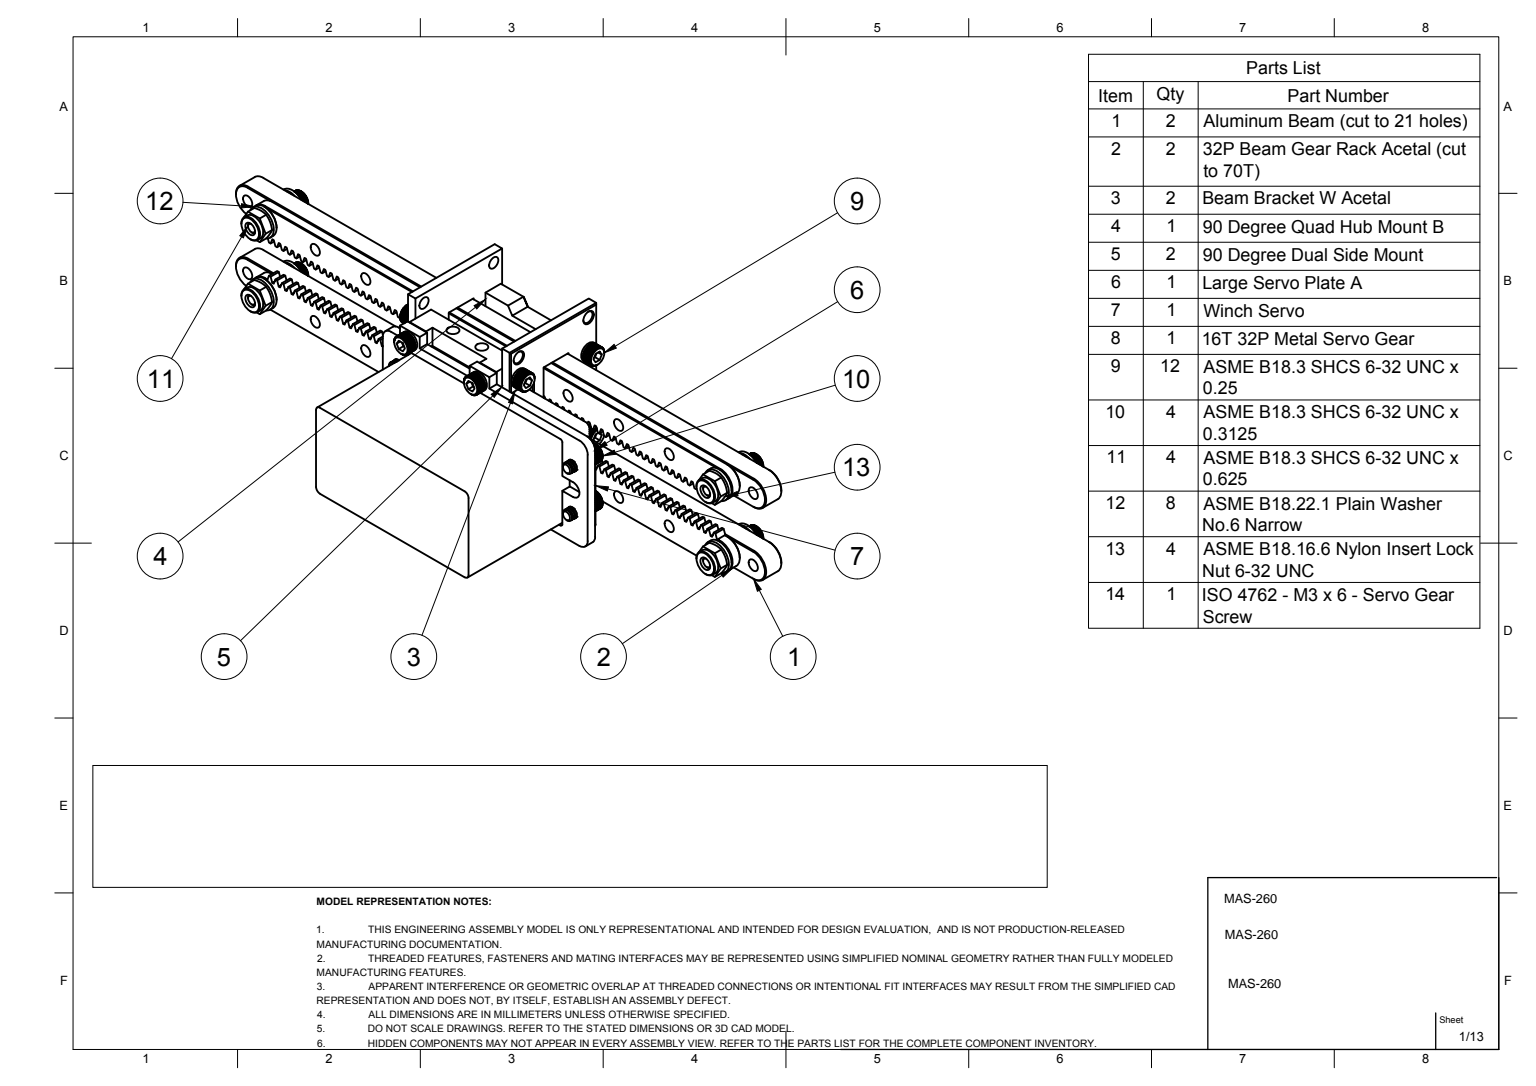
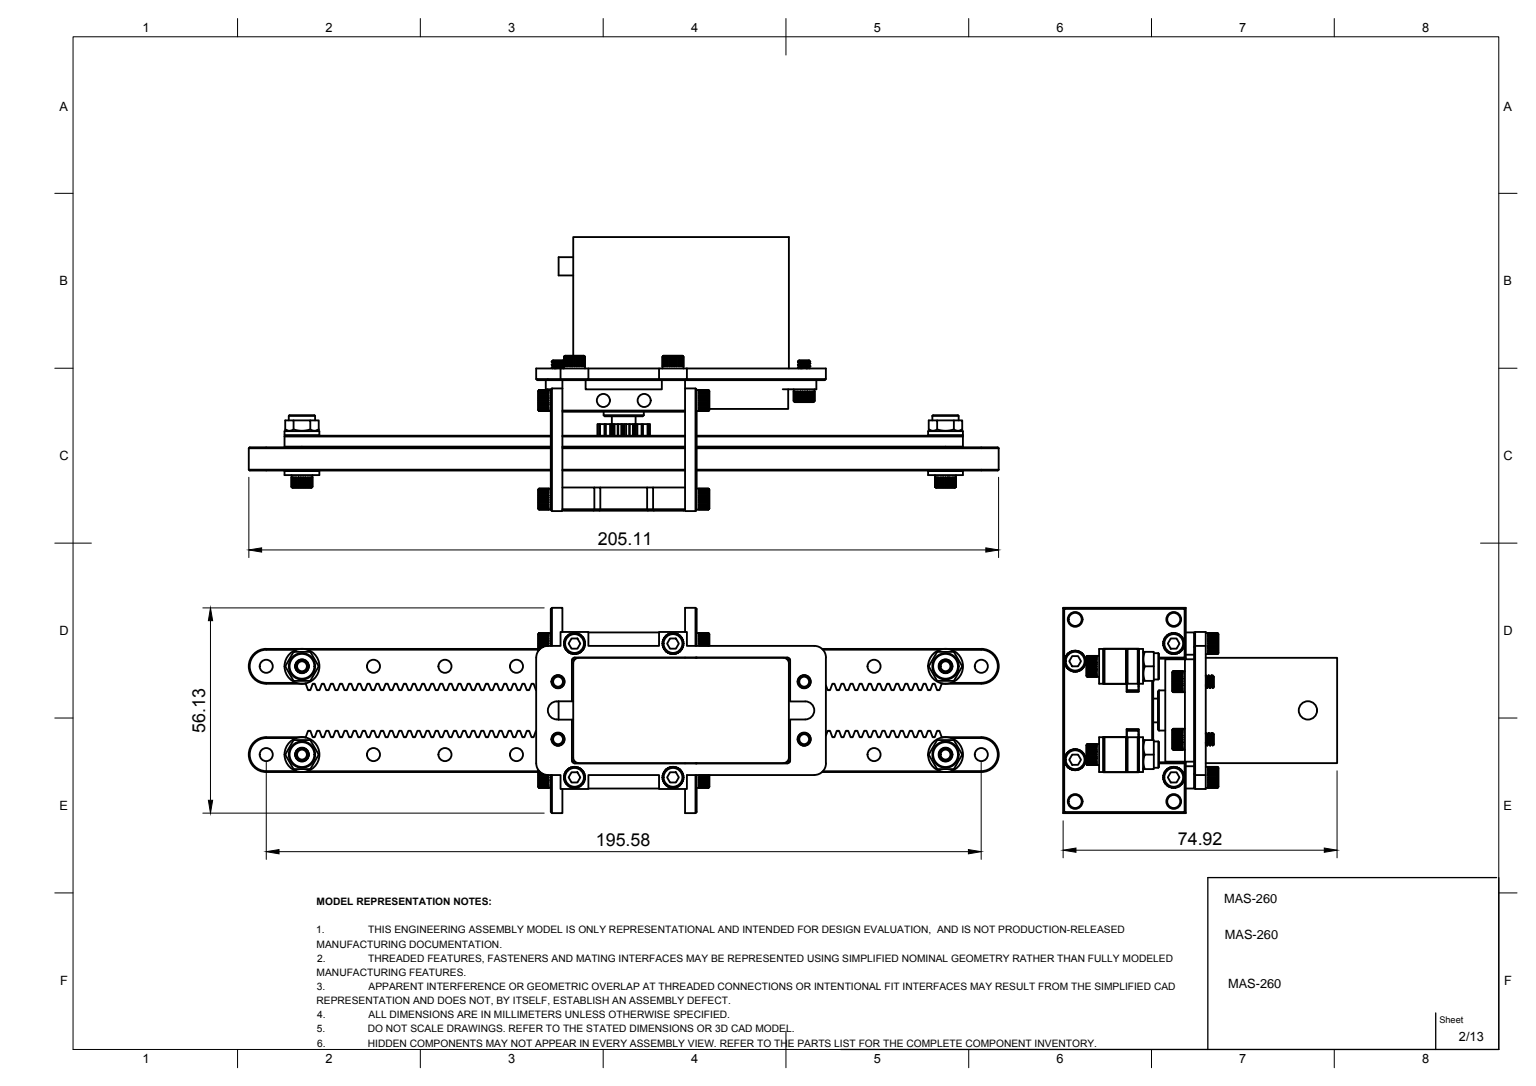
ISO-10303-21;
HEADER;
/* Generated by software containing ST-Developer
 * from STEP Tools, Inc. (www.steptools.com) 
 */

FILE_DESCRIPTION(
/* description */ (''),
/* implementation_level */ '2;1');

FILE_NAME(
/* name */ 'MAS-260',
/* time_stamp */ '2026-10-15T13:29:10-07:00',
/* author */ (''),
/* organization */ (''),
/* preprocessor_version */ 'ST-DEVELOPER v20.2',
/* originating_system */ 'Autodesk Translation Framework v15.15.0.0',
/* authorisation */ '');

FILE_SCHEMA (('AUTOMOTIVE_DESIGN { 1 0 10303 214 3 1 1 }'));
ENDSEC;

DATA;
#10=MECHANICAL_DESIGN_GEOMETRIC_PRESENTATION_REPRESENTATION('',(#933,#934,
#935,#936,#937,#938,#939,#940,#941,#942,#943,#944,#945,#946),#83219);
#11=ITEM_DEFINED_TRANSFORMATION($,$,#27872,#29210);
#12=ITEM_DEFINED_TRANSFORMATION($,$,#28000,#29211);
#13=ITEM_DEFINED_TRANSFORMATION($,$,#28335,#29212);
#14=ITEM_DEFINED_TRANSFORMATION($,$,#27099,#29213);
#15=ITEM_DEFINED_TRANSFORMATION($,$,#28406,#29214);
#16=ITEM_DEFINED_TRANSFORMATION($,$,#27207,#29215);
#17=ITEM_DEFINED_TRANSFORMATION($,$,#27360,#29216);
#18=ITEM_DEFINED_TRANSFORMATION($,$,#27453,#29217);
#19=ITEM_DEFINED_TRANSFORMATION($,$,#28461,#29218);
#20=ITEM_DEFINED_TRANSFORMATION($,$,#28693,#29219);
#21=ITEM_DEFINED_TRANSFORMATION($,$,#28927,#29220);
#22=ITEM_DEFINED_TRANSFORMATION($,$,#29171,#29221);
#23=ITEM_DEFINED_TRANSFORMATION($,$,#29184,#29222);
#24=ITEM_DEFINED_TRANSFORMATION($,$,#27595,#29223);
#25=ITEM_DEFINED_TRANSFORMATION($,$,#27872,#29224);
#26=ITEM_DEFINED_TRANSFORMATION($,$,#28000,#29225);
#27=ITEM_DEFINED_TRANSFORMATION($,$,#28335,#29226);
#28=ITEM_DEFINED_TRANSFORMATION($,$,#28406,#29227);
#29=ITEM_DEFINED_TRANSFORMATION($,$,#28461,#29228);
#30=ITEM_DEFINED_TRANSFORMATION($,$,#28461,#29229);
#31=ITEM_DEFINED_TRANSFORMATION($,$,#28461,#29230);
#32=ITEM_DEFINED_TRANSFORMATION($,$,#28461,#29231);
#33=ITEM_DEFINED_TRANSFORMATION($,$,#28461,#29232);
#34=ITEM_DEFINED_TRANSFORMATION($,$,#28461,#29233);
#35=ITEM_DEFINED_TRANSFORMATION($,$,#28461,#29234);
#36=ITEM_DEFINED_TRANSFORMATION($,$,#28461,#29235);
#37=ITEM_DEFINED_TRANSFORMATION($,$,#28461,#29236);
#38=ITEM_DEFINED_TRANSFORMATION($,$,#28461,#29237);
#39=ITEM_DEFINED_TRANSFORMATION($,$,#28461,#29238);
#40=ITEM_DEFINED_TRANSFORMATION($,$,#28693,#29239);
#41=ITEM_DEFINED_TRANSFORMATION($,$,#28693,#29240);
#42=ITEM_DEFINED_TRANSFORMATION($,$,#28693,#29241);
#43=ITEM_DEFINED_TRANSFORMATION($,$,#28927,#29242);
#44=ITEM_DEFINED_TRANSFORMATION($,$,#28927,#29243);
#45=ITEM_DEFINED_TRANSFORMATION($,$,#28927,#29244);
#46=ITEM_DEFINED_TRANSFORMATION($,$,#29171,#29245);
#47=ITEM_DEFINED_TRANSFORMATION($,$,#29171,#29246);
#48=ITEM_DEFINED_TRANSFORMATION($,$,#29171,#29247);
#49=ITEM_DEFINED_TRANSFORMATION($,$,#29171,#29248);
#50=ITEM_DEFINED_TRANSFORMATION($,$,#29171,#29249);
#51=ITEM_DEFINED_TRANSFORMATION($,$,#29171,#29250);
#52=ITEM_DEFINED_TRANSFORMATION($,$,#29171,#29251);
#53=ITEM_DEFINED_TRANSFORMATION($,$,#29184,#29252);
#54=ITEM_DEFINED_TRANSFORMATION($,$,#29184,#29253);
#55=ITEM_DEFINED_TRANSFORMATION($,$,#29184,#29254);
#56=(
REPRESENTATION_RELATIONSHIP($,$,#83305,#83299)
REPRESENTATION_RELATIONSHIP_WITH_TRANSFORMATION(#11)
SHAPE_REPRESENTATION_RELATIONSHIP()
);
#57=(
REPRESENTATION_RELATIONSHIP($,$,#83306,#83299)
REPRESENTATION_RELATIONSHIP_WITH_TRANSFORMATION(#12)
SHAPE_REPRESENTATION_RELATIONSHIP()
);
#58=(
REPRESENTATION_RELATIONSHIP($,$,#83307,#83299)
REPRESENTATION_RELATIONSHIP_WITH_TRANSFORMATION(#13)
SHAPE_REPRESENTATION_RELATIONSHIP()
);
#59=(
REPRESENTATION_RELATIONSHIP($,$,#83300,#83299)
REPRESENTATION_RELATIONSHIP_WITH_TRANSFORMATION(#14)
SHAPE_REPRESENTATION_RELATIONSHIP()
);
#60=(
REPRESENTATION_RELATIONSHIP($,$,#83308,#83299)
REPRESENTATION_RELATIONSHIP_WITH_TRANSFORMATION(#15)
SHAPE_REPRESENTATION_RELATIONSHIP()
);
#61=(
REPRESENTATION_RELATIONSHIP($,$,#83301,#83299)
REPRESENTATION_RELATIONSHIP_WITH_TRANSFORMATION(#16)
SHAPE_REPRESENTATION_RELATIONSHIP()
);
#62=(
REPRESENTATION_RELATIONSHIP($,$,#83302,#83299)
REPRESENTATION_RELATIONSHIP_WITH_TRANSFORMATION(#17)
SHAPE_REPRESENTATION_RELATIONSHIP()
);
#63=(
REPRESENTATION_RELATIONSHIP($,$,#83303,#83299)
REPRESENTATION_RELATIONSHIP_WITH_TRANSFORMATION(#18)
SHAPE_REPRESENTATION_RELATIONSHIP()
);
#64=(
REPRESENTATION_RELATIONSHIP($,$,#83309,#83299)
REPRESENTATION_RELATIONSHIP_WITH_TRANSFORMATION(#19)
SHAPE_REPRESENTATION_RELATIONSHIP()
);
#65=(
REPRESENTATION_RELATIONSHIP($,$,#83310,#83299)
REPRESENTATION_RELATIONSHIP_WITH_TRANSFORMATION(#20)
SHAPE_REPRESENTATION_RELATIONSHIP()
);
#66=(
REPRESENTATION_RELATIONSHIP($,$,#83311,#83299)
REPRESENTATION_RELATIONSHIP_WITH_TRANSFORMATION(#21)
SHAPE_REPRESENTATION_RELATIONSHIP()
);
#67=(
REPRESENTATION_RELATIONSHIP($,$,#83312,#83299)
REPRESENTATION_RELATIONSHIP_WITH_TRANSFORMATION(#22)
SHAPE_REPRESENTATION_RELATIONSHIP()
);
#68=(
REPRESENTATION_RELATIONSHIP($,$,#83313,#83299)
REPRESENTATION_RELATIONSHIP_WITH_TRANSFORMATION(#23)
SHAPE_REPRESENTATION_RELATIONSHIP()
);
#69=(
REPRESENTATION_RELATIONSHIP($,$,#83304,#83299)
REPRESENTATION_RELATIONSHIP_WITH_TRANSFORMATION(#24)
SHAPE_REPRESENTATION_RELATIONSHIP()
);
#70=(
REPRESENTATION_RELATIONSHIP($,$,#83305,#83299)
REPRESENTATION_RELATIONSHIP_WITH_TRANSFORMATION(#25)
SHAPE_REPRESENTATION_RELATIONSHIP()
);
#71=(
REPRESENTATION_RELATIONSHIP($,$,#83306,#83299)
REPRESENTATION_RELATIONSHIP_WITH_TRANSFORMATION(#26)
SHAPE_REPRESENTATION_RELATIONSHIP()
);
#72=(
REPRESENTATION_RELATIONSHIP($,$,#83307,#83299)
REPRESENTATION_RELATIONSHIP_WITH_TRANSFORMATION(#27)
SHAPE_REPRESENTATION_RELATIONSHIP()
);
#73=(
REPRESENTATION_RELATIONSHIP($,$,#83308,#83299)
REPRESENTATION_RELATIONSHIP_WITH_TRANSFORMATION(#28)
SHAPE_REPRESENTATION_RELATIONSHIP()
);
#74=(
REPRESENTATION_RELATIONSHIP($,$,#83309,#83299)
REPRESENTATION_RELATIONSHIP_WITH_TRANSFORMATION(#29)
SHAPE_REPRESENTATION_RELATIONSHIP()
);
#75=(
REPRESENTATION_RELATIONSHIP($,$,#83309,#83299)
REPRESENTATION_RELATIONSHIP_WITH_TRANSFORMATION(#30)
SHAPE_REPRESENTATION_RELATIONSHIP()
);
#76=(
REPRESENTATION_RELATIONSHIP($,$,#83309,#83299)
REPRESENTATION_RELATIONSHIP_WITH_TRANSFORMATION(#31)
SHAPE_REPRESENTATION_RELATIONSHIP()
);
#77=(
REPRESENTATION_RELATIONSHIP($,$,#83309,#83299)
REPRESENTATION_RELATIONSHIP_WITH_TRANSFORMATION(#32)
SHAPE_REPRESENTATION_RELATIONSHIP()
);
#78=(
REPRESENTATION_RELATIONSHIP($,$,#83309,#83299)
REPRESENTATION_RELATIONSHIP_WITH_TRANSFORMATION(#33)
SHAPE_REPRESENTATION_RELATIONSHIP()
);
#79=(
REPRESENTATION_RELATIONSHIP($,$,#83309,#83299)
REPRESENTATION_RELATIONSHIP_WITH_TRANSFORMATION(#34)
SHAPE_REPRESENTATION_RELATIONSHIP()
);
#80=(
REPRESENTATION_RELATIONSHIP($,$,#83309,#83299)
REPRESENTATION_RELATIONSHIP_WITH_TRANSFORMATION(#35)
SHAPE_REPRESENTATION_RELATIONSHIP()
);
#81=(
REPRESENTATION_RELATIONSHIP($,$,#83309,#83299)
REPRESENTATION_RELATIONSHIP_WITH_TRANSFORMATION(#36)
SHAPE_REPRESENTATION_RELATIONSHIP()
);
#82=(
REPRESENTATION_RELATIONSHIP($,$,#83309,#83299)
REPRESENTATION_RELATIONSHIP_WITH_TRANSFORMATION(#37)
SHAPE_REPRESENTATION_RELATIONSHIP()
);
#83=(
REPRESENTATION_RELATIONSHIP($,$,#83309,#83299)
REPRESENTATION_RELATIONSHIP_WITH_TRANSFORMATION(#38)
SHAPE_REPRESENTATION_RELATIONSHIP()
);
#84=(
REPRESENTATION_RELATIONSHIP($,$,#83309,#83299)
REPRESENTATION_RELATIONSHIP_WITH_TRANSFORMATION(#39)
SHAPE_REPRESENTATION_RELATIONSHIP()
);
#85=(
REPRESENTATION_RELATIONSHIP($,$,#83310,#83299)
REPRESENTATION_RELATIONSHIP_WITH_TRANSFORMATION(#40)
SHAPE_REPRESENTATION_RELATIONSHIP()
);
#86=(
REPRESENTATION_RELATIONSHIP($,$,#83310,#83299)
REPRESENTATION_RELATIONSHIP_WITH_TRANSFORMATION(#41)
SHAPE_REPRESENTATION_RELATIONSHIP()
);
#87=(
REPRESENTATION_RELATIONSHIP($,$,#83310,#83299)
REPRESENTATION_RELATIONSHIP_WITH_TRANSFORMATION(#42)
SHAPE_REPRESENTATION_RELATIONSHIP()
);
#88=(
REPRESENTATION_RELATIONSHIP($,$,#83311,#83299)
REPRESENTATION_RELATIONSHIP_WITH_TRANSFORMATION(#43)
SHAPE_REPRESENTATION_RELATIONSHIP()
);
#89=(
REPRESENTATION_RELATIONSHIP($,$,#83311,#83299)
REPRESENTATION_RELATIONSHIP_WITH_TRANSFORMATION(#44)
SHAPE_REPRESENTATION_RELATIONSHIP()
);
#90=(
REPRESENTATION_RELATIONSHIP($,$,#83311,#83299)
REPRESENTATION_RELATIONSHIP_WITH_TRANSFORMATION(#45)
SHAPE_REPRESENTATION_RELATIONSHIP()
);
#91=(
REPRESENTATION_RELATIONSHIP($,$,#83312,#83299)
REPRESENTATION_RELATIONSHIP_WITH_TRANSFORMATION(#46)
SHAPE_REPRESENTATION_RELATIONSHIP()
);
#92=(
REPRESENTATION_RELATIONSHIP($,$,#83312,#83299)
REPRESENTATION_RELATIONSHIP_WITH_TRANSFORMATION(#47)
SHAPE_REPRESENTATION_RELATIONSHIP()
);
#93=(
REPRESENTATION_RELATIONSHIP($,$,#83312,#83299)
REPRESENTATION_RELATIONSHIP_WITH_TRANSFORMATION(#48)
SHAPE_REPRESENTATION_RELATIONSHIP()
);
#94=(
REPRESENTATION_RELATIONSHIP($,$,#83312,#83299)
REPRESENTATION_RELATIONSHIP_WITH_TRANSFORMATION(#49)
SHAPE_REPRESENTATION_RELATIONSHIP()
);
#95=(
REPRESENTATION_RELATIONSHIP($,$,#83312,#83299)
REPRESENTATION_RELATIONSHIP_WITH_TRANSFORMATION(#50)
SHAPE_REPRESENTATION_RELATIONSHIP()
);
#96=(
REPRESENTATION_RELATIONSHIP($,$,#83312,#83299)
REPRESENTATION_RELATIONSHIP_WITH_TRANSFORMATION(#51)
SHAPE_REPRESENTATION_RELATIONSHIP()
);
#97=(
REPRESENTATION_RELATIONSHIP($,$,#83312,#83299)
REPRESENTATION_RELATIONSHIP_WITH_TRANSFORMATION(#52)
SHAPE_REPRESENTATION_RELATIONSHIP()
);
#98=(
REPRESENTATION_RELATIONSHIP($,$,#83313,#83299)
REPRESENTATION_RELATIONSHIP_WITH_TRANSFORMATION(#53)
SHAPE_REPRESENTATION_RELATIONSHIP()
);
#99=(
REPRESENTATION_RELATIONSHIP($,$,#83313,#83299)
REPRESENTATION_RELATIONSHIP_WITH_TRANSFORMATION(#54)
SHAPE_REPRESENTATION_RELATIONSHIP()
);
#100=(
REPRESENTATION_RELATIONSHIP($,$,#83313,#83299)
REPRESENTATION_RELATIONSHIP_WITH_TRANSFORMATION(#55)
SHAPE_REPRESENTATION_RELATIONSHIP()
);
#101=CONTEXT_DEPENDENT_SHAPE_REPRESENTATION(#56,#83254);
#102=CONTEXT_DEPENDENT_SHAPE_REPRESENTATION(#57,#83255);
#103=CONTEXT_DEPENDENT_SHAPE_REPRESENTATION(#58,#83256);
#104=CONTEXT_DEPENDENT_SHAPE_REPRESENTATION(#59,#83257);
#105=CONTEXT_DEPENDENT_SHAPE_REPRESENTATION(#60,#83258);
#106=CONTEXT_DEPENDENT_SHAPE_REPRESENTATION(#61,#83259);
#107=CONTEXT_DEPENDENT_SHAPE_REPRESENTATION(#62,#83260);
#108=CONTEXT_DEPENDENT_SHAPE_REPRESENTATION(#63,#83261);
#109=CONTEXT_DEPENDENT_SHAPE_REPRESENTATION(#64,#83262);
#110=CONTEXT_DEPENDENT_SHAPE_REPRESENTATION(#65,#83263);
#111=CONTEXT_DEPENDENT_SHAPE_REPRESENTATION(#66,#83264);
#112=CONTEXT_DEPENDENT_SHAPE_REPRESENTATION(#67,#83265);
#113=CONTEXT_DEPENDENT_SHAPE_REPRESENTATION(#68,#83266);
#114=CONTEXT_DEPENDENT_SHAPE_REPRESENTATION(#69,#83267);
#115=CONTEXT_DEPENDENT_SHAPE_REPRESENTATION(#70,#83268);
#116=CONTEXT_DEPENDENT_SHAPE_REPRESENTATION(#71,#83269);
#117=CONTEXT_DEPENDENT_SHAPE_REPRESENTATION(#72,#83270);
#118=CONTEXT_DEPENDENT_SHAPE_REPRESENTATION(#73,#83271);
#119=CONTEXT_DEPENDENT_SHAPE_REPRESENTATION(#74,#83272);
#120=CONTEXT_DEPENDENT_SHAPE_REPRESENTATION(#75,#83273);
#121=CONTEXT_DEPENDENT_SHAPE_REPRESENTATION(#76,#83274);
#122=CONTEXT_DEPENDENT_SHAPE_REPRESENTATION(#77,#83275);
#123=CONTEXT_DEPENDENT_SHAPE_REPRESENTATION(#78,#83276);
#124=CONTEXT_DEPENDENT_SHAPE_REPRESENTATION(#79,#83277);
#125=CONTEXT_DEPENDENT_SHAPE_REPRESENTATION(#80,#83278);
#126=CONTEXT_DEPENDENT_SHAPE_REPRESENTATION(#81,#83279);
#127=CONTEXT_DEPENDENT_SHAPE_REPRESENTATION(#82,#83280);
#128=CONTEXT_DEPENDENT_SHAPE_REPRESENTATION(#83,#83281);
#129=CONTEXT_DEPENDENT_SHAPE_REPRESENTATION(#84,#83282);
#130=CONTEXT_DEPENDENT_SHAPE_REPRESENTATION(#85,#83283);
#131=CONTEXT_DEPENDENT_SHAPE_REPRESENTATION(#86,#83284);
#132=CONTEXT_DEPENDENT_SHAPE_REPRESENTATION(#87,#83285);
#133=CONTEXT_DEPENDENT_SHAPE_REPRESENTATION(#88,#83286);
#134=CONTEXT_DEPENDENT_SHAPE_REPRESENTATION(#89,#83287);
#135=CONTEXT_DEPENDENT_SHAPE_REPRESENTATION(#90,#83288);
#136=CONTEXT_DEPENDENT_SHAPE_REPRESENTATION(#91,#83289);
#137=CONTEXT_DEPENDENT_SHAPE_REPRESENTATION(#92,#83290);
#138=CONTEXT_DEPENDENT_SHAPE_REPRESENTATION(#93,#83291);
#139=CONTEXT_DEPENDENT_SHAPE_REPRESENTATION(#94,#83292);
#140=CONTEXT_DEPENDENT_SHAPE_REPRESENTATION(#95,#83293);
#141=CONTEXT_DEPENDENT_SHAPE_REPRESENTATION(#96,#83294);
#142=CONTEXT_DEPENDENT_SHAPE_REPRESENTATION(#97,#83295);
#143=CONTEXT_DEPENDENT_SHAPE_REPRESENTATION(#98,#83296);
#144=CONTEXT_DEPENDENT_SHAPE_REPRESENTATION(#99,#83297);
#145=CONTEXT_DEPENDENT_SHAPE_REPRESENTATION(#100,#83298);
#146=NEXT_ASSEMBLY_USAGE_OCCURRENCE('Aluminum Beam (cut to 21 holes):1',
'Aluminum Beam (cut to 21 holes):1','Aluminum Beam (cut to 21 holes):1',
#83315,#83321,'Aluminum Beam (cut to 21 holes):1');
#147=NEXT_ASSEMBLY_USAGE_OCCURRENCE(
'32P Beam Gear Rack Acetal (cut to 70T):1',
'32P Beam Gear Rack Acetal (cut to 70T):1',
'32P Beam Gear Rack Acetal (cut to 70T):1',#83315,#83322,
'32P Beam Gear Rack Acetal (cut to 70T):1');
#148=NEXT_ASSEMBLY_USAGE_OCCURRENCE('Beam Bracket W Acetal:1',
'Beam Bracket W Acetal:1','Beam Bracket W Acetal:1',#83315,#83323,
'Beam Bracket W Acetal:1');
#149=NEXT_ASSEMBLY_USAGE_OCCURRENCE('90 Degree Quad Hub Mount B:1',
'90 Degree Quad Hub Mount B:1','90 Degree Quad Hub Mount B:1',#83315,#83316,
'90 Degree Quad Hub Mount B:1');
#150=NEXT_ASSEMBLY_USAGE_OCCURRENCE('90 Degree Dual Side Mount:1',
'90 Degree Dual Side Mount:1','90 Degree Dual Side Mount:1',#83315,#83324,
'90 Degree Dual Side Mount:1');
#151=NEXT_ASSEMBLY_USAGE_OCCURRENCE('Large Servo Plate A:1',
'Large Servo Plate A:1','Large Servo Plate A:1',#83315,#83317,
'Large Servo Plate A:1');
#152=NEXT_ASSEMBLY_USAGE_OCCURRENCE('Winch Servo:1','Winch Servo:1',
'Winch Servo:1',#83315,#83318,'Winch Servo:1');
#153=NEXT_ASSEMBLY_USAGE_OCCURRENCE('16T 32P Metal Servo Gear:1',
'16T 32P Metal Servo Gear:1','16T 32P Metal Servo Gear:1',#83315,#83319,
'16T 32P Metal Servo Gear:1');
#154=NEXT_ASSEMBLY_USAGE_OCCURRENCE('ASME B18.3 SHCS 6-32 UNC x 0.25:1',
'ASME B18.3 SHCS 6-32 UNC x 0.25:1','ASME B18.3 SHCS 6-32 UNC x 0.25:1',
#83315,#83325,'ASME B18.3 SHCS 6-32 UNC x 0.25:1');
#155=NEXT_ASSEMBLY_USAGE_OCCURRENCE(
'ASME B18.3 SHCS 6-32 UNC x 0.3125:1',
'ASME B18.3 SHCS 6-32 UNC x 0.3125:1',
'ASME B18.3 SHCS 6-32 UNC x 0.3125:1',#83315,#83326,
'ASME B18.3 SHCS 6-32 UNC x 0.3125:1');
#156=NEXT_ASSEMBLY_USAGE_OCCURRENCE(
'ASME B18.3 SHCS 6-32 UNC x 0.625:1',
'ASME B18.3 SHCS 6-32 UNC x 0.625:1',
'ASME B18.3 SHCS 6-32 UNC x 0.625:1',#83315,#83327,
'ASME B18.3 SHCS 6-32 UNC x 0.625:1');
#157=NEXT_ASSEMBLY_USAGE_OCCURRENCE(
'ASME B18.22.1 Plain Washer No.6 Narrow:1',
'ASME B18.22.1 Plain Washer No.6 Narrow:1',
'ASME B18.22.1 Plain Washer No.6 Narrow:1',#83315,#83328,
'ASME B18.22.1 Plain Washer No.6 Narrow:1');
#158=NEXT_ASSEMBLY_USAGE_OCCURRENCE(
'ASME B18.16.6 Nylon Insert Lock Nut 6-32 UNC:1',
'ASME B18.16.6 Nylon Insert Lock Nut 6-32 UNC:1',
'ASME B18.16.6 Nylon Insert Lock Nut 6-32 UNC:1',#83315,#83329,
'ASME B18.16.6 Nylon Insert Lock Nut 6-32 UNC:1');
#159=NEXT_ASSEMBLY_USAGE_OCCURRENCE(
'ISO 4762 - M3 x 6 - Servo Gear Screw:1',
'ISO 4762 - M3 x 6 - Servo Gear Screw:1',
'ISO 4762 - M3 x 6 - Servo Gear Screw:1',#83315,#83320,
'ISO 4762 - M3 x 6 - Servo Gear Screw:1');
#160=NEXT_ASSEMBLY_USAGE_OCCURRENCE('Aluminum Beam (cut to 21 holes):2',
'Aluminum Beam (cut to 21 holes):2','Aluminum Beam (cut to 21 holes):2',
#83315,#83321,'Aluminum Beam (cut to 21 holes):2');
#161=NEXT_ASSEMBLY_USAGE_OCCURRENCE(
'32P Beam Gear Rack Acetal (cut to 70T):2',
'32P Beam Gear Rack Acetal (cut to 70T):2',
'32P Beam Gear Rack Acetal (cut to 70T):2',#83315,#83322,
'32P Beam Gear Rack Acetal (cut to 70T):2');
#162=NEXT_ASSEMBLY_USAGE_OCCURRENCE('Beam Bracket W Acetal:2',
'Beam Bracket W Acetal:2','Beam Bracket W Acetal:2',#83315,#83323,
'Beam Bracket W Acetal:2');
#163=NEXT_ASSEMBLY_USAGE_OCCURRENCE('90 Degree Dual Side Mount:2',
'90 Degree Dual Side Mount:2','90 Degree Dual Side Mount:2',#83315,#83324,
'90 Degree Dual Side Mount:2');
#164=NEXT_ASSEMBLY_USAGE_OCCURRENCE('ASME B18.3 SHCS 6-32 UNC x 0.25:2',
'ASME B18.3 SHCS 6-32 UNC x 0.25:2','ASME B18.3 SHCS 6-32 UNC x 0.25:2',
#83315,#83325,'ASME B18.3 SHCS 6-32 UNC x 0.25:2');
#165=NEXT_ASSEMBLY_USAGE_OCCURRENCE('ASME B18.3 SHCS 6-32 UNC x 0.25:3',
'ASME B18.3 SHCS 6-32 UNC x 0.25:3','ASME B18.3 SHCS 6-32 UNC x 0.25:3',
#83315,#83325,'ASME B18.3 SHCS 6-32 UNC x 0.25:3');
#166=NEXT_ASSEMBLY_USAGE_OCCURRENCE('ASME B18.3 SHCS 6-32 UNC x 0.25:4',
'ASME B18.3 SHCS 6-32 UNC x 0.25:4','ASME B18.3 SHCS 6-32 UNC x 0.25:4',
#83315,#83325,'ASME B18.3 SHCS 6-32 UNC x 0.25:4');
#167=NEXT_ASSEMBLY_USAGE_OCCURRENCE('ASME B18.3 SHCS 6-32 UNC x 0.25:5',
'ASME B18.3 SHCS 6-32 UNC x 0.25:5','ASME B18.3 SHCS 6-32 UNC x 0.25:5',
#83315,#83325,'ASME B18.3 SHCS 6-32 UNC x 0.25:5');
#168=NEXT_ASSEMBLY_USAGE_OCCURRENCE('ASME B18.3 SHCS 6-32 UNC x 0.25:6',
'ASME B18.3 SHCS 6-32 UNC x 0.25:6','ASME B18.3 SHCS 6-32 UNC x 0.25:6',
#83315,#83325,'ASME B18.3 SHCS 6-32 UNC x 0.25:6');
#169=NEXT_ASSEMBLY_USAGE_OCCURRENCE('ASME B18.3 SHCS 6-32 UNC x 0.25:7',
'ASME B18.3 SHCS 6-32 UNC x 0.25:7','ASME B18.3 SHCS 6-32 UNC x 0.25:7',
#83315,#83325,'ASME B18.3 SHCS 6-32 UNC x 0.25:7');
#170=NEXT_ASSEMBLY_USAGE_OCCURRENCE('ASME B18.3 SHCS 6-32 UNC x 0.25:8',
'ASME B18.3 SHCS 6-32 UNC x 0.25:8','ASME B18.3 SHCS 6-32 UNC x 0.25:8',
#83315,#83325,'ASME B18.3 SHCS 6-32 UNC x 0.25:8');
#171=NEXT_ASSEMBLY_USAGE_OCCURRENCE('ASME B18.3 SHCS 6-32 UNC x 0.25:9',
'ASME B18.3 SHCS 6-32 UNC x 0.25:9','ASME B18.3 SHCS 6-32 UNC x 0.25:9',
#83315,#83325,'ASME B18.3 SHCS 6-32 UNC x 0.25:9');
#172=NEXT_ASSEMBLY_USAGE_OCCURRENCE(
'ASME B18.3 SHCS 6-32 UNC x 0.25:10',
'ASME B18.3 SHCS 6-32 UNC x 0.25:10',
'ASME B18.3 SHCS 6-32 UNC x 0.25:10',#83315,#83325,
'ASME B18.3 SHCS 6-32 UNC x 0.25:10');
#173=NEXT_ASSEMBLY_USAGE_OCCURRENCE(
'ASME B18.3 SHCS 6-32 UNC x 0.25:11',
'ASME B18.3 SHCS 6-32 UNC x 0.25:11',
'ASME B18.3 SHCS 6-32 UNC x 0.25:11',#83315,#83325,
'ASME B18.3 SHCS 6-32 UNC x 0.25:11');
#174=NEXT_ASSEMBLY_USAGE_OCCURRENCE(
'ASME B18.3 SHCS 6-32 UNC x 0.25:12',
'ASME B18.3 SHCS 6-32 UNC x 0.25:12',
'ASME B18.3 SHCS 6-32 UNC x 0.25:12',#83315,#83325,
'ASME B18.3 SHCS 6-32 UNC x 0.25:12');
#175=NEXT_ASSEMBLY_USAGE_OCCURRENCE(
'ASME B18.3 SHCS 6-32 UNC x 0.3125:2',
'ASME B18.3 SHCS 6-32 UNC x 0.3125:2',
'ASME B18.3 SHCS 6-32 UNC x 0.3125:2',#83315,#83326,
'ASME B18.3 SHCS 6-32 UNC x 0.3125:2');
#176=NEXT_ASSEMBLY_USAGE_OCCURRENCE(
'ASME B18.3 SHCS 6-32 UNC x 0.3125:3',
'ASME B18.3 SHCS 6-32 UNC x 0.3125:3',
'ASME B18.3 SHCS 6-32 UNC x 0.3125:3',#83315,#83326,
'ASME B18.3 SHCS 6-32 UNC x 0.3125:3');
#177=NEXT_ASSEMBLY_USAGE_OCCURRENCE(
'ASME B18.3 SHCS 6-32 UNC x 0.3125:4',
'ASME B18.3 SHCS 6-32 UNC x 0.3125:4',
'ASME B18.3 SHCS 6-32 UNC x 0.3125:4',#83315,#83326,
'ASME B18.3 SHCS 6-32 UNC x 0.3125:4');
#178=NEXT_ASSEMBLY_USAGE_OCCURRENCE(
'ASME B18.3 SHCS 6-32 UNC x 0.625:2',
'ASME B18.3 SHCS 6-32 UNC x 0.625:2',
'ASME B18.3 SHCS 6-32 UNC x 0.625:2',#83315,#83327,
'ASME B18.3 SHCS 6-32 UNC x 0.625:2');
#179=NEXT_ASSEMBLY_USAGE_OCCURRENCE(
'ASME B18.3 SHCS 6-32 UNC x 0.625:3',
'ASME B18.3 SHCS 6-32 UNC x 0.625:3',
'ASME B18.3 SHCS 6-32 UNC x 0.625:3',#83315,#83327,
'ASME B18.3 SHCS 6-32 UNC x 0.625:3');
#180=NEXT_ASSEMBLY_USAGE_OCCURRENCE(
'ASME B18.3 SHCS 6-32 UNC x 0.625:4',
'ASME B18.3 SHCS 6-32 UNC x 0.625:4',
'ASME B18.3 SHCS 6-32 UNC x 0.625:4',#83315,#83327,
'ASME B18.3 SHCS 6-32 UNC x 0.625:4');
#181=NEXT_ASSEMBLY_USAGE_OCCURRENCE(
'ASME B18.22.1 Plain Washer No.6 Narrow:2',
'ASME B18.22.1 Plain Washer No.6 Narrow:2',
'ASME B18.22.1 Plain Washer No.6 Narrow:2',#83315,#83328,
'ASME B18.22.1 Plain Washer No.6 Narrow:2');
#182=NEXT_ASSEMBLY_USAGE_OCCURRENCE(
'ASME B18.22.1 Plain Washer No.6 Narrow:3',
'ASME B18.22.1 Plain Washer No.6 Narrow:3',
'ASME B18.22.1 Plain Washer No.6 Narrow:3',#83315,#83328,
'ASME B18.22.1 Plain Washer No.6 Narrow:3');
#183=NEXT_ASSEMBLY_USAGE_OCCURRENCE(
'ASME B18.22.1 Plain Washer No.6 Narrow:4',
'ASME B18.22.1 Plain Washer No.6 Narrow:4',
'ASME B18.22.1 Plain Washer No.6 Narrow:4',#83315,#83328,
'ASME B18.22.1 Plain Washer No.6 Narrow:4');
#184=NEXT_ASSEMBLY_USAGE_OCCURRENCE(
'ASME B18.22.1 Plain Washer No.6 Narrow:5',
'ASME B18.22.1 Plain Washer No.6 Narrow:5',
'ASME B18.22.1 Plain Washer No.6 Narrow:5',#83315,#83328,
'ASME B18.22.1 Plain Washer No.6 Narrow:5');
#185=NEXT_ASSEMBLY_USAGE_OCCURRENCE(
'ASME B18.22.1 Plain Washer No.6 Narrow:6',
'ASME B18.22.1 Plain Washer No.6 Narrow:6',
'ASME B18.22.1 Plain Washer No.6 Narrow:6',#83315,#83328,
'ASME B18.22.1 Plain Washer No.6 Narrow:6');
#186=NEXT_ASSEMBLY_USAGE_OCCURRENCE(
'ASME B18.22.1 Plain Washer No.6 Narrow:7',
'ASME B18.22.1 Plain Washer No.6 Narrow:7',
'ASME B18.22.1 Plain Washer No.6 Narrow:7',#83315,#83328,
'ASME B18.22.1 Plain Washer No.6 Narrow:7');
#187=NEXT_ASSEMBLY_USAGE_OCCURRENCE(
'ASME B18.22.1 Plain Washer No.6 Narrow:8',
'ASME B18.22.1 Plain Washer No.6 Narrow:8',
'ASME B18.22.1 Plain Washer No.6 Narrow:8',#83315,#83328,
'ASME B18.22.1 Plain Washer No.6 Narrow:8');
#188=NEXT_ASSEMBLY_USAGE_OCCURRENCE(
'ASME B18.16.6 Nylon Insert Lock Nut 6-32 UNC:2',
'ASME B18.16.6 Nylon Insert Lock Nut 6-32 UNC:2',
'ASME B18.16.6 Nylon Insert Lock Nut 6-32 UNC:2',#83315,#83329,
'ASME B18.16.6 Nylon Insert Lock Nut 6-32 UNC:2');
#189=NEXT_ASSEMBLY_USAGE_OCCURRENCE(
'ASME B18.16.6 Nylon Insert Lock Nut 6-32 UNC:3',
'ASME B18.16.6 Nylon Insert Lock Nut 6-32 UNC:3',
'ASME B18.16.6 Nylon Insert Lock Nut 6-32 UNC:3',#83315,#83329,
'ASME B18.16.6 Nylon Insert Lock Nut 6-32 UNC:3');
#190=NEXT_ASSEMBLY_USAGE_OCCURRENCE(
'ASME B18.16.6 Nylon Insert Lock Nut 6-32 UNC:4',
'ASME B18.16.6 Nylon Insert Lock Nut 6-32 UNC:4',
'ASME B18.16.6 Nylon Insert Lock Nut 6-32 UNC:4',#83315,#83329,
'ASME B18.16.6 Nylon Insert Lock Nut 6-32 UNC:4');
#191=ELLIPSE('',#28417,2.5491199461775,1.8025);
#192=ELLIPSE('',#28419,2.5491199461775,1.8025);
#193=ELLIPSE('',#28421,2.5491199461775,1.8025);
#194=ELLIPSE('',#28427,2.5491199461775,1.8025);
#195=ELLIPSE('',#28429,2.5491199461775,1.8025);
#196=ELLIPSE('',#28431,2.5491199461775,1.8025);
#197=(
BOUNDED_CURVE()
B_SPLINE_CURVE(2,(#49716,#49717,#49718),.UNSPECIFIED.,.F.,.F.)
B_SPLINE_CURVE_WITH_KNOTS((3,3),(0.022587909800489,0.0437523366271109),
 .UNSPECIFIED.)
CURVE()
GEOMETRIC_REPRESENTATION_ITEM()
RATIONAL_B_SPLINE_CURVE((1.0009393918053,1.00090979171719,1.))
REPRESENTATION_ITEM('')
);
#198=(
BOUNDED_CURVE()
B_SPLINE_CURVE(2,(#49730,#49731,#49732),.UNSPECIFIED.,.F.,.F.)
B_SPLINE_CURVE_WITH_KNOTS((3,3),(0.,0.021164426826556),.UNSPECIFIED.)
CURVE()
GEOMETRIC_REPRESENTATION_ITEM()
RATIONAL_B_SPLINE_CURVE((1.,1.0009097917188,1.00093939180696))
REPRESENTATION_ITEM('')
);
#199=(
BOUNDED_CURVE()
B_SPLINE_CURVE(2,(#50025,#50026,#50027),.UNSPECIFIED.,.F.,.F.)
B_SPLINE_CURVE_WITH_KNOTS((3,3),(0.0225879098005002,0.0437523366271109),
 .UNSPECIFIED.)
CURVE()
GEOMETRIC_REPRESENTATION_ITEM()
RATIONAL_B_SPLINE_CURVE((1.00093939180451,1.00090979171643,1.))
REPRESENTATION_ITEM('')
);
#200=(
BOUNDED_CURVE()
B_SPLINE_CURVE(2,(#50034,#50035,#50036),.UNSPECIFIED.,.F.,.F.)
B_SPLINE_CURVE_WITH_KNOTS((3,3),(0.,0.0211644268266061),.UNSPECIFIED.)
CURVE()
GEOMETRIC_REPRESENTATION_ITEM()
RATIONAL_B_SPLINE_CURVE((1.,1.00090979171738,1.0009393918055))
REPRESENTATION_ITEM('')
);
#201=(
BOUNDED_CURVE()
B_SPLINE_CURVE(2,(#50039,#50040,#50041),.UNSPECIFIED.,.F.,.F.)
B_SPLINE_CURVE_WITH_KNOTS((3,3),(0.0225879098006031,0.0437523366271109),
 .UNSPECIFIED.)
CURVE()
GEOMETRIC_REPRESENTATION_ITEM()
RATIONAL_B_SPLINE_CURVE((1.00093939180394,1.00090979171587,1.))
REPRESENTATION_ITEM('')
);
#202=(
BOUNDED_CURVE()
B_SPLINE_CURVE(2,(#50048,#50049,#50050),.UNSPECIFIED.,.F.,.F.)
B_SPLINE_CURVE_WITH_KNOTS((3,3),(0.,0.0211644268265667),.UNSPECIFIED.)
CURVE()
GEOMETRIC_REPRESENTATION_ITEM()
RATIONAL_B_SPLINE_CURVE((1.,1.00090979171289,1.00093939180086))
REPRESENTATION_ITEM('')
);
#203=(
BOUNDED_CURVE()
B_SPLINE_CURVE(2,(#50053,#50054,#50055),.UNSPECIFIED.,.F.,.F.)
B_SPLINE_CURVE_WITH_KNOTS((3,3),(0.0225879098005541,0.0437523366271109),
 .UNSPECIFIED.)
CURVE()
GEOMETRIC_REPRESENTATION_ITEM()
RATIONAL_B_SPLINE_CURVE((1.00093939180201,1.000909791714,1.))
REPRESENTATION_ITEM('')
);
#204=(
BOUNDED_CURVE()
B_SPLINE_CURVE(2,(#50062,#50063,#50064),.UNSPECIFIED.,.F.,.F.)
B_SPLINE_CURVE_WITH_KNOTS((3,3),(0.,0.0211644268265858),.UNSPECIFIED.)
CURVE()
GEOMETRIC_REPRESENTATION_ITEM()
RATIONAL_B_SPLINE_CURVE((1.,1.00090979171717,1.00093939180528))
REPRESENTATION_ITEM('')
);
#205=(
BOUNDED_CURVE()
B_SPLINE_CURVE(2,(#50067,#50068,#50069),.UNSPECIFIED.,.F.,.F.)
B_SPLINE_CURVE_WITH_KNOTS((3,3),(0.0225879098004799,0.0437523366271109),
 .UNSPECIFIED.)
CURVE()
GEOMETRIC_REPRESENTATION_ITEM()
RATIONAL_B_SPLINE_CURVE((1.00093939180147,1.00090979171348,1.))
REPRESENTATION_ITEM('')
);
#206=(
BOUNDED_CURVE()
B_SPLINE_CURVE(2,(#50076,#50077,#50078),.UNSPECIFIED.,.F.,.F.)
B_SPLINE_CURVE_WITH_KNOTS((3,3),(0.,0.0211644268266267),.UNSPECIFIED.)
CURVE()
GEOMETRIC_REPRESENTATION_ITEM()
RATIONAL_B_SPLINE_CURVE((1.,1.00090979171262,1.00093939180058))
REPRESENTATION_ITEM('')
);
#207=(
BOUNDED_CURVE()
B_SPLINE_CURVE(2,(#50081,#50082,#50083),.UNSPECIFIED.,.F.,.F.)
B_SPLINE_CURVE_WITH_KNOTS((3,3),(0.0225879098005392,0.0437523366271109),
 .UNSPECIFIED.)
CURVE()
GEOMETRIC_REPRESENTATION_ITEM()
RATIONAL_B_SPLINE_CURVE((1.00093939179924,1.00090979171132,1.))
REPRESENTATION_ITEM('')
);
#208=(
BOUNDED_CURVE()
B_SPLINE_CURVE(2,(#50090,#50091,#50092),.UNSPECIFIED.,.F.,.F.)
B_SPLINE_CURVE_WITH_KNOTS((3,3),(0.,0.0211644268265472),.UNSPECIFIED.)
CURVE()
GEOMETRIC_REPRESENTATION_ITEM()
RATIONAL_B_SPLINE_CURVE((1.,1.00090979171511,1.00093939180316))
REPRESENTATION_ITEM('')
);
#209=(
BOUNDED_CURVE()
B_SPLINE_CURVE(2,(#50095,#50096,#50097),.UNSPECIFIED.,.F.,.F.)
B_SPLINE_CURVE_WITH_KNOTS((3,3),(0.0225879098005708,0.0437523366271109),
 .UNSPECIFIED.)
CURVE()
GEOMETRIC_REPRESENTATION_ITEM()
RATIONAL_B_SPLINE_CURVE((1.00093939180557,1.00090979171745,1.))
REPRESENTATION_ITEM('')
);
#210=(
BOUNDED_CURVE()
B_SPLINE_CURVE(2,(#50104,#50105,#50106),.UNSPECIFIED.,.F.,.F.)
B_SPLINE_CURVE_WITH_KNOTS((3,3),(0.,0.0211644268265667),.UNSPECIFIED.)
CURVE()
GEOMETRIC_REPRESENTATION_ITEM()
RATIONAL_B_SPLINE_CURVE((1.,1.00090979171694,1.00093939180505))
REPRESENTATION_ITEM('')
);
#211=(
BOUNDED_CURVE()
B_SPLINE_CURVE(2,(#50109,#50110,#50111),.UNSPECIFIED.,.F.,.F.)
B_SPLINE_CURVE_WITH_KNOTS((3,3),(0.0225879098005834,0.0437523366271109),
 .UNSPECIFIED.)
CURVE()
GEOMETRIC_REPRESENTATION_ITEM()
RATIONAL_B_SPLINE_CURVE((1.00093939180667,1.00090979171851,1.))
REPRESENTATION_ITEM('')
);
#212=(
BOUNDED_CURVE()
B_SPLINE_CURVE(2,(#50118,#50119,#50120),.UNSPECIFIED.,.F.,.F.)
B_SPLINE_CURVE_WITH_KNOTS((3,3),(0.,0.021164426826593),.UNSPECIFIED.)
CURVE()
GEOMETRIC_REPRESENTATION_ITEM()
RATIONAL_B_SPLINE_CURVE((1.,1.00090979171443,1.00093939180245))
REPRESENTATION_ITEM('')
);
#213=(
BOUNDED_CURVE()
B_SPLINE_CURVE(2,(#50123,#50124,#50125),.UNSPECIFIED.,.F.,.F.)
B_SPLINE_CURVE_WITH_KNOTS((3,3),(0.0225879098005489,0.0437523366271109),
 .UNSPECIFIED.)
CURVE()
GEOMETRIC_REPRESENTATION_ITEM()
RATIONAL_B_SPLINE_CURVE((1.00093939180192,1.00090979171391,1.))
REPRESENTATION_ITEM('')
);
#214=(
BOUNDED_CURVE()
B_SPLINE_CURVE(2,(#50132,#50133,#50134),.UNSPECIFIED.,.F.,.F.)
B_SPLINE_CURVE_WITH_KNOTS((3,3),(0.,0.0211644268265642),.UNSPECIFIED.)
CURVE()
GEOMETRIC_REPRESENTATION_ITEM()
RATIONAL_B_SPLINE_CURVE((1.,1.00090979171418,1.00093939180219))
REPRESENTATION_ITEM('')
);
#215=(
BOUNDED_CURVE()
B_SPLINE_CURVE(2,(#50137,#50138,#50139),.UNSPECIFIED.,.F.,.F.)
B_SPLINE_CURVE_WITH_KNOTS((3,3),(0.022587909800521,0.0437523366271108),
 .UNSPECIFIED.)
CURVE()
GEOMETRIC_REPRESENTATION_ITEM()
RATIONAL_B_SPLINE_CURVE((1.000939391805,1.00090979171689,1.))
REPRESENTATION_ITEM('')
);
#216=(
BOUNDED_CURVE()
B_SPLINE_CURVE(2,(#50146,#50147,#50148),.UNSPECIFIED.,.F.,.F.)
B_SPLINE_CURVE_WITH_KNOTS((3,3),(0.,0.0211644268266283),.UNSPECIFIED.)
CURVE()
GEOMETRIC_REPRESENTATION_ITEM()
RATIONAL_B_SPLINE_CURVE((1.,1.0009097917149,1.00093939180294))
REPRESENTATION_ITEM('')
);
#217=(
BOUNDED_CURVE()
B_SPLINE_CURVE(2,(#50151,#50152,#50153),.UNSPECIFIED.,.F.,.F.)
B_SPLINE_CURVE_WITH_KNOTS((3,3),(0.0225879098005678,0.0437523366271109),
 .UNSPECIFIED.)
CURVE()
GEOMETRIC_REPRESENTATION_ITEM()
RATIONAL_B_SPLINE_CURVE((1.0009393918065,1.00090979171835,1.))
REPRESENTATION_ITEM('')
);
#218=(
BOUNDED_CURVE()
B_SPLINE_CURVE(2,(#50160,#50161,#50162),.UNSPECIFIED.,.F.,.F.)
B_SPLINE_CURVE_WITH_KNOTS((3,3),(0.,0.0211644268266094),.UNSPECIFIED.)
CURVE()
GEOMETRIC_REPRESENTATION_ITEM()
RATIONAL_B_SPLINE_CURVE((1.,1.00090979171261,1.00093939180057))
REPRESENTATION_ITEM('')
);
#219=(
BOUNDED_CURVE()
B_SPLINE_CURVE(2,(#50165,#50166,#50167),.UNSPECIFIED.,.F.,.F.)
B_SPLINE_CURVE_WITH_KNOTS((3,3),(0.022587909800501,0.0437523366271109),
 .UNSPECIFIED.)
CURVE()
GEOMETRIC_REPRESENTATION_ITEM()
RATIONAL_B_SPLINE_CURVE((1.00093939180006,1.00090979171211,1.))
REPRESENTATION_ITEM('')
);
#220=(
BOUNDED_CURVE()
B_SPLINE_CURVE(2,(#50174,#50175,#50176),.UNSPECIFIED.,.F.,.F.)
B_SPLINE_CURVE_WITH_KNOTS((3,3),(0.,0.0211644268266066),.UNSPECIFIED.)
CURVE()
GEOMETRIC_REPRESENTATION_ITEM()
RATIONAL_B_SPLINE_CURVE((1.,1.00090979171135,1.00093939179927))
REPRESENTATION_ITEM('')
);
#221=(
BOUNDED_CURVE()
B_SPLINE_CURVE(2,(#50179,#50180,#50181),.UNSPECIFIED.,.F.,.F.)
B_SPLINE_CURVE_WITH_KNOTS((3,3),(0.0225879098005609,0.0437523366271108),
 .UNSPECIFIED.)
CURVE()
GEOMETRIC_REPRESENTATION_ITEM()
RATIONAL_B_SPLINE_CURVE((1.00093939180654,1.00090979171839,1.))
REPRESENTATION_ITEM('')
);
#222=(
BOUNDED_CURVE()
B_SPLINE_CURVE(2,(#50188,#50189,#50190),.UNSPECIFIED.,.F.,.F.)
B_SPLINE_CURVE_WITH_KNOTS((3,3),(0.,0.0211644268266203),.UNSPECIFIED.)
CURVE()
GEOMETRIC_REPRESENTATION_ITEM()
RATIONAL_B_SPLINE_CURVE((1.,1.00090979171634,1.00093939180443))
REPRESENTATION_ITEM('')
);
#223=(
BOUNDED_CURVE()
B_SPLINE_CURVE(2,(#50193,#50194,#50195),.UNSPECIFIED.,.F.,.F.)
B_SPLINE_CURVE_WITH_KNOTS((3,3),(0.0225879098005457,0.0437523366271109),
 .UNSPECIFIED.)
CURVE()
GEOMETRIC_REPRESENTATION_ITEM()
RATIONAL_B_SPLINE_CURVE((1.00093939180273,1.0009097917147,1.))
REPRESENTATION_ITEM('')
);
#224=(
BOUNDED_CURVE()
B_SPLINE_CURVE(2,(#50202,#50203,#50204),.UNSPECIFIED.,.F.,.F.)
B_SPLINE_CURVE_WITH_KNOTS((3,3),(0.,0.0211644268265952),.UNSPECIFIED.)
CURVE()
GEOMETRIC_REPRESENTATION_ITEM()
RATIONAL_B_SPLINE_CURVE((1.,1.00090979171439,1.00093939180241))
REPRESENTATION_ITEM('')
);
#225=(
BOUNDED_CURVE()
B_SPLINE_CURVE(2,(#50207,#50208,#50209),.UNSPECIFIED.,.F.,.F.)
B_SPLINE_CURVE_WITH_KNOTS((3,3),(0.0225879098005205,0.0437523366271109),
 .UNSPECIFIED.)
CURVE()
GEOMETRIC_REPRESENTATION_ITEM()
RATIONAL_B_SPLINE_CURVE((1.00093939180427,1.00090979171619,1.))
REPRESENTATION_ITEM('')
);
#226=(
BOUNDED_CURVE()
B_SPLINE_CURVE(2,(#50216,#50217,#50218),.UNSPECIFIED.,.F.,.F.)
B_SPLINE_CURVE_WITH_KNOTS((3,3),(0.,0.0211644268265894),.UNSPECIFIED.)
CURVE()
GEOMETRIC_REPRESENTATION_ITEM()
RATIONAL_B_SPLINE_CURVE((1.,1.00090979171495,1.00093939180299))
REPRESENTATION_ITEM('')
);
#227=(
BOUNDED_CURVE()
B_SPLINE_CURVE(2,(#50221,#50222,#50223),.UNSPECIFIED.,.F.,.F.)
B_SPLINE_CURVE_WITH_KNOTS((3,3),(0.0225879098005011,0.0437523366271109),
 .UNSPECIFIED.)
CURVE()
GEOMETRIC_REPRESENTATION_ITEM()
RATIONAL_B_SPLINE_CURVE((1.00093939180012,1.00090979171217,1.))
REPRESENTATION_ITEM('')
);
#228=(
BOUNDED_CURVE()
B_SPLINE_CURVE(2,(#50230,#50231,#50232),.UNSPECIFIED.,.F.,.F.)
B_SPLINE_CURVE_WITH_KNOTS((3,3),(0.,0.0211644268265743),.UNSPECIFIED.)
CURVE()
GEOMETRIC_REPRESENTATION_ITEM()
RATIONAL_B_SPLINE_CURVE((1.,1.00090979171694,1.00093939180504))
REPRESENTATION_ITEM('')
);
#229=(
BOUNDED_CURVE()
B_SPLINE_CURVE(2,(#50235,#50236,#50237),.UNSPECIFIED.,.F.,.F.)
B_SPLINE_CURVE_WITH_KNOTS((3,3),(0.0225879098005504,0.0437523366271109),
 .UNSPECIFIED.)
CURVE()
GEOMETRIC_REPRESENTATION_ITEM()
RATIONAL_B_SPLINE_CURVE((1.00093939180379,1.00090979171572,1.))
REPRESENTATION_ITEM('')
);
#230=(
BOUNDED_CURVE()
B_SPLINE_CURVE(2,(#50244,#50245,#50246),.UNSPECIFIED.,.F.,.F.)
B_SPLINE_CURVE_WITH_KNOTS((3,3),(0.,0.0211644268265842),.UNSPECIFIED.)
CURVE()
GEOMETRIC_REPRESENTATION_ITEM()
RATIONAL_B_SPLINE_CURVE((1.,1.00090979171899,1.00093939180716))
REPRESENTATION_ITEM('')
);
#231=(
BOUNDED_CURVE()
B_SPLINE_CURVE(2,(#50249,#50250,#50251),.UNSPECIFIED.,.F.,.F.)
B_SPLINE_CURVE_WITH_KNOTS((3,3),(0.0225879098005829,0.0437523366271109),
 .UNSPECIFIED.)
CURVE()
GEOMETRIC_REPRESENTATION_ITEM()
RATIONAL_B_SPLINE_CURVE((1.00093939180477,1.00090979171667,1.))
REPRESENTATION_ITEM('')
);
#232=(
BOUNDED_CURVE()
B_SPLINE_CURVE(2,(#50258,#50259,#50260),.UNSPECIFIED.,.F.,.F.)
B_SPLINE_CURVE_WITH_KNOTS((3,3),(0.,0.0211644268266254),.UNSPECIFIED.)
CURVE()
GEOMETRIC_REPRESENTATION_ITEM()
RATIONAL_B_SPLINE_CURVE((1.,1.00090979171259,1.00093939180055))
REPRESENTATION_ITEM('')
);
#233=(
BOUNDED_CURVE()
B_SPLINE_CURVE(2,(#50263,#50264,#50265),.UNSPECIFIED.,.F.,.F.)
B_SPLINE_CURVE_WITH_KNOTS((3,3),(0.0225879098005341,0.0437523366271108),
 .UNSPECIFIED.)
CURVE()
GEOMETRIC_REPRESENTATION_ITEM()
RATIONAL_B_SPLINE_CURVE((1.00093939180657,1.00090979171842,1.))
REPRESENTATION_ITEM('')
);
#234=(
BOUNDED_CURVE()
B_SPLINE_CURVE(2,(#50272,#50273,#50274),.UNSPECIFIED.,.F.,.F.)
B_SPLINE_CURVE_WITH_KNOTS((3,3),(0.,0.0211644268265998),.UNSPECIFIED.)
CURVE()
GEOMETRIC_REPRESENTATION_ITEM()
RATIONAL_B_SPLINE_CURVE((1.,1.00090979171367,1.00093939180166))
REPRESENTATION_ITEM('')
);
#235=(
BOUNDED_CURVE()
B_SPLINE_CURVE(2,(#50277,#50278,#50279),.UNSPECIFIED.,.F.,.F.)
B_SPLINE_CURVE_WITH_KNOTS((3,3),(0.0225879098005594,0.0437523366271109),
 .UNSPECIFIED.)
CURVE()
GEOMETRIC_REPRESENTATION_ITEM()
RATIONAL_B_SPLINE_CURVE((1.00093939180571,1.00090979171758,1.))
REPRESENTATION_ITEM('')
);
#236=(
BOUNDED_CURVE()
B_SPLINE_CURVE(2,(#50286,#50287,#50288),.UNSPECIFIED.,.F.,.F.)
B_SPLINE_CURVE_WITH_KNOTS((3,3),(0.,0.0211644268265771),.UNSPECIFIED.)
CURVE()
GEOMETRIC_REPRESENTATION_ITEM()
RATIONAL_B_SPLINE_CURVE((1.,1.00090979171472,1.00093939180275))
REPRESENTATION_ITEM('')
);
#237=(
BOUNDED_CURVE()
B_SPLINE_CURVE(2,(#50291,#50292,#50293),.UNSPECIFIED.,.F.,.F.)
B_SPLINE_CURVE_WITH_KNOTS((3,3),(0.0225879098005193,0.0437523366271108),
 .UNSPECIFIED.)
CURVE()
GEOMETRIC_REPRESENTATION_ITEM()
RATIONAL_B_SPLINE_CURVE((1.00093939180378,1.00090979171571,1.))
REPRESENTATION_ITEM('')
);
#238=(
BOUNDED_CURVE()
B_SPLINE_CURVE(2,(#50300,#50301,#50302),.UNSPECIFIED.,.F.,.F.)
B_SPLINE_CURVE_WITH_KNOTS((3,3),(0.,0.0211644268265921),.UNSPECIFIED.)
CURVE()
GEOMETRIC_REPRESENTATION_ITEM()
RATIONAL_B_SPLINE_CURVE((1.,1.00090979171676,1.00093939180485))
REPRESENTATION_ITEM('')
);
#239=(
BOUNDED_CURVE()
B_SPLINE_CURVE(2,(#50305,#50306,#50307),.UNSPECIFIED.,.F.,.F.)
B_SPLINE_CURVE_WITH_KNOTS((3,3),(0.0225879098004847,0.0437523366271108),
 .UNSPECIFIED.)
CURVE()
GEOMETRIC_REPRESENTATION_ITEM()
RATIONAL_B_SPLINE_CURVE((1.00093939180062,1.00090979171266,1.))
REPRESENTATION_ITEM('')
);
#240=(
BOUNDED_CURVE()
B_SPLINE_CURVE(2,(#50314,#50315,#50316),.UNSPECIFIED.,.F.,.F.)
B_SPLINE_CURVE_WITH_KNOTS((3,3),(0.,0.0211644268265503),.UNSPECIFIED.)
CURVE()
GEOMETRIC_REPRESENTATION_ITEM()
RATIONAL_B_SPLINE_CURVE((1.,1.00090979171894,1.00093939180711))
REPRESENTATION_ITEM('')
);
#241=(
BOUNDED_CURVE()
B_SPLINE_CURVE(2,(#50319,#50320,#50321),.UNSPECIFIED.,.F.,.F.)
B_SPLINE_CURVE_WITH_KNOTS((3,3),(0.022587909800518,0.0437523366271109),
 .UNSPECIFIED.)
CURVE()
GEOMETRIC_REPRESENTATION_ITEM()
RATIONAL_B_SPLINE_CURVE((1.00093939180195,1.00090979171394,1.))
REPRESENTATION_ITEM('')
);
#242=(
BOUNDED_CURVE()
B_SPLINE_CURVE(2,(#50328,#50329,#50330),.UNSPECIFIED.,.F.,.F.)
B_SPLINE_CURVE_WITH_KNOTS((3,3),(0.,0.0211644268265849),.UNSPECIFIED.)
CURVE()
GEOMETRIC_REPRESENTATION_ITEM()
RATIONAL_B_SPLINE_CURVE((1.,1.00090979171243,1.00093939180038))
REPRESENTATION_ITEM('')
);
#243=(
BOUNDED_CURVE()
B_SPLINE_CURVE(2,(#50333,#50334,#50335),.UNSPECIFIED.,.F.,.F.)
B_SPLINE_CURVE_WITH_KNOTS((3,3),(0.0225879098005176,0.0437523366271109),
 .UNSPECIFIED.)
CURVE()
GEOMETRIC_REPRESENTATION_ITEM()
RATIONAL_B_SPLINE_CURVE((1.00093939180297,1.00090979171494,1.))
REPRESENTATION_ITEM('')
);
#244=(
BOUNDED_CURVE()
B_SPLINE_CURVE(2,(#50342,#50343,#50344),.UNSPECIFIED.,.F.,.F.)
B_SPLINE_CURVE_WITH_KNOTS((3,3),(0.,0.0211644268266227),.UNSPECIFIED.)
CURVE()
GEOMETRIC_REPRESENTATION_ITEM()
RATIONAL_B_SPLINE_CURVE((1.,1.00090979171573,1.00093939180379))
REPRESENTATION_ITEM('')
);
#245=(
BOUNDED_CURVE()
B_SPLINE_CURVE(2,(#50347,#50348,#50349),.UNSPECIFIED.,.F.,.F.)
B_SPLINE_CURVE_WITH_KNOTS((3,3),(0.0225879098005391,0.0437523366271109),
 .UNSPECIFIED.)
CURVE()
GEOMETRIC_REPRESENTATION_ITEM()
RATIONAL_B_SPLINE_CURVE((1.00093939180643,1.00090979171828,1.))
REPRESENTATION_ITEM('')
);
#246=(
BOUNDED_CURVE()
B_SPLINE_CURVE(2,(#50356,#50357,#50358),.UNSPECIFIED.,.F.,.F.)
B_SPLINE_CURVE_WITH_KNOTS((3,3),(0.,0.0211644268265862),.UNSPECIFIED.)
CURVE()
GEOMETRIC_REPRESENTATION_ITEM()
RATIONAL_B_SPLINE_CURVE((1.,1.00090979171409,1.0009393918021))
REPRESENTATION_ITEM('')
);
#247=(
BOUNDED_CURVE()
B_SPLINE_CURVE(2,(#50361,#50362,#50363),.UNSPECIFIED.,.F.,.F.)
B_SPLINE_CURVE_WITH_KNOTS((3,3),(0.0225879098005106,0.0437523366271109),
 .UNSPECIFIED.)
CURVE()
GEOMETRIC_REPRESENTATION_ITEM()
RATIONAL_B_SPLINE_CURVE((1.0009393918006,1.00090979171264,1.))
REPRESENTATION_ITEM('')
);
#248=(
BOUNDED_CURVE()
B_SPLINE_CURVE(2,(#50370,#50371,#50372),.UNSPECIFIED.,.F.,.F.)
B_SPLINE_CURVE_WITH_KNOTS((3,3),(0.,0.0211644268265897),.UNSPECIFIED.)
CURVE()
GEOMETRIC_REPRESENTATION_ITEM()
RATIONAL_B_SPLINE_CURVE((1.,1.00090979171702,1.00093939180512))
REPRESENTATION_ITEM('')
);
#249=(
BOUNDED_CURVE()
B_SPLINE_CURVE(2,(#50375,#50376,#50377),.UNSPECIFIED.,.F.,.F.)
B_SPLINE_CURVE_WITH_KNOTS((3,3),(0.0225879098004859,0.0437523366271109),
 .UNSPECIFIED.)
CURVE()
GEOMETRIC_REPRESENTATION_ITEM()
RATIONAL_B_SPLINE_CURVE((1.0009393918034,1.00090979171535,1.))
REPRESENTATION_ITEM('')
);
#250=(
BOUNDED_CURVE()
B_SPLINE_CURVE(2,(#50384,#50385,#50386),.UNSPECIFIED.,.F.,.F.)
B_SPLINE_CURVE_WITH_KNOTS((3,3),(0.,0.021164426826622),.UNSPECIFIED.)
CURVE()
GEOMETRIC_REPRESENTATION_ITEM()
RATIONAL_B_SPLINE_CURVE((1.,1.0009097917149,1.00093939180294))
REPRESENTATION_ITEM('')
);
#251=(
BOUNDED_CURVE()
B_SPLINE_CURVE(2,(#50389,#50390,#50391),.UNSPECIFIED.,.F.,.F.)
B_SPLINE_CURVE_WITH_KNOTS((3,3),(0.0225879098005208,0.0437523366271109),
 .UNSPECIFIED.)
CURVE()
GEOMETRIC_REPRESENTATION_ITEM()
RATIONAL_B_SPLINE_CURVE((1.00093939180214,1.00090979171413,1.))
REPRESENTATION_ITEM('')
);
#252=(
BOUNDED_CURVE()
B_SPLINE_CURVE(2,(#50398,#50399,#50400),.UNSPECIFIED.,.F.,.F.)
B_SPLINE_CURVE_WITH_KNOTS((3,3),(0.,0.021164426826624),.UNSPECIFIED.)
CURVE()
GEOMETRIC_REPRESENTATION_ITEM()
RATIONAL_B_SPLINE_CURVE((1.,1.00090979171573,1.00093939180379))
REPRESENTATION_ITEM('')
);
#253=(
BOUNDED_CURVE()
B_SPLINE_CURVE(2,(#50403,#50404,#50405),.UNSPECIFIED.,.F.,.F.)
B_SPLINE_CURVE_WITH_KNOTS((3,3),(0.0225879098005246,0.0437523366271109),
 .UNSPECIFIED.)
CURVE()
GEOMETRIC_REPRESENTATION_ITEM()
RATIONAL_B_SPLINE_CURVE((1.00093939179848,1.00090979171058,1.))
REPRESENTATION_ITEM('')
);
#254=(
BOUNDED_CURVE()
B_SPLINE_CURVE(2,(#50412,#50413,#50414),.UNSPECIFIED.,.F.,.F.)
B_SPLINE_CURVE_WITH_KNOTS((3,3),(0.,0.0211644268266093),.UNSPECIFIED.)
CURVE()
GEOMETRIC_REPRESENTATION_ITEM()
RATIONAL_B_SPLINE_CURVE((1.,1.00090979171292,1.00093939180089))
REPRESENTATION_ITEM('')
);
#255=(
BOUNDED_CURVE()
B_SPLINE_CURVE(2,(#50417,#50418,#50419),.UNSPECIFIED.,.F.,.F.)
B_SPLINE_CURVE_WITH_KNOTS((3,3),(0.0225879098005556,0.0437523366271108),
 .UNSPECIFIED.)
CURVE()
GEOMETRIC_REPRESENTATION_ITEM()
RATIONAL_B_SPLINE_CURVE((1.00093939180208,1.00090979171407,1.))
REPRESENTATION_ITEM('')
);
#256=(
BOUNDED_CURVE()
B_SPLINE_CURVE(2,(#50426,#50427,#50428),.UNSPECIFIED.,.F.,.F.)
B_SPLINE_CURVE_WITH_KNOTS((3,3),(0.,0.0211644268265253),.UNSPECIFIED.)
CURVE()
GEOMETRIC_REPRESENTATION_ITEM()
RATIONAL_B_SPLINE_CURVE((1.,1.00090979171634,1.00093939180442))
REPRESENTATION_ITEM('')
);
#257=(
BOUNDED_CURVE()
B_SPLINE_CURVE(2,(#50431,#50432,#50433),.UNSPECIFIED.,.F.,.F.)
B_SPLINE_CURVE_WITH_KNOTS((3,3),(0.0225879098004964,0.0437523366271109),
 .UNSPECIFIED.)
CURVE()
GEOMETRIC_REPRESENTATION_ITEM()
RATIONAL_B_SPLINE_CURVE((1.00093939180221,1.00090979171419,1.))
REPRESENTATION_ITEM('')
);
#258=(
BOUNDED_CURVE()
B_SPLINE_CURVE(2,(#50440,#50441,#50442),.UNSPECIFIED.,.F.,.F.)
B_SPLINE_CURVE_WITH_KNOTS((3,3),(0.,0.0211644268265929),.UNSPECIFIED.)
CURVE()
GEOMETRIC_REPRESENTATION_ITEM()
RATIONAL_B_SPLINE_CURVE((1.,1.00090979171394,1.00093939180195))
REPRESENTATION_ITEM('')
);
#259=(
BOUNDED_CURVE()
B_SPLINE_CURVE(2,(#50445,#50446,#50447),.UNSPECIFIED.,.F.,.F.)
B_SPLINE_CURVE_WITH_KNOTS((3,3),(0.0225879098005457,0.0437523366271109),
 .UNSPECIFIED.)
CURVE()
GEOMETRIC_REPRESENTATION_ITEM()
RATIONAL_B_SPLINE_CURVE((1.00093939180273,1.0009097917147,1.))
REPRESENTATION_ITEM('')
);
#260=(
BOUNDED_CURVE()
B_SPLINE_CURVE(2,(#50454,#50455,#50456),.UNSPECIFIED.,.F.,.F.)
B_SPLINE_CURVE_WITH_KNOTS((3,3),(0.,0.0211644268265952),.UNSPECIFIED.)
CURVE()
GEOMETRIC_REPRESENTATION_ITEM()
RATIONAL_B_SPLINE_CURVE((1.,1.00090979171439,1.00093939180241))
REPRESENTATION_ITEM('')
);
#261=(
BOUNDED_CURVE()
B_SPLINE_CURVE(2,(#50459,#50460,#50461),.UNSPECIFIED.,.F.,.F.)
B_SPLINE_CURVE_WITH_KNOTS((3,3),(0.0225879098005144,0.0437523366271109),
 .UNSPECIFIED.)
CURVE()
GEOMETRIC_REPRESENTATION_ITEM()
RATIONAL_B_SPLINE_CURVE((1.00093939180272,1.00090979171469,1.))
REPRESENTATION_ITEM('')
);
#262=(
BOUNDED_CURVE()
B_SPLINE_CURVE(2,(#50468,#50469,#50470),.UNSPECIFIED.,.F.,.F.)
B_SPLINE_CURVE_WITH_KNOTS((3,3),(0.,0.0211644268265596),.UNSPECIFIED.)
CURVE()
GEOMETRIC_REPRESENTATION_ITEM()
RATIONAL_B_SPLINE_CURVE((1.,1.00090979171197,1.00093939179992))
REPRESENTATION_ITEM('')
);
#263=(
BOUNDED_CURVE()
B_SPLINE_CURVE(2,(#50473,#50474,#50475),.UNSPECIFIED.,.F.,.F.)
B_SPLINE_CURVE_WITH_KNOTS((3,3),(0.0225879098005319,0.0437523366271109),
 .UNSPECIFIED.)
CURVE()
GEOMETRIC_REPRESENTATION_ITEM()
RATIONAL_B_SPLINE_CURVE((1.00093939180304,1.000909791715,1.))
REPRESENTATION_ITEM('')
);
#264=(
BOUNDED_CURVE()
B_SPLINE_CURVE(2,(#50482,#50483,#50484),.UNSPECIFIED.,.F.,.F.)
B_SPLINE_CURVE_WITH_KNOTS((3,3),(0.,0.0211644268266268),.UNSPECIFIED.)
CURVE()
GEOMETRIC_REPRESENTATION_ITEM()
RATIONAL_B_SPLINE_CURVE((1.,1.00090979171561,1.00093939180367))
REPRESENTATION_ITEM('')
);
#265=(
BOUNDED_CURVE()
B_SPLINE_CURVE(2,(#50487,#50488,#50489),.UNSPECIFIED.,.F.,.F.)
B_SPLINE_CURVE_WITH_KNOTS((3,3),(0.0225879098005574,0.0437523366271109),
 .UNSPECIFIED.)
CURVE()
GEOMETRIC_REPRESENTATION_ITEM()
RATIONAL_B_SPLINE_CURVE((1.00093939180693,1.00090979171876,1.))
REPRESENTATION_ITEM('')
);
#266=(
BOUNDED_CURVE()
B_SPLINE_CURVE(2,(#50496,#50497,#50498),.UNSPECIFIED.,.F.,.F.)
B_SPLINE_CURVE_WITH_KNOTS((3,3),(0.,0.0211644268265904),.UNSPECIFIED.)
CURVE()
GEOMETRIC_REPRESENTATION_ITEM()
RATIONAL_B_SPLINE_CURVE((1.,1.0009097917121,1.00093939180005))
REPRESENTATION_ITEM('')
);
#267=(
BOUNDED_CURVE()
B_SPLINE_CURVE(2,(#50501,#50502,#50503),.UNSPECIFIED.,.F.,.F.)
B_SPLINE_CURVE_WITH_KNOTS((3,3),(0.0225879098005213,0.0437523366271109),
 .UNSPECIFIED.)
CURVE()
GEOMETRIC_REPRESENTATION_ITEM()
RATIONAL_B_SPLINE_CURVE((1.00093939180114,1.00090979171316,1.))
REPRESENTATION_ITEM('')
);
#268=(
BOUNDED_CURVE()
B_SPLINE_CURVE(2,(#50510,#50511,#50512),.UNSPECIFIED.,.F.,.F.)
B_SPLINE_CURVE_WITH_KNOTS((3,3),(0.,0.0211644268266229),.UNSPECIFIED.)
CURVE()
GEOMETRIC_REPRESENTATION_ITEM()
RATIONAL_B_SPLINE_CURVE((1.,1.00090979171429,1.00093939180231))
REPRESENTATION_ITEM('')
);
#269=(
BOUNDED_CURVE()
B_SPLINE_CURVE(2,(#50525,#50526,#50527),.UNSPECIFIED.,.F.,.F.)
B_SPLINE_CURVE_WITH_KNOTS((3,3),(0.,0.0126130588257639),.UNSPECIFIED.)
CURVE()
GEOMETRIC_REPRESENTATION_ITEM()
RATIONAL_B_SPLINE_CURVE((1.,1.00234596681253,1.0032929802757))
REPRESENTATION_ITEM('')
);
#270=(
BOUNDED_CURVE()
B_SPLINE_CURVE(2,(#50531,#50532,#50533),.UNSPECIFIED.,.F.,.F.)
B_SPLINE_CURVE_WITH_KNOTS((3,3),(0.0296897347922131,0.0423027936179769),
 .UNSPECIFIED.)
CURVE()
GEOMETRIC_REPRESENTATION_ITEM()
RATIONAL_B_SPLINE_CURVE((1.00329298027569,1.00234596681253,1.))
REPRESENTATION_ITEM('')
);
#271=(
BOUNDED_CURVE()
B_SPLINE_CURVE(2,(#50535,#50536,#50537),.UNSPECIFIED.,.F.,.F.)
B_SPLINE_CURVE_WITH_KNOTS((3,3),(0.,0.0126130588257639),.UNSPECIFIED.)
CURVE()
GEOMETRIC_REPRESENTATION_ITEM()
RATIONAL_B_SPLINE_CURVE((1.,1.00234596681251,1.00329298027567))
REPRESENTATION_ITEM('')
);
#272=(
BOUNDED_CURVE()
B_SPLINE_CURVE(2,(#50541,#50542,#50543),.UNSPECIFIED.,.F.,.F.)
B_SPLINE_CURVE_WITH_KNOTS((3,3),(0.0296897347922128,0.0423027936179769),
 .UNSPECIFIED.)
CURVE()
GEOMETRIC_REPRESENTATION_ITEM()
RATIONAL_B_SPLINE_CURVE((1.00329298027567,1.00234596681251,1.))
REPRESENTATION_ITEM('')
);
#273=(
BOUNDED_CURVE()
B_SPLINE_CURVE(2,(#50545,#50546,#50547),.UNSPECIFIED.,.F.,.F.)
B_SPLINE_CURVE_WITH_KNOTS((3,3),(0.,0.0126130588257636),.UNSPECIFIED.)
CURVE()
GEOMETRIC_REPRESENTATION_ITEM()
RATIONAL_B_SPLINE_CURVE((1.,1.00234596681253,1.00329298027569))
REPRESENTATION_ITEM('')
);
#274=(
BOUNDED_CURVE()
B_SPLINE_CURVE(2,(#50551,#50552,#50553),.UNSPECIFIED.,.F.,.F.)
B_SPLINE_CURVE_WITH_KNOTS((3,3),(0.0296897347922129,0.0423027936179769),
 .UNSPECIFIED.)
CURVE()
GEOMETRIC_REPRESENTATION_ITEM()
RATIONAL_B_SPLINE_CURVE((1.00329298027566,1.0023459668125,1.))
REPRESENTATION_ITEM('')
);
#275=(
BOUNDED_CURVE()
B_SPLINE_CURVE(2,(#50555,#50556,#50557),.UNSPECIFIED.,.F.,.F.)
B_SPLINE_CURVE_WITH_KNOTS((3,3),(0.,0.0126130588257639),.UNSPECIFIED.)
CURVE()
GEOMETRIC_REPRESENTATION_ITEM()
RATIONAL_B_SPLINE_CURVE((1.,1.00234596681251,1.00329298027567))
REPRESENTATION_ITEM('')
);
#276=(
BOUNDED_CURVE()
B_SPLINE_CURVE(2,(#50561,#50562,#50563),.UNSPECIFIED.,.F.,.F.)
B_SPLINE_CURVE_WITH_KNOTS((3,3),(0.0296897347922131,0.0423027936179769),
 .UNSPECIFIED.)
CURVE()
GEOMETRIC_REPRESENTATION_ITEM()
RATIONAL_B_SPLINE_CURVE((1.00329298027568,1.00234596681252,1.))
REPRESENTATION_ITEM('')
);
#277=(
BOUNDED_CURVE()
B_SPLINE_CURVE(2,(#50565,#50566,#50567),.UNSPECIFIED.,.F.,.F.)
B_SPLINE_CURVE_WITH_KNOTS((3,3),(0.,0.0126130588257641),.UNSPECIFIED.)
CURVE()
GEOMETRIC_REPRESENTATION_ITEM()
RATIONAL_B_SPLINE_CURVE((1.,1.00234596681251,1.00329298027567))
REPRESENTATION_ITEM('')
);
#278=(
BOUNDED_CURVE()
B_SPLINE_CURVE(2,(#50571,#50572,#50573),.UNSPECIFIED.,.F.,.F.)
B_SPLINE_CURVE_WITH_KNOTS((3,3),(0.0296897347922131,0.0423027936179769),
 .UNSPECIFIED.)
CURVE()
GEOMETRIC_REPRESENTATION_ITEM()
RATIONAL_B_SPLINE_CURVE((1.0032929802757,1.00234596681253,1.))
REPRESENTATION_ITEM('')
);
#279=(
BOUNDED_CURVE()
B_SPLINE_CURVE(2,(#50575,#50576,#50577),.UNSPECIFIED.,.F.,.F.)
B_SPLINE_CURVE_WITH_KNOTS((3,3),(0.,0.0126130588257639),.UNSPECIFIED.)
CURVE()
GEOMETRIC_REPRESENTATION_ITEM()
RATIONAL_B_SPLINE_CURVE((1.,1.00234596681251,1.00329298027567))
REPRESENTATION_ITEM('')
);
#280=(
BOUNDED_CURVE()
B_SPLINE_CURVE(2,(#50580,#50581,#50582),.UNSPECIFIED.,.F.,.F.)
B_SPLINE_CURVE_WITH_KNOTS((3,3),(0.029689734792213,0.0423027936179769),
 .UNSPECIFIED.)
CURVE()
GEOMETRIC_REPRESENTATION_ITEM()
RATIONAL_B_SPLINE_CURVE((1.00329298027566,1.00234596681251,1.))
REPRESENTATION_ITEM('')
);
#281=(
BOUNDED_CURVE()
B_SPLINE_CURVE(2,(#58539,#58540,#58541),.UNSPECIFIED.,.F.,.F.)
B_SPLINE_CURVE_WITH_KNOTS((3,3),(0.,0.0169283274324264),.UNSPECIFIED.)
CURVE()
GEOMETRIC_REPRESENTATION_ITEM()
RATIONAL_B_SPLINE_CURVE((1.,1.00067437544971,1.00082963690249))
REPRESENTATION_ITEM('')
);
#282=(
BOUNDED_CURVE()
B_SPLINE_CURVE(2,(#58546,#58547,#58548),.UNSPECIFIED.,.F.,.F.)
B_SPLINE_CURVE_WITH_KNOTS((3,3),(0.0270544913418749,0.0439828187741895),
 .UNSPECIFIED.)
CURVE()
GEOMETRIC_REPRESENTATION_ITEM()
RATIONAL_B_SPLINE_CURVE((1.00082963691396,1.00067437545903,1.))
REPRESENTATION_ITEM('')
);
#283=(
BOUNDED_CURVE()
B_SPLINE_CURVE(2,(#58555,#58556,#58557),.UNSPECIFIED.,.F.,.F.)
B_SPLINE_CURVE_WITH_KNOTS((3,3),(0.0270544913418551,0.0439828187741901),
 .UNSPECIFIED.)
CURVE()
GEOMETRIC_REPRESENTATION_ITEM()
RATIONAL_B_SPLINE_CURVE((1.0008296369069,1.0006743754533,1.))
REPRESENTATION_ITEM('')
);
#284=(
BOUNDED_CURVE()
B_SPLINE_CURVE(2,(#58561,#58562,#58563),.UNSPECIFIED.,.F.,.F.)
B_SPLINE_CURVE_WITH_KNOTS((3,3),(0.,0.0169283274323742),.UNSPECIFIED.)
CURVE()
GEOMETRIC_REPRESENTATION_ITEM()
RATIONAL_B_SPLINE_CURVE((1.,1.00067437545167,1.0008296369049))
REPRESENTATION_ITEM('')
);
#285=(
BOUNDED_CURVE()
B_SPLINE_CURVE(2,(#58565,#58566,#58567),.UNSPECIFIED.,.F.,.F.)
B_SPLINE_CURVE_WITH_KNOTS((3,3),(0.0270544913418838,0.0439828187741893),
 .UNSPECIFIED.)
CURVE()
GEOMETRIC_REPRESENTATION_ITEM()
RATIONAL_B_SPLINE_CURVE((1.00082963690705,1.00067437545341,1.))
REPRESENTATION_ITEM('')
);
#286=(
BOUNDED_CURVE()
B_SPLINE_CURVE(2,(#58571,#58572,#58573),.UNSPECIFIED.,.F.,.F.)
B_SPLINE_CURVE_WITH_KNOTS((3,3),(0.,0.0169283274323636),.UNSPECIFIED.)
CURVE()
GEOMETRIC_REPRESENTATION_ITEM()
RATIONAL_B_SPLINE_CURVE((1.,1.00067437545192,1.00082963690521))
REPRESENTATION_ITEM('')
);
#287=(
BOUNDED_CURVE()
B_SPLINE_CURVE(2,(#58575,#58576,#58577),.UNSPECIFIED.,.F.,.F.)
B_SPLINE_CURVE_WITH_KNOTS((3,3),(0.0270544913418794,0.0439828187741893),
 .UNSPECIFIED.)
CURVE()
GEOMETRIC_REPRESENTATION_ITEM()
RATIONAL_B_SPLINE_CURVE((1.00082963691317,1.00067437545839,1.))
REPRESENTATION_ITEM('')
);
#288=(
BOUNDED_CURVE()
B_SPLINE_CURVE(2,(#58581,#58582,#58583),.UNSPECIFIED.,.F.,.F.)
B_SPLINE_CURVE_WITH_KNOTS((3,3),(0.,0.0169283274323019),.UNSPECIFIED.)
CURVE()
GEOMETRIC_REPRESENTATION_ITEM()
RATIONAL_B_SPLINE_CURVE((1.,1.0006743754572,1.00082963691171))
REPRESENTATION_ITEM('')
);
#289=(
BOUNDED_CURVE()
B_SPLINE_CURVE(2,(#58585,#58586,#58587),.UNSPECIFIED.,.F.,.F.)
B_SPLINE_CURVE_WITH_KNOTS((3,3),(0.0270544913418195,0.0439828187741896),
 .UNSPECIFIED.)
CURVE()
GEOMETRIC_REPRESENTATION_ITEM()
RATIONAL_B_SPLINE_CURVE((1.00082963691305,1.00067437545829,1.))
REPRESENTATION_ITEM('')
);
#290=(
BOUNDED_CURVE()
B_SPLINE_CURVE(2,(#58591,#58592,#58593),.UNSPECIFIED.,.F.,.F.)
B_SPLINE_CURVE_WITH_KNOTS((3,3),(0.,0.0169283274324256),.UNSPECIFIED.)
CURVE()
GEOMETRIC_REPRESENTATION_ITEM()
RATIONAL_B_SPLINE_CURVE((1.,1.00067437545036,1.00082963690329))
REPRESENTATION_ITEM('')
);
#291=(
BOUNDED_CURVE()
B_SPLINE_CURVE(2,(#58595,#58596,#58597),.UNSPECIFIED.,.F.,.F.)
B_SPLINE_CURVE_WITH_KNOTS((3,3),(0.0270544913418591,0.0439828187741892),
 .UNSPECIFIED.)
CURVE()
GEOMETRIC_REPRESENTATION_ITEM()
RATIONAL_B_SPLINE_CURVE((1.0008296369132,1.00067437545842,1.))
REPRESENTATION_ITEM('')
);
#292=(
BOUNDED_CURVE()
B_SPLINE_CURVE(2,(#58601,#58602,#58603),.UNSPECIFIED.,.F.,.F.)
B_SPLINE_CURVE_WITH_KNOTS((3,3),(0.,0.0169283274324107),.UNSPECIFIED.)
CURVE()
GEOMETRIC_REPRESENTATION_ITEM()
RATIONAL_B_SPLINE_CURVE((1.,1.00067437544792,1.00082963690028))
REPRESENTATION_ITEM('')
);
#293=(
BOUNDED_CURVE()
B_SPLINE_CURVE(2,(#58605,#58606,#58607),.UNSPECIFIED.,.F.,.F.)
B_SPLINE_CURVE_WITH_KNOTS((3,3),(0.0270544913419236,0.0439828187741892),
 .UNSPECIFIED.)
CURVE()
GEOMETRIC_REPRESENTATION_ITEM()
RATIONAL_B_SPLINE_CURVE((1.00082963691831,1.00067437546256,1.))
REPRESENTATION_ITEM('')
);
#294=(
BOUNDED_CURVE()
B_SPLINE_CURVE(2,(#58611,#58612,#58613),.UNSPECIFIED.,.F.,.F.)
B_SPLINE_CURVE_WITH_KNOTS((3,3),(0.,0.0169283274324074),.UNSPECIFIED.)
CURVE()
GEOMETRIC_REPRESENTATION_ITEM()
RATIONAL_B_SPLINE_CURVE((1.,1.00067437544939,1.00082963690209))
REPRESENTATION_ITEM('')
);
#295=(
BOUNDED_CURVE()
B_SPLINE_CURVE(2,(#58615,#58616,#58617),.UNSPECIFIED.,.F.,.F.)
B_SPLINE_CURVE_WITH_KNOTS((3,3),(0.0270544913418797,0.0439828187741898),
 .UNSPECIFIED.)
CURVE()
GEOMETRIC_REPRESENTATION_ITEM()
RATIONAL_B_SPLINE_CURVE((1.00082963691791,1.00067437546225,1.))
REPRESENTATION_ITEM('')
);
#296=(
BOUNDED_CURVE()
B_SPLINE_CURVE(2,(#58621,#58622,#58623),.UNSPECIFIED.,.F.,.F.)
B_SPLINE_CURVE_WITH_KNOTS((3,3),(0.,0.0169283274324609),.UNSPECIFIED.)
CURVE()
GEOMETRIC_REPRESENTATION_ITEM()
RATIONAL_B_SPLINE_CURVE((1.,1.00067437544233,1.00082963689341))
REPRESENTATION_ITEM('')
);
#297=(
BOUNDED_CURVE()
B_SPLINE_CURVE(2,(#58625,#58626,#58627),.UNSPECIFIED.,.F.,.F.)
B_SPLINE_CURVE_WITH_KNOTS((3,3),(0.0270544913417432,0.043982818774189),
 .UNSPECIFIED.)
CURVE()
GEOMETRIC_REPRESENTATION_ITEM()
RATIONAL_B_SPLINE_CURVE((1.00082963689481,1.00067437544347,1.))
REPRESENTATION_ITEM('')
);
#298=(
BOUNDED_CURVE()
B_SPLINE_CURVE(2,(#58631,#58632,#58633),.UNSPECIFIED.,.F.,.F.)
B_SPLINE_CURVE_WITH_KNOTS((3,3),(0.,0.0169283274323957),.UNSPECIFIED.)
CURVE()
GEOMETRIC_REPRESENTATION_ITEM()
RATIONAL_B_SPLINE_CURVE((1.,1.00067437545152,1.00082963690471))
REPRESENTATION_ITEM('')
);
#299=(
BOUNDED_CURVE()
B_SPLINE_CURVE(2,(#58635,#58636,#58637),.UNSPECIFIED.,.F.,.F.)
B_SPLINE_CURVE_WITH_KNOTS((3,3),(0.0270544913418118,0.043982818774189),
 .UNSPECIFIED.)
CURVE()
GEOMETRIC_REPRESENTATION_ITEM()
RATIONAL_B_SPLINE_CURVE((1.0008296369071,1.00067437545346,1.))
REPRESENTATION_ITEM('')
);
#300=(
BOUNDED_CURVE()
B_SPLINE_CURVE(2,(#58641,#58642,#58643),.UNSPECIFIED.,.F.,.F.)
B_SPLINE_CURVE_WITH_KNOTS((3,3),(0.,0.0169283274322737),.UNSPECIFIED.)
CURVE()
GEOMETRIC_REPRESENTATION_ITEM()
RATIONAL_B_SPLINE_CURVE((1.,1.00067437546411,1.00082963692021))
REPRESENTATION_ITEM('')
);
#301=(
BOUNDED_CURVE()
B_SPLINE_CURVE(2,(#58645,#58646,#58647),.UNSPECIFIED.,.F.,.F.)
B_SPLINE_CURVE_WITH_KNOTS((3,3),(0.0270544913418171,0.0439828187741889),
 .UNSPECIFIED.)
CURVE()
GEOMETRIC_REPRESENTATION_ITEM()
RATIONAL_B_SPLINE_CURVE((1.00082963690763,1.00067437545389,1.))
REPRESENTATION_ITEM('')
);
#302=(
BOUNDED_CURVE()
B_SPLINE_CURVE(2,(#58651,#58652,#58653),.UNSPECIFIED.,.F.,.F.)
B_SPLINE_CURVE_WITH_KNOTS((3,3),(0.,0.0169283274324309),.UNSPECIFIED.)
CURVE()
GEOMETRIC_REPRESENTATION_ITEM()
RATIONAL_B_SPLINE_CURVE((1.,1.00067437544897,1.00082963690158))
REPRESENTATION_ITEM('')
);
#303=(
BOUNDED_CURVE()
B_SPLINE_CURVE(2,(#58655,#58656,#58657),.UNSPECIFIED.,.F.,.F.)
B_SPLINE_CURVE_WITH_KNOTS((3,3),(0.0270544913417901,0.0439828187741889),
 .UNSPECIFIED.)
CURVE()
GEOMETRIC_REPRESENTATION_ITEM()
RATIONAL_B_SPLINE_CURVE((1.00082963690151,1.00067437544892,1.))
REPRESENTATION_ITEM('')
);
#304=(
BOUNDED_CURVE()
B_SPLINE_CURVE(2,(#58661,#58662,#58663),.UNSPECIFIED.,.F.,.F.)
B_SPLINE_CURVE_WITH_KNOTS((3,3),(0.,0.0169283274324599),.UNSPECIFIED.)
CURVE()
GEOMETRIC_REPRESENTATION_ITEM()
RATIONAL_B_SPLINE_CURVE((1.,1.00067437544707,1.00082963689925))
REPRESENTATION_ITEM('')
);
#305=(
BOUNDED_CURVE()
B_SPLINE_CURVE(2,(#58665,#58666,#58667),.UNSPECIFIED.,.F.,.F.)
B_SPLINE_CURVE_WITH_KNOTS((3,3),(0.0270544913417598,0.0439828187741897),
 .UNSPECIFIED.)
CURVE()
GEOMETRIC_REPRESENTATION_ITEM()
RATIONAL_B_SPLINE_CURVE((1.00082963689893,1.00067437544681,1.))
REPRESENTATION_ITEM('')
);
#306=(
BOUNDED_CURVE()
B_SPLINE_CURVE(2,(#58671,#58672,#58673),.UNSPECIFIED.,.F.,.F.)
B_SPLINE_CURVE_WITH_KNOTS((3,3),(0.,0.0169283274324799),.UNSPECIFIED.)
CURVE()
GEOMETRIC_REPRESENTATION_ITEM()
RATIONAL_B_SPLINE_CURVE((1.,1.00067437544677,1.00082963689888))
REPRESENTATION_ITEM('')
);
#307=(
BOUNDED_CURVE()
B_SPLINE_CURVE(2,(#58675,#58676,#58677),.UNSPECIFIED.,.F.,.F.)
B_SPLINE_CURVE_WITH_KNOTS((3,3),(0.0270544913418231,0.0439828187741892),
 .UNSPECIFIED.)
CURVE()
GEOMETRIC_REPRESENTATION_ITEM()
RATIONAL_B_SPLINE_CURVE((1.00082963690453,1.00067437545137,1.))
REPRESENTATION_ITEM('')
);
#308=(
BOUNDED_CURVE()
B_SPLINE_CURVE(2,(#58681,#58682,#58683),.UNSPECIFIED.,.F.,.F.)
B_SPLINE_CURVE_WITH_KNOTS((3,3),(0.,0.0169283274323869),.UNSPECIFIED.)
CURVE()
GEOMETRIC_REPRESENTATION_ITEM()
RATIONAL_B_SPLINE_CURVE((1.,1.00067437545224,1.0008296369056))
REPRESENTATION_ITEM('')
);
#309=(
BOUNDED_CURVE()
B_SPLINE_CURVE(2,(#58685,#58686,#58687),.UNSPECIFIED.,.F.,.F.)
B_SPLINE_CURVE_WITH_KNOTS((3,3),(0.0270544913417943,0.0439828187741897),
 .UNSPECIFIED.)
CURVE()
GEOMETRIC_REPRESENTATION_ITEM()
RATIONAL_B_SPLINE_CURVE((1.00082963690791,1.00067437545412,1.))
REPRESENTATION_ITEM('')
);
#310=(
BOUNDED_CURVE()
B_SPLINE_CURVE(2,(#58691,#58692,#58693),.UNSPECIFIED.,.F.,.F.)
B_SPLINE_CURVE_WITH_KNOTS((3,3),(0.,0.0169283274323051),.UNSPECIFIED.)
CURVE()
GEOMETRIC_REPRESENTATION_ITEM()
RATIONAL_B_SPLINE_CURVE((1.,1.00067437546317,1.00082963691906))
REPRESENTATION_ITEM('')
);
#311=(
BOUNDED_CURVE()
B_SPLINE_CURVE(2,(#58695,#58696,#58697),.UNSPECIFIED.,.F.,.F.)
B_SPLINE_CURVE_WITH_KNOTS((3,3),(0.027054491341705,0.0439828187741902),
 .UNSPECIFIED.)
CURVE()
GEOMETRIC_REPRESENTATION_ITEM()
RATIONAL_B_SPLINE_CURVE((1.00082963689389,1.00067437544272,1.))
REPRESENTATION_ITEM('')
);
#312=(
BOUNDED_CURVE()
B_SPLINE_CURVE(2,(#58701,#58702,#58703),.UNSPECIFIED.,.F.,.F.)
B_SPLINE_CURVE_WITH_KNOTS((3,3),(0.,0.0169283274323258),.UNSPECIFIED.)
CURVE()
GEOMETRIC_REPRESENTATION_ITEM()
RATIONAL_B_SPLINE_CURVE((1.,1.00067437545656,1.00082963691092))
REPRESENTATION_ITEM('')
);
#313=(
BOUNDED_CURVE()
B_SPLINE_CURVE(2,(#58705,#58706,#58707),.UNSPECIFIED.,.F.,.F.)
B_SPLINE_CURVE_WITH_KNOTS((3,3),(0.0270544913418574,0.0439828187741888),
 .UNSPECIFIED.)
CURVE()
GEOMETRIC_REPRESENTATION_ITEM()
RATIONAL_B_SPLINE_CURVE((1.00082963691715,1.00067437546163,1.))
REPRESENTATION_ITEM('')
);
#314=(
BOUNDED_CURVE()
B_SPLINE_CURVE(2,(#58711,#58712,#58713),.UNSPECIFIED.,.F.,.F.)
B_SPLINE_CURVE_WITH_KNOTS((3,3),(0.,0.0169283274323776),.UNSPECIFIED.)
CURVE()
GEOMETRIC_REPRESENTATION_ITEM()
RATIONAL_B_SPLINE_CURVE((1.,1.00067437544935,1.00082963690205))
REPRESENTATION_ITEM('')
);
#315=(
BOUNDED_CURVE()
B_SPLINE_CURVE(2,(#58715,#58716,#58717),.UNSPECIFIED.,.F.,.F.)
B_SPLINE_CURVE_WITH_KNOTS((3,3),(0.0270544913418392,0.0439828187741898),
 .UNSPECIFIED.)
CURVE()
GEOMETRIC_REPRESENTATION_ITEM()
RATIONAL_B_SPLINE_CURVE((1.00082963690784,1.00067437545406,1.))
REPRESENTATION_ITEM('')
);
#316=(
BOUNDED_CURVE()
B_SPLINE_CURVE(2,(#58721,#58722,#58723),.UNSPECIFIED.,.F.,.F.)
B_SPLINE_CURVE_WITH_KNOTS((3,3),(0.,0.0169283274323582),.UNSPECIFIED.)
CURVE()
GEOMETRIC_REPRESENTATION_ITEM()
RATIONAL_B_SPLINE_CURVE((1.,1.0006743754544,1.00082963690826))
REPRESENTATION_ITEM('')
);
#317=(
BOUNDED_CURVE()
B_SPLINE_CURVE(2,(#58725,#58726,#58727),.UNSPECIFIED.,.F.,.F.)
B_SPLINE_CURVE_WITH_KNOTS((3,3),(0.0270544913418716,0.0439828187741891),
 .UNSPECIFIED.)
CURVE()
GEOMETRIC_REPRESENTATION_ITEM()
RATIONAL_B_SPLINE_CURVE((1.00082963691279,1.00067437545808,1.))
REPRESENTATION_ITEM('')
);
#318=(
BOUNDED_CURVE()
B_SPLINE_CURVE(2,(#58731,#58732,#58733),.UNSPECIFIED.,.F.,.F.)
B_SPLINE_CURVE_WITH_KNOTS((3,3),(0.,0.0169283274323239),.UNSPECIFIED.)
CURVE()
GEOMETRIC_REPRESENTATION_ITEM()
RATIONAL_B_SPLINE_CURVE((1.,1.00067437545309,1.00082963690665))
REPRESENTATION_ITEM('')
);
#319=(
BOUNDED_CURVE()
B_SPLINE_CURVE(2,(#58735,#58736,#58737),.UNSPECIFIED.,.F.,.F.)
B_SPLINE_CURVE_WITH_KNOTS((3,3),(0.0270544913418909,0.0439828187741894),
 .UNSPECIFIED.)
CURVE()
GEOMETRIC_REPRESENTATION_ITEM()
RATIONAL_B_SPLINE_CURVE((1.00082963691804,1.00067437546234,1.))
REPRESENTATION_ITEM('')
);
#320=(
BOUNDED_CURVE()
B_SPLINE_CURVE(2,(#58741,#58742,#58743),.UNSPECIFIED.,.F.,.F.)
B_SPLINE_CURVE_WITH_KNOTS((3,3),(0.,0.0169283274323187),.UNSPECIFIED.)
CURVE()
GEOMETRIC_REPRESENTATION_ITEM()
RATIONAL_B_SPLINE_CURVE((1.,1.00067437545808,1.00082963691279))
REPRESENTATION_ITEM('')
);
#321=(
BOUNDED_CURVE()
B_SPLINE_CURVE(2,(#58745,#58746,#58747),.UNSPECIFIED.,.F.,.F.)
B_SPLINE_CURVE_WITH_KNOTS((3,3),(0.0270544913417975,0.0439828187741893),
 .UNSPECIFIED.)
CURVE()
GEOMETRIC_REPRESENTATION_ITEM()
RATIONAL_B_SPLINE_CURVE((1.00082963690175,1.00067437544911,1.))
REPRESENTATION_ITEM('')
);
#322=(
BOUNDED_CURVE()
B_SPLINE_CURVE(2,(#58751,#58752,#58753),.UNSPECIFIED.,.F.,.F.)
B_SPLINE_CURVE_WITH_KNOTS((3,3),(0.,0.0169283274323514),.UNSPECIFIED.)
CURVE()
GEOMETRIC_REPRESENTATION_ITEM()
RATIONAL_B_SPLINE_CURVE((1.,1.00067437545079,1.00082963690382))
REPRESENTATION_ITEM('')
);
#323=(
BOUNDED_CURVE()
B_SPLINE_CURVE(2,(#58755,#58756,#58757),.UNSPECIFIED.,.F.,.F.)
B_SPLINE_CURVE_WITH_KNOTS((3,3),(0.0270544913418461,0.043982818774189),
 .UNSPECIFIED.)
CURVE()
GEOMETRIC_REPRESENTATION_ITEM()
RATIONAL_B_SPLINE_CURVE((1.00082963691007,1.00067437545587,1.))
REPRESENTATION_ITEM('')
);
#324=(
BOUNDED_CURVE()
B_SPLINE_CURVE(2,(#58761,#58762,#58763),.UNSPECIFIED.,.F.,.F.)
B_SPLINE_CURVE_WITH_KNOTS((3,3),(0.,0.0169283274323367),.UNSPECIFIED.)
CURVE()
GEOMETRIC_REPRESENTATION_ITEM()
RATIONAL_B_SPLINE_CURVE((1.,1.00067437545527,1.00082963690933))
REPRESENTATION_ITEM('')
);
#325=(
BOUNDED_CURVE()
B_SPLINE_CURVE(2,(#58765,#58766,#58767),.UNSPECIFIED.,.F.,.F.)
B_SPLINE_CURVE_WITH_KNOTS((3,3),(0.0270544913418436,0.0439828187741888),
 .UNSPECIFIED.)
CURVE()
GEOMETRIC_REPRESENTATION_ITEM()
RATIONAL_B_SPLINE_CURVE((1.00082963691215,1.00067437545756,1.))
REPRESENTATION_ITEM('')
);
#326=(
BOUNDED_CURVE()
B_SPLINE_CURVE(2,(#58771,#58772,#58773),.UNSPECIFIED.,.F.,.F.)
B_SPLINE_CURVE_WITH_KNOTS((3,3),(0.,0.0169283274324564),.UNSPECIFIED.)
CURVE()
GEOMETRIC_REPRESENTATION_ITEM()
RATIONAL_B_SPLINE_CURVE((1.,1.00067437544799,1.00082963690037))
REPRESENTATION_ITEM('')
);
#327=(
BOUNDED_CURVE()
B_SPLINE_CURVE(2,(#58775,#58776,#58777),.UNSPECIFIED.,.F.,.F.)
B_SPLINE_CURVE_WITH_KNOTS((3,3),(0.0270544913419147,0.0439828187741882),
 .UNSPECIFIED.)
CURVE()
GEOMETRIC_REPRESENTATION_ITEM()
RATIONAL_B_SPLINE_CURVE((1.00082963691331,1.00067437545851,1.))
REPRESENTATION_ITEM('')
);
#328=(
BOUNDED_CURVE()
B_SPLINE_CURVE(2,(#58781,#58782,#58783),.UNSPECIFIED.,.F.,.F.)
B_SPLINE_CURVE_WITH_KNOTS((3,3),(0.,0.0169283274324423),.UNSPECIFIED.)
CURVE()
GEOMETRIC_REPRESENTATION_ITEM()
RATIONAL_B_SPLINE_CURVE((1.,1.00067437544741,1.00082963689965))
REPRESENTATION_ITEM('')
);
#329=(
BOUNDED_CURVE()
B_SPLINE_CURVE(2,(#58785,#58786,#58787),.UNSPECIFIED.,.F.,.F.)
B_SPLINE_CURVE_WITH_KNOTS((3,3),(0.0270544913418278,0.0439828187741883),
 .UNSPECIFIED.)
CURVE()
GEOMETRIC_REPRESENTATION_ITEM()
RATIONAL_B_SPLINE_CURVE((1.00082963690487,1.00067437545164,1.))
REPRESENTATION_ITEM('')
);
#330=(
BOUNDED_CURVE()
B_SPLINE_CURVE(2,(#58791,#58792,#58793),.UNSPECIFIED.,.F.,.F.)
B_SPLINE_CURVE_WITH_KNOTS((3,3),(0.,0.0169283274324055),.UNSPECIFIED.)
CURVE()
GEOMETRIC_REPRESENTATION_ITEM()
RATIONAL_B_SPLINE_CURVE((1.,1.00067437544812,1.00082963690053))
REPRESENTATION_ITEM('')
);
#331=(
BOUNDED_CURVE()
B_SPLINE_CURVE(2,(#58795,#58796,#58797),.UNSPECIFIED.,.F.,.F.)
B_SPLINE_CURVE_WITH_KNOTS((3,3),(0.0270544913418545,0.0439828187741889),
 .UNSPECIFIED.)
CURVE()
GEOMETRIC_REPRESENTATION_ITEM()
RATIONAL_B_SPLINE_CURVE((1.00082963690979,1.00067437545564,1.))
REPRESENTATION_ITEM('')
);
#332=(
BOUNDED_CURVE()
B_SPLINE_CURVE(2,(#58801,#58802,#58803),.UNSPECIFIED.,.F.,.F.)
B_SPLINE_CURVE_WITH_KNOTS((3,3),(0.,0.016928327432381),.UNSPECIFIED.)
CURVE()
GEOMETRIC_REPRESENTATION_ITEM()
RATIONAL_B_SPLINE_CURVE((1.,1.0006743754549,1.00082963690887))
REPRESENTATION_ITEM('')
);
#333=(
BOUNDED_CURVE()
B_SPLINE_CURVE(2,(#58805,#58806,#58807),.UNSPECIFIED.,.F.,.F.)
B_SPLINE_CURVE_WITH_KNOTS((3,3),(0.0270544913418599,0.043982818774188),
 .UNSPECIFIED.)
CURVE()
GEOMETRIC_REPRESENTATION_ITEM()
RATIONAL_B_SPLINE_CURVE((1.00082963691264,1.00067437545796,1.))
REPRESENTATION_ITEM('')
);
#334=(
BOUNDED_CURVE()
B_SPLINE_CURVE(2,(#58811,#58812,#58813),.UNSPECIFIED.,.F.,.F.)
B_SPLINE_CURVE_WITH_KNOTS((3,3),(0.,0.0169283274323032),.UNSPECIFIED.)
CURVE()
GEOMETRIC_REPRESENTATION_ITEM()
RATIONAL_B_SPLINE_CURVE((1.,1.00067437546434,1.00082963692049))
REPRESENTATION_ITEM('')
);
#335=(
BOUNDED_CURVE()
B_SPLINE_CURVE(2,(#58815,#58816,#58817),.UNSPECIFIED.,.F.,.F.)
B_SPLINE_CURVE_WITH_KNOTS((3,3),(0.0270544913418524,0.0439828187741887),
 .UNSPECIFIED.)
CURVE()
GEOMETRIC_REPRESENTATION_ITEM()
RATIONAL_B_SPLINE_CURVE((1.00082963690961,1.0006743754555,1.))
REPRESENTATION_ITEM('')
);
#336=(
BOUNDED_CURVE()
B_SPLINE_CURVE(2,(#58821,#58822,#58823),.UNSPECIFIED.,.F.,.F.)
B_SPLINE_CURVE_WITH_KNOTS((3,3),(0.,0.0169283274323137),.UNSPECIFIED.)
CURVE()
GEOMETRIC_REPRESENTATION_ITEM()
RATIONAL_B_SPLINE_CURVE((1.,1.00067437546296,1.00082963691879))
REPRESENTATION_ITEM('')
);
#337=(
BOUNDED_CURVE()
B_SPLINE_CURVE(2,(#58825,#58826,#58827),.UNSPECIFIED.,.F.,.F.)
B_SPLINE_CURVE_WITH_KNOTS((3,3),(0.0270544913418263,0.0439828187741885),
 .UNSPECIFIED.)
CURVE()
GEOMETRIC_REPRESENTATION_ITEM()
RATIONAL_B_SPLINE_CURVE((1.00082963691197,1.00067437545741,1.))
REPRESENTATION_ITEM('')
);
#338=(
BOUNDED_CURVE()
B_SPLINE_CURVE(2,(#58832,#58833,#58834),.UNSPECIFIED.,.F.,.F.)
B_SPLINE_CURVE_WITH_KNOTS((3,3),(0.,0.0169283274323449),.UNSPECIFIED.)
CURVE()
GEOMETRIC_REPRESENTATION_ITEM()
RATIONAL_B_SPLINE_CURVE((1.,1.00067437545405,1.00082963690783))
REPRESENTATION_ITEM('')
);
#339=(
BOUNDED_CURVE()
B_SPLINE_CURVE(2,(#58836,#58837,#58838),.UNSPECIFIED.,.F.,.F.)
B_SPLINE_CURVE_WITH_KNOTS((3,3),(0.0270544913417649,0.0439828187741904),
 .UNSPECIFIED.)
CURVE()
GEOMETRIC_REPRESENTATION_ITEM()
RATIONAL_B_SPLINE_CURVE((1.00082963690075,1.0006743754483,1.))
REPRESENTATION_ITEM('')
);
#340=(
BOUNDED_CURVE()
B_SPLINE_CURVE(2,(#58842,#58843,#58844),.UNSPECIFIED.,.F.,.F.)
B_SPLINE_CURVE_WITH_KNOTS((3,3),(0.,0.0169283274323657),.UNSPECIFIED.)
CURVE()
GEOMETRIC_REPRESENTATION_ITEM()
RATIONAL_B_SPLINE_CURVE((1.,1.00067437545132,1.00082963690448))
REPRESENTATION_ITEM('')
);
#341=(
BOUNDED_CURVE()
B_SPLINE_CURVE(2,(#58846,#58847,#58848),.UNSPECIFIED.,.F.,.F.)
B_SPLINE_CURVE_WITH_KNOTS((3,3),(0.0270544913418314,0.0439828187741895),
 .UNSPECIFIED.)
CURVE()
GEOMETRIC_REPRESENTATION_ITEM()
RATIONAL_B_SPLINE_CURVE((1.00082963690259,1.00067437544979,1.))
REPRESENTATION_ITEM('')
);
#342=(
BOUNDED_CURVE()
B_SPLINE_CURVE(2,(#58852,#58853,#58854),.UNSPECIFIED.,.F.,.F.)
B_SPLINE_CURVE_WITH_KNOTS((3,3),(0.,0.0169283274324112),.UNSPECIFIED.)
CURVE()
GEOMETRIC_REPRESENTATION_ITEM()
RATIONAL_B_SPLINE_CURVE((1.,1.00067437544367,1.00082963689506))
REPRESENTATION_ITEM('')
);
#343=(
BOUNDED_CURVE()
B_SPLINE_CURVE(2,(#58856,#58857,#58858),.UNSPECIFIED.,.F.,.F.)
B_SPLINE_CURVE_WITH_KNOTS((3,3),(0.0270544913417055,0.0439828187741905),
 .UNSPECIFIED.)
CURVE()
GEOMETRIC_REPRESENTATION_ITEM()
RATIONAL_B_SPLINE_CURVE((1.00082963689237,1.00067437544149,1.))
REPRESENTATION_ITEM('')
);
#344=(
BOUNDED_CURVE()
B_SPLINE_CURVE(2,(#58862,#58863,#58864),.UNSPECIFIED.,.F.,.F.)
B_SPLINE_CURVE_WITH_KNOTS((3,3),(0.,0.0169283274324376),.UNSPECIFIED.)
CURVE()
GEOMETRIC_REPRESENTATION_ITEM()
RATIONAL_B_SPLINE_CURVE((1.,1.0006743754461,1.00082963689805))
REPRESENTATION_ITEM('')
);
#345=(
BOUNDED_CURVE()
B_SPLINE_CURVE(2,(#58866,#58867,#58868),.UNSPECIFIED.,.F.,.F.)
B_SPLINE_CURVE_WITH_KNOTS((3,3),(0.0270544913417534,0.0439828187741907),
 .UNSPECIFIED.)
CURVE()
GEOMETRIC_REPRESENTATION_ITEM()
RATIONAL_B_SPLINE_CURVE((1.00082963689691,1.00067437544518,1.))
REPRESENTATION_ITEM('')
);
#346=(
BOUNDED_CURVE()
B_SPLINE_CURVE(2,(#58872,#58873,#58874),.UNSPECIFIED.,.F.,.F.)
B_SPLINE_CURVE_WITH_KNOTS((3,3),(0.,0.0169283274323307),.UNSPECIFIED.)
CURVE()
GEOMETRIC_REPRESENTATION_ITEM()
RATIONAL_B_SPLINE_CURVE((1.,1.00067437545699,1.00082963691144))
REPRESENTATION_ITEM('')
);
#347=(
BOUNDED_CURVE()
B_SPLINE_CURVE(2,(#58876,#58877,#58878),.UNSPECIFIED.,.F.,.F.)
B_SPLINE_CURVE_WITH_KNOTS((3,3),(0.0270544913418834,0.0439828187741894),
 .UNSPECIFIED.)
CURVE()
GEOMETRIC_REPRESENTATION_ITEM()
RATIONAL_B_SPLINE_CURVE((1.00082963691786,1.0006743754622,1.))
REPRESENTATION_ITEM('')
);
#348=(
BOUNDED_CURVE()
B_SPLINE_CURVE(2,(#58882,#58883,#58884),.UNSPECIFIED.,.F.,.F.)
B_SPLINE_CURVE_WITH_KNOTS((3,3),(0.,0.0169283274324524),.UNSPECIFIED.)
CURVE()
GEOMETRIC_REPRESENTATION_ITEM()
RATIONAL_B_SPLINE_CURVE((1.,1.000674375448,1.00082963690039))
REPRESENTATION_ITEM('')
);
#349=(
BOUNDED_CURVE()
B_SPLINE_CURVE(2,(#58886,#58887,#58888),.UNSPECIFIED.,.F.,.F.)
B_SPLINE_CURVE_WITH_KNOTS((3,3),(0.027054491341806,0.0439828187741904),
 .UNSPECIFIED.)
CURVE()
GEOMETRIC_REPRESENTATION_ITEM()
RATIONAL_B_SPLINE_CURVE((1.00082963690582,1.00067437545241,1.))
REPRESENTATION_ITEM('')
);
#350=(
BOUNDED_CURVE()
B_SPLINE_CURVE(2,(#58892,#58893,#58894),.UNSPECIFIED.,.F.,.F.)
B_SPLINE_CURVE_WITH_KNOTS((3,3),(0.,0.0169283274324273),.UNSPECIFIED.)
CURVE()
GEOMETRIC_REPRESENTATION_ITEM()
RATIONAL_B_SPLINE_CURVE((1.,1.00067437544657,1.00082963689862))
REPRESENTATION_ITEM('')
);
#351=(
BOUNDED_CURVE()
B_SPLINE_CURVE(2,(#58896,#58897,#58898),.UNSPECIFIED.,.F.,.F.)
B_SPLINE_CURVE_WITH_KNOTS((3,3),(0.0270544913418182,0.04398281877419),
 .UNSPECIFIED.)
CURVE()
GEOMETRIC_REPRESENTATION_ITEM()
RATIONAL_B_SPLINE_CURVE((1.00082963691171,1.0006743754572,1.))
REPRESENTATION_ITEM('')
);
#352=(
BOUNDED_CURVE()
B_SPLINE_CURVE(2,(#58901,#58902,#58903),.UNSPECIFIED.,.F.,.F.)
B_SPLINE_CURVE_WITH_KNOTS((3,3),(0.,0.0169283274324202),.UNSPECIFIED.)
CURVE()
GEOMETRIC_REPRESENTATION_ITEM()
RATIONAL_B_SPLINE_CURVE((1.,1.00067437545079,1.00082963690381))
REPRESENTATION_ITEM('')
);
#353=(
BOUNDED_CURVE()
B_SPLINE_CURVE(2,(#65992,#65993,#65994),.UNSPECIFIED.,.F.,.F.)
B_SPLINE_CURVE_WITH_KNOTS((3,3),(0.,0.0169283274323722),.UNSPECIFIED.)
CURVE()
GEOMETRIC_REPRESENTATION_ITEM()
RATIONAL_B_SPLINE_CURVE((1.,1.00067437545138,1.00082963690455))
REPRESENTATION_ITEM('')
);
#354=(
BOUNDED_CURVE()
B_SPLINE_CURVE(2,(#65999,#66000,#66001),.UNSPECIFIED.,.F.,.F.)
B_SPLINE_CURVE_WITH_KNOTS((3,3),(0.0270544913418023,0.0439828187741892),
 .UNSPECIFIED.)
CURVE()
GEOMETRIC_REPRESENTATION_ITEM()
RATIONAL_B_SPLINE_CURVE((1.00082963690332,1.00067437545039,1.))
REPRESENTATION_ITEM('')
);
#355=(
BOUNDED_CURVE()
B_SPLINE_CURVE(2,(#66008,#66009,#66010),.UNSPECIFIED.,.F.,.F.)
B_SPLINE_CURVE_WITH_KNOTS((3,3),(0.0270544913418047,0.0439828187741891),
 .UNSPECIFIED.)
CURVE()
GEOMETRIC_REPRESENTATION_ITEM()
RATIONAL_B_SPLINE_CURVE((1.00082963690338,1.00067437545043,1.))
REPRESENTATION_ITEM('')
);
#356=(
BOUNDED_CURVE()
B_SPLINE_CURVE(2,(#66014,#66015,#66016),.UNSPECIFIED.,.F.,.F.)
B_SPLINE_CURVE_WITH_KNOTS((3,3),(0.,0.0169283274323899),.UNSPECIFIED.)
CURVE()
GEOMETRIC_REPRESENTATION_ITEM()
RATIONAL_B_SPLINE_CURVE((1.,1.00067437544971,1.00082963690249))
REPRESENTATION_ITEM('')
);
#357=(
BOUNDED_CURVE()
B_SPLINE_CURVE(2,(#66018,#66019,#66020),.UNSPECIFIED.,.F.,.F.)
B_SPLINE_CURVE_WITH_KNOTS((3,3),(0.0270544913417485,0.0439828187741892),
 .UNSPECIFIED.)
CURVE()
GEOMETRIC_REPRESENTATION_ITEM()
RATIONAL_B_SPLINE_CURVE((1.00082963689667,1.00067437544498,1.))
REPRESENTATION_ITEM('')
);
#358=(
BOUNDED_CURVE()
B_SPLINE_CURVE(2,(#66024,#66025,#66026),.UNSPECIFIED.,.F.,.F.)
B_SPLINE_CURVE_WITH_KNOTS((3,3),(0.,0.0169283274324321),.UNSPECIFIED.)
CURVE()
GEOMETRIC_REPRESENTATION_ITEM()
RATIONAL_B_SPLINE_CURVE((1.,1.00067437544514,1.00082963689687))
REPRESENTATION_ITEM('')
);
#359=(
BOUNDED_CURVE()
B_SPLINE_CURVE(2,(#66028,#66029,#66030),.UNSPECIFIED.,.F.,.F.)
B_SPLINE_CURVE_WITH_KNOTS((3,3),(0.0270544913417875,0.0439828187741892),
 .UNSPECIFIED.)
CURVE()
GEOMETRIC_REPRESENTATION_ITEM()
RATIONAL_B_SPLINE_CURVE((1.00082963689786,1.00067437544595,1.))
REPRESENTATION_ITEM('')
);
#360=(
BOUNDED_CURVE()
B_SPLINE_CURVE(2,(#66034,#66035,#66036),.UNSPECIFIED.,.F.,.F.)
B_SPLINE_CURVE_WITH_KNOTS((3,3),(0.,0.0169283274323828),.UNSPECIFIED.)
CURVE()
GEOMETRIC_REPRESENTATION_ITEM()
RATIONAL_B_SPLINE_CURVE((1.,1.00067437545006,1.00082963690291))
REPRESENTATION_ITEM('')
);
#361=(
BOUNDED_CURVE()
B_SPLINE_CURVE(2,(#66038,#66039,#66040),.UNSPECIFIED.,.F.,.F.)
B_SPLINE_CURVE_WITH_KNOTS((3,3),(0.0270544913418211,0.0439828187741892),
 .UNSPECIFIED.)
CURVE()
GEOMETRIC_REPRESENTATION_ITEM()
RATIONAL_B_SPLINE_CURVE((1.00082963690425,1.00067437545114,1.))
REPRESENTATION_ITEM('')
);
#362=(
BOUNDED_CURVE()
B_SPLINE_CURVE(2,(#66044,#66045,#66046),.UNSPECIFIED.,.F.,.F.)
B_SPLINE_CURVE_WITH_KNOTS((3,3),(0.,0.0169283274323665),.UNSPECIFIED.)
CURVE()
GEOMETRIC_REPRESENTATION_ITEM()
RATIONAL_B_SPLINE_CURVE((1.,1.00067437544743,1.00082963689969))
REPRESENTATION_ITEM('')
);
#363=(
BOUNDED_CURVE()
B_SPLINE_CURVE(2,(#66048,#66049,#66050),.UNSPECIFIED.,.F.,.F.)
B_SPLINE_CURVE_WITH_KNOTS((3,3),(0.0270544913417642,0.043982818774189),
 .UNSPECIFIED.)
CURVE()
GEOMETRIC_REPRESENTATION_ITEM()
RATIONAL_B_SPLINE_CURVE((1.00082963689682,1.0006743754451,1.))
REPRESENTATION_ITEM('')
);
#364=(
BOUNDED_CURVE()
B_SPLINE_CURVE(2,(#66054,#66055,#66056),.UNSPECIFIED.,.F.,.F.)
B_SPLINE_CURVE_WITH_KNOTS((3,3),(0.,0.0169283274324012),.UNSPECIFIED.)
CURVE()
GEOMETRIC_REPRESENTATION_ITEM()
RATIONAL_B_SPLINE_CURVE((1.,1.00067437544784,1.00082963690019))
REPRESENTATION_ITEM('')
);
#365=(
BOUNDED_CURVE()
B_SPLINE_CURVE(2,(#66058,#66059,#66060),.UNSPECIFIED.,.F.,.F.)
B_SPLINE_CURVE_WITH_KNOTS((3,3),(0.0270544913418049,0.0439828187741891),
 .UNSPECIFIED.)
CURVE()
GEOMETRIC_REPRESENTATION_ITEM()
RATIONAL_B_SPLINE_CURVE((1.00082963689975,1.00067437544748,1.))
REPRESENTATION_ITEM('')
);
#366=(
BOUNDED_CURVE()
B_SPLINE_CURVE(2,(#66064,#66065,#66066),.UNSPECIFIED.,.F.,.F.)
B_SPLINE_CURVE_WITH_KNOTS((3,3),(0.,0.0169283274323776),.UNSPECIFIED.)
CURVE()
GEOMETRIC_REPRESENTATION_ITEM()
RATIONAL_B_SPLINE_CURVE((1.,1.00067437545055,1.00082963690352))
REPRESENTATION_ITEM('')
);
#367=(
BOUNDED_CURVE()
B_SPLINE_CURVE(2,(#66068,#66069,#66070),.UNSPECIFIED.,.F.,.F.)
B_SPLINE_CURVE_WITH_KNOTS((3,3),(0.0270544913417675,0.0439828187741888),
 .UNSPECIFIED.)
CURVE()
GEOMETRIC_REPRESENTATION_ITEM()
RATIONAL_B_SPLINE_CURVE((1.00082963689636,1.00067437544473,1.))
REPRESENTATION_ITEM('')
);
#368=(
BOUNDED_CURVE()
B_SPLINE_CURVE(2,(#66074,#66075,#66076),.UNSPECIFIED.,.F.,.F.)
B_SPLINE_CURVE_WITH_KNOTS((3,3),(0.,0.0169283274323805),.UNSPECIFIED.)
CURVE()
GEOMETRIC_REPRESENTATION_ITEM()
RATIONAL_B_SPLINE_CURVE((1.,1.00067437545024,1.00082963690314))
REPRESENTATION_ITEM('')
);
#369=(
BOUNDED_CURVE()
B_SPLINE_CURVE(2,(#66078,#66079,#66080),.UNSPECIFIED.,.F.,.F.)
B_SPLINE_CURVE_WITH_KNOTS((3,3),(0.0270544913417762,0.0439828187741891),
 .UNSPECIFIED.)
CURVE()
GEOMETRIC_REPRESENTATION_ITEM()
RATIONAL_B_SPLINE_CURVE((1.00082963689788,1.00067437544596,1.))
REPRESENTATION_ITEM('')
);
#370=(
BOUNDED_CURVE()
B_SPLINE_CURVE(2,(#66084,#66085,#66086),.UNSPECIFIED.,.F.,.F.)
B_SPLINE_CURVE_WITH_KNOTS((3,3),(0.,0.0169283274323929),.UNSPECIFIED.)
CURVE()
GEOMETRIC_REPRESENTATION_ITEM()
RATIONAL_B_SPLINE_CURVE((1.,1.00067437545034,1.00082963690327))
REPRESENTATION_ITEM('')
);
#371=(
BOUNDED_CURVE()
B_SPLINE_CURVE(2,(#66088,#66089,#66090),.UNSPECIFIED.,.F.,.F.)
B_SPLINE_CURVE_WITH_KNOTS((3,3),(0.0270544913417606,0.0439828187741894),
 .UNSPECIFIED.)
CURVE()
GEOMETRIC_REPRESENTATION_ITEM()
RATIONAL_B_SPLINE_CURVE((1.00082963689914,1.00067437544699,1.))
REPRESENTATION_ITEM('')
);
#372=(
BOUNDED_CURVE()
B_SPLINE_CURVE(2,(#66094,#66095,#66096),.UNSPECIFIED.,.F.,.F.)
B_SPLINE_CURVE_WITH_KNOTS((3,3),(0.,0.0169283274323603),.UNSPECIFIED.)
CURVE()
GEOMETRIC_REPRESENTATION_ITEM()
RATIONAL_B_SPLINE_CURVE((1.,1.00067437544665,1.00082963689872))
REPRESENTATION_ITEM('')
);
#373=(
BOUNDED_CURVE()
B_SPLINE_CURVE(2,(#66098,#66099,#66100),.UNSPECIFIED.,.F.,.F.)
B_SPLINE_CURVE_WITH_KNOTS((3,3),(0.0270544913417842,0.043982818774189),
 .UNSPECIFIED.)
CURVE()
GEOMETRIC_REPRESENTATION_ITEM()
RATIONAL_B_SPLINE_CURVE((1.00082963689636,1.00067437544473,1.))
REPRESENTATION_ITEM('')
);
#374=(
BOUNDED_CURVE()
B_SPLINE_CURVE(2,(#66104,#66105,#66106),.UNSPECIFIED.,.F.,.F.)
B_SPLINE_CURVE_WITH_KNOTS((3,3),(0.,0.0169283274323958),.UNSPECIFIED.)
CURVE()
GEOMETRIC_REPRESENTATION_ITEM()
RATIONAL_B_SPLINE_CURVE((1.,1.00067437544716,1.00082963689935))
REPRESENTATION_ITEM('')
);
#375=(
BOUNDED_CURVE()
B_SPLINE_CURVE(2,(#66108,#66109,#66110),.UNSPECIFIED.,.F.,.F.)
B_SPLINE_CURVE_WITH_KNOTS((3,3),(0.0270544913417961,0.0439828187741891),
 .UNSPECIFIED.)
CURVE()
GEOMETRIC_REPRESENTATION_ITEM()
RATIONAL_B_SPLINE_CURVE((1.00082963689727,1.00067437544546,1.))
REPRESENTATION_ITEM('')
);
#376=(
BOUNDED_CURVE()
B_SPLINE_CURVE(2,(#66114,#66115,#66116),.UNSPECIFIED.,.F.,.F.)
B_SPLINE_CURVE_WITH_KNOTS((3,3),(0.,0.016928327432345),.UNSPECIFIED.)
CURVE()
GEOMETRIC_REPRESENTATION_ITEM()
RATIONAL_B_SPLINE_CURVE((1.,1.00067437545236,1.00082963690575))
REPRESENTATION_ITEM('')
);
#377=(
BOUNDED_CURVE()
B_SPLINE_CURVE(2,(#66118,#66119,#66120),.UNSPECIFIED.,.F.,.F.)
B_SPLINE_CURVE_WITH_KNOTS((3,3),(0.0270544913417455,0.0439828187741891),
 .UNSPECIFIED.)
CURVE()
GEOMETRIC_REPRESENTATION_ITEM()
RATIONAL_B_SPLINE_CURVE((1.00082963689847,1.00067437544644,1.))
REPRESENTATION_ITEM('')
);
#378=(
BOUNDED_CURVE()
B_SPLINE_CURVE(2,(#66124,#66125,#66126),.UNSPECIFIED.,.F.,.F.)
B_SPLINE_CURVE_WITH_KNOTS((3,3),(0.,0.0169283274324359),.UNSPECIFIED.)
CURVE()
GEOMETRIC_REPRESENTATION_ITEM()
RATIONAL_B_SPLINE_CURVE((1.,1.00067437544276,1.00082963689394))
REPRESENTATION_ITEM('')
);
#379=(
BOUNDED_CURVE()
B_SPLINE_CURVE(2,(#66128,#66129,#66130),.UNSPECIFIED.,.F.,.F.)
B_SPLINE_CURVE_WITH_KNOTS((3,3),(0.0270544913417467,0.0439828187741893),
 .UNSPECIFIED.)
CURVE()
GEOMETRIC_REPRESENTATION_ITEM()
RATIONAL_B_SPLINE_CURVE((1.00082963690043,1.00067437544804,1.))
REPRESENTATION_ITEM('')
);
#380=(
BOUNDED_CURVE()
B_SPLINE_CURVE(2,(#66134,#66135,#66136),.UNSPECIFIED.,.F.,.F.)
B_SPLINE_CURVE_WITH_KNOTS((3,3),(0.,0.0169283274323855),.UNSPECIFIED.)
CURVE()
GEOMETRIC_REPRESENTATION_ITEM()
RATIONAL_B_SPLINE_CURVE((1.,1.00067437545031,1.00082963690323))
REPRESENTATION_ITEM('')
);
#381=(
BOUNDED_CURVE()
B_SPLINE_CURVE(2,(#66138,#66139,#66140),.UNSPECIFIED.,.F.,.F.)
B_SPLINE_CURVE_WITH_KNOTS((3,3),(0.0270544913418194,0.043982818774189),
 .UNSPECIFIED.)
CURVE()
GEOMETRIC_REPRESENTATION_ITEM()
RATIONAL_B_SPLINE_CURVE((1.0008296369013,1.00067437544875,1.))
REPRESENTATION_ITEM('')
);
#382=(
BOUNDED_CURVE()
B_SPLINE_CURVE(2,(#66144,#66145,#66146),.UNSPECIFIED.,.F.,.F.)
B_SPLINE_CURVE_WITH_KNOTS((3,3),(0.,0.0169283274324108),.UNSPECIFIED.)
CURVE()
GEOMETRIC_REPRESENTATION_ITEM()
RATIONAL_B_SPLINE_CURVE((1.,1.00067437544706,1.00082963689923))
REPRESENTATION_ITEM('')
);
#383=(
BOUNDED_CURVE()
B_SPLINE_CURVE(2,(#66148,#66149,#66150),.UNSPECIFIED.,.F.,.F.)
B_SPLINE_CURVE_WITH_KNOTS((3,3),(0.0270544913418122,0.043982818774189),
 .UNSPECIFIED.)
CURVE()
GEOMETRIC_REPRESENTATION_ITEM()
RATIONAL_B_SPLINE_CURVE((1.00082963689602,1.00067437544445,1.))
REPRESENTATION_ITEM('')
);
#384=(
BOUNDED_CURVE()
B_SPLINE_CURVE(2,(#66154,#66155,#66156),.UNSPECIFIED.,.F.,.F.)
B_SPLINE_CURVE_WITH_KNOTS((3,3),(0.,0.0169283274323979),.UNSPECIFIED.)
CURVE()
GEOMETRIC_REPRESENTATION_ITEM()
RATIONAL_B_SPLINE_CURVE((1.,1.00067437544686,1.00082963689898))
REPRESENTATION_ITEM('')
);
#385=(
BOUNDED_CURVE()
B_SPLINE_CURVE(2,(#66158,#66159,#66160),.UNSPECIFIED.,.F.,.F.)
B_SPLINE_CURVE_WITH_KNOTS((3,3),(0.0270544913417752,0.0439828187741891),
 .UNSPECIFIED.)
CURVE()
GEOMETRIC_REPRESENTATION_ITEM()
RATIONAL_B_SPLINE_CURVE((1.0008296369011,1.00067437544858,1.))
REPRESENTATION_ITEM('')
);
#386=(
BOUNDED_CURVE()
B_SPLINE_CURVE(2,(#66164,#66165,#66166),.UNSPECIFIED.,.F.,.F.)
B_SPLINE_CURVE_WITH_KNOTS((3,3),(0.,0.0169283274324112),.UNSPECIFIED.)
CURVE()
GEOMETRIC_REPRESENTATION_ITEM()
RATIONAL_B_SPLINE_CURVE((1.,1.00067437544825,1.00082963690069))
REPRESENTATION_ITEM('')
);
#387=(
BOUNDED_CURVE()
B_SPLINE_CURVE(2,(#66168,#66169,#66170),.UNSPECIFIED.,.F.,.F.)
B_SPLINE_CURVE_WITH_KNOTS((3,3),(0.0270544913417757,0.0439828187741891),
 .UNSPECIFIED.)
CURVE()
GEOMETRIC_REPRESENTATION_ITEM()
RATIONAL_B_SPLINE_CURVE((1.00082963690205,1.00067437544935,1.))
REPRESENTATION_ITEM('')
);
#388=(
BOUNDED_CURVE()
B_SPLINE_CURVE(2,(#66174,#66175,#66176),.UNSPECIFIED.,.F.,.F.)
B_SPLINE_CURVE_WITH_KNOTS((3,3),(0.,0.0169283274323844),.UNSPECIFIED.)
CURVE()
GEOMETRIC_REPRESENTATION_ITEM()
RATIONAL_B_SPLINE_CURVE((1.,1.00067437545136,1.00082963690451))
REPRESENTATION_ITEM('')
);
#389=(
BOUNDED_CURVE()
B_SPLINE_CURVE(2,(#66178,#66179,#66180),.UNSPECIFIED.,.F.,.F.)
B_SPLINE_CURVE_WITH_KNOTS((3,3),(0.0270544913417712,0.0439828187741894),
 .UNSPECIFIED.)
CURVE()
GEOMETRIC_REPRESENTATION_ITEM()
RATIONAL_B_SPLINE_CURVE((1.00082963690333,1.00067437545039,1.))
REPRESENTATION_ITEM('')
);
#390=(
BOUNDED_CURVE()
B_SPLINE_CURVE(2,(#66184,#66185,#66186),.UNSPECIFIED.,.F.,.F.)
B_SPLINE_CURVE_WITH_KNOTS((3,3),(0.,0.016928327432381),.UNSPECIFIED.)
CURVE()
GEOMETRIC_REPRESENTATION_ITEM()
RATIONAL_B_SPLINE_CURVE((1.,1.00067437544975,1.00082963690255))
REPRESENTATION_ITEM('')
);
#391=(
BOUNDED_CURVE()
B_SPLINE_CURVE(2,(#66188,#66189,#66190),.UNSPECIFIED.,.F.,.F.)
B_SPLINE_CURVE_WITH_KNOTS((3,3),(0.0270544913418043,0.0439828187741891),
 .UNSPECIFIED.)
CURVE()
GEOMETRIC_REPRESENTATION_ITEM()
RATIONAL_B_SPLINE_CURVE((1.00082963690328,1.00067437545035,1.))
REPRESENTATION_ITEM('')
);
#392=(
BOUNDED_CURVE()
B_SPLINE_CURVE(2,(#66195,#66196,#66197),.UNSPECIFIED.,.F.,.F.)
B_SPLINE_CURVE_WITH_KNOTS((3,3),(0.,0.0169283274323967),.UNSPECIFIED.)
CURVE()
GEOMETRIC_REPRESENTATION_ITEM()
RATIONAL_B_SPLINE_CURVE((1.,1.00067437544999,1.00082963690283))
REPRESENTATION_ITEM('')
);
#393=(
BOUNDED_CURVE()
B_SPLINE_CURVE(2,(#66199,#66200,#66201),.UNSPECIFIED.,.F.,.F.)
B_SPLINE_CURVE_WITH_KNOTS((3,3),(0.0270544913417582,0.0439828187741891),
 .UNSPECIFIED.)
CURVE()
GEOMETRIC_REPRESENTATION_ITEM()
RATIONAL_B_SPLINE_CURVE((1.00082963689937,1.00067437544717,1.))
REPRESENTATION_ITEM('')
);
#394=(
BOUNDED_CURVE()
B_SPLINE_CURVE(2,(#66205,#66206,#66207),.UNSPECIFIED.,.F.,.F.)
B_SPLINE_CURVE_WITH_KNOTS((3,3),(0.,0.0169283274324266),.UNSPECIFIED.)
CURVE()
GEOMETRIC_REPRESENTATION_ITEM()
RATIONAL_B_SPLINE_CURVE((1.,1.00067437544832,1.00082963690078))
REPRESENTATION_ITEM('')
);
#395=(
BOUNDED_CURVE()
B_SPLINE_CURVE(2,(#66209,#66210,#66211),.UNSPECIFIED.,.F.,.F.)
B_SPLINE_CURVE_WITH_KNOTS((3,3),(0.0270544913417777,0.043982818774189),
 .UNSPECIFIED.)
CURVE()
GEOMETRIC_REPRESENTATION_ITEM()
RATIONAL_B_SPLINE_CURVE((1.00082963690226,1.00067437544952,1.))
REPRESENTATION_ITEM('')
);
#396=(
BOUNDED_CURVE()
B_SPLINE_CURVE(2,(#66215,#66216,#66217),.UNSPECIFIED.,.F.,.F.)
B_SPLINE_CURVE_WITH_KNOTS((3,3),(0.,0.0169283274324427),.UNSPECIFIED.)
CURVE()
GEOMETRIC_REPRESENTATION_ITEM()
RATIONAL_B_SPLINE_CURVE((1.,1.00067437544511,1.00082963689683))
REPRESENTATION_ITEM('')
);
#397=(
BOUNDED_CURVE()
B_SPLINE_CURVE(2,(#66219,#66220,#66221),.UNSPECIFIED.,.F.,.F.)
B_SPLINE_CURVE_WITH_KNOTS((3,3),(0.0270544913417577,0.0439828187741891),
 .UNSPECIFIED.)
CURVE()
GEOMETRIC_REPRESENTATION_ITEM()
RATIONAL_B_SPLINE_CURVE((1.00082963689736,1.00067437544554,1.))
REPRESENTATION_ITEM('')
);
#398=(
BOUNDED_CURVE()
B_SPLINE_CURVE(2,(#66225,#66226,#66227),.UNSPECIFIED.,.F.,.F.)
B_SPLINE_CURVE_WITH_KNOTS((3,3),(0.,0.0169283274323561),.UNSPECIFIED.)
CURVE()
GEOMETRIC_REPRESENTATION_ITEM()
RATIONAL_B_SPLINE_CURVE((1.,1.00067437544767,1.00082963689998))
REPRESENTATION_ITEM('')
);
#399=(
BOUNDED_CURVE()
B_SPLINE_CURVE(2,(#66229,#66230,#66231),.UNSPECIFIED.,.F.,.F.)
B_SPLINE_CURVE_WITH_KNOTS((3,3),(0.0270544913417733,0.0439828187741891),
 .UNSPECIFIED.)
CURVE()
GEOMETRIC_REPRESENTATION_ITEM()
RATIONAL_B_SPLINE_CURVE((1.00082963689921,1.00067437544705,1.))
REPRESENTATION_ITEM('')
);
#400=(
BOUNDED_CURVE()
B_SPLINE_CURVE(2,(#66235,#66236,#66237),.UNSPECIFIED.,.F.,.F.)
B_SPLINE_CURVE_WITH_KNOTS((3,3),(0.,0.0169283274323988),.UNSPECIFIED.)
CURVE()
GEOMETRIC_REPRESENTATION_ITEM()
RATIONAL_B_SPLINE_CURVE((1.,1.00067437544932,1.000829636902))
REPRESENTATION_ITEM('')
);
#401=(
BOUNDED_CURVE()
B_SPLINE_CURVE(2,(#66239,#66240,#66241),.UNSPECIFIED.,.F.,.F.)
B_SPLINE_CURVE_WITH_KNOTS((3,3),(0.027054491341826,0.0439828187741891),
 .UNSPECIFIED.)
CURVE()
GEOMETRIC_REPRESENTATION_ITEM()
RATIONAL_B_SPLINE_CURVE((1.00082963690548,1.00067437545214,1.))
REPRESENTATION_ITEM('')
);
#402=(
BOUNDED_CURVE()
B_SPLINE_CURVE(2,(#66245,#66246,#66247),.UNSPECIFIED.,.F.,.F.)
B_SPLINE_CURVE_WITH_KNOTS((3,3),(0.,0.0169283274323669),.UNSPECIFIED.)
CURVE()
GEOMETRIC_REPRESENTATION_ITEM()
RATIONAL_B_SPLINE_CURVE((1.,1.0006743754502,1.00082963690309))
REPRESENTATION_ITEM('')
);
#403=(
BOUNDED_CURVE()
B_SPLINE_CURVE(2,(#66249,#66250,#66251),.UNSPECIFIED.,.F.,.F.)
B_SPLINE_CURVE_WITH_KNOTS((3,3),(0.0270544913418174,0.0439828187741891),
 .UNSPECIFIED.)
CURVE()
GEOMETRIC_REPRESENTATION_ITEM()
RATIONAL_B_SPLINE_CURVE((1.00082963690504,1.00067437545178,1.))
REPRESENTATION_ITEM('')
);
#404=(
BOUNDED_CURVE()
B_SPLINE_CURVE(2,(#66255,#66256,#66257),.UNSPECIFIED.,.F.,.F.)
B_SPLINE_CURVE_WITH_KNOTS((3,3),(0.,0.0169283274323848),.UNSPECIFIED.)
CURVE()
GEOMETRIC_REPRESENTATION_ITEM()
RATIONAL_B_SPLINE_CURVE((1.,1.00067437544897,1.00082963690158))
REPRESENTATION_ITEM('')
);
#405=(
BOUNDED_CURVE()
B_SPLINE_CURVE(2,(#66259,#66260,#66261),.UNSPECIFIED.,.F.,.F.)
B_SPLINE_CURVE_WITH_KNOTS((3,3),(0.0270544913417889,0.0439828187741892),
 .UNSPECIFIED.)
CURVE()
GEOMETRIC_REPRESENTATION_ITEM()
RATIONAL_B_SPLINE_CURVE((1.0008296369053,1.000674375452,1.))
REPRESENTATION_ITEM('')
);
#406=(
BOUNDED_CURVE()
B_SPLINE_CURVE(2,(#66265,#66266,#66267),.UNSPECIFIED.,.F.,.F.)
B_SPLINE_CURVE_WITH_KNOTS((3,3),(0.,0.0169283274323906),.UNSPECIFIED.)
CURVE()
GEOMETRIC_REPRESENTATION_ITEM()
RATIONAL_B_SPLINE_CURVE((1.,1.00067437544955,1.0008296369023))
REPRESENTATION_ITEM('')
);
#407=(
BOUNDED_CURVE()
B_SPLINE_CURVE(2,(#66269,#66270,#66271),.UNSPECIFIED.,.F.,.F.)
B_SPLINE_CURVE_WITH_KNOTS((3,3),(0.02705449134179,0.0439828187741892),
 .UNSPECIFIED.)
CURVE()
GEOMETRIC_REPRESENTATION_ITEM()
RATIONAL_B_SPLINE_CURVE((1.00082963689801,1.00067437544607,1.))
REPRESENTATION_ITEM('')
);
#408=(
BOUNDED_CURVE()
B_SPLINE_CURVE(2,(#66275,#66276,#66277),.UNSPECIFIED.,.F.,.F.)
B_SPLINE_CURVE_WITH_KNOTS((3,3),(0.,0.0169283274324299),.UNSPECIFIED.)
CURVE()
GEOMETRIC_REPRESENTATION_ITEM()
RATIONAL_B_SPLINE_CURVE((1.,1.00067437544605,1.00082963689799))
REPRESENTATION_ITEM('')
);
#409=(
BOUNDED_CURVE()
B_SPLINE_CURVE(2,(#66279,#66280,#66281),.UNSPECIFIED.,.F.,.F.)
B_SPLINE_CURVE_WITH_KNOTS((3,3),(0.0270544913418079,0.0439828187741891),
 .UNSPECIFIED.)
CURVE()
GEOMETRIC_REPRESENTATION_ITEM()
RATIONAL_B_SPLINE_CURVE((1.00082963690421,1.00067437545111,1.))
REPRESENTATION_ITEM('')
);
#410=(
BOUNDED_CURVE()
B_SPLINE_CURVE(2,(#66285,#66286,#66287),.UNSPECIFIED.,.F.,.F.)
B_SPLINE_CURVE_WITH_KNOTS((3,3),(0.,0.0169283274324045),.UNSPECIFIED.)
CURVE()
GEOMETRIC_REPRESENTATION_ITEM()
RATIONAL_B_SPLINE_CURVE((1.,1.00067437544845,1.00082963690094))
REPRESENTATION_ITEM('')
);
#411=(
BOUNDED_CURVE()
B_SPLINE_CURVE(2,(#66289,#66290,#66291),.UNSPECIFIED.,.F.,.F.)
B_SPLINE_CURVE_WITH_KNOTS((3,3),(0.0270544913417581,0.0439828187741892),
 .UNSPECIFIED.)
CURVE()
GEOMETRIC_REPRESENTATION_ITEM()
RATIONAL_B_SPLINE_CURVE((1.00082963689906,1.00067437544692,1.))
REPRESENTATION_ITEM('')
);
#412=(
BOUNDED_CURVE()
B_SPLINE_CURVE(2,(#66295,#66296,#66297),.UNSPECIFIED.,.F.,.F.)
B_SPLINE_CURVE_WITH_KNOTS((3,3),(0.,0.0169283274323899),.UNSPECIFIED.)
CURVE()
GEOMETRIC_REPRESENTATION_ITEM()
RATIONAL_B_SPLINE_CURVE((1.,1.00067437544785,1.0008296369002))
REPRESENTATION_ITEM('')
);
#413=(
BOUNDED_CURVE()
B_SPLINE_CURVE(2,(#66299,#66300,#66301),.UNSPECIFIED.,.F.,.F.)
B_SPLINE_CURVE_WITH_KNOTS((3,3),(0.0270544913417886,0.0439828187741892),
 .UNSPECIFIED.)
CURVE()
GEOMETRIC_REPRESENTATION_ITEM()
RATIONAL_B_SPLINE_CURVE((1.00082963689982,1.00067437544754,1.))
REPRESENTATION_ITEM('')
);
#414=(
BOUNDED_CURVE()
B_SPLINE_CURVE(2,(#66305,#66306,#66307),.UNSPECIFIED.,.F.,.F.)
B_SPLINE_CURVE_WITH_KNOTS((3,3),(0.,0.0169283274324022),.UNSPECIFIED.)
CURVE()
GEOMETRIC_REPRESENTATION_ITEM()
RATIONAL_B_SPLINE_CURVE((1.,1.0006743754471,1.00082963689928))
REPRESENTATION_ITEM('')
);
#415=(
BOUNDED_CURVE()
B_SPLINE_CURVE(2,(#66309,#66310,#66311),.UNSPECIFIED.,.F.,.F.)
B_SPLINE_CURVE_WITH_KNOTS((3,3),(0.02705449134173,0.0439828187741892),
 .UNSPECIFIED.)
CURVE()
GEOMETRIC_REPRESENTATION_ITEM()
RATIONAL_B_SPLINE_CURVE((1.00082963689882,1.00067437544673,1.))
REPRESENTATION_ITEM('')
);
#416=(
BOUNDED_CURVE()
B_SPLINE_CURVE(2,(#66315,#66316,#66317),.UNSPECIFIED.,.F.,.F.)
B_SPLINE_CURVE_WITH_KNOTS((3,3),(0.,0.0169283274323878),.UNSPECIFIED.)
CURVE()
GEOMETRIC_REPRESENTATION_ITEM()
RATIONAL_B_SPLINE_CURVE((1.,1.00067437545001,1.00082963690286))
REPRESENTATION_ITEM('')
);
#417=(
BOUNDED_CURVE()
B_SPLINE_CURVE(2,(#66319,#66320,#66321),.UNSPECIFIED.,.F.,.F.)
B_SPLINE_CURVE_WITH_KNOTS((3,3),(0.0270544913417747,0.043982818774189),
 .UNSPECIFIED.)
CURVE()
GEOMETRIC_REPRESENTATION_ITEM()
RATIONAL_B_SPLINE_CURVE((1.00082963690212,1.00067437544941,1.))
REPRESENTATION_ITEM('')
);
#418=(
BOUNDED_CURVE()
B_SPLINE_CURVE(2,(#66325,#66326,#66327),.UNSPECIFIED.,.F.,.F.)
B_SPLINE_CURVE_WITH_KNOTS((3,3),(0.,0.0169283274324349),.UNSPECIFIED.)
CURVE()
GEOMETRIC_REPRESENTATION_ITEM()
RATIONAL_B_SPLINE_CURVE((1.,1.00067437544449,1.00082963689607))
REPRESENTATION_ITEM('')
);
#419=(
BOUNDED_CURVE()
B_SPLINE_CURVE(2,(#66329,#66330,#66331),.UNSPECIFIED.,.F.,.F.)
B_SPLINE_CURVE_WITH_KNOTS((3,3),(0.0270544913417629,0.0439828187741891),
 .UNSPECIFIED.)
CURVE()
GEOMETRIC_REPRESENTATION_ITEM()
RATIONAL_B_SPLINE_CURVE((1.00082963689925,1.00067437544708,1.))
REPRESENTATION_ITEM('')
);
#420=(
BOUNDED_CURVE()
B_SPLINE_CURVE(2,(#66335,#66336,#66337),.UNSPECIFIED.,.F.,.F.)
B_SPLINE_CURVE_WITH_KNOTS((3,3),(0.,0.01692832743245),.UNSPECIFIED.)
CURVE()
GEOMETRIC_REPRESENTATION_ITEM()
RATIONAL_B_SPLINE_CURVE((1.,1.0006743754471,1.00082963689927))
REPRESENTATION_ITEM('')
);
#421=(
BOUNDED_CURVE()
B_SPLINE_CURVE(2,(#66339,#66340,#66341),.UNSPECIFIED.,.F.,.F.)
B_SPLINE_CURVE_WITH_KNOTS((3,3),(0.027054491341727,0.0439828187741896),
 .UNSPECIFIED.)
CURVE()
GEOMETRIC_REPRESENTATION_ITEM()
RATIONAL_B_SPLINE_CURVE((1.00082963689923,1.00067437544706,1.))
REPRESENTATION_ITEM('')
);
#422=(
BOUNDED_CURVE()
B_SPLINE_CURVE(2,(#66345,#66346,#66347),.UNSPECIFIED.,.F.,.F.)
B_SPLINE_CURVE_WITH_KNOTS((3,3),(0.,0.0169283274324584),.UNSPECIFIED.)
CURVE()
GEOMETRIC_REPRESENTATION_ITEM()
RATIONAL_B_SPLINE_CURVE((1.,1.00067437544543,1.00082963689722))
REPRESENTATION_ITEM('')
);
#423=(
BOUNDED_CURVE()
B_SPLINE_CURVE(2,(#66349,#66350,#66351),.UNSPECIFIED.,.F.,.F.)
B_SPLINE_CURVE_WITH_KNOTS((3,3),(0.0270544913416968,0.0439828187741891),
 .UNSPECIFIED.)
CURVE()
GEOMETRIC_REPRESENTATION_ITEM()
RATIONAL_B_SPLINE_CURVE((1.00082963689609,1.00067437544451,1.))
REPRESENTATION_ITEM('')
);
#424=(
BOUNDED_CURVE()
B_SPLINE_CURVE(2,(#66354,#66355,#66356),.UNSPECIFIED.,.F.,.F.)
B_SPLINE_CURVE_WITH_KNOTS((3,3),(0.,0.0169283274323624),.UNSPECIFIED.)
CURVE()
GEOMETRIC_REPRESENTATION_ITEM()
RATIONAL_B_SPLINE_CURVE((1.,1.00067437544963,1.0008296369024))
REPRESENTATION_ITEM('')
);
#425=(
BOUNDED_CURVE()
B_SPLINE_CURVE(2,(#82193,#82194,#82195),.UNSPECIFIED.,.F.,.F.)
B_SPLINE_CURVE_WITH_KNOTS((3,3),(0.,0.0169283274323949),.UNSPECIFIED.)
CURVE()
GEOMETRIC_REPRESENTATION_ITEM()
RATIONAL_B_SPLINE_CURVE((1.,1.00067437544385,1.00082963689528))
REPRESENTATION_ITEM('')
);
#426=(
BOUNDED_CURVE()
B_SPLINE_CURVE(2,(#82200,#82201,#82202),.UNSPECIFIED.,.F.,.F.)
B_SPLINE_CURVE_WITH_KNOTS((3,3),(0.027054491341878,0.0439828187741921),
 .UNSPECIFIED.)
CURVE()
GEOMETRIC_REPRESENTATION_ITEM()
RATIONAL_B_SPLINE_CURVE((1.00082963691689,1.00067437546141,1.))
REPRESENTATION_ITEM('')
);
#427=(
BOUNDED_CURVE()
B_SPLINE_CURVE(2,(#82209,#82210,#82211),.UNSPECIFIED.,.F.,.F.)
B_SPLINE_CURVE_WITH_KNOTS((3,3),(0.0270544913416899,0.0439828187741926),
 .UNSPECIFIED.)
CURVE()
GEOMETRIC_REPRESENTATION_ITEM()
RATIONAL_B_SPLINE_CURVE((1.00082963689398,1.0006743754428,1.))
REPRESENTATION_ITEM('')
);
#428=(
BOUNDED_CURVE()
B_SPLINE_CURVE(2,(#82215,#82216,#82217),.UNSPECIFIED.,.F.,.F.)
B_SPLINE_CURVE_WITH_KNOTS((3,3),(0.,0.016928327432378),.UNSPECIFIED.)
CURVE()
GEOMETRIC_REPRESENTATION_ITEM()
RATIONAL_B_SPLINE_CURVE((1.,1.00067437544454,1.00082963689613))
REPRESENTATION_ITEM('')
);
#429=(
BOUNDED_CURVE()
B_SPLINE_CURVE(2,(#82219,#82220,#82221),.UNSPECIFIED.,.F.,.F.)
B_SPLINE_CURVE_WITH_KNOTS((3,3),(0.0270544913417352,0.0439828187741927),
 .UNSPECIFIED.)
CURVE()
GEOMETRIC_REPRESENTATION_ITEM()
RATIONAL_B_SPLINE_CURVE((1.00082963690354,1.00067437545056,1.))
REPRESENTATION_ITEM('')
);
#430=(
BOUNDED_CURVE()
B_SPLINE_CURVE(2,(#82225,#82226,#82227),.UNSPECIFIED.,.F.,.F.)
B_SPLINE_CURVE_WITH_KNOTS((3,3),(0.,0.0169283274324875),.UNSPECIFIED.)
CURVE()
GEOMETRIC_REPRESENTATION_ITEM()
RATIONAL_B_SPLINE_CURVE((1.,1.00067437544421,1.00082963689573))
REPRESENTATION_ITEM('')
);
#431=(
BOUNDED_CURVE()
B_SPLINE_CURVE(2,(#82229,#82230,#82231),.UNSPECIFIED.,.F.,.F.)
B_SPLINE_CURVE_WITH_KNOTS((3,3),(0.0270544913417807,0.0439828187741914),
 .UNSPECIFIED.)
CURVE()
GEOMETRIC_REPRESENTATION_ITEM()
RATIONAL_B_SPLINE_CURVE((1.00082963690149,1.0006743754489,1.))
REPRESENTATION_ITEM('')
);
#432=(
BOUNDED_CURVE()
B_SPLINE_CURVE(2,(#82235,#82236,#82237),.UNSPECIFIED.,.F.,.F.)
B_SPLINE_CURVE_WITH_KNOTS((3,3),(0.,0.0169283274326477),.UNSPECIFIED.)
CURVE()
GEOMETRIC_REPRESENTATION_ITEM()
RATIONAL_B_SPLINE_CURVE((1.,1.00067437542316,1.00082963686982))
REPRESENTATION_ITEM('')
);
#433=(
BOUNDED_CURVE()
B_SPLINE_CURVE(2,(#82239,#82240,#82241),.UNSPECIFIED.,.F.,.F.)
B_SPLINE_CURVE_WITH_KNOTS((3,3),(0.0270544913419272,0.0439828187741907),
 .UNSPECIFIED.)
CURVE()
GEOMETRIC_REPRESENTATION_ITEM()
RATIONAL_B_SPLINE_CURVE((1.00082963692254,1.000674375466,1.))
REPRESENTATION_ITEM('')
);
#434=(
BOUNDED_CURVE()
B_SPLINE_CURVE(2,(#82245,#82246,#82247),.UNSPECIFIED.,.F.,.F.)
B_SPLINE_CURVE_WITH_KNOTS((3,3),(0.,0.0169283274324231),.UNSPECIFIED.)
CURVE()
GEOMETRIC_REPRESENTATION_ITEM()
RATIONAL_B_SPLINE_CURVE((1.,1.00067437544818,1.00082963690061))
REPRESENTATION_ITEM('')
);
#435=(
BOUNDED_CURVE()
B_SPLINE_CURVE(2,(#82249,#82250,#82251),.UNSPECIFIED.,.F.,.F.)
B_SPLINE_CURVE_WITH_KNOTS((3,3),(0.0270544913416623,0.0439828187741918),
 .UNSPECIFIED.)
CURVE()
GEOMETRIC_REPRESENTATION_ITEM()
RATIONAL_B_SPLINE_CURVE((1.00082963688688,1.00067437543703,1.))
REPRESENTATION_ITEM('')
);
#436=(
BOUNDED_CURVE()
B_SPLINE_CURVE(2,(#82255,#82256,#82257),.UNSPECIFIED.,.F.,.F.)
B_SPLINE_CURVE_WITH_KNOTS((3,3),(0.,0.016928327432524),.UNSPECIFIED.)
CURVE()
GEOMETRIC_REPRESENTATION_ITEM()
RATIONAL_B_SPLINE_CURVE((1.,1.00067437543311,1.00082963688207))
REPRESENTATION_ITEM('')
);
#437=(
BOUNDED_CURVE()
B_SPLINE_CURVE(2,(#82259,#82260,#82261),.UNSPECIFIED.,.F.,.F.)
B_SPLINE_CURVE_WITH_KNOTS((3,3),(0.0270544913417664,0.0439828187741907),
 .UNSPECIFIED.)
CURVE()
GEOMETRIC_REPRESENTATION_ITEM()
RATIONAL_B_SPLINE_CURVE((1.00082963689261,1.00067437544168,1.))
REPRESENTATION_ITEM('')
);
#438=(
BOUNDED_CURVE()
B_SPLINE_CURVE(2,(#82265,#82266,#82267),.UNSPECIFIED.,.F.,.F.)
B_SPLINE_CURVE_WITH_KNOTS((3,3),(0.,0.0169283274324059),.UNSPECIFIED.)
CURVE()
GEOMETRIC_REPRESENTATION_ITEM()
RATIONAL_B_SPLINE_CURVE((1.,1.00067437545304,1.00082963690658))
REPRESENTATION_ITEM('')
);
#439=(
BOUNDED_CURVE()
B_SPLINE_CURVE(2,(#82269,#82270,#82271),.UNSPECIFIED.,.F.,.F.)
B_SPLINE_CURVE_WITH_KNOTS((3,3),(0.0270544913417434,0.0439828187741902),
 .UNSPECIFIED.)
CURVE()
GEOMETRIC_REPRESENTATION_ITEM()
RATIONAL_B_SPLINE_CURVE((1.0008296368963,1.00067437544468,1.))
REPRESENTATION_ITEM('')
);
#440=(
BOUNDED_CURVE()
B_SPLINE_CURVE(2,(#82275,#82276,#82277),.UNSPECIFIED.,.F.,.F.)
B_SPLINE_CURVE_WITH_KNOTS((3,3),(0.,0.0169283274323925),.UNSPECIFIED.)
CURVE()
GEOMETRIC_REPRESENTATION_ITEM()
RATIONAL_B_SPLINE_CURVE((1.,1.00067437545304,1.00082963690659))
REPRESENTATION_ITEM('')
);
#441=(
BOUNDED_CURVE()
B_SPLINE_CURVE(2,(#82279,#82280,#82281),.UNSPECIFIED.,.F.,.F.)
B_SPLINE_CURVE_WITH_KNOTS((3,3),(0.0270544913417717,0.0439828187741908),
 .UNSPECIFIED.)
CURVE()
GEOMETRIC_REPRESENTATION_ITEM()
RATIONAL_B_SPLINE_CURVE((1.00082963689559,1.0006743754441,1.))
REPRESENTATION_ITEM('')
);
#442=(
BOUNDED_CURVE()
B_SPLINE_CURVE(2,(#82285,#82286,#82287),.UNSPECIFIED.,.F.,.F.)
B_SPLINE_CURVE_WITH_KNOTS((3,3),(0.,0.0169283274324336),.UNSPECIFIED.)
CURVE()
GEOMETRIC_REPRESENTATION_ITEM()
RATIONAL_B_SPLINE_CURVE((1.,1.00067437544179,1.00082963689274))
REPRESENTATION_ITEM('')
);
#443=(
BOUNDED_CURVE()
B_SPLINE_CURVE(2,(#82289,#82290,#82291),.UNSPECIFIED.,.F.,.F.)
B_SPLINE_CURVE_WITH_KNOTS((3,3),(0.0270544913417271,0.04398281877419),
 .UNSPECIFIED.)
CURVE()
GEOMETRIC_REPRESENTATION_ITEM()
RATIONAL_B_SPLINE_CURVE((1.00082963690167,1.00067437544904,1.))
REPRESENTATION_ITEM('')
);
#444=(
BOUNDED_CURVE()
B_SPLINE_CURVE(2,(#82295,#82296,#82297),.UNSPECIFIED.,.F.,.F.)
B_SPLINE_CURVE_WITH_KNOTS((3,3),(0.,0.0169283274323986),.UNSPECIFIED.)
CURVE()
GEOMETRIC_REPRESENTATION_ITEM()
RATIONAL_B_SPLINE_CURVE((1.,1.00067437544723,1.00082963689944))
REPRESENTATION_ITEM('')
);
#445=(
BOUNDED_CURVE()
B_SPLINE_CURVE(2,(#82299,#82300,#82301),.UNSPECIFIED.,.F.,.F.)
B_SPLINE_CURVE_WITH_KNOTS((3,3),(0.0270544913417658,0.0439828187741907),
 .UNSPECIFIED.)
CURVE()
GEOMETRIC_REPRESENTATION_ITEM()
RATIONAL_B_SPLINE_CURVE((1.00082963689458,1.00067437544328,1.))
REPRESENTATION_ITEM('')
);
#446=(
BOUNDED_CURVE()
B_SPLINE_CURVE(2,(#82305,#82306,#82307),.UNSPECIFIED.,.F.,.F.)
B_SPLINE_CURVE_WITH_KNOTS((3,3),(0.,0.0169283274323524),.UNSPECIFIED.)
CURVE()
GEOMETRIC_REPRESENTATION_ITEM()
RATIONAL_B_SPLINE_CURVE((1.,1.00067437545192,1.00082963690521))
REPRESENTATION_ITEM('')
);
#447=(
BOUNDED_CURVE()
B_SPLINE_CURVE(2,(#82309,#82310,#82311),.UNSPECIFIED.,.F.,.F.)
B_SPLINE_CURVE_WITH_KNOTS((3,3),(0.0270544913417437,0.0439828187741922),
 .UNSPECIFIED.)
CURVE()
GEOMETRIC_REPRESENTATION_ITEM()
RATIONAL_B_SPLINE_CURVE((1.0008296368979,1.00067437544598,1.))
REPRESENTATION_ITEM('')
);
#448=(
BOUNDED_CURVE()
B_SPLINE_CURVE(2,(#82315,#82316,#82317),.UNSPECIFIED.,.F.,.F.)
B_SPLINE_CURVE_WITH_KNOTS((3,3),(0.,0.0169283274322953),.UNSPECIFIED.)
CURVE()
GEOMETRIC_REPRESENTATION_ITEM()
RATIONAL_B_SPLINE_CURVE((1.,1.00067437546283,1.00082963691863))
REPRESENTATION_ITEM('')
);
#449=(
BOUNDED_CURVE()
B_SPLINE_CURVE(2,(#82319,#82320,#82321),.UNSPECIFIED.,.F.,.F.)
B_SPLINE_CURVE_WITH_KNOTS((3,3),(0.027054491341941,0.0439828187741898),
 .UNSPECIFIED.)
CURVE()
GEOMETRIC_REPRESENTATION_ITEM()
RATIONAL_B_SPLINE_CURVE((1.00082963692429,1.00067437546742,1.))
REPRESENTATION_ITEM('')
);
#450=(
BOUNDED_CURVE()
B_SPLINE_CURVE(2,(#82325,#82326,#82327),.UNSPECIFIED.,.F.,.F.)
B_SPLINE_CURVE_WITH_KNOTS((3,3),(0.,0.0169283274322328),.UNSPECIFIED.)
CURVE()
GEOMETRIC_REPRESENTATION_ITEM()
RATIONAL_B_SPLINE_CURVE((1.,1.00067437546617,1.00082963692274))
REPRESENTATION_ITEM('')
);
#451=(
BOUNDED_CURVE()
B_SPLINE_CURVE(2,(#82329,#82330,#82331),.UNSPECIFIED.,.F.,.F.)
B_SPLINE_CURVE_WITH_KNOTS((3,3),(0.0270544913418974,0.0439828187741896),
 .UNSPECIFIED.)
CURVE()
GEOMETRIC_REPRESENTATION_ITEM()
RATIONAL_B_SPLINE_CURVE((1.00082963691993,1.00067437546389,1.))
REPRESENTATION_ITEM('')
);
#452=(
BOUNDED_CURVE()
B_SPLINE_CURVE(2,(#82335,#82336,#82337),.UNSPECIFIED.,.F.,.F.)
B_SPLINE_CURVE_WITH_KNOTS((3,3),(0.,0.0169283274324175),.UNSPECIFIED.)
CURVE()
GEOMETRIC_REPRESENTATION_ITEM()
RATIONAL_B_SPLINE_CURVE((1.,1.00067437544813,1.00082963690054))
REPRESENTATION_ITEM('')
);
#453=(
BOUNDED_CURVE()
B_SPLINE_CURVE(2,(#82339,#82340,#82341),.UNSPECIFIED.,.F.,.F.)
B_SPLINE_CURVE_WITH_KNOTS((3,3),(0.0270544913419329,0.0439828187741885),
 .UNSPECIFIED.)
CURVE()
GEOMETRIC_REPRESENTATION_ITEM()
RATIONAL_B_SPLINE_CURVE((1.00082963691274,1.00067437545804,1.))
REPRESENTATION_ITEM('')
);
#454=(
BOUNDED_CURVE()
B_SPLINE_CURVE(2,(#82345,#82346,#82347),.UNSPECIFIED.,.F.,.F.)
B_SPLINE_CURVE_WITH_KNOTS((3,3),(0.,0.0169283274323868),.UNSPECIFIED.)
CURVE()
GEOMETRIC_REPRESENTATION_ITEM()
RATIONAL_B_SPLINE_CURVE((1.,1.00067437545154,1.00082963690474))
REPRESENTATION_ITEM('')
);
#455=(
BOUNDED_CURVE()
B_SPLINE_CURVE(2,(#82349,#82350,#82351),.UNSPECIFIED.,.F.,.F.)
B_SPLINE_CURVE_WITH_KNOTS((3,3),(0.0270544913418465,0.0439828187741911),
 .UNSPECIFIED.)
CURVE()
GEOMETRIC_REPRESENTATION_ITEM()
RATIONAL_B_SPLINE_CURVE((1.00082963692434,1.00067437546747,1.))
REPRESENTATION_ITEM('')
);
#456=(
BOUNDED_CURVE()
B_SPLINE_CURVE(2,(#82355,#82356,#82357),.UNSPECIFIED.,.F.,.F.)
B_SPLINE_CURVE_WITH_KNOTS((3,3),(0.,0.016928327432223),.UNSPECIFIED.)
CURVE()
GEOMETRIC_REPRESENTATION_ITEM()
RATIONAL_B_SPLINE_CURVE((1.,1.00067437546906,1.00082963692629))
REPRESENTATION_ITEM('')
);
#457=(
BOUNDED_CURVE()
B_SPLINE_CURVE(2,(#82359,#82360,#82361),.UNSPECIFIED.,.F.,.F.)
B_SPLINE_CURVE_WITH_KNOTS((3,3),(0.0270544913418792,0.0439828187741897),
 .UNSPECIFIED.)
CURVE()
GEOMETRIC_REPRESENTATION_ITEM()
RATIONAL_B_SPLINE_CURVE((1.0008296369223,1.00067437546581,1.))
REPRESENTATION_ITEM('')
);
#458=(
BOUNDED_CURVE()
B_SPLINE_CURVE(2,(#82365,#82366,#82367),.UNSPECIFIED.,.F.,.F.)
B_SPLINE_CURVE_WITH_KNOTS((3,3),(0.,0.0169283274325481),.UNSPECIFIED.)
CURVE()
GEOMETRIC_REPRESENTATION_ITEM()
RATIONAL_B_SPLINE_CURVE((1.,1.00067437544352,1.00082963689487))
REPRESENTATION_ITEM('')
);
#459=(
BOUNDED_CURVE()
B_SPLINE_CURVE(2,(#82369,#82370,#82371),.UNSPECIFIED.,.F.,.F.)
B_SPLINE_CURVE_WITH_KNOTS((3,3),(0.0270544913417793,0.0439828187741915),
 .UNSPECIFIED.)
CURVE()
GEOMETRIC_REPRESENTATION_ITEM()
RATIONAL_B_SPLINE_CURVE((1.00082963691087,1.00067437545653,1.))
REPRESENTATION_ITEM('')
);
#460=(
BOUNDED_CURVE()
B_SPLINE_CURVE(2,(#82375,#82376,#82377),.UNSPECIFIED.,.F.,.F.)
B_SPLINE_CURVE_WITH_KNOTS((3,3),(0.,0.0169283274323758),.UNSPECIFIED.)
CURVE()
GEOMETRIC_REPRESENTATION_ITEM()
RATIONAL_B_SPLINE_CURVE((1.,1.00067437544934,1.00082963690204))
REPRESENTATION_ITEM('')
);
#461=(
BOUNDED_CURVE()
B_SPLINE_CURVE(2,(#82379,#82380,#82381),.UNSPECIFIED.,.F.,.F.)
B_SPLINE_CURVE_WITH_KNOTS((3,3),(0.0270544913417685,0.0439828187741897),
 .UNSPECIFIED.)
CURVE()
GEOMETRIC_REPRESENTATION_ITEM()
RATIONAL_B_SPLINE_CURVE((1.00082963689898,1.00067437544686,1.))
REPRESENTATION_ITEM('')
);
#462=(
BOUNDED_CURVE()
B_SPLINE_CURVE(2,(#82385,#82386,#82387),.UNSPECIFIED.,.F.,.F.)
B_SPLINE_CURVE_WITH_KNOTS((3,3),(0.,0.0169283274324469),.UNSPECIFIED.)
CURVE()
GEOMETRIC_REPRESENTATION_ITEM()
RATIONAL_B_SPLINE_CURVE((1.,1.00067437544897,1.00082963690158))
REPRESENTATION_ITEM('')
);
#463=(
BOUNDED_CURVE()
B_SPLINE_CURVE(2,(#82389,#82390,#82391),.UNSPECIFIED.,.F.,.F.)
B_SPLINE_CURVE_WITH_KNOTS((3,3),(0.0270544913418427,0.04398281877419),
 .UNSPECIFIED.)
CURVE()
GEOMETRIC_REPRESENTATION_ITEM()
RATIONAL_B_SPLINE_CURVE((1.00082963692428,1.00067437546742,1.))
REPRESENTATION_ITEM('')
);
#464=(
BOUNDED_CURVE()
B_SPLINE_CURVE(2,(#82396,#82397,#82398),.UNSPECIFIED.,.F.,.F.)
B_SPLINE_CURVE_WITH_KNOTS((3,3),(0.,0.0169283274326309),.UNSPECIFIED.)
CURVE()
GEOMETRIC_REPRESENTATION_ITEM()
RATIONAL_B_SPLINE_CURVE((1.,1.00067437542865,1.00082963687657))
REPRESENTATION_ITEM('')
);
#465=(
BOUNDED_CURVE()
B_SPLINE_CURVE(2,(#82400,#82401,#82402),.UNSPECIFIED.,.F.,.F.)
B_SPLINE_CURVE_WITH_KNOTS((3,3),(0.0270544913417494,0.0439828187741933),
 .UNSPECIFIED.)
CURVE()
GEOMETRIC_REPRESENTATION_ITEM()
RATIONAL_B_SPLINE_CURVE((1.00082963689727,1.00067437544547,1.))
REPRESENTATION_ITEM('')
);
#466=(
BOUNDED_CURVE()
B_SPLINE_CURVE(2,(#82406,#82407,#82408),.UNSPECIFIED.,.F.,.F.)
B_SPLINE_CURVE_WITH_KNOTS((3,3),(0.,0.0169283274321813),.UNSPECIFIED.)
CURVE()
GEOMETRIC_REPRESENTATION_ITEM()
RATIONAL_B_SPLINE_CURVE((1.,1.00067437546612,1.00082963692269))
REPRESENTATION_ITEM('')
);
#467=(
BOUNDED_CURVE()
B_SPLINE_CURVE(2,(#82410,#82411,#82412),.UNSPECIFIED.,.F.,.F.)
B_SPLINE_CURVE_WITH_KNOTS((3,3),(0.0270544913418634,0.0439828187741926),
 .UNSPECIFIED.)
CURVE()
GEOMETRIC_REPRESENTATION_ITEM()
RATIONAL_B_SPLINE_CURVE((1.00082963691427,1.00067437545928,1.))
REPRESENTATION_ITEM('')
);
#468=(
BOUNDED_CURVE()
B_SPLINE_CURVE(2,(#82416,#82417,#82418),.UNSPECIFIED.,.F.,.F.)
B_SPLINE_CURVE_WITH_KNOTS((3,3),(0.,0.0169283274324664),.UNSPECIFIED.)
CURVE()
GEOMETRIC_REPRESENTATION_ITEM()
RATIONAL_B_SPLINE_CURVE((1.,1.00067437544028,1.00082963689088))
REPRESENTATION_ITEM('')
);
#469=(
BOUNDED_CURVE()
B_SPLINE_CURVE(2,(#82420,#82421,#82422),.UNSPECIFIED.,.F.,.F.)
B_SPLINE_CURVE_WITH_KNOTS((3,3),(0.0270544913418777,0.0439828187741926),
 .UNSPECIFIED.)
CURVE()
GEOMETRIC_REPRESENTATION_ITEM()
RATIONAL_B_SPLINE_CURVE((1.00082963691853,1.00067437546274,1.))
REPRESENTATION_ITEM('')
);
#470=(
BOUNDED_CURVE()
B_SPLINE_CURVE(2,(#82426,#82427,#82428),.UNSPECIFIED.,.F.,.F.)
B_SPLINE_CURVE_WITH_KNOTS((3,3),(0.,0.0169283274323108),.UNSPECIFIED.)
CURVE()
GEOMETRIC_REPRESENTATION_ITEM()
RATIONAL_B_SPLINE_CURVE((1.,1.00067437545943,1.00082963691444))
REPRESENTATION_ITEM('')
);
#471=(
BOUNDED_CURVE()
B_SPLINE_CURVE(2,(#82430,#82431,#82432),.UNSPECIFIED.,.F.,.F.)
B_SPLINE_CURVE_WITH_KNOTS((3,3),(0.0270544913417395,0.0439828187741916),
 .UNSPECIFIED.)
CURVE()
GEOMETRIC_REPRESENTATION_ITEM()
RATIONAL_B_SPLINE_CURVE((1.00082963689027,1.00067437543978,1.))
REPRESENTATION_ITEM('')
);
#472=(
BOUNDED_CURVE()
B_SPLINE_CURVE(2,(#82436,#82437,#82438),.UNSPECIFIED.,.F.,.F.)
B_SPLINE_CURVE_WITH_KNOTS((3,3),(0.,0.0169283274323638),.UNSPECIFIED.)
CURVE()
GEOMETRIC_REPRESENTATION_ITEM()
RATIONAL_B_SPLINE_CURVE((1.,1.00067437545187,1.00082963690515))
REPRESENTATION_ITEM('')
);
#473=(
BOUNDED_CURVE()
B_SPLINE_CURVE(2,(#82440,#82441,#82442),.UNSPECIFIED.,.F.,.F.)
B_SPLINE_CURVE_WITH_KNOTS((3,3),(0.0270544913417076,0.0439828187741916),
 .UNSPECIFIED.)
CURVE()
GEOMETRIC_REPRESENTATION_ITEM()
RATIONAL_B_SPLINE_CURVE((1.00082963689143,1.00067437544072,1.))
REPRESENTATION_ITEM('')
);
#474=(
BOUNDED_CURVE()
B_SPLINE_CURVE(2,(#82446,#82447,#82448),.UNSPECIFIED.,.F.,.F.)
B_SPLINE_CURVE_WITH_KNOTS((3,3),(0.,0.0169283274324132),.UNSPECIFIED.)
CURVE()
GEOMETRIC_REPRESENTATION_ITEM()
RATIONAL_B_SPLINE_CURVE((1.,1.00067437545166,1.00082963690489))
REPRESENTATION_ITEM('')
);
#475=(
BOUNDED_CURVE()
B_SPLINE_CURVE(2,(#82450,#82451,#82452),.UNSPECIFIED.,.F.,.F.)
B_SPLINE_CURVE_WITH_KNOTS((3,3),(0.0270544913417581,0.0439828187741926),
 .UNSPECIFIED.)
CURVE()
GEOMETRIC_REPRESENTATION_ITEM()
RATIONAL_B_SPLINE_CURVE((1.00082963689712,1.00067437544534,1.))
REPRESENTATION_ITEM('')
);
#476=(
BOUNDED_CURVE()
B_SPLINE_CURVE(2,(#82456,#82457,#82458),.UNSPECIFIED.,.F.,.F.)
B_SPLINE_CURVE_WITH_KNOTS((3,3),(0.,0.0169283274323258),.UNSPECIFIED.)
CURVE()
GEOMETRIC_REPRESENTATION_ITEM()
RATIONAL_B_SPLINE_CURVE((1.,1.00067437545421,1.00082963690803))
REPRESENTATION_ITEM('')
);
#477=(
BOUNDED_CURVE()
B_SPLINE_CURVE(2,(#82460,#82461,#82462),.UNSPECIFIED.,.F.,.F.)
B_SPLINE_CURVE_WITH_KNOTS((3,3),(0.0270544913417721,0.0439828187741926),
 .UNSPECIFIED.)
CURVE()
GEOMETRIC_REPRESENTATION_ITEM()
RATIONAL_B_SPLINE_CURVE((1.00082963689922,1.00067437544705,1.))
REPRESENTATION_ITEM('')
);
#478=(
BOUNDED_CURVE()
B_SPLINE_CURVE(2,(#82466,#82467,#82468),.UNSPECIFIED.,.F.,.F.)
B_SPLINE_CURVE_WITH_KNOTS((3,3),(0.,0.0169283274323368),.UNSPECIFIED.)
CURVE()
GEOMETRIC_REPRESENTATION_ITEM()
RATIONAL_B_SPLINE_CURVE((1.,1.00067437545165,1.00082963690488))
REPRESENTATION_ITEM('')
);
#479=(
BOUNDED_CURVE()
B_SPLINE_CURVE(2,(#82470,#82471,#82472),.UNSPECIFIED.,.F.,.F.)
B_SPLINE_CURVE_WITH_KNOTS((3,3),(0.0270544913418129,0.0439828187741918),
 .UNSPECIFIED.)
CURVE()
GEOMETRIC_REPRESENTATION_ITEM()
RATIONAL_B_SPLINE_CURVE((1.00082963690488,1.00067437545165,1.))
REPRESENTATION_ITEM('')
);
#480=(
BOUNDED_CURVE()
B_SPLINE_CURVE(2,(#82476,#82477,#82478),.UNSPECIFIED.,.F.,.F.)
B_SPLINE_CURVE_WITH_KNOTS((3,3),(0.,0.0169283274323829),.UNSPECIFIED.)
CURVE()
GEOMETRIC_REPRESENTATION_ITEM()
RATIONAL_B_SPLINE_CURVE((1.,1.00067437545407,1.00082963690785))
REPRESENTATION_ITEM('')
);
#481=(
BOUNDED_CURVE()
B_SPLINE_CURVE(2,(#82480,#82481,#82482),.UNSPECIFIED.,.F.,.F.)
B_SPLINE_CURVE_WITH_KNOTS((3,3),(0.0270544913418384,0.0439828187741921),
 .UNSPECIFIED.)
CURVE()
GEOMETRIC_REPRESENTATION_ITEM()
RATIONAL_B_SPLINE_CURVE((1.00082963690821,1.00067437545436,1.))
REPRESENTATION_ITEM('')
);
#482=(
BOUNDED_CURVE()
B_SPLINE_CURVE(2,(#82486,#82487,#82488),.UNSPECIFIED.,.F.,.F.)
B_SPLINE_CURVE_WITH_KNOTS((3,3),(0.,0.0169283274323058),.UNSPECIFIED.)
CURVE()
GEOMETRIC_REPRESENTATION_ITEM()
RATIONAL_B_SPLINE_CURVE((1.,1.00067437546416,1.00082963692027))
REPRESENTATION_ITEM('')
);
#483=(
BOUNDED_CURVE()
B_SPLINE_CURVE(2,(#82490,#82491,#82492),.UNSPECIFIED.,.F.,.F.)
B_SPLINE_CURVE_WITH_KNOTS((3,3),(0.0270544913418702,0.0439828187741907),
 .UNSPECIFIED.)
CURVE()
GEOMETRIC_REPRESENTATION_ITEM()
RATIONAL_B_SPLINE_CURVE((1.00082963692018,1.00067437546409,1.))
REPRESENTATION_ITEM('')
);
#484=(
BOUNDED_CURVE()
B_SPLINE_CURVE(2,(#82496,#82497,#82498),.UNSPECIFIED.,.F.,.F.)
B_SPLINE_CURVE_WITH_KNOTS((3,3),(0.,0.0169283274324372),.UNSPECIFIED.)
CURVE()
GEOMETRIC_REPRESENTATION_ITEM()
RATIONAL_B_SPLINE_CURVE((1.,1.00067437545102,1.0008296369041))
REPRESENTATION_ITEM('')
);
#485=(
BOUNDED_CURVE()
B_SPLINE_CURVE(2,(#82500,#82501,#82502),.UNSPECIFIED.,.F.,.F.)
B_SPLINE_CURVE_WITH_KNOTS((3,3),(0.0270544913418863,0.0439828187741916),
 .UNSPECIFIED.)
CURVE()
GEOMETRIC_REPRESENTATION_ITEM()
RATIONAL_B_SPLINE_CURVE((1.00082963691192,1.00067437545738,1.))
REPRESENTATION_ITEM('')
);
#486=(
BOUNDED_CURVE()
B_SPLINE_CURVE(2,(#82506,#82507,#82508),.UNSPECIFIED.,.F.,.F.)
B_SPLINE_CURVE_WITH_KNOTS((3,3),(0.,0.0169283274323833),.UNSPECIFIED.)
CURVE()
GEOMETRIC_REPRESENTATION_ITEM()
RATIONAL_B_SPLINE_CURVE((1.,1.00067437544615,1.00082963689811))
REPRESENTATION_ITEM('')
);
#487=(
BOUNDED_CURVE()
B_SPLINE_CURVE(2,(#82510,#82511,#82512),.UNSPECIFIED.,.F.,.F.)
B_SPLINE_CURVE_WITH_KNOTS((3,3),(0.0270544913417211,0.0439828187741927),
 .UNSPECIFIED.)
CURVE()
GEOMETRIC_REPRESENTATION_ITEM()
RATIONAL_B_SPLINE_CURVE((1.00082963690189,1.00067437544923,1.))
REPRESENTATION_ITEM('')
);
#488=(
BOUNDED_CURVE()
B_SPLINE_CURVE(2,(#82516,#82517,#82518),.UNSPECIFIED.,.F.,.F.)
B_SPLINE_CURVE_WITH_KNOTS((3,3),(0.,0.0169283274324049),.UNSPECIFIED.)
CURVE()
GEOMETRIC_REPRESENTATION_ITEM()
RATIONAL_B_SPLINE_CURVE((1.,1.00067437545222,1.00082963690557))
REPRESENTATION_ITEM('')
);
#489=(
BOUNDED_CURVE()
B_SPLINE_CURVE(2,(#82520,#82521,#82522),.UNSPECIFIED.,.F.,.F.)
B_SPLINE_CURVE_WITH_KNOTS((3,3),(0.0270544913418404,0.0439828187741917),
 .UNSPECIFIED.)
CURVE()
GEOMETRIC_REPRESENTATION_ITEM()
RATIONAL_B_SPLINE_CURVE((1.00082963691628,1.00067437546092,1.))
REPRESENTATION_ITEM('')
);
#490=(
BOUNDED_CURVE()
B_SPLINE_CURVE(2,(#82526,#82527,#82528),.UNSPECIFIED.,.F.,.F.)
B_SPLINE_CURVE_WITH_KNOTS((3,3),(0.,0.016928327432346),.UNSPECIFIED.)
CURVE()
GEOMETRIC_REPRESENTATION_ITEM()
RATIONAL_B_SPLINE_CURVE((1.,1.00067437545423,1.00082963690805))
REPRESENTATION_ITEM('')
);
#491=(
BOUNDED_CURVE()
B_SPLINE_CURVE(2,(#82530,#82531,#82532),.UNSPECIFIED.,.F.,.F.)
B_SPLINE_CURVE_WITH_KNOTS((3,3),(0.0270544913418446,0.0439828187741916),
 .UNSPECIFIED.)
CURVE()
GEOMETRIC_REPRESENTATION_ITEM()
RATIONAL_B_SPLINE_CURVE((1.00082963690992,1.00067437545575,1.))
REPRESENTATION_ITEM('')
);
#492=(
BOUNDED_CURVE()
B_SPLINE_CURVE(2,(#82536,#82537,#82538),.UNSPECIFIED.,.F.,.F.)
B_SPLINE_CURVE_WITH_KNOTS((3,3),(0.,0.0169283274324851),.UNSPECIFIED.)
CURVE()
GEOMETRIC_REPRESENTATION_ITEM()
RATIONAL_B_SPLINE_CURVE((1.,1.00067437545061,1.00082963690359))
REPRESENTATION_ITEM('')
);
#493=(
BOUNDED_CURVE()
B_SPLINE_CURVE(2,(#82540,#82541,#82542),.UNSPECIFIED.,.F.,.F.)
B_SPLINE_CURVE_WITH_KNOTS((3,3),(0.0270544913417195,0.0439828187741921),
 .UNSPECIFIED.)
CURVE()
GEOMETRIC_REPRESENTATION_ITEM()
RATIONAL_B_SPLINE_CURVE((1.00082963689352,1.00067437544242,1.))
REPRESENTATION_ITEM('')
);
#494=(
BOUNDED_CURVE()
B_SPLINE_CURVE(2,(#82546,#82547,#82548),.UNSPECIFIED.,.F.,.F.)
B_SPLINE_CURVE_WITH_KNOTS((3,3),(0.,0.0169283274324387),.UNSPECIFIED.)
CURVE()
GEOMETRIC_REPRESENTATION_ITEM()
RATIONAL_B_SPLINE_CURVE((1.,1.00067437545353,1.00082963690719))
REPRESENTATION_ITEM('')
);
#495=(
BOUNDED_CURVE()
B_SPLINE_CURVE(2,(#82550,#82551,#82552),.UNSPECIFIED.,.F.,.F.)
B_SPLINE_CURVE_WITH_KNOTS((3,3),(0.0270544913416745,0.0439828187741916),
 .UNSPECIFIED.)
CURVE()
GEOMETRIC_REPRESENTATION_ITEM()
RATIONAL_B_SPLINE_CURVE((1.00082963688426,1.00067437543489,1.))
REPRESENTATION_ITEM('')
);
#496=(
BOUNDED_CURVE()
B_SPLINE_CURVE(2,(#82555,#82556,#82557),.UNSPECIFIED.,.F.,.F.)
B_SPLINE_CURVE_WITH_KNOTS((3,3),(0.,0.0169283274326045),.UNSPECIFIED.)
CURVE()
GEOMETRIC_REPRESENTATION_ITEM()
RATIONAL_B_SPLINE_CURVE((1.,1.0006743754289,1.00082963687688))
REPRESENTATION_ITEM('')
);
#497=(
BOUNDED_CURVE()
B_SPLINE_CURVE(2,(#83095,#83096,#83097),.UNSPECIFIED.,.F.,.F.)
B_SPLINE_CURVE_WITH_KNOTS((3,3),(0.0765277474505289,0.571444001127736),
 .UNSPECIFIED.)
CURVE()
GEOMETRIC_REPRESENTATION_ITEM()
RATIONAL_B_SPLINE_CURVE((1.05846949482053,1.2222152955272,1.05846949482053))
REPRESENTATION_ITEM('')
);
#498=(
BOUNDED_CURVE()
B_SPLINE_CURVE(2,(#83099,#83100,#83101),.UNSPECIFIED.,.F.,.F.)
B_SPLINE_CURVE_WITH_KNOTS((3,3),(0.0765277474505272,0.571444001127737),
 .UNSPECIFIED.)
CURVE()
GEOMETRIC_REPRESENTATION_ITEM()
RATIONAL_B_SPLINE_CURVE((1.05846949482054,1.22221529552722,1.05846949482054))
REPRESENTATION_ITEM('')
);
#499=(
BOUNDED_CURVE()
B_SPLINE_CURVE(2,(#83103,#83104,#83105),.UNSPECIFIED.,.F.,.F.)
B_SPLINE_CURVE_WITH_KNOTS((3,3),(0.0765277474505292,0.571444001127744),
 .UNSPECIFIED.)
CURVE()
GEOMETRIC_REPRESENTATION_ITEM()
RATIONAL_B_SPLINE_CURVE((1.05846949482055,1.22221529552726,1.05846949482055))
REPRESENTATION_ITEM('')
);
#500=(
BOUNDED_CURVE()
B_SPLINE_CURVE(2,(#83107,#83108,#83109),.UNSPECIFIED.,.F.,.F.)
B_SPLINE_CURVE_WITH_KNOTS((3,3),(0.0765277474505268,0.571444001127737),
 .UNSPECIFIED.)
CURVE()
GEOMETRIC_REPRESENTATION_ITEM()
RATIONAL_B_SPLINE_CURVE((1.05846949482054,1.22221529552723,1.05846949482054))
REPRESENTATION_ITEM('')
);
#501=(
BOUNDED_CURVE()
B_SPLINE_CURVE(2,(#83111,#83112,#83113),.UNSPECIFIED.,.F.,.F.)
B_SPLINE_CURVE_WITH_KNOTS((3,3),(0.0765277474505273,0.571444001127738),
 .UNSPECIFIED.)
CURVE()
GEOMETRIC_REPRESENTATION_ITEM()
RATIONAL_B_SPLINE_CURVE((1.05846949482054,1.22221529552722,1.05846949482054))
REPRESENTATION_ITEM('')
);
#502=(
BOUNDED_CURVE()
B_SPLINE_CURVE(2,(#83114,#83115,#83116),.UNSPECIFIED.,.F.,.F.)
B_SPLINE_CURVE_WITH_KNOTS((3,3),(0.0765277474505272,0.571444001127742),
 .UNSPECIFIED.)
CURVE()
GEOMETRIC_REPRESENTATION_ITEM()
RATIONAL_B_SPLINE_CURVE((1.05846949482054,1.22221529552725,1.05846949482054))
REPRESENTATION_ITEM('')
);
#503=TOROIDAL_SURFACE('',#27630,1.5635,0.1);
#504=TOROIDAL_SURFACE('',#27822,2.55,0.2);
#505=TOROIDAL_SURFACE('',#28481,1.85434,0.15);
#506=TOROIDAL_SURFACE('',#28715,1.85434,0.15);
#507=TOROIDAL_SURFACE('',#28959,1.85434,0.15);
#508=B_SPLINE_CURVE_WITH_KNOTS('',5,(#37220,#37221,#37222,#37223,#37224,
#37225,#37226,#37227,#37228,#37229,#37230,#37231,#37232,#37233,#37234,#37235,
#37236,#37237,#37238,#37239,#37240,#37241,#37242,#37243,#37244,#37245,#37246,
#37247,#37248,#37249,#37250,#37251,#37252,#37253,#37254),.UNSPECIFIED.,
 .F.,.F.,(6,1,1,1,1,1,1,1,1,1,1,1,1,1,1,1,1,1,1,1,1,1,1,1,1,1,1,1,1,1,6),
(0.,0.0333333333333333,0.0666666666666667,0.1,0.133333333333333,0.166666666666667,
0.2,0.233333333333333,0.266666666666667,0.3,0.333333333333333,0.366666666666667,
0.4,0.433333333333333,0.466666666666667,0.5,0.533333333333333,0.566666666666667,
0.6,0.633333333333333,0.666666666666667,0.7,0.733333333333333,0.766666666666667,
0.8,0.833333333333333,0.866666666666667,0.9,0.933333333333333,0.966666666666667,
1.),.UNSPECIFIED.);
#509=B_SPLINE_CURVE_WITH_KNOTS('',5,(#37256,#37257,#37258,#37259,#37260,
#37261,#37262,#37263,#37264,#37265,#37266,#37267,#37268,#37269,#37270,#37271,
#37272,#37273,#37274,#37275,#37276,#37277,#37278,#37279,#37280,#37281,#37282,
#37283,#37284,#37285,#37286,#37287,#37288,#37289,#37290),.UNSPECIFIED.,
 .F.,.F.,(6,1,1,1,1,1,1,1,1,1,1,1,1,1,1,1,1,1,1,1,1,1,1,1,1,1,1,1,1,1,6),
(0.,0.0333333333333333,0.0666666666666667,0.1,0.133333333333333,0.166666666666667,
0.2,0.233333333333333,0.266666666666667,0.3,0.333333333333333,0.366666666666667,
0.4,0.433333333333333,0.466666666666667,0.5,0.533333333333333,0.566666666666667,
0.6,0.633333333333333,0.666666666666667,0.7,0.733333333333333,0.766666666666667,
0.8,0.833333333333333,0.866666666666667,0.9,0.933333333333333,0.966666666666667,
1.),.UNSPECIFIED.);
#510=B_SPLINE_CURVE_WITH_KNOTS('',5,(#37368,#37369,#37370,#37371,#37372,
#37373,#37374,#37375,#37376,#37377,#37378,#37379,#37380,#37381,#37382,#37383,
#37384,#37385,#37386,#37387,#37388,#37389,#37390,#37391,#37392,#37393,#37394,
#37395,#37396,#37397,#37398,#37399,#37400,#37401,#37402),.UNSPECIFIED.,
 .F.,.F.,(6,1,1,1,1,1,1,1,1,1,1,1,1,1,1,1,1,1,1,1,1,1,1,1,1,1,1,1,1,1,6),
(0.,0.0333333333333333,0.0666666666666667,0.1,0.133333333333333,0.166666666666667,
0.2,0.233333333333333,0.266666666666667,0.3,0.333333333333333,0.366666666666667,
0.4,0.433333333333333,0.466666666666667,0.5,0.533333333333333,0.566666666666667,
0.6,0.633333333333333,0.666666666666667,0.7,0.733333333333333,0.766666666666667,
0.8,0.833333333333333,0.866666666666667,0.9,0.933333333333333,0.966666666666667,
1.),.UNSPECIFIED.);
#511=B_SPLINE_CURVE_WITH_KNOTS('',5,(#37403,#37404,#37405,#37406,#37407,
#37408,#37409,#37410,#37411,#37412,#37413,#37414,#37415,#37416,#37417,#37418,
#37419,#37420,#37421,#37422,#37423,#37424,#37425,#37426,#37427,#37428,#37429,
#37430,#37431,#37432,#37433,#37434,#37435,#37436,#37437),.UNSPECIFIED.,
 .F.,.F.,(6,1,1,1,1,1,1,1,1,1,1,1,1,1,1,1,1,1,1,1,1,1,1,1,1,1,1,1,1,1,6),
(-1.,-0.966666666666667,-0.933333333333333,-0.9,-0.866666666666667,-0.833333333333333,
-0.8,-0.766666666666667,-0.733333333333333,-0.7,-0.666666666666667,-0.633333333333333,
-0.6,-0.566666666666667,-0.533333333333333,-0.5,-0.466666666666667,-0.433333333333333,
-0.4,-0.366666666666667,-0.333333333333333,-0.3,-0.266666666666667,-0.233333333333333,
-0.2,-0.166666666666667,-0.133333333333333,-0.1,-0.0666666666666667,-0.0333333333333333,
0.),.UNSPECIFIED.);
#512=B_SPLINE_CURVE_WITH_KNOTS('',5,(#37444,#37445,#37446,#37447,#37448,
#37449,#37450,#37451,#37452,#37453,#37454,#37455,#37456,#37457,#37458,#37459,
#37460,#37461,#37462,#37463,#37464,#37465,#37466,#37467,#37468,#37469,#37470,
#37471,#37472,#37473,#37474,#37475,#37476,#37477,#37478),.UNSPECIFIED.,
 .F.,.F.,(6,1,1,1,1,1,1,1,1,1,1,1,1,1,1,1,1,1,1,1,1,1,1,1,1,1,1,1,1,1,6),
(0.,0.0333333333333333,0.0666666666666667,0.1,0.133333333333333,0.166666666666667,
0.2,0.233333333333333,0.266666666666667,0.3,0.333333333333333,0.366666666666667,
0.4,0.433333333333333,0.466666666666667,0.5,0.533333333333333,0.566666666666667,
0.6,0.633333333333333,0.666666666666667,0.7,0.733333333333333,0.766666666666667,
0.8,0.833333333333333,0.866666666666667,0.9,0.933333333333333,0.966666666666667,
1.),.UNSPECIFIED.);
#513=B_SPLINE_CURVE_WITH_KNOTS('',5,(#37482,#37483,#37484,#37485,#37486,
#37487,#37488,#37489,#37490,#37491,#37492,#37493,#37494,#37495,#37496,#37497,
#37498,#37499,#37500,#37501,#37502,#37503,#37504,#37505,#37506,#37507,#37508,
#37509,#37510,#37511,#37512,#37513,#37514,#37515,#37516),.UNSPECIFIED.,
 .F.,.F.,(6,1,1,1,1,1,1,1,1,1,1,1,1,1,1,1,1,1,1,1,1,1,1,1,1,1,1,1,1,1,6),
(0.,0.0333333333333333,0.0666666666666667,0.1,0.133333333333333,0.166666666666667,
0.2,0.233333333333333,0.266666666666667,0.3,0.333333333333333,0.366666666666667,
0.4,0.433333333333333,0.466666666666667,0.5,0.533333333333333,0.566666666666667,
0.6,0.633333333333333,0.666666666666667,0.7,0.733333333333333,0.766666666666667,
0.8,0.833333333333333,0.866666666666667,0.9,0.933333333333333,0.966666666666667,
1.),.UNSPECIFIED.);
#514=B_SPLINE_CURVE_WITH_KNOTS('',5,(#37524,#37525,#37526,#37527,#37528,
#37529,#37530,#37531,#37532,#37533,#37534,#37535,#37536,#37537,#37538,#37539,
#37540,#37541,#37542,#37543,#37544,#37545,#37546,#37547,#37548,#37549,#37550,
#37551,#37552,#37553,#37554,#37555,#37556,#37557,#37558),.UNSPECIFIED.,
 .F.,.F.,(6,1,1,1,1,1,1,1,1,1,1,1,1,1,1,1,1,1,1,1,1,1,1,1,1,1,1,1,1,1,6),
(0.,0.0333333333333333,0.0666666666666667,0.1,0.133333333333333,0.166666666666667,
0.2,0.233333333333333,0.266666666666667,0.3,0.333333333333333,0.366666666666667,
0.4,0.433333333333333,0.466666666666667,0.5,0.533333333333333,0.566666666666667,
0.6,0.633333333333333,0.666666666666667,0.7,0.733333333333333,0.766666666666667,
0.8,0.833333333333333,0.866666666666667,0.9,0.933333333333333,0.966666666666667,
1.),.UNSPECIFIED.);
#515=B_SPLINE_CURVE_WITH_KNOTS('',5,(#37562,#37563,#37564,#37565,#37566,
#37567,#37568,#37569,#37570,#37571,#37572,#37573,#37574,#37575,#37576,#37577,
#37578,#37579,#37580,#37581,#37582,#37583,#37584,#37585,#37586,#37587,#37588,
#37589,#37590,#37591,#37592,#37593,#37594,#37595,#37596),.UNSPECIFIED.,
 .F.,.F.,(6,1,1,1,1,1,1,1,1,1,1,1,1,1,1,1,1,1,1,1,1,1,1,1,1,1,1,1,1,1,6),
(0.,0.0333333333333333,0.0666666666666667,0.1,0.133333333333333,0.166666666666667,
0.2,0.233333333333333,0.266666666666667,0.3,0.333333333333333,0.366666666666667,
0.4,0.433333333333333,0.466666666666667,0.5,0.533333333333333,0.566666666666667,
0.6,0.633333333333333,0.666666666666667,0.7,0.733333333333333,0.766666666666667,
0.8,0.833333333333333,0.866666666666667,0.9,0.933333333333333,0.966666666666667,
1.),.UNSPECIFIED.);
#516=B_SPLINE_CURVE_WITH_KNOTS('',5,(#37604,#37605,#37606,#37607,#37608,
#37609,#37610,#37611,#37612,#37613,#37614,#37615,#37616,#37617,#37618,#37619,
#37620,#37621,#37622,#37623,#37624,#37625,#37626,#37627,#37628,#37629,#37630,
#37631,#37632,#37633,#37634,#37635,#37636,#37637,#37638),.UNSPECIFIED.,
 .F.,.F.,(6,1,1,1,1,1,1,1,1,1,1,1,1,1,1,1,1,1,1,1,1,1,1,1,1,1,1,1,1,1,6),
(0.,0.0333333333333333,0.0666666666666667,0.1,0.133333333333333,0.166666666666667,
0.2,0.233333333333333,0.266666666666667,0.3,0.333333333333333,0.366666666666667,
0.4,0.433333333333333,0.466666666666667,0.5,0.533333333333333,0.566666666666667,
0.6,0.633333333333333,0.666666666666667,0.7,0.733333333333333,0.766666666666667,
0.8,0.833333333333333,0.866666666666667,0.9,0.933333333333333,0.966666666666667,
1.),.UNSPECIFIED.);
#517=B_SPLINE_CURVE_WITH_KNOTS('',5,(#37642,#37643,#37644,#37645,#37646,
#37647,#37648,#37649,#37650,#37651,#37652,#37653,#37654,#37655,#37656,#37657,
#37658,#37659,#37660,#37661,#37662,#37663,#37664,#37665,#37666,#37667,#37668,
#37669,#37670,#37671,#37672,#37673,#37674,#37675,#37676),.UNSPECIFIED.,
 .F.,.F.,(6,1,1,1,1,1,1,1,1,1,1,1,1,1,1,1,1,1,1,1,1,1,1,1,1,1,1,1,1,1,6),
(0.,0.0333333333333333,0.0666666666666667,0.1,0.133333333333333,0.166666666666667,
0.2,0.233333333333333,0.266666666666667,0.3,0.333333333333333,0.366666666666667,
0.4,0.433333333333333,0.466666666666667,0.5,0.533333333333333,0.566666666666667,
0.6,0.633333333333333,0.666666666666667,0.7,0.733333333333333,0.766666666666667,
0.8,0.833333333333333,0.866666666666667,0.9,0.933333333333333,0.966666666666667,
1.),.UNSPECIFIED.);
#518=B_SPLINE_CURVE_WITH_KNOTS('',5,(#37684,#37685,#37686,#37687,#37688,
#37689,#37690,#37691,#37692,#37693,#37694,#37695,#37696,#37697,#37698,#37699,
#37700,#37701,#37702,#37703,#37704,#37705,#37706,#37707,#37708,#37709,#37710,
#37711,#37712,#37713,#37714,#37715,#37716,#37717,#37718),.UNSPECIFIED.,
 .F.,.F.,(6,1,1,1,1,1,1,1,1,1,1,1,1,1,1,1,1,1,1,1,1,1,1,1,1,1,1,1,1,1,6),
(0.,0.0333333333333333,0.0666666666666667,0.1,0.133333333333333,0.166666666666667,
0.2,0.233333333333333,0.266666666666667,0.3,0.333333333333333,0.366666666666667,
0.4,0.433333333333333,0.466666666666667,0.5,0.533333333333333,0.566666666666667,
0.6,0.633333333333333,0.666666666666667,0.7,0.733333333333333,0.766666666666667,
0.8,0.833333333333333,0.866666666666667,0.9,0.933333333333333,0.966666666666667,
1.),.UNSPECIFIED.);
#519=B_SPLINE_CURVE_WITH_KNOTS('',5,(#37722,#37723,#37724,#37725,#37726,
#37727,#37728,#37729,#37730,#37731,#37732,#37733,#37734,#37735,#37736,#37737,
#37738,#37739,#37740,#37741,#37742,#37743,#37744,#37745,#37746,#37747,#37748,
#37749,#37750,#37751,#37752,#37753,#37754,#37755,#37756),.UNSPECIFIED.,
 .F.,.F.,(6,1,1,1,1,1,1,1,1,1,1,1,1,1,1,1,1,1,1,1,1,1,1,1,1,1,1,1,1,1,6),
(0.,0.0333333333333333,0.0666666666666667,0.1,0.133333333333333,0.166666666666667,
0.2,0.233333333333333,0.266666666666667,0.3,0.333333333333333,0.366666666666667,
0.4,0.433333333333333,0.466666666666667,0.5,0.533333333333333,0.566666666666667,
0.6,0.633333333333333,0.666666666666667,0.7,0.733333333333333,0.766666666666667,
0.8,0.833333333333333,0.866666666666667,0.9,0.933333333333333,0.966666666666667,
1.),.UNSPECIFIED.);
#520=B_SPLINE_CURVE_WITH_KNOTS('',5,(#37764,#37765,#37766,#37767,#37768,
#37769,#37770,#37771,#37772,#37773,#37774,#37775,#37776,#37777,#37778,#37779,
#37780,#37781,#37782,#37783,#37784,#37785,#37786,#37787,#37788,#37789,#37790,
#37791,#37792,#37793,#37794,#37795,#37796,#37797,#37798),.UNSPECIFIED.,
 .F.,.F.,(6,1,1,1,1,1,1,1,1,1,1,1,1,1,1,1,1,1,1,1,1,1,1,1,1,1,1,1,1,1,6),
(0.,0.0333333333333333,0.0666666666666667,0.1,0.133333333333333,0.166666666666667,
0.2,0.233333333333333,0.266666666666667,0.3,0.333333333333333,0.366666666666667,
0.4,0.433333333333333,0.466666666666667,0.5,0.533333333333333,0.566666666666667,
0.6,0.633333333333333,0.666666666666667,0.7,0.733333333333333,0.766666666666667,
0.8,0.833333333333333,0.866666666666667,0.9,0.933333333333333,0.966666666666667,
1.),.UNSPECIFIED.);
#521=B_SPLINE_CURVE_WITH_KNOTS('',5,(#37802,#37803,#37804,#37805,#37806,
#37807,#37808,#37809,#37810,#37811,#37812,#37813,#37814,#37815,#37816,#37817,
#37818,#37819,#37820,#37821,#37822,#37823,#37824,#37825,#37826,#37827,#37828,
#37829,#37830,#37831,#37832,#37833,#37834,#37835,#37836),.UNSPECIFIED.,
 .F.,.F.,(6,1,1,1,1,1,1,1,1,1,1,1,1,1,1,1,1,1,1,1,1,1,1,1,1,1,1,1,1,1,6),
(0.,0.0333333333333333,0.0666666666666667,0.1,0.133333333333333,0.166666666666667,
0.2,0.233333333333333,0.266666666666667,0.3,0.333333333333333,0.366666666666667,
0.4,0.433333333333333,0.466666666666667,0.5,0.533333333333333,0.566666666666667,
0.6,0.633333333333333,0.666666666666667,0.7,0.733333333333333,0.766666666666667,
0.8,0.833333333333333,0.866666666666667,0.9,0.933333333333333,0.966666666666667,
1.),.UNSPECIFIED.);
#522=B_SPLINE_CURVE_WITH_KNOTS('',5,(#37844,#37845,#37846,#37847,#37848,
#37849,#37850,#37851,#37852,#37853,#37854,#37855,#37856,#37857,#37858,#37859,
#37860,#37861,#37862,#37863,#37864,#37865,#37866,#37867,#37868,#37869,#37870,
#37871,#37872,#37873,#37874,#37875,#37876,#37877,#37878),.UNSPECIFIED.,
 .F.,.F.,(6,1,1,1,1,1,1,1,1,1,1,1,1,1,1,1,1,1,1,1,1,1,1,1,1,1,1,1,1,1,6),
(0.,0.0333333333333333,0.0666666666666667,0.1,0.133333333333333,0.166666666666667,
0.2,0.233333333333333,0.266666666666667,0.3,0.333333333333333,0.366666666666667,
0.4,0.433333333333333,0.466666666666667,0.5,0.533333333333333,0.566666666666667,
0.6,0.633333333333333,0.666666666666667,0.7,0.733333333333333,0.766666666666667,
0.8,0.833333333333333,0.866666666666667,0.9,0.933333333333333,0.966666666666667,
1.),.UNSPECIFIED.);
#523=B_SPLINE_CURVE_WITH_KNOTS('',5,(#37882,#37883,#37884,#37885,#37886,
#37887,#37888,#37889,#37890,#37891,#37892,#37893,#37894,#37895,#37896,#37897,
#37898,#37899,#37900,#37901,#37902,#37903,#37904,#37905,#37906,#37907,#37908,
#37909,#37910,#37911,#37912,#37913,#37914,#37915,#37916),.UNSPECIFIED.,
 .F.,.F.,(6,1,1,1,1,1,1,1,1,1,1,1,1,1,1,1,1,1,1,1,1,1,1,1,1,1,1,1,1,1,6),
(0.,0.0333333333333333,0.0666666666666667,0.1,0.133333333333333,0.166666666666667,
0.2,0.233333333333333,0.266666666666667,0.3,0.333333333333333,0.366666666666667,
0.4,0.433333333333333,0.466666666666667,0.5,0.533333333333333,0.566666666666667,
0.6,0.633333333333333,0.666666666666667,0.7,0.733333333333333,0.766666666666667,
0.8,0.833333333333333,0.866666666666667,0.9,0.933333333333333,0.966666666666667,
1.),.UNSPECIFIED.);
#524=B_SPLINE_CURVE_WITH_KNOTS('',5,(#37924,#37925,#37926,#37927,#37928,
#37929,#37930,#37931,#37932,#37933,#37934,#37935,#37936,#37937,#37938,#37939,
#37940,#37941,#37942,#37943,#37944,#37945,#37946,#37947,#37948,#37949,#37950,
#37951,#37952,#37953,#37954,#37955,#37956,#37957,#37958),.UNSPECIFIED.,
 .F.,.F.,(6,1,1,1,1,1,1,1,1,1,1,1,1,1,1,1,1,1,1,1,1,1,1,1,1,1,1,1,1,1,6),
(0.,0.0333333333333333,0.0666666666666667,0.1,0.133333333333333,0.166666666666667,
0.2,0.233333333333333,0.266666666666667,0.3,0.333333333333333,0.366666666666667,
0.4,0.433333333333333,0.466666666666667,0.5,0.533333333333333,0.566666666666667,
0.6,0.633333333333333,0.666666666666667,0.7,0.733333333333333,0.766666666666667,
0.8,0.833333333333333,0.866666666666667,0.9,0.933333333333333,0.966666666666667,
1.),.UNSPECIFIED.);
#525=B_SPLINE_CURVE_WITH_KNOTS('',5,(#37962,#37963,#37964,#37965,#37966,
#37967,#37968,#37969,#37970,#37971,#37972,#37973,#37974,#37975,#37976,#37977,
#37978,#37979,#37980,#37981,#37982,#37983,#37984,#37985,#37986,#37987,#37988,
#37989,#37990,#37991,#37992,#37993,#37994,#37995,#37996),.UNSPECIFIED.,
 .F.,.F.,(6,1,1,1,1,1,1,1,1,1,1,1,1,1,1,1,1,1,1,1,1,1,1,1,1,1,1,1,1,1,6),
(0.,0.0333333333333333,0.0666666666666667,0.1,0.133333333333333,0.166666666666667,
0.2,0.233333333333333,0.266666666666667,0.3,0.333333333333333,0.366666666666667,
0.4,0.433333333333333,0.466666666666667,0.5,0.533333333333333,0.566666666666667,
0.6,0.633333333333333,0.666666666666667,0.7,0.733333333333333,0.766666666666667,
0.8,0.833333333333333,0.866666666666667,0.9,0.933333333333333,0.966666666666667,
1.),.UNSPECIFIED.);
#526=B_SPLINE_CURVE_WITH_KNOTS('',5,(#38004,#38005,#38006,#38007,#38008,
#38009,#38010,#38011,#38012,#38013,#38014,#38015,#38016,#38017,#38018,#38019,
#38020,#38021,#38022,#38023,#38024,#38025,#38026,#38027,#38028,#38029,#38030,
#38031,#38032,#38033,#38034,#38035,#38036,#38037,#38038),.UNSPECIFIED.,
 .F.,.F.,(6,1,1,1,1,1,1,1,1,1,1,1,1,1,1,1,1,1,1,1,1,1,1,1,1,1,1,1,1,1,6),
(0.,0.0333333333333333,0.0666666666666667,0.1,0.133333333333333,0.166666666666667,
0.2,0.233333333333333,0.266666666666667,0.3,0.333333333333333,0.366666666666667,
0.4,0.433333333333333,0.466666666666667,0.5,0.533333333333333,0.566666666666667,
0.6,0.633333333333333,0.666666666666667,0.7,0.733333333333333,0.766666666666667,
0.8,0.833333333333333,0.866666666666667,0.9,0.933333333333333,0.966666666666667,
1.),.UNSPECIFIED.);
#527=B_SPLINE_CURVE_WITH_KNOTS('',5,(#38042,#38043,#38044,#38045,#38046,
#38047,#38048,#38049,#38050,#38051,#38052,#38053,#38054,#38055,#38056,#38057,
#38058,#38059,#38060,#38061,#38062,#38063,#38064,#38065,#38066,#38067,#38068,
#38069,#38070,#38071,#38072,#38073,#38074,#38075,#38076),.UNSPECIFIED.,
 .F.,.F.,(6,1,1,1,1,1,1,1,1,1,1,1,1,1,1,1,1,1,1,1,1,1,1,1,1,1,1,1,1,1,6),
(0.,0.0333333333333333,0.0666666666666667,0.1,0.133333333333333,0.166666666666667,
0.2,0.233333333333333,0.266666666666667,0.3,0.333333333333333,0.366666666666667,
0.4,0.433333333333333,0.466666666666667,0.5,0.533333333333333,0.566666666666667,
0.6,0.633333333333333,0.666666666666667,0.7,0.733333333333333,0.766666666666667,
0.8,0.833333333333333,0.866666666666667,0.9,0.933333333333333,0.966666666666667,
1.),.UNSPECIFIED.);
#528=B_SPLINE_CURVE_WITH_KNOTS('',5,(#38084,#38085,#38086,#38087,#38088,
#38089,#38090,#38091,#38092,#38093,#38094,#38095,#38096,#38097,#38098,#38099,
#38100,#38101,#38102,#38103,#38104,#38105,#38106,#38107,#38108,#38109,#38110,
#38111,#38112,#38113,#38114,#38115,#38116,#38117,#38118),.UNSPECIFIED.,
 .F.,.F.,(6,1,1,1,1,1,1,1,1,1,1,1,1,1,1,1,1,1,1,1,1,1,1,1,1,1,1,1,1,1,6),
(0.,0.0333333333333333,0.0666666666666667,0.1,0.133333333333333,0.166666666666667,
0.2,0.233333333333333,0.266666666666667,0.3,0.333333333333333,0.366666666666667,
0.4,0.433333333333333,0.466666666666667,0.5,0.533333333333333,0.566666666666667,
0.6,0.633333333333333,0.666666666666667,0.7,0.733333333333333,0.766666666666667,
0.8,0.833333333333333,0.866666666666667,0.9,0.933333333333333,0.966666666666667,
1.),.UNSPECIFIED.);
#529=B_SPLINE_CURVE_WITH_KNOTS('',5,(#38122,#38123,#38124,#38125,#38126,
#38127,#38128,#38129,#38130,#38131,#38132,#38133,#38134,#38135,#38136,#38137,
#38138,#38139,#38140,#38141,#38142,#38143,#38144,#38145,#38146,#38147,#38148,
#38149,#38150,#38151,#38152,#38153,#38154,#38155,#38156),.UNSPECIFIED.,
 .F.,.F.,(6,1,1,1,1,1,1,1,1,1,1,1,1,1,1,1,1,1,1,1,1,1,1,1,1,1,1,1,1,1,6),
(0.,0.0333333333333333,0.0666666666666667,0.1,0.133333333333333,0.166666666666667,
0.2,0.233333333333333,0.266666666666667,0.3,0.333333333333333,0.366666666666667,
0.4,0.433333333333333,0.466666666666667,0.5,0.533333333333333,0.566666666666667,
0.6,0.633333333333333,0.666666666666667,0.7,0.733333333333333,0.766666666666667,
0.8,0.833333333333333,0.866666666666667,0.9,0.933333333333333,0.966666666666667,
1.),.UNSPECIFIED.);
#530=B_SPLINE_CURVE_WITH_KNOTS('',5,(#38164,#38165,#38166,#38167,#38168,
#38169,#38170,#38171,#38172,#38173,#38174,#38175,#38176,#38177,#38178,#38179,
#38180,#38181,#38182,#38183,#38184,#38185,#38186,#38187,#38188,#38189,#38190,
#38191,#38192,#38193,#38194,#38195,#38196,#38197,#38198),.UNSPECIFIED.,
 .F.,.F.,(6,1,1,1,1,1,1,1,1,1,1,1,1,1,1,1,1,1,1,1,1,1,1,1,1,1,1,1,1,1,6),
(0.,0.0333333333333333,0.0666666666666667,0.1,0.133333333333333,0.166666666666667,
0.2,0.233333333333333,0.266666666666667,0.3,0.333333333333333,0.366666666666667,
0.4,0.433333333333333,0.466666666666667,0.5,0.533333333333333,0.566666666666667,
0.6,0.633333333333333,0.666666666666667,0.7,0.733333333333333,0.766666666666667,
0.8,0.833333333333333,0.866666666666667,0.9,0.933333333333333,0.966666666666667,
1.),.UNSPECIFIED.);
#531=B_SPLINE_CURVE_WITH_KNOTS('',5,(#38202,#38203,#38204,#38205,#38206,
#38207,#38208,#38209,#38210,#38211,#38212,#38213,#38214,#38215,#38216,#38217,
#38218,#38219,#38220,#38221,#38222,#38223,#38224,#38225,#38226,#38227,#38228,
#38229,#38230,#38231,#38232,#38233,#38234,#38235,#38236),.UNSPECIFIED.,
 .F.,.F.,(6,1,1,1,1,1,1,1,1,1,1,1,1,1,1,1,1,1,1,1,1,1,1,1,1,1,1,1,1,1,6),
(0.,0.0333333333333333,0.0666666666666667,0.1,0.133333333333333,0.166666666666667,
0.2,0.233333333333333,0.266666666666667,0.3,0.333333333333333,0.366666666666667,
0.4,0.433333333333333,0.466666666666667,0.5,0.533333333333333,0.566666666666667,
0.6,0.633333333333333,0.666666666666667,0.7,0.733333333333333,0.766666666666667,
0.8,0.833333333333333,0.866666666666667,0.9,0.933333333333333,0.966666666666667,
1.),.UNSPECIFIED.);
#532=B_SPLINE_CURVE_WITH_KNOTS('',5,(#38244,#38245,#38246,#38247,#38248,
#38249,#38250,#38251,#38252,#38253,#38254,#38255,#38256,#38257,#38258,#38259,
#38260,#38261,#38262,#38263,#38264,#38265,#38266,#38267,#38268,#38269,#38270,
#38271,#38272,#38273,#38274,#38275,#38276,#38277,#38278),.UNSPECIFIED.,
 .F.,.F.,(6,1,1,1,1,1,1,1,1,1,1,1,1,1,1,1,1,1,1,1,1,1,1,1,1,1,1,1,1,1,6),
(0.,0.0333333333333333,0.0666666666666667,0.1,0.133333333333333,0.166666666666667,
0.2,0.233333333333333,0.266666666666667,0.3,0.333333333333333,0.366666666666667,
0.4,0.433333333333333,0.466666666666667,0.5,0.533333333333333,0.566666666666667,
0.6,0.633333333333333,0.666666666666667,0.7,0.733333333333333,0.766666666666667,
0.8,0.833333333333333,0.866666666666667,0.9,0.933333333333333,0.966666666666667,
1.),.UNSPECIFIED.);
#533=B_SPLINE_CURVE_WITH_KNOTS('',5,(#38282,#38283,#38284,#38285,#38286,
#38287,#38288,#38289,#38290,#38291,#38292,#38293,#38294,#38295,#38296,#38297,
#38298,#38299,#38300,#38301,#38302,#38303,#38304,#38305,#38306,#38307,#38308,
#38309,#38310,#38311,#38312,#38313,#38314,#38315,#38316),.UNSPECIFIED.,
 .F.,.F.,(6,1,1,1,1,1,1,1,1,1,1,1,1,1,1,1,1,1,1,1,1,1,1,1,1,1,1,1,1,1,6),
(0.,0.0333333333333333,0.0666666666666667,0.1,0.133333333333333,0.166666666666667,
0.2,0.233333333333333,0.266666666666667,0.3,0.333333333333333,0.366666666666667,
0.4,0.433333333333333,0.466666666666667,0.5,0.533333333333333,0.566666666666667,
0.6,0.633333333333333,0.666666666666667,0.7,0.733333333333333,0.766666666666667,
0.8,0.833333333333333,0.866666666666667,0.9,0.933333333333333,0.966666666666667,
1.),.UNSPECIFIED.);
#534=B_SPLINE_CURVE_WITH_KNOTS('',5,(#38324,#38325,#38326,#38327,#38328,
#38329,#38330,#38331,#38332,#38333,#38334,#38335,#38336,#38337,#38338,#38339,
#38340,#38341,#38342,#38343,#38344,#38345,#38346,#38347,#38348,#38349,#38350,
#38351,#38352,#38353,#38354,#38355,#38356,#38357,#38358),.UNSPECIFIED.,
 .F.,.F.,(6,1,1,1,1,1,1,1,1,1,1,1,1,1,1,1,1,1,1,1,1,1,1,1,1,1,1,1,1,1,6),
(0.,0.0333333333333333,0.0666666666666667,0.1,0.133333333333333,0.166666666666667,
0.2,0.233333333333333,0.266666666666667,0.3,0.333333333333333,0.366666666666667,
0.4,0.433333333333333,0.466666666666667,0.5,0.533333333333333,0.566666666666667,
0.6,0.633333333333333,0.666666666666667,0.7,0.733333333333333,0.766666666666667,
0.8,0.833333333333333,0.866666666666667,0.9,0.933333333333333,0.966666666666667,
1.),.UNSPECIFIED.);
#535=B_SPLINE_CURVE_WITH_KNOTS('',5,(#38362,#38363,#38364,#38365,#38366,
#38367,#38368,#38369,#38370,#38371,#38372,#38373,#38374,#38375,#38376,#38377,
#38378,#38379,#38380,#38381,#38382,#38383,#38384,#38385,#38386,#38387,#38388,
#38389,#38390,#38391,#38392,#38393,#38394,#38395,#38396),.UNSPECIFIED.,
 .F.,.F.,(6,1,1,1,1,1,1,1,1,1,1,1,1,1,1,1,1,1,1,1,1,1,1,1,1,1,1,1,1,1,6),
(0.,0.0333333333333333,0.0666666666666667,0.1,0.133333333333333,0.166666666666667,
0.2,0.233333333333333,0.266666666666667,0.3,0.333333333333333,0.366666666666667,
0.4,0.433333333333333,0.466666666666667,0.5,0.533333333333333,0.566666666666667,
0.6,0.633333333333333,0.666666666666667,0.7,0.733333333333333,0.766666666666667,
0.8,0.833333333333333,0.866666666666667,0.9,0.933333333333333,0.966666666666667,
1.),.UNSPECIFIED.);
#536=B_SPLINE_CURVE_WITH_KNOTS('',5,(#38404,#38405,#38406,#38407,#38408,
#38409,#38410,#38411,#38412,#38413,#38414,#38415,#38416,#38417,#38418,#38419,
#38420,#38421,#38422,#38423,#38424,#38425,#38426,#38427,#38428,#38429,#38430,
#38431,#38432,#38433,#38434,#38435,#38436,#38437,#38438),.UNSPECIFIED.,
 .F.,.F.,(6,1,1,1,1,1,1,1,1,1,1,1,1,1,1,1,1,1,1,1,1,1,1,1,1,1,1,1,1,1,6),
(0.,0.0333333333333333,0.0666666666666667,0.1,0.133333333333333,0.166666666666667,
0.2,0.233333333333333,0.266666666666667,0.3,0.333333333333333,0.366666666666667,
0.4,0.433333333333333,0.466666666666667,0.5,0.533333333333333,0.566666666666667,
0.6,0.633333333333333,0.666666666666667,0.7,0.733333333333333,0.766666666666667,
0.8,0.833333333333333,0.866666666666667,0.9,0.933333333333333,0.966666666666667,
1.),.UNSPECIFIED.);
#537=B_SPLINE_CURVE_WITH_KNOTS('',5,(#38442,#38443,#38444,#38445,#38446,
#38447,#38448,#38449,#38450,#38451,#38452,#38453,#38454,#38455,#38456,#38457,
#38458,#38459,#38460,#38461,#38462,#38463,#38464,#38465,#38466,#38467,#38468,
#38469,#38470,#38471,#38472,#38473,#38474,#38475,#38476),.UNSPECIFIED.,
 .F.,.F.,(6,1,1,1,1,1,1,1,1,1,1,1,1,1,1,1,1,1,1,1,1,1,1,1,1,1,1,1,1,1,6),
(0.,0.0333333333333333,0.0666666666666667,0.1,0.133333333333333,0.166666666666667,
0.2,0.233333333333333,0.266666666666667,0.3,0.333333333333333,0.366666666666667,
0.4,0.433333333333333,0.466666666666667,0.5,0.533333333333333,0.566666666666667,
0.6,0.633333333333333,0.666666666666667,0.7,0.733333333333333,0.766666666666667,
0.8,0.833333333333333,0.866666666666667,0.9,0.933333333333333,0.966666666666667,
1.),.UNSPECIFIED.);
#538=B_SPLINE_CURVE_WITH_KNOTS('',5,(#38484,#38485,#38486,#38487,#38488,
#38489,#38490,#38491,#38492,#38493,#38494,#38495,#38496,#38497,#38498,#38499,
#38500,#38501,#38502,#38503,#38504,#38505,#38506,#38507,#38508,#38509,#38510,
#38511,#38512,#38513,#38514,#38515,#38516,#38517,#38518),.UNSPECIFIED.,
 .F.,.F.,(6,1,1,1,1,1,1,1,1,1,1,1,1,1,1,1,1,1,1,1,1,1,1,1,1,1,1,1,1,1,6),
(0.,0.0333333333333333,0.0666666666666667,0.1,0.133333333333333,0.166666666666667,
0.2,0.233333333333333,0.266666666666667,0.3,0.333333333333333,0.366666666666667,
0.4,0.433333333333333,0.466666666666667,0.5,0.533333333333333,0.566666666666667,
0.6,0.633333333333333,0.666666666666667,0.7,0.733333333333333,0.766666666666667,
0.8,0.833333333333333,0.866666666666667,0.9,0.933333333333333,0.966666666666667,
1.),.UNSPECIFIED.);
#539=B_SPLINE_CURVE_WITH_KNOTS('',5,(#38522,#38523,#38524,#38525,#38526,
#38527,#38528,#38529,#38530,#38531,#38532,#38533,#38534,#38535,#38536,#38537,
#38538,#38539,#38540,#38541,#38542,#38543,#38544,#38545,#38546,#38547,#38548,
#38549,#38550,#38551,#38552,#38553,#38554,#38555,#38556),.UNSPECIFIED.,
 .F.,.F.,(6,1,1,1,1,1,1,1,1,1,1,1,1,1,1,1,1,1,1,1,1,1,1,1,1,1,1,1,1,1,6),
(0.,0.0333333333333333,0.0666666666666667,0.1,0.133333333333333,0.166666666666667,
0.2,0.233333333333333,0.266666666666667,0.3,0.333333333333333,0.366666666666667,
0.4,0.433333333333333,0.466666666666667,0.5,0.533333333333333,0.566666666666667,
0.6,0.633333333333333,0.666666666666667,0.7,0.733333333333333,0.766666666666667,
0.8,0.833333333333333,0.866666666666667,0.9,0.933333333333333,0.966666666666667,
1.),.UNSPECIFIED.);
#540=B_SPLINE_CURVE_WITH_KNOTS('',5,(#38564,#38565,#38566,#38567,#38568,
#38569,#38570,#38571,#38572,#38573,#38574,#38575,#38576,#38577,#38578,#38579,
#38580,#38581,#38582,#38583,#38584,#38585,#38586,#38587,#38588,#38589,#38590,
#38591,#38592,#38593,#38594,#38595,#38596,#38597,#38598),.UNSPECIFIED.,
 .F.,.F.,(6,1,1,1,1,1,1,1,1,1,1,1,1,1,1,1,1,1,1,1,1,1,1,1,1,1,1,1,1,1,6),
(0.,0.0333333333333333,0.0666666666666667,0.1,0.133333333333333,0.166666666666667,
0.2,0.233333333333333,0.266666666666667,0.3,0.333333333333333,0.366666666666667,
0.4,0.433333333333333,0.466666666666667,0.5,0.533333333333333,0.566666666666667,
0.6,0.633333333333333,0.666666666666667,0.7,0.733333333333333,0.766666666666667,
0.8,0.833333333333333,0.866666666666667,0.9,0.933333333333333,0.966666666666667,
1.),.UNSPECIFIED.);
#541=B_SPLINE_CURVE_WITH_KNOTS('',5,(#38602,#38603,#38604,#38605,#38606,
#38607,#38608,#38609,#38610,#38611,#38612,#38613,#38614,#38615,#38616,#38617,
#38618,#38619,#38620,#38621,#38622,#38623,#38624,#38625,#38626,#38627,#38628,
#38629,#38630,#38631,#38632,#38633,#38634,#38635,#38636),.UNSPECIFIED.,
 .F.,.F.,(6,1,1,1,1,1,1,1,1,1,1,1,1,1,1,1,1,1,1,1,1,1,1,1,1,1,1,1,1,1,6),
(0.,0.0333333333333333,0.0666666666666667,0.1,0.133333333333333,0.166666666666667,
0.2,0.233333333333333,0.266666666666667,0.3,0.333333333333333,0.366666666666667,
0.4,0.433333333333333,0.466666666666667,0.5,0.533333333333333,0.566666666666667,
0.6,0.633333333333333,0.666666666666667,0.7,0.733333333333333,0.766666666666667,
0.8,0.833333333333333,0.866666666666667,0.9,0.933333333333333,0.966666666666667,
1.),.UNSPECIFIED.);
#542=B_SPLINE_CURVE_WITH_KNOTS('',5,(#38727,#38728,#38729,#38730,#38731,
#38732,#38733,#38734,#38735,#38736,#38737,#38738,#38739,#38740,#38741,#38742,
#38743,#38744,#38745,#38746,#38747,#38748,#38749,#38750,#38751,#38752,#38753,
#38754,#38755,#38756,#38757,#38758,#38759,#38760,#38761),.UNSPECIFIED.,
 .F.,.F.,(6,1,1,1,1,1,1,1,1,1,1,1,1,1,1,1,1,1,1,1,1,1,1,1,1,1,1,1,1,1,6),
(0.,0.0333333333333333,0.0666666666666667,0.1,0.133333333333333,0.166666666666667,
0.2,0.233333333333333,0.266666666666667,0.3,0.333333333333333,0.366666666666667,
0.4,0.433333333333333,0.466666666666667,0.5,0.533333333333333,0.566666666666667,
0.6,0.633333333333333,0.666666666666667,0.7,0.733333333333333,0.766666666666667,
0.8,0.833333333333333,0.866666666666667,0.9,0.933333333333333,0.966666666666667,
1.),.UNSPECIFIED.);
#543=B_SPLINE_CURVE_WITH_KNOTS('',5,(#38837,#38838,#38839,#38840,#38841,
#38842,#38843,#38844,#38845,#38846,#38847,#38848,#38849,#38850,#38851,#38852,
#38853,#38854,#38855,#38856,#38857,#38858,#38859,#38860,#38861,#38862,#38863,
#38864,#38865,#38866,#38867,#38868,#38869,#38870,#38871),.UNSPECIFIED.,
 .F.,.F.,(6,1,1,1,1,1,1,1,1,1,1,1,1,1,1,1,1,1,1,1,1,1,1,1,1,1,1,1,1,1,6),
(-1.,-0.966666666666667,-0.933333333333333,-0.9,-0.866666666666667,-0.833333333333333,
-0.8,-0.766666666666667,-0.733333333333333,-0.7,-0.666666666666667,-0.633333333333333,
-0.6,-0.566666666666667,-0.533333333333333,-0.5,-0.466666666666667,-0.433333333333333,
-0.4,-0.366666666666667,-0.333333333333333,-0.3,-0.266666666666667,-0.233333333333333,
-0.2,-0.166666666666667,-0.133333333333333,-0.1,-0.0666666666666667,-0.0333333333333333,
0.),.UNSPECIFIED.);
#544=B_SPLINE_CURVE_WITH_KNOTS('',5,(#38957,#38958,#38959,#38960,#38961,
#38962,#38963,#38964,#38965,#38966,#38967,#38968,#38969,#38970,#38971,#38972,
#38973,#38974,#38975,#38976,#38977,#38978,#38979,#38980,#38981,#38982,#38983,
#38984,#38985,#38986,#38987,#38988,#38989,#38990,#38991),.UNSPECIFIED.,
 .F.,.F.,(6,1,1,1,1,1,1,1,1,1,1,1,1,1,1,1,1,1,1,1,1,1,1,1,1,1,1,1,1,1,6),
(0.,0.0333333333333333,0.0666666666666667,0.1,0.133333333333333,0.166666666666667,
0.2,0.233333333333333,0.266666666666667,0.3,0.333333333333333,0.366666666666667,
0.4,0.433333333333333,0.466666666666667,0.5,0.533333333333333,0.566666666666667,
0.6,0.633333333333333,0.666666666666667,0.7,0.733333333333333,0.766666666666667,
0.8,0.833333333333333,0.866666666666667,0.9,0.933333333333333,0.966666666666667,
1.),.UNSPECIFIED.);
#545=B_SPLINE_CURVE_WITH_KNOTS('',5,(#39067,#39068,#39069,#39070,#39071,
#39072,#39073,#39074,#39075,#39076,#39077,#39078,#39079,#39080,#39081,#39082,
#39083,#39084,#39085,#39086,#39087,#39088,#39089,#39090,#39091,#39092,#39093,
#39094,#39095,#39096,#39097,#39098,#39099,#39100,#39101),.UNSPECIFIED.,
 .F.,.F.,(6,1,1,1,1,1,1,1,1,1,1,1,1,1,1,1,1,1,1,1,1,1,1,1,1,1,1,1,1,1,6),
(-1.,-0.966666666666667,-0.933333333333333,-0.9,-0.866666666666667,-0.833333333333333,
-0.8,-0.766666666666667,-0.733333333333333,-0.7,-0.666666666666667,-0.633333333333333,
-0.6,-0.566666666666667,-0.533333333333333,-0.5,-0.466666666666667,-0.433333333333333,
-0.4,-0.366666666666667,-0.333333333333333,-0.3,-0.266666666666667,-0.233333333333333,
-0.2,-0.166666666666667,-0.133333333333333,-0.1,-0.0666666666666667,-0.0333333333333333,
0.),.UNSPECIFIED.);
#546=B_SPLINE_CURVE_WITH_KNOTS('',5,(#39187,#39188,#39189,#39190,#39191,
#39192,#39193,#39194,#39195,#39196,#39197,#39198,#39199,#39200,#39201,#39202,
#39203,#39204,#39205,#39206,#39207,#39208,#39209,#39210,#39211,#39212,#39213,
#39214,#39215,#39216,#39217,#39218,#39219,#39220,#39221),.UNSPECIFIED.,
 .F.,.F.,(6,1,1,1,1,1,1,1,1,1,1,1,1,1,1,1,1,1,1,1,1,1,1,1,1,1,1,1,1,1,6),
(0.,0.0333333333333333,0.0666666666666667,0.1,0.133333333333333,0.166666666666667,
0.2,0.233333333333333,0.266666666666667,0.3,0.333333333333333,0.366666666666667,
0.4,0.433333333333333,0.466666666666667,0.5,0.533333333333333,0.566666666666667,
0.6,0.633333333333333,0.666666666666667,0.7,0.733333333333333,0.766666666666667,
0.8,0.833333333333333,0.866666666666667,0.9,0.933333333333333,0.966666666666667,
1.),.UNSPECIFIED.);
#547=B_SPLINE_CURVE_WITH_KNOTS('',5,(#39297,#39298,#39299,#39300,#39301,
#39302,#39303,#39304,#39305,#39306,#39307,#39308,#39309,#39310,#39311,#39312,
#39313,#39314,#39315,#39316,#39317,#39318,#39319,#39320,#39321,#39322,#39323,
#39324,#39325,#39326,#39327,#39328,#39329,#39330,#39331),.UNSPECIFIED.,
 .F.,.F.,(6,1,1,1,1,1,1,1,1,1,1,1,1,1,1,1,1,1,1,1,1,1,1,1,1,1,1,1,1,1,6),
(-1.,-0.966666666666667,-0.933333333333333,-0.9,-0.866666666666667,-0.833333333333333,
-0.8,-0.766666666666667,-0.733333333333333,-0.7,-0.666666666666667,-0.633333333333333,
-0.6,-0.566666666666667,-0.533333333333333,-0.5,-0.466666666666667,-0.433333333333333,
-0.4,-0.366666666666667,-0.333333333333333,-0.3,-0.266666666666667,-0.233333333333333,
-0.2,-0.166666666666667,-0.133333333333333,-0.1,-0.0666666666666667,-0.0333333333333333,
0.),.UNSPECIFIED.);
#548=B_SPLINE_CURVE_WITH_KNOTS('',5,(#39417,#39418,#39419,#39420,#39421,
#39422,#39423,#39424,#39425,#39426,#39427,#39428,#39429,#39430,#39431,#39432,
#39433,#39434,#39435,#39436,#39437,#39438,#39439,#39440,#39441,#39442,#39443,
#39444,#39445,#39446,#39447,#39448,#39449,#39450,#39451),.UNSPECIFIED.,
 .F.,.F.,(6,1,1,1,1,1,1,1,1,1,1,1,1,1,1,1,1,1,1,1,1,1,1,1,1,1,1,1,1,1,6),
(0.,0.0333333333333333,0.0666666666666667,0.1,0.133333333333333,0.166666666666667,
0.2,0.233333333333333,0.266666666666667,0.3,0.333333333333333,0.366666666666667,
0.4,0.433333333333333,0.466666666666667,0.5,0.533333333333333,0.566666666666667,
0.6,0.633333333333333,0.666666666666667,0.7,0.733333333333333,0.766666666666667,
0.8,0.833333333333333,0.866666666666667,0.9,0.933333333333333,0.966666666666667,
1.),.UNSPECIFIED.);
#549=B_SPLINE_CURVE_WITH_KNOTS('',5,(#39527,#39528,#39529,#39530,#39531,
#39532,#39533,#39534,#39535,#39536,#39537,#39538,#39539,#39540,#39541,#39542,
#39543,#39544,#39545,#39546,#39547,#39548,#39549,#39550,#39551,#39552,#39553,
#39554,#39555,#39556,#39557,#39558,#39559,#39560,#39561),.UNSPECIFIED.,
 .F.,.F.,(6,1,1,1,1,1,1,1,1,1,1,1,1,1,1,1,1,1,1,1,1,1,1,1,1,1,1,1,1,1,6),
(-1.,-0.966666666666667,-0.933333333333333,-0.9,-0.866666666666667,-0.833333333333333,
-0.8,-0.766666666666667,-0.733333333333333,-0.7,-0.666666666666667,-0.633333333333333,
-0.6,-0.566666666666667,-0.533333333333333,-0.5,-0.466666666666667,-0.433333333333333,
-0.4,-0.366666666666667,-0.333333333333333,-0.3,-0.266666666666667,-0.233333333333333,
-0.2,-0.166666666666667,-0.133333333333333,-0.1,-0.0666666666666667,-0.0333333333333333,
0.),.UNSPECIFIED.);
#550=B_SPLINE_CURVE_WITH_KNOTS('',5,(#39647,#39648,#39649,#39650,#39651,
#39652,#39653,#39654,#39655,#39656,#39657,#39658,#39659,#39660,#39661,#39662,
#39663,#39664,#39665,#39666,#39667,#39668,#39669,#39670,#39671,#39672,#39673,
#39674,#39675,#39676,#39677,#39678,#39679,#39680,#39681),.UNSPECIFIED.,
 .F.,.F.,(6,1,1,1,1,1,1,1,1,1,1,1,1,1,1,1,1,1,1,1,1,1,1,1,1,1,1,1,1,1,6),
(0.,0.0333333333333333,0.0666666666666667,0.1,0.133333333333333,0.166666666666667,
0.2,0.233333333333333,0.266666666666667,0.3,0.333333333333333,0.366666666666667,
0.4,0.433333333333333,0.466666666666667,0.5,0.533333333333333,0.566666666666667,
0.6,0.633333333333333,0.666666666666667,0.7,0.733333333333333,0.766666666666667,
0.8,0.833333333333333,0.866666666666667,0.9,0.933333333333333,0.966666666666667,
1.),.UNSPECIFIED.);
#551=B_SPLINE_CURVE_WITH_KNOTS('',5,(#39757,#39758,#39759,#39760,#39761,
#39762,#39763,#39764,#39765,#39766,#39767,#39768,#39769,#39770,#39771,#39772,
#39773,#39774,#39775,#39776,#39777,#39778,#39779,#39780,#39781,#39782,#39783,
#39784,#39785,#39786,#39787,#39788,#39789,#39790,#39791),.UNSPECIFIED.,
 .F.,.F.,(6,1,1,1,1,1,1,1,1,1,1,1,1,1,1,1,1,1,1,1,1,1,1,1,1,1,1,1,1,1,6),
(-1.,-0.966666666666667,-0.933333333333333,-0.9,-0.866666666666667,-0.833333333333333,
-0.8,-0.766666666666667,-0.733333333333333,-0.7,-0.666666666666667,-0.633333333333333,
-0.6,-0.566666666666667,-0.533333333333333,-0.5,-0.466666666666667,-0.433333333333333,
-0.4,-0.366666666666667,-0.333333333333333,-0.3,-0.266666666666667,-0.233333333333333,
-0.2,-0.166666666666667,-0.133333333333333,-0.1,-0.0666666666666667,-0.0333333333333333,
0.),.UNSPECIFIED.);
#552=B_SPLINE_CURVE_WITH_KNOTS('',5,(#39877,#39878,#39879,#39880,#39881,
#39882,#39883,#39884,#39885,#39886,#39887,#39888,#39889,#39890,#39891,#39892,
#39893,#39894,#39895,#39896,#39897,#39898,#39899,#39900,#39901,#39902,#39903,
#39904,#39905,#39906,#39907,#39908,#39909,#39910,#39911),.UNSPECIFIED.,
 .F.,.F.,(6,1,1,1,1,1,1,1,1,1,1,1,1,1,1,1,1,1,1,1,1,1,1,1,1,1,1,1,1,1,6),
(0.,0.0333333333333333,0.0666666666666667,0.1,0.133333333333333,0.166666666666667,
0.2,0.233333333333333,0.266666666666667,0.3,0.333333333333333,0.366666666666667,
0.4,0.433333333333333,0.466666666666667,0.5,0.533333333333333,0.566666666666667,
0.6,0.633333333333333,0.666666666666667,0.7,0.733333333333333,0.766666666666667,
0.8,0.833333333333333,0.866666666666667,0.9,0.933333333333333,0.966666666666667,
1.),.UNSPECIFIED.);
#553=B_SPLINE_CURVE_WITH_KNOTS('',5,(#39987,#39988,#39989,#39990,#39991,
#39992,#39993,#39994,#39995,#39996,#39997,#39998,#39999,#40000,#40001,#40002,
#40003,#40004,#40005,#40006,#40007,#40008,#40009,#40010,#40011,#40012,#40013,
#40014,#40015,#40016,#40017,#40018,#40019,#40020,#40021),.UNSPECIFIED.,
 .F.,.F.,(6,1,1,1,1,1,1,1,1,1,1,1,1,1,1,1,1,1,1,1,1,1,1,1,1,1,1,1,1,1,6),
(-1.,-0.966666666666667,-0.933333333333333,-0.9,-0.866666666666667,-0.833333333333333,
-0.8,-0.766666666666667,-0.733333333333333,-0.7,-0.666666666666667,-0.633333333333333,
-0.6,-0.566666666666667,-0.533333333333333,-0.5,-0.466666666666667,-0.433333333333333,
-0.4,-0.366666666666667,-0.333333333333333,-0.3,-0.266666666666667,-0.233333333333333,
-0.2,-0.166666666666667,-0.133333333333333,-0.1,-0.0666666666666667,-0.0333333333333333,
0.),.UNSPECIFIED.);
#554=B_SPLINE_CURVE_WITH_KNOTS('',5,(#40107,#40108,#40109,#40110,#40111,
#40112,#40113,#40114,#40115,#40116,#40117,#40118,#40119,#40120,#40121,#40122,
#40123,#40124,#40125,#40126,#40127,#40128,#40129,#40130,#40131,#40132,#40133,
#40134,#40135,#40136,#40137,#40138,#40139,#40140,#40141),.UNSPECIFIED.,
 .F.,.F.,(6,1,1,1,1,1,1,1,1,1,1,1,1,1,1,1,1,1,1,1,1,1,1,1,1,1,1,1,1,1,6),
(0.,0.0333333333333333,0.0666666666666667,0.1,0.133333333333333,0.166666666666667,
0.2,0.233333333333333,0.266666666666667,0.3,0.333333333333333,0.366666666666667,
0.4,0.433333333333333,0.466666666666667,0.5,0.533333333333333,0.566666666666667,
0.6,0.633333333333333,0.666666666666667,0.7,0.733333333333333,0.766666666666667,
0.8,0.833333333333333,0.866666666666667,0.9,0.933333333333333,0.966666666666667,
1.),.UNSPECIFIED.);
#555=B_SPLINE_CURVE_WITH_KNOTS('',5,(#40217,#40218,#40219,#40220,#40221,
#40222,#40223,#40224,#40225,#40226,#40227,#40228,#40229,#40230,#40231,#40232,
#40233,#40234,#40235,#40236,#40237,#40238,#40239,#40240,#40241,#40242,#40243,
#40244,#40245,#40246,#40247,#40248,#40249,#40250,#40251),.UNSPECIFIED.,
 .F.,.F.,(6,1,1,1,1,1,1,1,1,1,1,1,1,1,1,1,1,1,1,1,1,1,1,1,1,1,1,1,1,1,6),
(-1.,-0.966666666666667,-0.933333333333333,-0.9,-0.866666666666667,-0.833333333333333,
-0.8,-0.766666666666667,-0.733333333333333,-0.7,-0.666666666666667,-0.633333333333333,
-0.6,-0.566666666666667,-0.533333333333333,-0.5,-0.466666666666667,-0.433333333333333,
-0.4,-0.366666666666667,-0.333333333333333,-0.3,-0.266666666666667,-0.233333333333333,
-0.2,-0.166666666666667,-0.133333333333333,-0.1,-0.0666666666666667,-0.0333333333333333,
0.),.UNSPECIFIED.);
#556=B_SPLINE_CURVE_WITH_KNOTS('',5,(#40337,#40338,#40339,#40340,#40341,
#40342,#40343,#40344,#40345,#40346,#40347,#40348,#40349,#40350,#40351,#40352,
#40353,#40354,#40355,#40356,#40357,#40358,#40359,#40360,#40361,#40362,#40363,
#40364,#40365,#40366,#40367,#40368,#40369,#40370,#40371),.UNSPECIFIED.,
 .F.,.F.,(6,1,1,1,1,1,1,1,1,1,1,1,1,1,1,1,1,1,1,1,1,1,1,1,1,1,1,1,1,1,6),
(0.,0.0333333333333333,0.0666666666666667,0.1,0.133333333333333,0.166666666666667,
0.2,0.233333333333333,0.266666666666667,0.3,0.333333333333333,0.366666666666667,
0.4,0.433333333333333,0.466666666666667,0.5,0.533333333333333,0.566666666666667,
0.6,0.633333333333333,0.666666666666667,0.7,0.733333333333333,0.766666666666667,
0.8,0.833333333333333,0.866666666666667,0.9,0.933333333333333,0.966666666666667,
1.),.UNSPECIFIED.);
#557=B_SPLINE_CURVE_WITH_KNOTS('',5,(#40447,#40448,#40449,#40450,#40451,
#40452,#40453,#40454,#40455,#40456,#40457,#40458,#40459,#40460,#40461,#40462,
#40463,#40464,#40465,#40466,#40467,#40468,#40469,#40470,#40471,#40472,#40473,
#40474,#40475,#40476,#40477,#40478,#40479,#40480,#40481),.UNSPECIFIED.,
 .F.,.F.,(6,1,1,1,1,1,1,1,1,1,1,1,1,1,1,1,1,1,1,1,1,1,1,1,1,1,1,1,1,1,6),
(-1.,-0.966666666666667,-0.933333333333333,-0.9,-0.866666666666667,-0.833333333333333,
-0.8,-0.766666666666667,-0.733333333333333,-0.7,-0.666666666666667,-0.633333333333333,
-0.6,-0.566666666666667,-0.533333333333333,-0.5,-0.466666666666667,-0.433333333333333,
-0.4,-0.366666666666667,-0.333333333333333,-0.3,-0.266666666666667,-0.233333333333333,
-0.2,-0.166666666666667,-0.133333333333333,-0.1,-0.0666666666666667,-0.0333333333333333,
0.),.UNSPECIFIED.);
#558=B_SPLINE_CURVE_WITH_KNOTS('',5,(#40567,#40568,#40569,#40570,#40571,
#40572,#40573,#40574,#40575,#40576,#40577,#40578,#40579,#40580,#40581,#40582,
#40583,#40584,#40585,#40586,#40587,#40588,#40589,#40590,#40591,#40592,#40593,
#40594,#40595,#40596,#40597,#40598,#40599,#40600,#40601),.UNSPECIFIED.,
 .F.,.F.,(6,1,1,1,1,1,1,1,1,1,1,1,1,1,1,1,1,1,1,1,1,1,1,1,1,1,1,1,1,1,6),
(0.,0.0333333333333333,0.0666666666666667,0.1,0.133333333333333,0.166666666666667,
0.2,0.233333333333333,0.266666666666667,0.3,0.333333333333333,0.366666666666667,
0.4,0.433333333333333,0.466666666666667,0.5,0.533333333333333,0.566666666666667,
0.6,0.633333333333333,0.666666666666667,0.7,0.733333333333333,0.766666666666667,
0.8,0.833333333333333,0.866666666666667,0.9,0.933333333333333,0.966666666666667,
1.),.UNSPECIFIED.);
#559=B_SPLINE_CURVE_WITH_KNOTS('',5,(#40677,#40678,#40679,#40680,#40681,
#40682,#40683,#40684,#40685,#40686,#40687,#40688,#40689,#40690,#40691,#40692,
#40693,#40694,#40695,#40696,#40697,#40698,#40699,#40700,#40701,#40702,#40703,
#40704,#40705,#40706,#40707,#40708,#40709,#40710,#40711),.UNSPECIFIED.,
 .F.,.F.,(6,1,1,1,1,1,1,1,1,1,1,1,1,1,1,1,1,1,1,1,1,1,1,1,1,1,1,1,1,1,6),
(-1.,-0.966666666666667,-0.933333333333333,-0.9,-0.866666666666667,-0.833333333333333,
-0.8,-0.766666666666667,-0.733333333333333,-0.7,-0.666666666666667,-0.633333333333333,
-0.6,-0.566666666666667,-0.533333333333333,-0.5,-0.466666666666667,-0.433333333333333,
-0.4,-0.366666666666667,-0.333333333333333,-0.3,-0.266666666666667,-0.233333333333333,
-0.2,-0.166666666666667,-0.133333333333333,-0.1,-0.0666666666666667,-0.0333333333333333,
0.),.UNSPECIFIED.);
#560=B_SPLINE_CURVE_WITH_KNOTS('',5,(#40797,#40798,#40799,#40800,#40801,
#40802,#40803,#40804,#40805,#40806,#40807,#40808,#40809,#40810,#40811,#40812,
#40813,#40814,#40815,#40816,#40817,#40818,#40819,#40820,#40821,#40822,#40823,
#40824,#40825,#40826,#40827,#40828,#40829,#40830,#40831),.UNSPECIFIED.,
 .F.,.F.,(6,1,1,1,1,1,1,1,1,1,1,1,1,1,1,1,1,1,1,1,1,1,1,1,1,1,1,1,1,1,6),
(0.,0.0333333333333333,0.0666666666666667,0.1,0.133333333333333,0.166666666666667,
0.2,0.233333333333333,0.266666666666667,0.3,0.333333333333333,0.366666666666667,
0.4,0.433333333333333,0.466666666666667,0.5,0.533333333333333,0.566666666666667,
0.6,0.633333333333333,0.666666666666667,0.7,0.733333333333333,0.766666666666667,
0.8,0.833333333333333,0.866666666666667,0.9,0.933333333333333,0.966666666666667,
1.),.UNSPECIFIED.);
#561=B_SPLINE_CURVE_WITH_KNOTS('',5,(#40907,#40908,#40909,#40910,#40911,
#40912,#40913,#40914,#40915,#40916,#40917,#40918,#40919,#40920,#40921,#40922,
#40923,#40924,#40925,#40926,#40927,#40928,#40929,#40930,#40931,#40932,#40933,
#40934,#40935,#40936,#40937,#40938,#40939,#40940,#40941),.UNSPECIFIED.,
 .F.,.F.,(6,1,1,1,1,1,1,1,1,1,1,1,1,1,1,1,1,1,1,1,1,1,1,1,1,1,1,1,1,1,6),
(-1.,-0.966666666666667,-0.933333333333333,-0.9,-0.866666666666667,-0.833333333333333,
-0.8,-0.766666666666667,-0.733333333333333,-0.7,-0.666666666666667,-0.633333333333333,
-0.6,-0.566666666666667,-0.533333333333333,-0.5,-0.466666666666667,-0.433333333333333,
-0.4,-0.366666666666667,-0.333333333333333,-0.3,-0.266666666666667,-0.233333333333333,
-0.2,-0.166666666666667,-0.133333333333333,-0.1,-0.0666666666666667,-0.0333333333333333,
0.),.UNSPECIFIED.);
#562=B_SPLINE_CURVE_WITH_KNOTS('',5,(#41027,#41028,#41029,#41030,#41031,
#41032,#41033,#41034,#41035,#41036,#41037,#41038,#41039,#41040,#41041,#41042,
#41043,#41044,#41045,#41046,#41047,#41048,#41049,#41050,#41051,#41052,#41053,
#41054,#41055,#41056,#41057,#41058,#41059,#41060,#41061),.UNSPECIFIED.,
 .F.,.F.,(6,1,1,1,1,1,1,1,1,1,1,1,1,1,1,1,1,1,1,1,1,1,1,1,1,1,1,1,1,1,6),
(0.,0.0333333333333333,0.0666666666666667,0.1,0.133333333333333,0.166666666666667,
0.2,0.233333333333333,0.266666666666667,0.3,0.333333333333333,0.366666666666667,
0.4,0.433333333333333,0.466666666666667,0.5,0.533333333333333,0.566666666666667,
0.6,0.633333333333333,0.666666666666667,0.7,0.733333333333333,0.766666666666667,
0.8,0.833333333333333,0.866666666666667,0.9,0.933333333333333,0.966666666666667,
1.),.UNSPECIFIED.);
#563=B_SPLINE_CURVE_WITH_KNOTS('',5,(#41137,#41138,#41139,#41140,#41141,
#41142,#41143,#41144,#41145,#41146,#41147,#41148,#41149,#41150,#41151,#41152,
#41153,#41154,#41155,#41156,#41157,#41158,#41159,#41160,#41161,#41162,#41163,
#41164,#41165,#41166,#41167,#41168,#41169,#41170,#41171),.UNSPECIFIED.,
 .F.,.F.,(6,1,1,1,1,1,1,1,1,1,1,1,1,1,1,1,1,1,1,1,1,1,1,1,1,1,1,1,1,1,6),
(-1.,-0.966666666666667,-0.933333333333333,-0.9,-0.866666666666667,-0.833333333333333,
-0.8,-0.766666666666667,-0.733333333333333,-0.7,-0.666666666666667,-0.633333333333333,
-0.6,-0.566666666666667,-0.533333333333333,-0.5,-0.466666666666667,-0.433333333333333,
-0.4,-0.366666666666667,-0.333333333333333,-0.3,-0.266666666666667,-0.233333333333333,
-0.2,-0.166666666666667,-0.133333333333333,-0.1,-0.0666666666666667,-0.0333333333333333,
0.),.UNSPECIFIED.);
#564=B_SPLINE_CURVE_WITH_KNOTS('',5,(#41257,#41258,#41259,#41260,#41261,
#41262,#41263,#41264,#41265,#41266,#41267,#41268,#41269,#41270,#41271,#41272,
#41273,#41274,#41275,#41276,#41277,#41278,#41279,#41280,#41281,#41282,#41283,
#41284,#41285,#41286,#41287,#41288,#41289,#41290,#41291),.UNSPECIFIED.,
 .F.,.F.,(6,1,1,1,1,1,1,1,1,1,1,1,1,1,1,1,1,1,1,1,1,1,1,1,1,1,1,1,1,1,6),
(0.,0.0333333333333333,0.0666666666666667,0.1,0.133333333333333,0.166666666666667,
0.2,0.233333333333333,0.266666666666667,0.3,0.333333333333333,0.366666666666667,
0.4,0.433333333333333,0.466666666666667,0.5,0.533333333333333,0.566666666666667,
0.6,0.633333333333333,0.666666666666667,0.7,0.733333333333333,0.766666666666667,
0.8,0.833333333333333,0.866666666666667,0.9,0.933333333333333,0.966666666666667,
1.),.UNSPECIFIED.);
#565=B_SPLINE_CURVE_WITH_KNOTS('',5,(#41367,#41368,#41369,#41370,#41371,
#41372,#41373,#41374,#41375,#41376,#41377,#41378,#41379,#41380,#41381,#41382,
#41383,#41384,#41385,#41386,#41387,#41388,#41389,#41390,#41391,#41392,#41393,
#41394,#41395,#41396,#41397,#41398,#41399,#41400,#41401),.UNSPECIFIED.,
 .F.,.F.,(6,1,1,1,1,1,1,1,1,1,1,1,1,1,1,1,1,1,1,1,1,1,1,1,1,1,1,1,1,1,6),
(-1.,-0.966666666666667,-0.933333333333333,-0.9,-0.866666666666667,-0.833333333333333,
-0.8,-0.766666666666667,-0.733333333333333,-0.7,-0.666666666666667,-0.633333333333333,
-0.6,-0.566666666666667,-0.533333333333333,-0.5,-0.466666666666667,-0.433333333333333,
-0.4,-0.366666666666667,-0.333333333333333,-0.3,-0.266666666666667,-0.233333333333333,
-0.2,-0.166666666666667,-0.133333333333333,-0.1,-0.0666666666666667,-0.0333333333333333,
0.),.UNSPECIFIED.);
#566=B_SPLINE_CURVE_WITH_KNOTS('',5,(#41487,#41488,#41489,#41490,#41491,
#41492,#41493,#41494,#41495,#41496,#41497,#41498,#41499,#41500,#41501,#41502,
#41503,#41504,#41505,#41506,#41507,#41508,#41509,#41510,#41511,#41512,#41513,
#41514,#41515,#41516,#41517,#41518,#41519,#41520,#41521),.UNSPECIFIED.,
 .F.,.F.,(6,1,1,1,1,1,1,1,1,1,1,1,1,1,1,1,1,1,1,1,1,1,1,1,1,1,1,1,1,1,6),
(0.,0.0333333333333333,0.0666666666666667,0.1,0.133333333333333,0.166666666666667,
0.2,0.233333333333333,0.266666666666667,0.3,0.333333333333333,0.366666666666667,
0.4,0.433333333333333,0.466666666666667,0.5,0.533333333333333,0.566666666666667,
0.6,0.633333333333333,0.666666666666667,0.7,0.733333333333333,0.766666666666667,
0.8,0.833333333333333,0.866666666666667,0.9,0.933333333333333,0.966666666666667,
1.),.UNSPECIFIED.);
#567=B_SPLINE_CURVE_WITH_KNOTS('',5,(#41597,#41598,#41599,#41600,#41601,
#41602,#41603,#41604,#41605,#41606,#41607,#41608,#41609,#41610,#41611,#41612,
#41613,#41614,#41615,#41616,#41617,#41618,#41619,#41620,#41621,#41622,#41623,
#41624,#41625,#41626,#41627,#41628,#41629,#41630,#41631),.UNSPECIFIED.,
 .F.,.F.,(6,1,1,1,1,1,1,1,1,1,1,1,1,1,1,1,1,1,1,1,1,1,1,1,1,1,1,1,1,1,6),
(-1.,-0.966666666666667,-0.933333333333333,-0.9,-0.866666666666667,-0.833333333333333,
-0.8,-0.766666666666667,-0.733333333333333,-0.7,-0.666666666666667,-0.633333333333333,
-0.6,-0.566666666666667,-0.533333333333333,-0.5,-0.466666666666667,-0.433333333333333,
-0.4,-0.366666666666667,-0.333333333333333,-0.3,-0.266666666666667,-0.233333333333333,
-0.2,-0.166666666666667,-0.133333333333333,-0.1,-0.0666666666666667,-0.0333333333333333,
0.),.UNSPECIFIED.);
#568=B_SPLINE_CURVE_WITH_KNOTS('',5,(#41722,#41723,#41724,#41725,#41726,
#41727,#41728,#41729,#41730,#41731,#41732,#41733,#41734,#41735,#41736,#41737,
#41738,#41739,#41740,#41741,#41742,#41743,#41744,#41745,#41746,#41747,#41748,
#41749,#41750,#41751,#41752,#41753,#41754,#41755,#41756),.UNSPECIFIED.,
 .F.,.F.,(6,1,1,1,1,1,1,1,1,1,1,1,1,1,1,1,1,1,1,1,1,1,1,1,1,1,1,1,1,1,6),
(0.,0.0333333333333333,0.0666666666666667,0.1,0.133333333333333,0.166666666666667,
0.2,0.233333333333333,0.266666666666667,0.3,0.333333333333333,0.366666666666667,
0.4,0.433333333333333,0.466666666666667,0.5,0.533333333333333,0.566666666666667,
0.6,0.633333333333333,0.666666666666667,0.7,0.733333333333333,0.766666666666667,
0.8,0.833333333333333,0.866666666666667,0.9,0.933333333333333,0.966666666666667,
1.),.UNSPECIFIED.);
#569=B_SPLINE_CURVE_WITH_KNOTS('',5,(#41827,#41828,#41829,#41830,#41831,
#41832,#41833,#41834,#41835,#41836,#41837,#41838,#41839,#41840,#41841,#41842,
#41843,#41844,#41845,#41846,#41847,#41848,#41849,#41850,#41851,#41852,#41853,
#41854,#41855,#41856,#41857,#41858,#41859,#41860,#41861),.UNSPECIFIED.,
 .F.,.F.,(6,1,1,1,1,1,1,1,1,1,1,1,1,1,1,1,1,1,1,1,1,1,1,1,1,1,1,1,1,1,6),
(-1.,-0.966666666666667,-0.933333333333333,-0.9,-0.866666666666667,-0.833333333333333,
-0.8,-0.766666666666667,-0.733333333333333,-0.7,-0.666666666666667,-0.633333333333333,
-0.6,-0.566666666666667,-0.533333333333333,-0.5,-0.466666666666667,-0.433333333333333,
-0.4,-0.366666666666667,-0.333333333333333,-0.3,-0.266666666666667,-0.233333333333333,
-0.2,-0.166666666666667,-0.133333333333333,-0.1,-0.0666666666666667,-0.0333333333333333,
0.),.UNSPECIFIED.);
#570=B_SPLINE_CURVE_WITH_KNOTS('',5,(#41868,#41869,#41870,#41871,#41872,
#41873,#41874,#41875,#41876,#41877,#41878,#41879,#41880,#41881,#41882,#41883,
#41884,#41885,#41886,#41887,#41888,#41889,#41890,#41891,#41892,#41893,#41894,
#41895,#41896,#41897,#41898,#41899,#41900,#41901,#41902),.UNSPECIFIED.,
 .F.,.F.,(6,1,1,1,1,1,1,1,1,1,1,1,1,1,1,1,1,1,1,1,1,1,1,1,1,1,1,1,1,1,6),
(0.,0.0333333333333333,0.0666666666666667,0.1,0.133333333333333,0.166666666666667,
0.2,0.233333333333333,0.266666666666667,0.3,0.333333333333333,0.366666666666667,
0.4,0.433333333333333,0.466666666666667,0.5,0.533333333333333,0.566666666666667,
0.6,0.633333333333333,0.666666666666667,0.7,0.733333333333333,0.766666666666667,
0.8,0.833333333333333,0.866666666666667,0.9,0.933333333333333,0.966666666666667,
1.),.UNSPECIFIED.);
#571=B_SPLINE_CURVE_WITH_KNOTS('',5,(#41906,#41907,#41908,#41909,#41910,
#41911,#41912,#41913,#41914,#41915,#41916,#41917,#41918,#41919,#41920,#41921,
#41922,#41923,#41924,#41925,#41926,#41927,#41928,#41929,#41930,#41931,#41932,
#41933,#41934,#41935,#41936,#41937,#41938,#41939,#41940),.UNSPECIFIED.,
 .F.,.F.,(6,1,1,1,1,1,1,1,1,1,1,1,1,1,1,1,1,1,1,1,1,1,1,1,1,1,1,1,1,1,6),
(-1.,-0.966666666666667,-0.933333333333333,-0.9,-0.866666666666667,-0.833333333333333,
-0.8,-0.766666666666667,-0.733333333333333,-0.7,-0.666666666666667,-0.633333333333333,
-0.6,-0.566666666666667,-0.533333333333333,-0.5,-0.466666666666667,-0.433333333333333,
-0.4,-0.366666666666667,-0.333333333333333,-0.3,-0.266666666666667,-0.233333333333333,
-0.2,-0.166666666666667,-0.133333333333333,-0.1,-0.0666666666666667,-0.0333333333333333,
0.),.UNSPECIFIED.);
#572=B_SPLINE_CURVE_WITH_KNOTS('',3,(#42119,#42120,#42121,#42122,#42123,
#42124,#42125,#42126,#42127,#42128,#42129,#42130,#42131,#42132,#42133,#42134,
#42135,#42136,#42137,#42138,#42139,#42140,#42141,#42142,#42143,#42144,#42145,
#42146,#42147,#42148,#42149,#42150,#42151,#42152,#42153,#42154,#42155,#42156,
#42157,#42158,#42159,#42160,#42161,#42162,#42163,#42164,#42165,#42166,#42167,
#42168,#42169,#42170,#42171,#42172,#42173,#42174,#42175,#42176,#42177,#42178,
#42179,#42180,#42181,#42182,#42183,#42184,#42185,#42186,#42187,#42188,#42189,
#42190,#42191,#42192,#42193,#42194,#42195,#42196,#42197,#42198,#42199,#42200,
#42201,#42202,#42203,#42204,#42205,#42206,#42207,#42208,#42209,#42210,#42211,
#42212,#42213,#42214,#42215),.UNSPECIFIED.,.F.,.F.,(4,3,3,3,3,3,3,3,3,3,
3,3,3,3,3,3,3,3,3,3,3,3,3,3,3,3,3,3,3,3,3,3,4),(10.375658882214,10.4940757531313,
10.6123285343078,10.7304723820773,10.8485622595653,10.9667391963694,11.0849569770027,
11.2034015018678,11.2943915536004,11.4190730285709,11.5387903701137,11.6583914925965,
11.7779288428205,11.8974547568011,12.0171050008759,12.1368293768595,12.2567726910946,
12.2918433533645,12.416524828335,12.535895449855,12.655144429834,12.7743249216265,
12.8934899602376,13.0127760613286,13.1321339785519,13.2517111469998,13.2892951531286,
13.4090351474352,13.5285879960393,13.6480165300828,13.7673687408495,13.8867531641114,
13.9755457854933),.UNSPECIFIED.);
#573=B_SPLINE_CURVE_WITH_KNOTS('',3,(#42218,#42219,#42220,#42221,#42222,
#42223,#42224,#42225,#42226,#42227,#42228,#42229,#42230,#42231,#42232,#42233,
#42234,#42235,#42236,#42237,#42238,#42239,#42240,#42241,#42242,#42243,#42244,
#42245,#42246,#42247,#42248,#42249,#42250,#42251,#42252,#42253,#42254,#42255,
#42256,#42257,#42258,#42259,#42260,#42261,#42262,#42263,#42264,#42265,#42266,
#42267,#42268,#42269,#42270,#42271,#42272,#42273,#42274,#42275,#42276,#42277,
#42278),.UNSPECIFIED.,.F.,.F.,(4,3,3,3,3,3,3,3,3,3,3,3,3,3,3,3,3,3,3,3,
4),(11.6159397475002,11.7406212224707,11.8630161036116,11.9853820192075,
12.1077619590757,12.2341693561229,12.3568053456408,12.4850984464526,12.6133915472643,
12.7380730222348,12.8564493642578,12.9746907770413,13.092852164952,13.2109882875043,
13.3292381165421,13.4475540306047,13.5660912434974,13.6108433470284,13.7306772169464,
13.8535403363031,13.9764034556599),.UNSPECIFIED.);
#574=B_SPLINE_CURVE_WITH_KNOTS('',3,(#42284,#42285,#42286,#42287,#42288,
#42289,#42290,#42291),.UNSPECIFIED.,.F.,.F.,(4,1,1,1,1,4),(15.707963267949,
16.2816505524208,17.2791023521849,18.2765541519489,19.274005951713,20.2591548474271),
 .UNSPECIFIED.);
#575=B_SPLINE_CURVE_WITH_KNOTS('',3,(#42292,#42293,#42294,#42295,#42296,
#42297,#42298,#42299,#42300,#42301,#42302,#42303,#42304,#42305,#42306,#42307,
#42308,#42309,#42310,#42311,#42312,#42313,#42314,#42315,#42316,#42317,#42318,
#42319,#42320,#42321,#42322,#42323,#42324,#42325,#42326,#42327,#42328,#42329,
#42330,#42331,#42332,#42333,#42334,#42335,#42336,#42337,#42338,#42339,#42340),
 .UNSPECIFIED.,.F.,.F.,(4,3,3,3,3,3,3,3,3,3,3,3,3,3,3,3,4),(13.9755457854933,
14.0950474522977,14.2147780392736,14.2867469528926,14.4114284278631,14.5309629044171,
14.6503778549302,14.7697261077932,14.8890603761317,15.0085166358431,15.1280454520991,
15.2477928763345,15.2841987526567,15.4149977650239,15.5453793024121,15.6751404895075,
15.707963267949),.UNSPECIFIED.);
#576=B_SPLINE_CURVE_WITH_KNOTS('',3,(#42342,#42343,#42344,#42345,#42346,
#42347,#42348,#42349,#42350,#42351,#42352,#42353,#42354,#42355,#42356,#42357,
#42358,#42359,#42360,#42361,#42362,#42363,#42364,#42365,#42366,#42367,#42368,
#42369,#42370,#42371,#42372,#42373,#42374,#42375,#42376,#42377,#42378,#42379,
#42380,#42381,#42382,#42383,#42384,#42385,#42386,#42387,#42388,#42389,#42390),
 .UNSPECIFIED.,.F.,.F.,(4,3,3,3,3,3,3,3,3,3,3,3,3,3,3,3,4),(13.9764034556599,
14.0958475312092,14.2152765458788,14.3348246052786,14.4544439781282,14.5742776798784,
14.6082951467925,14.732976621763,14.8526939294842,14.9722950172258,15.0918323318563,
15.2113582094568,15.3310084162456,15.4507327543743,15.5706760302905,15.6057469465565,
15.707963267949),.UNSPECIFIED.);
#577=B_SPLINE_CURVE_WITH_KNOTS('',3,(#42391,#42392,#42393,#42394,#42395,
#42396,#42397,#42398,#42399,#42400,#42401,#42402,#42403,#42404,#42405,#42406,
#42407,#42408,#42409,#42410,#42411,#42412,#42413,#42414,#42415,#42416,#42417,
#42418,#42419,#42420,#42421,#42422,#42423,#42424,#42425,#42426,#42427,#42428,
#42429,#42430,#42431,#42432,#42433,#42434,#42435,#42436,#42437,#42438,#42439,
#42440,#42441,#42442,#42443,#42444,#42445,#42446,#42447,#42448,#42449,#42450,
#42451,#42452,#42453,#42454,#42455,#42456,#42457,#42458,#42459,#42460,#42461,
#42462,#42463,#42464,#42465,#42466,#42467,#42468,#42469,#42470,#42471,#42472,
#42473,#42474,#42475,#42476,#42477,#42478,#42479,#42480,#42481,#42482,#42483,
#42484,#42485,#42486,#42487,#42488,#42489,#42490,#42491,#42492,#42493,#42494,
#42495,#42496,#42497,#42498,#42499,#42500,#42501,#42502,#42503,#42504,#42505,
#42506,#42507,#42508,#42509,#42510,#42511,#42512,#42513,#42514,#42515,#42516,
#42517,#42518,#42519,#42520,#42521,#42522),.UNSPECIFIED.,.F.,.F.,(4,2,2,
2,2,2,2,2,2,2,2,2,2,2,2,2,2,2,2,2,2,2,2,2,2,2,2,2,2,2,2,2,2,2,2,2,2,2,2,
2,2,2,2,2,2,2,2,2,2,2,2,2,2,2,2,2,2,2,2,2,2,2,2,2,2,4),(-1.4844552026344,
-1.4687011027748,-1.44918397915652,-1.44256183555755,-1.43903750723833,
-1.43605059148294,-1.43240348709774,-1.42536314863845,-1.39659887439657,
-1.38770269719831,-1.38202502955999,-1.37970402710656,-1.37799993621768,
-1.37597493952397,-1.37216460249553,-1.35415839979739,-1.33678878154718,
-1.32633578172632,-1.32217004114304,-1.31910561777712,-1.31582777999402,
-1.31053219723985,-1.28253713340363,-1.27130417776362,-1.26675415588416,
-1.263239795581,-1.26129440045607,-1.25955561692127,-1.25744215010448,-1.25204579873155,
-1.22788915726227,-1.21371449333436,-1.20700536901352,-1.20344927278234,
-1.20044123866201,-1.19677420197572,-1.18947140855754,-1.16322223138289,
-1.15299657988415,-1.14676844006402,-1.1443565384256,-1.14263564515379,
-1.14065300064361,-1.13703741418214,-1.11526709117371,-1.09576750079987,
-1.08913123132775,-1.08559192209381,-1.08258745843083,-1.07891171828405,
-1.07178573968222,-1.04544936146396,-1.03520056552958,-1.02896468341169,
-1.02655299984568,-1.02483256359335,-1.02284935705574,-1.01923551350903,
-0.992909690546232,-0.974649809101956,-0.969804634397468,-0.966621120941967,
-0.96354867336833,-0.959827504685779,-0.950405395849426,-0.946967500878228),
 .UNSPECIFIED.);
#578=B_SPLINE_CURVE_WITH_KNOTS('',3,(#42528,#42529,#42530,#42531,#42532,
#42533,#42534,#42535,#42536,#42537,#42538,#42539,#42540,#42541,#42542,#42543,
#42544,#42545,#42546,#42547,#42548,#42549,#42550,#42551,#42552,#42553,#42554,
#42555,#42556,#42557,#42558,#42559,#42560,#42561,#42562,#42563,#42564,#42565,
#42566,#42567,#42568,#42569,#42570,#42571,#42572,#42573,#42574,#42575,#42576,
#42577,#42578,#42579,#42580,#42581,#42582,#42583,#42584,#42585,#42586,#42587,
#42588,#42589,#42590,#42591,#42592,#42593,#42594,#42595,#42596,#42597,#42598,
#42599,#42600,#42601,#42602,#42603,#42604,#42605,#42606,#42607,#42608,#42609,
#42610,#42611,#42612,#42613,#42614,#42615,#42616,#42617,#42618,#42619,#42620,
#42621,#42622,#42623,#42624,#42625,#42626,#42627,#42628,#42629,#42630,#42631,
#42632,#42633,#42634,#42635,#42636,#42637,#42638,#42639,#42640,#42641,#42642,
#42643,#42644,#42645,#42646,#42647,#42648,#42649,#42650,#42651),
 .UNSPECIFIED.,.F.,.F.,(4,3,3,3,3,3,3,3,3,3,3,3,3,3,3,3,3,3,3,3,3,3,3,3,
3,3,3,3,3,3,3,3,3,3,3,3,3,3,3,3,3,4),(21.9911485751285,22.1403488486178,
22.2663613510052,22.3910428259757,22.5105544745963,22.6299461484162,22.7492707221346,
22.8685809545573,22.9880128266408,23.1075170226214,23.2272397326252,23.2638131507693,
23.3884946257398,23.5080061717731,23.6273977426734,23.7467222133455,23.8660323428005,
23.9854641128103,24.1049682071207,24.224690817093,24.2612649505334,24.3859464255039,
24.5054579125581,24.6248494232083,24.7441738324787,24.8634838994978,24.982915605997,
25.102419636098,25.2221421814788,25.2587167502974,25.3833982252679,25.5029097714894,
25.622301342095,25.7416258119897,25.8609359401839,25.9803677082202,26.0998718001396,
26.2195944071251,26.2561685500615,26.3758980412773,26.49541998721,26.5429554215432),
 .UNSPECIFIED.);
#579=B_SPLINE_CURVE_WITH_KNOTS('',3,(#42652,#42653,#42654,#42655,#42656,
#42657),.UNSPECIFIED.,.F.,.F.,(4,1,1,4),(20.2591548474271,20.2714577514771,
21.2689095512411,21.9911485751285),.UNSPECIFIED.);
#580=B_SPLINE_CURVE_WITH_KNOTS('',3,(#42658,#42659,#42660,#42661,#42662,
#42663,#42664,#42665,#42666,#42667,#42668,#42669,#42670,#42671,#42672,#42673,
#42674,#42675,#42676,#42677,#42678,#42679,#42680,#42681,#42682,#42683,#42684,
#42685,#42686,#42687,#42688,#42689,#42690,#42691,#42692,#42693,#42694,#42695,
#42696,#42697,#42698,#42699,#42700,#42701,#42702,#42703,#42704,#42705,#42706,
#42707,#42708,#42709,#42710,#42711,#42712,#42713,#42714,#42715,#42716,#42717,
#42718,#42719,#42720,#42721,#42722,#42723,#42724,#42725,#42726,#42727,#42728,
#42729,#42730,#42731,#42732,#42733,#42734,#42735,#42736,#42737,#42738,#42739,
#42740,#42741,#42742,#42743,#42744,#42745,#42746,#42747,#42748,#42749,#42750,
#42751,#42752,#42753,#42754,#42755,#42756,#42757,#42758,#42759,#42760,#42761,
#42762,#42763,#42764,#42765,#42766,#42767,#42768,#42769,#42770,#42771,#42772,
#42773,#42774,#42775,#42776,#42777,#42778,#42779,#42780,#42781,#42782,#42783,
#42784,#42785,#42786,#42787,#42788,#42789,#42790,#42791,#42792,#42793,#42794,
#42795,#42796,#42797,#42798,#42799,#42800,#42801,#42802,#42803,#42804,#42805,
#42806,#42807,#42808,#42809,#42810,#42811,#42812,#42813,#42814,#42815,#42816,
#42817,#42818,#42819,#42820,#42821,#42822,#42823,#42824,#42825,#42826,#42827,
#42828,#42829,#42830,#42831,#42832,#42833,#42834,#42835),.UNSPECIFIED.,
 .F.,.F.,(4,2,2,2,2,2,2,2,2,2,2,2,2,2,2,2,2,2,2,2,2,2,2,2,2,2,2,2,2,2,2,
2,2,2,2,2,2,2,2,2,2,2,2,2,2,2,2,2,2,2,2,2,2,2,2,2,2,2,2,2,2,2,2,2,2,2,2,
2,2,2,2,2,2,2,2,2,2,2,2,2,2,2,2,2,2,2,2,2,4),(-0.946967500878228,-0.922468381690924,
-0.9154497701354,-0.910623957938968,-0.908431352505289,-0.906728346015609,
-0.904587904538674,-0.900053005137895,-0.877656795984915,-0.863912309720635,
-0.854825984971083,-0.850861003386889,-0.847829553977103,-0.844475295835823,
-0.838783116619881,-0.814017640143533,-0.795421493232167,-0.791998583472935,
-0.790076333873346,-0.78835448338196,-0.785825473887368,-0.779220455523365,
-0.756333432072061,-0.742490702556759,-0.736452638884795,-0.732691638190658,
-0.72968033513473,-0.726202818948079,-0.719893697788476,-0.711793903380419,
-0.689064812622101,-0.676898828139983,-0.673877130821646,-0.672040096985284,
-0.670247592003958,-0.667436559693061,-0.657525906745013,-0.632781276830887,
-0.620497135619826,-0.616020208073954,-0.612938375214289,-0.609768497229987,
-0.604991286731526,-0.587983419408895,-0.566370404228104,-0.558453727339228,
-0.555757057426252,-0.55416241386504,-0.552346877506135,-0.54942650625239,
-0.538007567037238,-0.523231383622395,-0.503753954143981,-0.498796130489219,
-0.495590539120956,-0.492498210231896,-0.488135856670422,-0.476038041351705,
-0.452682391769221,-0.441262258631334,-0.438270575162246,-0.436439791116939,
-0.434641737719111,-0.431804121868399,-0.421558482683881,-0.394402140799076,
-0.384280571523664,-0.38006974107086,-0.377002865800729,-0.373750673545418,
-0.368561547521138,-0.362325469483097,-0.348724021782114,-0.326744854498311,
-0.322227696775696,-0.32005298073731,-0.318319520768126,-0.316422919866036,
-0.313122529392659,-0.294157839183677,-0.269596750480482,-0.263891141771936,
-0.260534051336492,-0.257503056534744,-0.253543047323409,-0.244490680461125,
-0.230827395743105,-0.20867538173197,-0.204951810495098),.UNSPECIFIED.);
#581=B_SPLINE_CURVE_WITH_KNOTS('',3,(#42841,#42842,#42843,#42844,#42845,
#42846,#42847,#42848,#42849,#42850,#42851,#42852,#42853,#42854,#42855,#42856,
#42857,#42858,#42859,#42860,#42861,#42862,#42863,#42864,#42865,#42866,#42867,
#42868,#42869,#42870,#42871,#42872,#42873,#42874,#42875,#42876,#42877,#42878,
#42879,#42880,#42881,#42882,#42883,#42884,#42885,#42886,#42887,#42888,#42889,
#42890,#42891,#42892,#42893,#42894,#42895,#42896,#42897,#42898,#42899,#42900,
#42901,#42902,#42903,#42904,#42905,#42906,#42907,#42908,#42909,#42910,#42911,
#42912,#42913,#42914,#42915,#42916,#42917,#42918,#42919,#42920,#42921,#42922,
#42923,#42924,#42925,#42926,#42927,#42928,#42929,#42930,#42931,#42932,#42933,
#42934,#42935,#42936,#42937,#42938,#42939,#42940,#42941,#42942,#42943,#42944,
#42945,#42946,#42947,#42948,#42949,#42950,#42951,#42952,#42953,#42954,#42955,
#42956,#42957,#42958,#42959,#42960,#42961,#42962,#42963,#42964,#42965,#42966,
#42967,#42968,#42969,#42970,#42971,#42972,#42973,#42974,#42975,#42976),
 .UNSPECIFIED.,.F.,.F.,(4,2,2,2,2,2,2,2,2,2,2,2,2,2,2,2,2,2,2,2,2,2,2,2,
2,2,2,2,2,2,2,2,2,2,2,2,2,2,2,2,2,2,2,2,2,2,2,2,2,2,2,2,2,2,2,2,2,2,2,2,
2,2,2,2,2,2,2,4),(-0.537798266923256,-0.537506177459864,-0.531828068379447,
-0.528476355256648,-0.525443664043516,-0.521471867161082,-0.512343872931895,
-0.49849892361335,-0.47582306554166,-0.47155583492274,-0.469464843665186,
-0.467930616541699,-0.465780794147544,-0.461194588604739,-0.454660833371519,
-0.431721753353976,-0.417784759497364,-0.413092174304632,-0.410253500056579,
-0.407171279366293,-0.402868930199637,-0.391294205042398,-0.370114387362929,
-0.356068269150041,-0.352971699200996,-0.351118368510108,-0.34933777418127,
-0.346585987814439,-0.33736871064637,-0.316618981244855,-0.300306726738104,
-0.295478867603218,-0.292298808074558,-0.289188091770254,-0.284724252264618,
-0.271670552930376,-0.242972075436281,-0.236923170882173,-0.234478471263787,
-0.232752178756607,-0.230783658570783,-0.227139109909182,-0.222361304504011,
-0.210140098101275,-0.183923339213203,-0.178379309571443,-0.175054630686975,
-0.172014250956594,-0.167984732748016,-0.158473319658752,-0.14367931676018,
-0.12143378486745,-0.117854328944166,-0.115878250468057,-0.114154047461705,
-0.111724251984774,-0.105370515420435,-0.0948209917293399,-0.0672337401268089,
-0.0611511488656624,-0.0576837640980859,-0.0546703587498685,-0.0508923214782159,
-0.0429597972058361,-0.0317796072960284,-0.00405094180321479,-0.00172829229899956,
-0.000347817018397109),.UNSPECIFIED.);
#582=B_SPLINE_CURVE_WITH_KNOTS('',3,(#42977,#42978,#42979,#42980,#42981,
#42982,#42983,#42984,#42985,#42986,#42987,#42988,#42989,#42990,#42991,#42992,
#42993,#42994,#42995,#42996,#42997,#42998,#42999,#43000,#43001,#43002,#43003,
#43004,#43005,#43006,#43007,#43008,#43009,#43010,#43011,#43012,#43013,#43014,
#43015,#43016,#43017,#43018,#43019,#43020,#43021,#43022,#43023,#43024,#43025),
 .UNSPECIFIED.,.F.,.F.,(4,3,3,3,3,3,3,3,3,3,3,3,3,3,3,3,4),(26.5429554215432,
26.662316983425,26.7816302714825,26.9010405400129,27.0204926839711,27.1401882500657,
27.2536203498256,27.3783018247961,27.4978133478951,27.6172048951266,27.7365293414421,
27.8558394458981,27.9752711901376,28.0947752581988,28.2144978414786,28.2510721495896,
28.2743338823081),.UNSPECIFIED.);
#583=B_SPLINE_CURVE_WITH_KNOTS('',3,(#43027,#43028,#43029,#43030,#43031,
#43032,#43033,#43034,#43035,#43036,#43037,#43038,#43039,#43040,#43041,#43042,
#43043,#43044,#43045,#43046,#43047,#43048,#43049,#43050,#43051,#43052,#43053,
#43054,#43055,#43056,#43057,#43058,#43059,#43060,#43061,#43062,#43063,#43064,
#43065,#43066,#43067,#43068,#43069,#43070,#43071,#43072,#43073,#43074,#43075,
#43076,#43077,#43078,#43079,#43080,#43081,#43082,#43083,#43084),
 .UNSPECIFIED.,.F.,.F.,(4,2,2,2,2,2,2,2,2,2,2,2,2,2,2,2,2,2,2,2,2,2,2,2,
2,2,2,2,4),(-0.204951810495098,-0.203866411973684,-0.201677215860401,-0.19997466997083,
-0.197832178585648,-0.193285796636486,-0.186830922190499,-0.164570720576338,
-0.149832570566503,-0.145128439035206,-0.14228798365646,-0.139207791737628,
-0.134915838393065,-0.123426758250936,-0.102575518544609,-0.0881021819418686,
-0.0849945881575372,-0.0831390340203034,-0.0813604380740051,-0.0786179340158351,
-0.0695181708168154,-0.0493400313179309,-0.0322943140846844,-0.0274741063806191,
-0.0242958061789282,-0.0211844177002832,-0.0180756740011476,-0.0114983792101034,
-0.000347679328245713),.UNSPECIFIED.);
#584=B_SPLINE_CURVE_WITH_KNOTS('',3,(#43085,#43086,#43087,#43088,#43089,
#43090,#43091,#43092,#43093,#43094,#43095,#43096,#43097,#43098,#43099,#43100,
#43101,#43102,#43103,#43104,#43105,#43106,#43107,#43108,#43109,#43110,#43111,
#43112,#43113,#43114,#43115,#43116,#43117,#43118,#43119,#43120,#43121,#43122,
#43123,#43124,#43125,#43126,#43127,#43128,#43129,#43130,#43131,#43132,#43133,
#43134,#43135,#43136,#43137,#43138,#43139,#43140,#43141,#43142,#43143,#43144,
#43145,#43146,#43147,#43148,#43149,#43150,#43151,#43152,#43153,#43154,#43155,
#43156,#43157,#43158,#43159,#43160,#43161,#43162,#43163,#43164,#43165,#43166,
#43167,#43168,#43169,#43170,#43171,#43172,#43173,#43174,#43175,#43176,#43177,
#43178,#43179,#43180,#43181,#43182,#43183,#43184,#43185,#43186,#43187,#43188,
#43189,#43190,#43191,#43192,#43193,#43194,#43195,#43196,#43197,#43198,#43199,
#43200,#43201,#43202,#43203,#43204,#43205,#43206,#43207,#43208,#43209,#43210,
#43211,#43212,#43213,#43214,#43215,#43216,#43217,#43218),.UNSPECIFIED.,
 .F.,.F.,(4,2,2,2,2,2,2,2,2,2,2,2,2,2,2,2,2,2,2,2,2,2,2,2,2,2,2,2,2,2,2,
2,2,2,2,2,2,2,2,2,2,2,2,2,2,2,2,2,2,2,2,2,2,2,2,2,2,2,2,2,2,2,2,2,2,2,4),
(-1.48424114304962,-1.45604830120501,-1.45378992240823,-1.45089582985086,
-1.4490862183476,-1.44748832179174,-1.44477148214394,-1.43666243918882,
-1.4152524700204,-1.40391645806674,-1.39590905713369,-1.39211920263731,
-1.38913352407874,-1.3856871257414,-1.37970053019196,-1.34959551788675,
-1.34054677256897,-1.33655821862586,-1.3333790029775,-1.33150834333437,
-1.32976132477736,-1.32708995194451,-1.31938996172512,-1.29979482818213,
-1.28074995764395,-1.27586985834611,-1.27268006380297,-1.26961349564257,
-1.26591420844108,-1.25665984176262,-1.2285012221601,-1.21813033006686,
-1.21528316827322,-1.21348325667859,-1.2116549800296,-1.20867453763984,
-1.19738117055466,-1.17393361909052,-1.16181821780584,-1.15745437878462,
-1.15436201404728,-1.15115724093523,-1.14620250992566,-1.1267277110755,
-1.10867429175684,-1.10003980983029,-1.0973431720958,-1.09557375209416,
-1.09370495614477,-1.09053485040334,-1.07281567825276,-1.05479576455955,
-1.04727433373738,-1.04130064784165,-1.03788967846321,-1.03486973065885,
-1.03100774115379,-1.02257121807353,-0.993940066231286,-0.986307563268444,
-0.981189491840714,-0.978947672249757,-0.977405866271079,-0.975387956099528,
-0.971611167607907,-0.952423986733965,-0.946896429152393),.UNSPECIFIED.);
#585=B_SPLINE_CURVE_WITH_KNOTS('',3,(#43223,#43224,#43225,#43226,#43227,
#43228,#43229,#43230,#43231,#43232,#43233,#43234,#43235,#43236,#43237,#43238,
#43239,#43240,#43241,#43242,#43243,#43244,#43245,#43246,#43247,#43248,#43249,
#43250,#43251,#43252,#43253,#43254,#43255,#43256,#43257,#43258,#43259,#43260,
#43261,#43262,#43263,#43264,#43265,#43266,#43267,#43268,#43269,#43270,#43271,
#43272,#43273,#43274,#43275,#43276,#43277,#43278,#43279,#43280,#43281,#43282,
#43283,#43284,#43285,#43286,#43287,#43288,#43289,#43290,#43291,#43292,#43293,
#43294,#43295,#43296,#43297,#43298,#43299,#43300,#43301,#43302,#43303,#43304,
#43305,#43306,#43307,#43308,#43309,#43310,#43311,#43312,#43313,#43314,#43315,
#43316,#43317,#43318,#43319,#43320,#43321,#43322,#43323,#43324,#43325,#43326,
#43327,#43328,#43329,#43330,#43331,#43332,#43333,#43334,#43335,#43336,#43337,
#43338,#43339,#43340,#43341,#43342,#43343,#43344,#43345,#43346,#43347,#43348,
#43349,#43350,#43351,#43352,#43353,#43354,#43355,#43356,#43357,#43358,#43359,
#43360,#43361,#43362,#43363,#43364,#43365,#43366,#43367,#43368,#43369,#43370,
#43371,#43372,#43373,#43374,#43375,#43376,#43377,#43378,#43379,#43380,#43381,
#43382,#43383,#43384,#43385,#43386,#43387,#43388,#43389,#43390,#43391,#43392,
#43393,#43394),.UNSPECIFIED.,.F.,.F.,(4,2,2,2,2,2,2,2,2,2,2,2,2,2,2,2,2,
2,2,2,2,2,2,2,2,2,2,2,2,2,2,2,2,2,2,2,2,2,2,2,2,2,2,2,2,2,2,2,2,2,2,2,2,
2,2,2,2,2,2,2,2,2,2,2,2,2,2,2,2,2,2,2,2,2,2,2,2,2,2,2,2,2,2,2,2,4),(-1.27966179244307,
-1.25432717498015,-1.24158842886276,-1.2371574925959,-1.2340531215572,-1.230865718625,
-1.22599879383902,-1.20863462638208,-1.18878268537098,-1.17974795108809,
-1.17701303955952,-1.17523602989445,-1.17337834488173,-1.17026057131706,
-1.15477728216396,-1.14126503865543,-1.13009250046016,-1.12216360894302,
-1.11838673713112,-1.11537396990238,-1.11190699758364,-1.10582434286145,
-1.07321315589925,-1.06228504618835,-1.05939720603118,-1.0575885328328,
-1.05576912087322,-1.05283101130116,-1.042165278365,-1.0181625283419,-1.00592840967352,
-1.00155107299411,-0.99845596497942,-0.995254117715596,-0.990315806241641,
-0.97096163951348,-0.956362066789855,-0.944624942034149,-0.941684404284013,
-0.939864510715884,-0.938272617597187,-0.935591697269273,-0.927813272939215,
-0.901041368883797,-0.888286906079143,-0.883854085520051,-0.880749188036927,
-0.877561907294845,-0.872696513530942,-0.855396477001483,-0.8354872592761,
-0.826440120405065,-0.823703904789483,-0.821926535121514,-0.820299941522499,
-0.817429748403217,-0.807925467898566,-0.782888236627016,-0.770446084880686,
-0.766046329086853,-0.762947409578457,-0.760128455756349,-0.755549687091231,
-0.742209132301279,-0.718619495801313,-0.708938212870643,-0.706072629149713,
-0.704446909773715,-0.70266865940466,-0.699928157616893,-0.690833355869004,
-0.670688859175166,-0.653687280382199,-0.648832169237673,-0.645646882679134,
-0.642540424940144,-0.638099238427744,-0.625266498095185,-0.598035051358098,
-0.590673835796256,-0.58804340024516,-0.586303653107998,-0.584418742815152,
-0.581174035884805,-0.562400442600069,-0.537798266923256),.UNSPECIFIED.);
#586=B_SPLINE_CURVE_WITH_KNOTS('',3,(#43395,#43396,#43397,#43398,#43399,
#43400,#43401,#43402,#43403,#43404,#43405,#43406,#43407,#43408,#43409,#43410,
#43411,#43412,#43413,#43414,#43415,#43416,#43417,#43418,#43419,#43420,#43421,
#43422,#43423,#43424,#43425,#43426,#43427,#43428,#43429,#43430,#43431,#43432,
#43433,#43434,#43435,#43436,#43437,#43438,#43439,#43440,#43441,#43442,#43443,
#43444,#43445,#43446,#43447,#43448,#43449,#43450,#43451,#43452,#43453,#43454,
#43455,#43456,#43457,#43458,#43459,#43460,#43461,#43462,#43463,#43464,#43465,
#43466,#43467,#43468,#43469,#43470,#43471,#43472,#43473,#43474,#43475,#43476,
#43477,#43478,#43479,#43480,#43481,#43482,#43483,#43484,#43485,#43486,#43487,
#43488,#43489,#43490,#43491,#43492,#43493,#43494,#43495,#43496,#43497,#43498,
#43499,#43500,#43501,#43502,#43503,#43504,#43505,#43506,#43507,#43508,#43509,
#43510,#43511,#43512,#43513,#43514,#43515,#43516,#43517,#43518,#43519,#43520,
#43521,#43522,#43523,#43524,#43525,#43526,#43527,#43528,#43529,#43530,#43531,
#43532,#43533,#43534,#43535,#43536,#43537,#43538,#43539,#43540,#43541,#43542,
#43543,#43544,#43545,#43546,#43547,#43548,#43549,#43550,#43551,#43552,#43553,
#43554,#43555,#43556,#43557,#43558,#43559,#43560,#43561,#43562,#43563,#43564,
#43565,#43566,#43567,#43568,#43569,#43570,#43571,#43572,#43573,#43574),
 .UNSPECIFIED.,.F.,.F.,(4,2,2,2,2,2,2,2,2,2,2,2,2,2,2,2,2,2,2,2,2,2,2,2,
2,2,2,2,2,2,2,2,2,2,2,2,2,2,2,2,2,2,2,2,2,2,2,2,2,2,2,2,2,2,2,2,2,2,2,2,
2,2,2,2,2,2,2,2,2,2,2,2,2,2,2,2,2,2,2,2,2,2,2,2,2,2,2,2,2,4),(-0.946896429152393,
-0.935842993036999,-0.925667135350627,-0.921543726905473,-0.918490479732483,
-0.915206420376403,-0.909860056159538,-0.878666036446273,-0.869470750707056,
-0.865441875260651,-0.862238073896102,-0.860361933680669,-0.858617532695414,
-0.855961512331845,-0.848392397106035,-0.821390886709287,-0.808596590695199,
-0.804159511298146,-0.801053857304842,-0.797867696746628,-0.793007940488407,
-0.775902769465838,-0.758062947926695,-0.747047635991104,-0.744153776794232,
-0.742343881263691,-0.740525987880981,-0.737594727649649,-0.726004914285177,
-0.711299885231577,-0.691912226532235,-0.686968316133644,-0.683765414514044,
-0.680671158006654,-0.676298327255101,-0.664107267223547,-0.640323824407185,
-0.629373892365169,-0.626419761938131,-0.624596948961982,-0.622791564500296,
-0.619919320312464,-0.609210400316061,-0.577821792500602,-0.570876153331307,
-0.567233633494638,-0.564227199620881,-0.560651367644482,-0.553835042197994,
-0.537625984015797,-0.516897578586285,-0.510574211193969,-0.508085876193291,
-0.506353295857856,-0.50440631757677,-0.500865282665242,-0.483657092636642,
-0.457470251759231,-0.451922636834185,-0.448597667376053,-0.445558219757716,
-0.441531780187535,-0.432038120329208,-0.417288952292675,-0.394954804695401,
-0.391383788395766,-0.389409766908238,-0.387685497361857,-0.385253175592056,
-0.378879091347329,-0.368276097846622,-0.340470326342199,-0.334552944295256,
-0.331120680243266,-0.328405549661733,-0.324729312773739,-0.317370994331972,
-0.288257050103309,-0.276071876122829,-0.273049223859322,-0.271211782379053,
-0.269419243667921,-0.266608375613737,-0.256700962337173,-0.231980086619663,
-0.219672029865783,-0.215192207549624,-0.212109813356784,-0.208940536423249,
-0.204814060717158),.UNSPECIFIED.);
#587=B_SPLINE_CURVE_WITH_KNOTS('',3,(#43580,#43581,#43582,#43583,#43584,
#43585,#43586,#43587,#43588,#43589,#43590,#43591,#43592,#43593,#43594,#43595,
#43596,#43597,#43598,#43599,#43600,#43601,#43602,#43603,#43604,#43605,#43606,
#43607,#43608,#43609,#43610,#43611,#43612,#43613,#43614,#43615,#43616,#43617,
#43618,#43619,#43620,#43621,#43622,#43623,#43624,#43625,#43626,#43627,#43628,
#43629,#43630,#43631,#43632,#43633,#43634,#43635,#43636,#43637,#43638,#43639,
#43640,#43641,#43642,#43643,#43644,#43645,#43646,#43647,#43648,#43649,#43650,
#43651,#43652,#43653,#43654,#43655,#43656,#43657,#43658,#43659,#43660,#43661,
#43662,#43663,#43664,#43665,#43666,#43667,#43668,#43669,#43670,#43671,#43672,
#43673,#43674,#43675,#43676,#43677,#43678,#43679,#43680,#43681,#43682,#43683,
#43684,#43685,#43686,#43687,#43688,#43689,#43690,#43691,#43692,#43693,#43694,
#43695,#43696,#43697,#43698,#43699,#43700,#43701,#43702,#43703,#43704,#43705,
#43706,#43707,#43708,#43709),.UNSPECIFIED.,.F.,.F.,(4,2,2,2,2,2,2,2,2,2,
2,2,2,2,2,2,2,2,2,2,2,2,2,2,2,2,2,2,2,2,2,2,2,2,2,2,2,2,2,2,2,2,2,2,2,2,
2,2,2,2,2,2,2,2,2,2,2,2,2,2,2,2,2,2,4),(-0.537776489716364,-0.534198513703777,
-0.52103880817225,-0.517975708792139,-0.516129398949848,-0.514343229570971,
-0.511564537665593,-0.502044724931717,-0.479685058663251,-0.4650862917619,
-0.46037386413174,-0.457531440826043,-0.454451372287482,-0.450163793312434,
-0.438716588464773,-0.418023263243845,-0.403348000688067,-0.400236089950503,
-0.398379310035032,-0.396600727053666,-0.393859877240925,-0.384765717702204,
-0.364629473374132,-0.347609664737636,-0.342753020577864,-0.339566955288556,
-0.336459904990986,-0.33201816515001,-0.319186530878157,-0.291973217950856,
-0.284587916690818,-0.281954092550411,-0.28021345836489,-0.278329107447126,
-0.27508823695252,-0.256411419357537,-0.231381764138882,-0.225713760365959,
-0.222363627386267,-0.219329715902291,-0.215352458514932,-0.20619229086423,
-0.192271411725321,-0.169374160836966,-0.165316050793369,-0.163264831626422,
-0.161555085887664,-0.159250430226323,-0.153746726175966,-0.145264839539994,
-0.119316067387194,-0.11021533613045,-0.10653845342432,-0.103476209136044,
-0.100276211392115,-0.0953498031450175,-0.0751294366217575,-0.0534188318608297,
-0.0482609969301123,-0.0461655263615747,-0.0444325672152798,-0.042484323128687,
-0.0389390292264036,-0.0146040278328785,-0.000347987605346437),
 .UNSPECIFIED.);
#588=B_SPLINE_CURVE_WITH_KNOTS('',3,(#43710,#43711,#43712,#43713,#43714,
#43715,#43716,#43717,#43718,#43719,#43720,#43721,#43722,#43723,#43724,#43725,
#43726,#43727,#43728,#43729,#43730,#43731,#43732,#43733,#43734,#43735,#43736,
#43737,#43738,#43739,#43740,#43741,#43742,#43743,#43744,#43745,#43746,#43747,
#43748,#43749,#43750,#43751,#43752,#43753,#43754,#43755,#43756,#43757,#43758,
#43759,#43760,#43761,#43762,#43763,#43764,#43765,#43766,#43767,#43768,#43769),
 .UNSPECIFIED.,.F.,.F.,(4,2,2,2,2,2,2,2,2,2,2,2,2,2,2,2,2,2,2,2,2,2,2,2,
2,2,2,2,2,4),(-1.4841886454229,-1.47940069237929,-1.47549041408193,-1.47244534473254,
-1.46959525256703,-1.46641335063947,-1.46157478749194,-1.44411610319639,
-1.42625695166726,-1.41554489031622,-1.41267248613528,-1.4108671759522,
-1.40904449329911,-1.40609063216606,-1.3951333211173,-1.37138855096943,
-1.35920971863448,-1.35483872415153,-1.35174491660862,-1.34854170222424,
-1.34359564740901,-1.3241801964729,-1.30944087487755,-1.29790114529091,
-1.29497302760088,-1.29315588500588,-1.29156242598973,-1.28887205891143,
-1.28100926508778,-1.27966179244307),.UNSPECIFIED.);
#589=B_SPLINE_CURVE_WITH_KNOTS('',3,(#43771,#43772,#43773,#43774,#43775,
#43776,#43777,#43778,#43779,#43780,#43781,#43782,#43783,#43784,#43785,#43786,
#43787,#43788,#43789,#43790,#43791,#43792,#43793,#43794,#43795,#43796,#43797,
#43798,#43799,#43800,#43801,#43802,#43803,#43804,#43805,#43806,#43807,#43808,
#43809,#43810,#43811,#43812,#43813,#43814,#43815,#43816,#43817,#43818,#43819,
#43820),.UNSPECIFIED.,.F.,.F.,(4,2,2,2,2,2,2,2,2,2,2,2,2,2,2,2,2,2,2,2,
2,2,2,2,4),(-0.204814060717158,-0.204166609680667,-0.187215917834386,-0.165816146214042,
-0.157668351142534,-0.154946746566997,-0.153347665623864,-0.15153847245285,
-0.14864814877196,-0.137682112602079,-0.108778642902585,-0.100318642772258,
-0.0964526102798113,-0.0934319757398673,-0.0900228099528017,-0.0840594167740254,
-0.0765548085537383,-0.0573560458344415,-0.0419804058744758,-0.0381441985147878,
-0.0361137299898091,-0.0344178346005035,-0.032094638147647,-0.0264692456979172,
-0.000347917537283366),.UNSPECIFIED.);
#590=B_SPLINE_CURVE_WITH_KNOTS('',3,(#43821,#43822,#43823,#43824,#43825,
#43826,#43827,#43828,#43829,#43830,#43831,#43832,#43833,#43834,#43835,#43836,
#43837,#43838,#43839,#43840,#43841,#43842,#43843,#43844,#43845,#43846,#43847,
#43848,#43849,#43850,#43851,#43852,#43853,#43854,#43855,#43856,#43857,#43858,
#43859,#43860,#43861,#43862,#43863,#43864,#43865,#43866,#43867,#43868,#43869,
#43870,#43871,#43872,#43873,#43874,#43875,#43876,#43877,#43878,#43879,#43880,
#43881,#43882,#43883,#43884,#43885,#43886,#43887,#43888,#43889,#43890,#43891,
#43892,#43893,#43894,#43895,#43896,#43897,#43898,#43899,#43900,#43901,#43902,
#43903,#43904,#43905,#43906,#43907,#43908,#43909,#43910,#43911,#43912,#43913,
#43914,#43915,#43916,#43917,#43918,#43919,#43920,#43921,#43922,#43923,#43924,
#43925,#43926,#43927,#43928,#43929,#43930,#43931,#43932,#43933,#43934,#43935,
#43936,#43937,#43938,#43939,#43940,#43941,#43942,#43943,#43944,#43945,#43946,
#43947,#43948,#43949,#43950),.UNSPECIFIED.,.F.,.F.,(4,2,2,2,2,2,2,2,2,2,
2,2,2,2,2,2,2,2,2,2,2,2,2,2,2,2,2,2,2,2,2,2,2,2,2,2,2,2,2,2,2,2,2,2,2,2,
2,2,2,2,2,2,2,2,2,2,2,2,2,2,2,2,2,2,4),(-1.48422776005814,-1.47313386088049,
-1.46656213293468,-1.46345549907946,-1.46034567045354,-1.45716791219661,
-1.45234645931115,-1.43524767424402,-1.41510713073786,-1.40601550622607,
-1.40327431232798,-1.40149641561978,-1.3996413756044,-1.39653435055193,
-1.38201921101944,-1.36123076358577,-1.34976145861204,-1.34547298846352,
-1.34239416073621,-1.33955416351908,-1.33484897705716,-1.32031076266756,
-1.29787871881556,-1.29140299357479,-1.28684684144652,-1.28470299019188,
-1.28316971808169,-1.28107519164268,-1.2767863312319,-1.25415083719961,
-1.24032371616758,-1.23120356317904,-1.22723401446115,-1.22420262816217,
-1.22085198138127,-1.21517493004383,-1.19025670760812,-1.17147896937039,
-1.16823757337857,-1.16635382954829,-1.16461454636331,-1.16198408125417,
-1.15461732365704,-1.12741318748726,-1.11458880234348,-1.11014964182435,
-1.10704436714992,-1.10386012497405,-1.09900638818332,-1.08203829039826,
-1.06184523177728,-1.05273989569101,-1.04999886908596,-1.04822094435502,
-1.04636572578455,-1.04325814328873,-1.0287220277255,-1.0079481971626,-0.996482490150635,
-0.992194304677656,-0.989115407141688,-0.986275159095789,-0.981569112867491,
-0.967492830556251,-0.946819715823378),.UNSPECIFIED.);
#591=B_SPLINE_CURVE_WITH_KNOTS('',3,(#43955,#43956,#43957,#43958,#43959,
#43960,#43961,#43962,#43963,#43964,#43965,#43966,#43967,#43968,#43969,#43970,
#43971,#43972,#43973,#43974,#43975,#43976,#43977,#43978,#43979,#43980,#43981,
#43982,#43983,#43984,#43985,#43986,#43987,#43988,#43989,#43990,#43991,#43992,
#43993,#43994,#43995,#43996,#43997,#43998,#43999,#44000,#44001,#44002,#44003,
#44004,#44005,#44006,#44007,#44008,#44009,#44010,#44011,#44012,#44013,#44014,
#44015,#44016,#44017,#44018,#44019,#44020,#44021,#44022,#44023,#44024,#44025,
#44026,#44027,#44028,#44029,#44030,#44031,#44032,#44033,#44034,#44035,#44036,
#44037,#44038,#44039,#44040,#44041,#44042,#44043,#44044,#44045,#44046,#44047,
#44048,#44049,#44050,#44051,#44052,#44053,#44054,#44055,#44056,#44057,#44058,
#44059,#44060,#44061,#44062,#44063,#44064,#44065,#44066,#44067,#44068,#44069,
#44070,#44071,#44072,#44073,#44074,#44075,#44076,#44077,#44078,#44079,#44080,
#44081,#44082,#44083,#44084,#44085,#44086,#44087,#44088,#44089,#44090,#44091,
#44092,#44093,#44094,#44095,#44096,#44097,#44098,#44099,#44100,#44101,#44102,
#44103,#44104,#44105,#44106,#44107,#44108,#44109,#44110,#44111,#44112,#44113,
#44114,#44115,#44116,#44117,#44118,#44119,#44120,#44121,#44122,#44123,#44124,
#44125,#44126,#44127,#44128,#44129,#44130,#44131,#44132,#44133,#44134),
 .UNSPECIFIED.,.F.,.F.,(4,2,2,2,2,2,2,2,2,2,2,2,2,2,2,2,2,2,2,2,2,2,2,2,
2,2,2,2,2,2,2,2,2,2,2,2,2,2,2,2,2,2,2,2,2,2,2,2,2,2,2,2,2,2,2,2,2,2,2,2,
2,2,2,2,2,2,2,2,2,2,2,2,2,2,2,2,2,2,2,2,2,2,2,2,2,2,2,2,2,4),(-1.27980850632928,
-1.27760533835833,-1.27202400355896,-1.24611093649757,-1.22869009499228,
-1.22513691135587,-1.22318718483132,-1.22145497831031,-1.21936252476966,
-1.21422187449833,-1.18980813348732,-1.17555817832044,-1.16884423297993,
-1.16528746138688,-1.16227985960788,-1.1586146109491,-1.15155555990615,
-1.12514953797021,-1.11488751227358,-1.10864533370155,-1.10623098369459,
-1.10450887174509,-1.10252454383414,-1.09890703173291,-1.07714016506507,
-1.0576408461584,-1.05100093532538,-1.04745835761557,-1.04445023580903,
-1.04076869989509,-1.03338403181038,-1.00725094959236,-0.997057566574456,
-0.990842310947649,-0.98843176089814,-0.986710165402452,-0.984723815926787,
-0.981096858518842,-0.959476954769453,-0.9443465784611,-0.934704038503723,
-0.930655288161407,-0.927612124994902,-0.924295706468068,-0.918793080749838,
-0.892200275205504,-0.88016266695316,-0.873264695418516,-0.870762543215849,
-0.869027460866021,-0.867085875578691,-0.863572197940217,-0.840357004955942,
-0.826083239451038,-0.816778620106407,-0.81277975525902,-0.80974325775482,
-0.806403958164091,-0.800788746354681,-0.775187405426704,-0.757119737238613,
-0.75379055254264,-0.75188756155927,-0.750156351888907,-0.747992531102661,
-0.742373700943728,-0.733308050256024,-0.703048005436398,-0.697171720781083,
-0.69374756147312,-0.691030517810713,-0.687340693368818,-0.679910401741977,
-0.669740234184557,-0.65590759122521,-0.640288952476128,-0.636439345855426,
-0.634405829272063,-0.632709976205251,-0.630390158255074,-0.62478842292603,
-0.616081811044127,-0.588534007849584,-0.580572312185066,-0.576789239067628,
-0.573775365067762,-0.570311301098227,-0.564074295972497,-0.556100784075032,
-0.537776489716364),.UNSPECIFIED.);
#592=B_SPLINE_CURVE_WITH_KNOTS('',3,(#44135,#44136,#44137,#44138,#44139,
#44140,#44141,#44142,#44143,#44144,#44145,#44146,#44147,#44148,#44149,#44150,
#44151,#44152,#44153,#44154,#44155,#44156,#44157,#44158,#44159,#44160,#44161,
#44162,#44163,#44164,#44165,#44166,#44167,#44168,#44169,#44170,#44171,#44172,
#44173,#44174,#44175,#44176,#44177,#44178,#44179,#44180,#44181,#44182,#44183,
#44184,#44185,#44186,#44187,#44188,#44189,#44190,#44191,#44192,#44193,#44194,
#44195,#44196,#44197,#44198,#44199,#44200,#44201,#44202,#44203,#44204,#44205,
#44206,#44207,#44208,#44209,#44210,#44211,#44212,#44213,#44214,#44215,#44216,
#44217,#44218,#44219,#44220,#44221,#44222,#44223,#44224,#44225,#44226,#44227,
#44228,#44229,#44230,#44231,#44232,#44233,#44234,#44235,#44236,#44237,#44238,
#44239,#44240,#44241,#44242,#44243,#44244,#44245,#44246,#44247,#44248,#44249,
#44250,#44251,#44252,#44253,#44254,#44255,#44256,#44257,#44258,#44259,#44260,
#44261,#44262,#44263,#44264,#44265,#44266,#44267,#44268,#44269,#44270,#44271,
#44272,#44273,#44274,#44275,#44276,#44277,#44278,#44279,#44280,#44281,#44282,
#44283,#44284,#44285,#44286,#44287,#44288,#44289,#44290,#44291,#44292,#44293,
#44294,#44295,#44296,#44297,#44298,#44299,#44300,#44301,#44302,#44303,#44304,
#44305,#44306,#44307,#44308,#44309,#44310,#44311,#44312,#44313,#44314,#44315,
#44316,#44317,#44318,#44319,#44320,#44321,#44322),.UNSPECIFIED.,.F.,.F.,
(4,2,2,2,2,2,2,2,2,2,2,2,2,2,2,2,2,2,2,2,2,2,2,2,2,2,2,2,2,2,2,2,2,2,2,
2,2,2,2,2,2,2,2,2,2,2,2,2,2,2,2,2,2,2,2,2,2,2,2,2,2,2,2,2,2,2,2,2,2,2,2,
2,2,2,2,2,2,2,2,2,2,2,2,2,2,2,2,2,2,2,2,2,2,4),(-0.946819715823378,-0.944676539999871,
-0.935076828038626,-0.932292076290245,-0.930505316705579,-0.928889090752232,
-0.926071942353666,-0.916881483189701,-0.891504469725059,-0.878998296090072,
-0.874592534986822,-0.871493295580457,-0.868676647070157,-0.864107604048417,
-0.850872411149378,-0.827100572834544,-0.817341449412502,-0.814543299147451,
-0.81275380795323,-0.810913986593012,-0.807878394495823,-0.795293230791608,
-0.772939415035423,-0.764898993792395,-0.758623664436144,-0.755153180680186,
-0.752141708206595,-0.748372244106774,-0.742302342198529,-0.727623535650372,
-0.701102900562991,-0.697522563918068,-0.695546785226429,-0.693823469602608,
-0.691395878611511,-0.685053685381215,-0.674532593703952,-0.647063413207413,
-0.640893185733333,-0.637408414405273,-0.634398072474785,-0.630647714502164,
-0.622869592828021,-0.612004485384715,-0.599054768639518,-0.583764540586666,
-0.579933276122199,-0.577904173494799,-0.576208601054083,-0.573884764731901,
-0.56825267410162,-0.559474394781421,-0.531398598766086,-0.523864120927975,
-0.520156844101676,-0.517149029385311,-0.513631118177445,-0.507113610239251,
-0.49864538529204,-0.473157169991846,-0.464060753103059,-0.46125124283949,
-0.459636384436826,-0.45784789805943,-0.45505513997049,-0.445360404148334,
-0.421972869851715,-0.408371971523109,-0.403771542685049,-0.400949395119775,
-0.397854853428461,-0.393476856731378,-0.381231570422997,-0.357183016218841,
-0.346545791215524,-0.34360951195502,-0.341790832733748,-0.339982494335379,
-0.337094783929389,-0.326158788437954,-0.294858651238629,-0.28802652325261,
-0.284407072230248,-0.281401714403851,-0.27780583378705,-0.270880043155716,
-0.238549072877998,-0.22863218022941,-0.225743671118562,-0.224113771967344,
-0.222340105173282,-0.219621574969192,-0.210758836892982,-0.204933271960559),
 .UNSPECIFIED.);
#593=B_SPLINE_CURVE_WITH_KNOTS('',3,(#44328,#44329,#44330,#44331,#44332,
#44333,#44334,#44335),.UNSPECIFIED.,.F.,.F.,(4,1,1,1,1,4),(53.4070764126742,
54.1848189434555,55.1822707432196,56.1797225429836,57.1771743427477,57.9574404719481),
 .UNSPECIFIED.);
#594=B_SPLINE_CURVE_WITH_KNOTS('',3,(#44336,#44337,#44338,#44339,#44340,
#44341,#44342,#44343,#44344,#44345,#44346,#44347,#44348,#44349,#44350,#44351,
#44352,#44353,#44354,#44355,#44356,#44357,#44358,#44359,#44360,#44361,#44362,
#44363,#44364,#44365,#44366,#44367,#44368,#44369,#44370,#44371,#44372,#44373,
#44374,#44375,#44376,#44377,#44378,#44379,#44380,#44381,#44382,#44383,#44384,
#44385,#44386,#44387,#44388,#44389),.UNSPECIFIED.,.F.,.F.,(4,2,2,2,2,2,
2,2,2,2,2,2,2,2,2,2,2,2,2,2,2,2,2,2,2,2,4),(-1.48420160976377,-1.46442302160507,
-1.46177965705685,-1.45945977695506,-1.45776409714973,-1.45573100399282,
-1.45188281404087,-1.43516050495058,-1.4169622897526,-1.40625631497045,
-1.40205626670841,-1.39899079202854,-1.39573420029934,-1.39052476860652,
-1.36183780261404,-1.35084074448908,-1.34431803830977,-1.34186519269882,
-1.34013776811861,-1.33817340543135,-1.33464796804164,-1.31190142067794,
-1.29738895903596,-1.28798870265809,-1.28397574080648,-1.28093759263062,
-1.27980850632928),.UNSPECIFIED.);
#595=B_SPLINE_CURVE_WITH_KNOTS('',3,(#44391,#44392,#44393,#44394,#44395,
#44396,#44397,#44398,#44399,#44400,#44401,#44402,#44403,#44404,#44405,#44406,
#44407,#44408,#44409,#44410,#44411,#44412,#44413,#44414,#44415,#44416,#44417,
#44418,#44419,#44420,#44421,#44422,#44423,#44424,#44425,#44426,#44427,#44428,
#44429,#44430,#44431,#44432,#44433,#44434,#44435,#44436),.UNSPECIFIED.,
 .F.,.F.,(4,2,2,2,2,2,2,2,2,2,2,2,2,2,2,2,2,2,2,2,2,2,4),(-0.204933271960559,
-0.193610744071927,-0.173609752213875,-0.168619346997917,-0.165407512488029,
-0.162319690211239,-0.157981592593195,-0.146094999274754,-0.123657667876321,
-0.111154201353178,-0.108114289236958,-0.106273326207953,-0.104484102155178,
-0.101688499279261,-0.091962803369415,-0.0683916817828056,-0.0549692722591983,
-0.0503840172232408,-0.0475641962116398,-0.0444667589965546,-0.0400740093147337,
-0.0276969669859353,-0.000348048528551123),.UNSPECIFIED.);
#596=B_SPLINE_CURVE_WITH_KNOTS('',3,(#44437,#44438,#44439,#44440,#44441,
#44442,#44443,#44444,#44445,#44446,#44447,#44448,#44449,#44450,#44451,#44452,
#44453,#44454,#44455,#44456,#44457,#44458,#44459,#44460,#44461,#44462,#44463,
#44464,#44465,#44466,#44467,#44468,#44469,#44470,#44471,#44472,#44473,#44474,
#44475,#44476,#44477,#44478,#44479,#44480,#44481,#44482,#44483,#44484,#44485,
#44486,#44487,#44488,#44489,#44490,#44491,#44492,#44493,#44494,#44495,#44496,
#44497,#44498,#44499,#44500,#44501,#44502,#44503,#44504,#44505,#44506,#44507,
#44508,#44509,#44510,#44511,#44512,#44513,#44514,#44515,#44516,#44517,#44518,
#44519,#44520,#44521,#44522,#44523,#44524,#44525,#44526,#44527,#44528,#44529,
#44530,#44531,#44532,#44533,#44534,#44535,#44536,#44537,#44538,#44539,#44540,
#44541,#44542,#44543,#44544,#44545,#44546,#44547,#44548,#44549,#44550,#44551,
#44552,#44553,#44554,#44555,#44556,#44557,#44558,#44559,#44560,#44561,#44562,
#44563,#44564,#44565,#44566,#44567,#44568,#44569,#44570),.UNSPECIFIED.,
 .F.,.F.,(4,2,2,2,2,2,2,2,2,2,2,2,2,2,2,2,2,2,2,2,2,2,2,2,2,2,2,2,2,2,2,
2,2,2,2,2,2,2,2,2,2,2,2,2,2,2,2,2,2,2,2,2,2,2,2,2,2,2,2,2,2,2,2,2,2,2,4),
(-1.48430166607142,-1.47889192298633,-1.47529624805926,-1.4735682429476,
-1.47191690410003,-1.46995830580524,-1.4664577751231,-1.45041785091773,
-1.43284714499154,-1.42065567768791,-1.41628357434739,-1.41318989829041,
-1.40998764063816,-1.40504485665597,-1.38564972040756,-1.3709383577164,
-1.35934261495105,-1.35641116887526,-1.35459347556701,-1.35300080675906,
-1.35031405421988,-1.34248172221607,-1.31576207622309,-1.3030162681603,
-1.29858488322316,-1.29548075354232,-1.29229410238292,-1.28742943295573,
-1.27013735491797,-1.24455416434874,-1.23982938758071,-1.23765512330591,
-1.23595297366096,-1.23379673766841,-1.22917327113744,-1.20686195338864,
-1.19314628642084,-1.18407187511922,-1.18010879638047,-1.17707767033437,
-1.17372264365296,-1.1680262731,-1.14332349154197,-1.12468305174694,-1.12125810824455,
-1.1193353868194,-1.11761352652868,-1.11508512112894,-1.10848631069315,
-1.08800488269144,-1.07495625118098,-1.06616600206954,-1.0622469985798,
-1.05922083654373,-1.05584218653558,-1.05002996954381,-1.02995476766433,
-1.01362235263153,-1.00802780286182,-1.00393075188198,-1.00187240562504,
-1.00016424924206,-0.99791134675134,-0.992793649928703,-0.962952904346267,
-0.949751005501392,-0.946940986422606),.UNSPECIFIED.);
#597=B_SPLINE_CURVE_WITH_KNOTS('',3,(#44576,#44577,#44578,#44579,#44580,
#44581,#44582,#44583,#44584,#44585,#44586,#44587,#44588,#44589,#44590,#44591,
#44592,#44593,#44594,#44595,#44596,#44597,#44598,#44599,#44600,#44601,#44602,
#44603,#44604,#44605,#44606,#44607,#44608,#44609,#44610,#44611,#44612,#44613,
#44614,#44615,#44616,#44617,#44618,#44619,#44620,#44621,#44622,#44623,#44624,
#44625,#44626,#44627,#44628,#44629,#44630,#44631,#44632,#44633,#44634,#44635,
#44636,#44637,#44638,#44639,#44640,#44641,#44642,#44643,#44644,#44645,#44646,
#44647,#44648,#44649,#44650,#44651,#44652,#44653,#44654,#44655,#44656,#44657,
#44658,#44659,#44660,#44661,#44662,#44663,#44664,#44665,#44666,#44667,#44668,
#44669,#44670,#44671,#44672,#44673,#44674,#44675,#44676,#44677,#44678,#44679,
#44680,#44681,#44682,#44683,#44684,#44685,#44686,#44687,#44688,#44689,#44690,
#44691,#44692,#44693,#44694,#44695,#44696,#44697,#44698,#44699,#44700,#44701,
#44702,#44703,#44704,#44705,#44706,#44707),.UNSPECIFIED.,.F.,.F.,(4,2,2,
2,2,2,2,2,2,2,2,2,2,2,2,2,2,2,2,2,2,2,2,2,2,2,2,2,2,2,2,2,2,2,2,2,2,2,2,
2,2,2,2,2,2,2,2,2,2,2,2,2,2,2,2,2,2,2,2,2,2,2,2,2,2,4),(-0.537894309400619,
-0.533213023061253,-0.530146767499444,-0.528299718798876,-0.526513942106161,
-0.523737506313799,-0.514245033064368,-0.492040195169155,-0.477283299942744,
-0.472556031510676,-0.469710903305401,-0.4666325925218,-0.462356285683449,
-0.451003884271354,-0.430660626675176,-0.41552074734285,-0.412403153331535,
-0.410545094255675,-0.408767235546628,-0.406030368929641,-0.396980563888222,
-0.377059427124444,-0.359785895119985,-0.354920900350778,-0.351733055542335,
-0.348626984053177,-0.344191413696158,-0.331421255928584,-0.304586585746469,
-0.296839343142064,-0.29416142786641,-0.292569704049276,-0.290748153301413,
-0.287801726779752,-0.275975268433924,-0.261471724955338,-0.242132862770731,
-0.23719417371081,-0.233991537569654,-0.230895255952026,-0.226515573942646,
-0.214270844514413,-0.190238637442558,-0.179571531704665,-0.176632253726846,
-0.174812200456691,-0.173002919717492,-0.1701142396868,-0.159181724509775,
-0.127151370184006,-0.121302249952503,-0.117592966019391,-0.11458328867609,
-0.111062890349529,-0.104539639292293,-0.0875154561512914,-0.066232950840203,
-0.0605865857542987,-0.0584200588427744,-0.0566881374008508,-0.0547862963146238,
-0.051463008905974,-0.0335559941265448,-0.00733093514828557,-0.0031099699046096,
-0.00036640004475231),.UNSPECIFIED.);
#598=B_SPLINE_CURVE_WITH_KNOTS('',3,(#44708,#44709,#44710,#44711,#44712,
#44713),.UNSPECIFIED.,.F.,.F.,(4,1,1,4),(57.9574404719481,58.1746261425118,
59.1720779422758,59.690260418206),.UNSPECIFIED.);
#599=B_SPLINE_CURVE_WITH_KNOTS('',3,(#44714,#44715,#44716,#44717,#44718,
#44719,#44720,#44721,#44722,#44723,#44724,#44725,#44726,#44727,#44728,#44729,
#44730,#44731,#44732,#44733,#44734,#44735,#44736,#44737,#44738,#44739,#44740,
#44741,#44742,#44743,#44744,#44745,#44746,#44747,#44748,#44749,#44750,#44751,
#44752,#44753,#44754,#44755,#44756,#44757,#44758,#44759,#44760,#44761,#44762,
#44763,#44764,#44765,#44766,#44767,#44768,#44769,#44770,#44771,#44772,#44773,
#44774,#44775,#44776,#44777,#44778,#44779,#44780,#44781,#44782,#44783,#44784,
#44785,#44786,#44787,#44788,#44789,#44790,#44791,#44792,#44793,#44794,#44795,
#44796,#44797,#44798,#44799,#44800,#44801,#44802,#44803,#44804,#44805,#44806,
#44807,#44808,#44809,#44810,#44811,#44812,#44813,#44814,#44815,#44816,#44817,
#44818,#44819,#44820,#44821,#44822,#44823,#44824,#44825,#44826,#44827,#44828,
#44829,#44830,#44831,#44832,#44833,#44834,#44835,#44836,#44837,#44838,#44839,
#44840,#44841,#44842,#44843,#44844,#44845,#44846,#44847,#44848,#44849,#44850,
#44851,#44852,#44853,#44854,#44855,#44856,#44857,#44858,#44859,#44860,#44861,
#44862,#44863,#44864,#44865,#44866,#44867,#44868,#44869,#44870,#44871,#44872,
#44873,#44874,#44875,#44876,#44877,#44878,#44879,#44880,#44881,#44882,#44883,
#44884,#44885,#44886,#44887,#44888,#44889,#44890,#44891,#44892,#44893,#44894,
#44895,#44896,#44897,#44898,#44899),.UNSPECIFIED.,.F.,.F.,(4,2,2,2,2,2,
2,2,2,2,2,2,2,2,2,2,2,2,2,2,2,2,2,2,2,2,2,2,2,2,2,2,2,2,2,2,2,2,2,2,2,2,
2,2,2,2,2,2,2,2,2,2,2,2,2,2,2,2,2,2,2,2,2,2,2,2,2,2,2,2,2,2,2,2,2,2,2,2,
2,2,2,2,2,2,2,2,2,2,2,2,2,2,4),(-0.946940986422606,-0.945273129429978,-0.942160311314846,
-0.938984453190988,-0.934175772564391,-0.918248594807293,-0.897127199870089,
-0.887835764106582,-0.885077458287909,-0.883295787308269,-0.881444785116189,
-0.878358208390088,-0.864596914267385,-0.843204236032207,-0.835314447087802,
-0.829125524487421,-0.825671593094014,-0.822657541866112,-0.818862318905677,
-0.810826146230518,-0.78335051547628,-0.774650674287677,-0.769052473036572,
-0.766733531961685,-0.765038182655621,-0.763005133583983,-0.759156303535479,
-0.742523950964127,-0.716361306456947,-0.71081108452574,-0.707485634065531,
-0.704446417435343,-0.70042128422846,-0.690936090814075,-0.676208217414093,
-0.653835422583673,-0.65026833950149,-0.648295193675655,-0.646570733017929,
-0.644136839121935,-0.637751084756656,-0.627117411670784,-0.599182957370083,
-0.593362861750196,-0.589951202174112,-0.586931213099849,-0.583069957631787,
-0.574638569714413,-0.562395052833682,-0.53613807859232,-0.532507612759943,
-0.530520765212932,-0.528799765121625,-0.526391624163697,-0.520191088440316,
-0.510035419802304,-0.484044541654161,-0.476546816441148,-0.472845431415462,
-0.469837085995646,-0.46631252417331,-0.459763982547263,-0.44175462194786,
-0.418645314570392,-0.414830573686059,-0.412804561520743,-0.411263783971376,
-0.409032986596193,-0.403981540457007,-0.396492341688873,-0.367777930730709,
-0.359248162891342,-0.355370748663632,-0.352348935800174,-0.348946461336781,
-0.343016513313748,-0.335568494788288,-0.316665470627747,-0.300913413829313,
-0.297055588947873,-0.295020588922136,-0.293325397822012,-0.291009091073461,
-0.285428307338621,-0.276769629828269,-0.249570163727085,-0.241320447274573,
-0.237489117061739,-0.234471782714412,-0.231041172390308,-0.224970569268392,
-0.217283494883199,-0.204898626771331),.UNSPECIFIED.);
#600=B_SPLINE_CURVE_WITH_KNOTS('',3,(#44904,#44905,#44906,#44907,#44908,
#44909,#44910,#44911,#44912,#44913,#44914,#44915,#44916,#44917,#44918,#44919,
#44920,#44921,#44922,#44923,#44924,#44925,#44926,#44927,#44928,#44929,#44930,
#44931,#44932,#44933,#44934,#44935,#44936,#44937,#44938,#44939,#44940,#44941,
#44942,#44943,#44944,#44945,#44946,#44947,#44948,#44949,#44950,#44951,#44952,
#44953,#44954,#44955,#44956,#44957,#44958,#44959,#44960,#44961,#44962,#44963,
#44964,#44965,#44966,#44967,#44968,#44969,#44970,#44971,#44972,#44973,#44974,
#44975,#44976,#44977,#44978,#44979,#44980,#44981,#44982,#44983,#44984,#44985,
#44986,#44987,#44988,#44989,#44990,#44991,#44992,#44993,#44994,#44995,#44996,
#44997,#44998,#44999,#45000,#45001,#45002,#45003,#45004,#45005,#45006,#45007,
#45008,#45009,#45010,#45011,#45012,#45013,#45014,#45015,#45016,#45017,#45018,
#45019,#45020,#45021,#45022,#45023,#45024,#45025,#45026,#45027,#45028,#45029,
#45030,#45031,#45032,#45033,#45034,#45035,#45036,#45037,#45038,#45039,#45040,
#45041,#45042,#45043,#45044,#45045,#45046,#45047,#45048,#45049,#45050,#45051,
#45052,#45053,#45054,#45055,#45056,#45057,#45058,#45059,#45060,#45061,#45062,
#45063,#45064,#45065,#45066,#45067,#45068,#45069,#45070,#45071,#45072,#45073,
#45074,#45075,#45076,#45077,#45078,#45079,#45080,#45081),.UNSPECIFIED.,
 .F.,.F.,(4,2,2,2,2,2,2,2,2,2,2,2,2,2,2,2,2,2,2,2,2,2,2,2,2,2,2,2,2,2,2,
2,2,2,2,2,2,2,2,2,2,2,2,2,2,2,2,2,2,2,2,2,2,2,2,2,2,2,2,2,2,2,2,2,2,2,2,
2,2,2,2,2,2,2,2,2,2,2,2,2,2,2,2,2,2,2,2,2,4),(-1.27993629200949,-1.25838528934253,
-1.24046364626388,-1.23714001774422,-1.23523842844544,-1.23350717076722,
-1.23134194145366,-1.22570290877557,-1.20443469292664,-1.19109793829111,
-1.18218348531449,-1.17824477603145,-1.17521611578875,-1.17184751934819,
-1.16608598933105,-1.13689143543466,-1.12691592614631,-1.12078703885223,
-1.11838894770219,-1.11666911667411,-1.11467618616052,-1.11101845011242,
-1.09003583687508,-1.07452246129919,-1.06780472055512,-1.06231488789013,
-1.05900103536451,-1.05595695983437,-1.05197226829816,-1.0431911546825,
-1.01685093444682,-1.00831211758722,-1.00278388854634,-1.00047540770876,
-0.998765398195904,-0.996716971036565,-0.992672705825595,-0.969777975801975,
-0.955862542643372,-0.946704510215881,-0.942727833543562,-0.939694163111128,
-0.93634408901286,-0.930675744374352,-0.905625657612196,-0.887022359456591,
-0.883738917736678,-0.881845619516375,-0.880109790718354,-0.877502229657632,
-0.870321639209526,-0.850312656505014,-0.831035632592875,-0.82614456984875,
-0.8229516795489,-0.819884988601071,-0.816189006419218,-0.806962714754732,
-0.779555801492472,-0.772049316339871,-0.766989871910192,-0.764757372632763,
-0.763216078827397,-0.761190190844976,-0.757377645968129,-0.742551582456069,
-0.713866195979949,-0.70865222442012,-0.705394378095877,-0.702328759868338,
-0.698130193527889,-0.687397720548324,-0.669151973577296,-0.652464714678316,
-0.648614527989473,-0.646580810570882,-0.644884865664761,-0.642565013702663,
-0.636963594497172,-0.628257948666415,-0.600719074393753,-0.59274849249036,
-0.588963763656592,-0.585949614305228,-0.582486369257423,-0.576254132829627,
-0.568289060658438,-0.546441838554268,-0.537894309400619),.UNSPECIFIED.);
#601=B_SPLINE_CURVE_WITH_KNOTS('',3,(#45083,#45084,#45085,#45086,#45087,
#45088,#45089,#45090,#45091,#45092,#45093,#45094,#45095,#45096,#45097,#45098,
#45099,#45100,#45101,#45102,#45103,#45104,#45105,#45106,#45107,#45108,#45109,
#45110,#45111,#45112,#45113,#45114,#45115,#45116,#45117,#45118,#45119,#45120,
#45121,#45122,#45123,#45124,#45125,#45126,#45127,#45128,#45129,#45130,#45131,
#45132,#45133,#45134,#45135,#45136),.UNSPECIFIED.,.F.,.F.,(4,2,2,2,2,2,
2,2,2,2,2,2,2,2,2,2,2,2,2,2,2,2,2,2,2,2,4),(-0.204898626771331,-0.198446153233599,
-0.183080360398766,-0.17924463951519,-0.177214273588691,-0.175518362895264,
-0.173195011964068,-0.16756861108729,-0.158804659985722,-0.130843744826638,
-0.123210654704607,-0.119485237308615,-0.116475728362113,-0.112970479982118,
-0.106521256637508,-0.0833930600211793,-0.065258886004377,-0.0614304673950918,
-0.0594016131898563,-0.05770542227049,-0.0553796452063263,-0.049737640895587,
-0.040937586280751,-0.0142283439117813,-0.00595310739962801,-0.00265801665500284,
-0.000347696305143031),.UNSPECIFIED.);
#602=B_SPLINE_CURVE_WITH_KNOTS('',3,(#45137,#45138,#45139,#45140,#45141,
#45142,#45143,#45144,#45145,#45146,#45147,#45148,#45149,#45150,#45151,#45152,
#45153,#45154,#45155,#45156,#45157,#45158,#45159,#45160,#45161,#45162,#45163,
#45164,#45165,#45166,#45167,#45168,#45169,#45170,#45171,#45172,#45173,#45174,
#45175,#45176,#45177,#45178,#45179,#45180,#45181,#45182,#45183,#45184,#45185,
#45186,#45187,#45188,#45189,#45190,#45191,#45192,#45193,#45194,#45195,#45196,
#45197,#45198,#45199,#45200,#45201,#45202,#45203,#45204,#45205,#45206,#45207,
#45208,#45209,#45210,#45211,#45212,#45213,#45214,#45215,#45216,#45217,#45218,
#45219,#45220,#45221,#45222,#45223,#45224,#45225,#45226,#45227,#45228,#45229,
#45230,#45231,#45232,#45233,#45234,#45235,#45236,#45237,#45238,#45239,#45240,
#45241,#45242,#45243,#45244,#45245,#45246,#45247,#45248,#45249,#45250,#45251,
#45252,#45253,#45254,#45255,#45256,#45257,#45258,#45259,#45260),
 .UNSPECIFIED.,.F.,.F.,(4,3,3,3,3,3,3,3,3,3,3,3,3,3,3,3,3,3,3,3,3,3,3,3,
3,3,3,3,3,3,3,3,3,3,3,3,3,3,3,3,3,4),(65.9734457253857,66.0990314776703,
66.2241716615538,66.3499801980389,66.4757887345241,66.6004702094946,66.719981694683,
66.8393732042342,66.95869761317,67.078007680618,67.1974393886703,67.3169434209799,
67.4366659695107,67.4732405342882,67.5979220092587,67.7174335580785,67.8368251306602,
67.9561496019118,68.0754597308459,68.1948914987132,68.3143955899358,68.4341181954617,
68.4706923340523,68.5953738090228,68.7148854589353,68.8342771334435,68.9536017072489,
69.0729119391582,69.1923438098461,69.3118480039161,69.4315707112718,69.4681441338164,
69.5928256087869,69.7123367977167,69.8317280117834,69.951052126569,70.070361901761,
70.18979332251,70.3092970700651,70.4290193404745,70.4655959335804,70.525019783164),
 .UNSPECIFIED.);
#603=B_SPLINE_CURVE_WITH_KNOTS('',3,(#45266,#45267,#45268,#45269,#45270,
#45271,#45272,#45273,#45274,#45275,#45276,#45277,#45278,#45279,#45280,#45281,
#45282,#45283,#45284,#45285,#45286,#45287,#45288,#45289,#45290,#45291,#45292,
#45293,#45294,#45295,#45296,#45297,#45298,#45299,#45300,#45301,#45302,#45303,
#45304,#45305,#45306,#45307,#45308,#45309,#45310,#45311,#45312,#45313,#45314,
#45315,#45316,#45317,#45318,#45319,#45320,#45321,#45322,#45323,#45324,#45325,
#45326,#45327,#45328,#45329,#45330,#45331,#45332,#45333,#45334,#45335,#45336,
#45337,#45338,#45339,#45340,#45341,#45342,#45343,#45344,#45345,#45346,#45347,
#45348,#45349,#45350,#45351,#45352,#45353,#45354,#45355,#45356,#45357,#45358,
#45359,#45360,#45361,#45362,#45363,#45364,#45365,#45366,#45367,#45368,#45369,
#45370,#45371,#45372,#45373,#45374,#45375,#45376,#45377,#45378,#45379,#45380,
#45381,#45382,#45383,#45384,#45385,#45386,#45387,#45388,#45389),
 .UNSPECIFIED.,.F.,.F.,(4,3,3,3,3,3,3,3,3,3,3,3,3,3,3,3,3,3,3,3,3,3,3,3,
3,3,3,3,3,3,3,3,3,3,3,3,3,3,3,3,3,4),(72.2566310330981,72.3746000738282,
72.4924200944505,72.6101467448915,72.7278354973385,72.8456247185995,72.9634700790888,
73.0815331296642,73.1364031389728,73.2610846139433,73.3806207054347,73.5000366324537,
73.6193852251617,73.7387191975766,73.858174224532,73.977701261838,74.0974461224598,
74.1338549387369,74.2585364137074,74.3780718711446,74.497487656099,74.616836592913,
74.7361713904628,74.8556279384821,74.9751569026416,75.0949042603196,75.131306738501,
75.2559882134715,75.3753544000741,75.4946006959659,75.6137802495987,75.7329460935138,
75.8522355715341,75.9715983635803,76.0911825638886,76.128758538265,76.2486946695722,
76.3684426008254,76.4880621388945,76.6076039822474,76.7271699042361,76.8075006878804),
 .UNSPECIFIED.);
#604=B_SPLINE_CURVE_WITH_KNOTS('',3,(#45390,#45391,#45392,#45393,#45394,
#45395,#45396,#45397,#45398,#45399,#45400,#45401,#45402,#45403,#45404,#45405,
#45406,#45407,#45408,#45409,#45410,#45411,#45412,#45413,#45414,#45415,#45416,
#45417,#45418,#45419,#45420,#45421,#45422,#45423,#45424,#45425,#45426,#45427,
#45428,#45429,#45430,#45431,#45432,#45433,#45434,#45435,#45436,#45437,#45438,
#45439,#45440,#45441,#45442,#45443,#45444,#45445,#45446,#45447),
 .UNSPECIFIED.,.F.,.F.,(4,2,2,2,2,2,2,2,2,2,2,2,2,2,2,2,2,2,2,2,2,2,2,2,
2,2,2,2,4),(-1.48433766817237,-1.47563063748376,-1.47332014712585,-1.47161845788704,
-1.46993229781918,-1.46790905738358,-1.46410793341904,-1.44500910995515,
-1.4287553840491,-1.41830408844958,-1.41414242371745,-1.4110823356441,-1.40781066287085,
-1.4025296177577,-1.37431356910048,-1.36311234463794,-1.35651410134926,
-1.35405056104863,-1.35232111084505,-1.35036111278482,-1.34685611593369,
-1.32392877667923,-1.30951371641234,-1.30015284979804,-1.29614588730459,
-1.29310863275993,-1.28977378438033,-1.28417923565751,-1.27993629200949),
 .UNSPECIFIED.);
#605=B_SPLINE_CURVE_WITH_KNOTS('',3,(#45449,#45450,#45451,#45452,#45453,
#45454,#45455,#45456,#45457,#45458,#45459,#45460,#45461,#45462,#45463,#45464,
#45465,#45466,#45467,#45468,#45469,#45470,#45471,#45472,#45473,#45474,#45475,
#45476,#45477,#45478,#45479,#45480,#45481,#45482,#45483,#45484,#45485,#45486,
#45487,#45488,#45489,#45490,#45491,#45492,#45493,#45494),.UNSPECIFIED.,
 .F.,.F.,(4,3,3,3,3,3,3,3,3,3,3,3,3,3,3,4),(70.525019783164,70.6446193576465,
70.7640700377342,70.8834247914381,71.0027364317802,71.1221489412945,71.2416079535534,
71.3613062955418,71.4630477333445,71.5810393630235,71.6988537785785,71.8165468469208,
71.9342244217906,72.05188624816,72.1696834755421,72.2566308475935),
 .UNSPECIFIED.);
#606=B_SPLINE_CURVE_WITH_KNOTS('',3,(#45495,#45496,#45497,#45498,#45499,
#45500,#45501,#45502,#45503),.UNSPECIFIED.,.F.,.F.,(4,1,1,1,1,1,4),(72.2566310325653,
72.4604995331086,73.4579513328726,74.4554031326367,75.4528549324008,76.4503067321649,
76.8085816652527),.UNSPECIFIED.);
#607=B_SPLINE_CURVE_WITH_KNOTS('',3,(#45509,#45510,#45511,#45512,#45513,
#45514,#45515,#45516,#45517,#45518,#45519,#45520,#45521,#45522,#45523,#45524,
#45525,#45526,#45527,#45528,#45529,#45530,#45531,#45532,#45533,#45534,#45535,
#45536,#45537,#45538,#45539,#45540,#45541,#45542,#45543,#45544,#45545,#45546,
#45547,#45548,#45549,#45550,#45551,#45552,#45553,#45554,#45555,#45556,#45557,
#45558,#45559,#45560,#45561,#45562,#45563,#45564,#45565,#45566),
 .UNSPECIFIED.,.F.,.F.,(4,3,3,3,3,3,3,3,3,3,3,3,3,3,3,3,3,3,3,4),(-4.09202352044871,
-3.98980719905628,-3.87618720905945,-3.76277252994605,-3.64947230427638,
-3.53624194244134,-3.42303695779458,-3.3097318571573,-3.19637810523371,
-3.08281265733122,-2.99235539929221,-2.87748405249459,-2.76546218494948,
-2.65354723694333,-2.54169248379193,-2.42461551907177,-2.31267073081522,
-2.20066051905403,-2.08847033816625,-2.07338462491128),.UNSPECIFIED.);
#608=B_SPLINE_CURVE_WITH_KNOTS('',3,(#45569,#45570,#45571,#45572,#45573),
 .UNSPECIFIED.,.F.,.F.,(4,1,4),(0.,0.997451799764071,1.12274180646108),
 .UNSPECIFIED.);
#609=B_SPLINE_CURVE_WITH_KNOTS('',3,(#45578,#45579,#45580,#45581,#45582,
#45583,#45584,#45585,#45586,#45587,#45588,#45589,#45590,#45591,#45592,#45593,
#45594,#45595,#45596,#45597,#45598,#45599,#45600,#45601,#45602,#45603,#45604,
#45605,#45606,#45607,#45608,#45609,#45610,#45611,#45612,#45613,#45614,#45615,
#45616,#45617,#45618,#45619,#45620,#45621,#45622,#45623,#45624,#45625,#45626,
#45627,#45628,#45629,#45630,#45631,#45632,#45633,#45634,#45635,#45636,#45637,
#45638,#45639,#45640,#45641,#45642,#45643,#45644,#45645,#45646,#45647,#45648,
#45649,#45650,#45651,#45652,#45653,#45654,#45655,#45656,#45657,#45658,#45659,
#45660,#45661,#45662,#45663,#45664,#45665,#45666,#45667,#45668,#45669,#45670,
#45671,#45672,#45673,#45674,#45675,#45676,#45677,#45678,#45679,#45680,#45681,
#45682,#45683,#45684,#45685,#45686,#45687,#45688,#45689,#45690,#45691,#45692,
#45693,#45694,#45695,#45696,#45697,#45698,#45699,#45700,#45701,#45702,#45703,
#45704,#45705,#45706,#45707,#45708,#45709,#45710,#45711,#45712,#45713,#45714,
#45715,#45716,#45717,#45718,#45719,#45720,#45721,#45722,#45723,#45724,#45725,
#45726,#45727,#45728,#45729,#45730,#45731,#45732,#45733,#45734,#45735,#45736,
#45737,#45738,#45739,#45740,#45741,#45742,#45743,#45744,#45745,#45746,#45747,
#45748,#45749),.UNSPECIFIED.,.F.,.F.,(4,3,3,3,3,3,3,3,3,3,3,3,3,3,3,3,3,
3,3,3,3,3,3,3,3,3,3,3,3,3,3,3,3,3,3,3,3,3,3,3,3,3,3,3,3,3,3,3,3,3,3,3,3,
3,3,3,3,4),(-10.3752083948442,-10.2503833026325,-10.1250731934845,-9.99915640520669,
-9.97451799764071,-9.86110404478188,-9.7478938926556,-9.63479711949915,
-9.5217687878178,-9.40876406182607,-9.29565488796158,-9.18249497057902,
-9.06911746887118,-8.97706619787663,-8.86365051339009,-8.7504385362878,
-8.63733988266257,-8.52430961893586,-8.41130291316752,-8.29819170237126,
-8.1850297132015,-8.07165010949183,-7.97961439811257,-7.866221606749,-7.75303258758301,
-7.6399569151839,-7.52694961616527,-7.41396581883048,-7.30087724665411,
-7.1877377834431,-7.07438023313187,-6.9821625983485,-6.86872768090052,-6.7554967577242,
-6.64237934606444,-6.52933054251218,-6.416305545515,-6.30317657085608,-6.18999708090129,
-6.07660062945385,-5.98471079858443,-5.87127727316595,-5.75804701760528,
-5.64492983239768,-5.53188081910232,-5.41885518058614,-5.30572490890431,
-5.19254375753916,-5.07914507247754,-4.98725899882036,-4.87535456408063,
-4.76370217495604,-4.65215993920821,-4.54068066613504,-4.42851637982691,
-4.31695888287723,-4.20449120188987,-4.09202352090251),.UNSPECIFIED.);
#610=B_SPLINE_CURVE_WITH_KNOTS('',3,(#45750,#45751,#45752,#45753,#45754,
#45755,#45756,#45757,#45758,#45759,#45760,#45761,#45762,#45763,#45764,#45765,
#45766,#45767,#45768,#45769,#45770,#45771,#45772,#45773,#45774,#45775,#45776,
#45777,#45778,#45779,#45780,#45781,#45782,#45783,#45784,#45785,#45786,#45787,
#45788,#45789,#45790,#45791,#45792,#45793,#45794,#45795,#45796,#45797,#45798,
#45799,#45800,#45801,#45802,#45803,#45804,#45805,#45806,#45807,#45808,#45809,
#45810,#45811,#45812,#45813,#45814,#45815,#45816,#45817,#45818,#45819,#45820,
#45821,#45822,#45823,#45824,#45825,#45826,#45827,#45828,#45829,#45830,#45831,
#45832,#45833,#45834,#45835,#45836,#45837,#45838,#45839,#45840,#45841,#45842,
#45843,#45844,#45845,#45846,#45847,#45848,#45849,#45850,#45851,#45852,#45853,
#45854,#45855,#45856,#45857,#45858,#45859,#45860,#45861,#45862,#45863,#45864,
#45865,#45866,#45867,#45868,#45869,#45870,#45871,#45872,#45873,#45874,#45875,
#45876,#45877,#45878,#45879,#45880,#45881,#45882,#45883,#45884,#45885,#45886,
#45887,#45888,#45889,#45890,#45891,#45892,#45893,#45894,#45895,#45896,#45897,
#45898,#45899,#45900,#45901,#45902,#45903,#45904,#45905,#45906,#45907,#45908,
#45909,#45910,#45911,#45912,#45913,#45914,#45915,#45916,#45917,#45918,#45919,
#45920,#45921),.UNSPECIFIED.,.F.,.F.,(4,3,3,3,3,3,3,3,3,3,3,3,3,3,3,3,3,
3,3,3,3,3,3,3,3,3,3,3,3,3,3,3,3,3,3,3,3,3,3,3,3,3,3,3,3,3,3,3,3,3,3,3,3,
3,3,3,3,4),(1.12274180646108,1.23349876035573,1.34411485397831,1.45463835255786,
1.56511733193191,1.67568120756514,1.78628277695729,1.89709830417144,1.99490359952814,
2.10843227033142,2.22175603103796,2.33496564339142,2.4481058330173,2.5612212229477,
2.67443827120793,2.78770468900851,2.90118502291775,2.99235539929221,3.10595521961689,
3.21935723981433,3.33264940080441,3.44587627945317,3.55908235530706,3.67239561566932,
3.78576145357676,3.89934529158946,3.98980719905628,4.10308827144724,4.21616283373811,
4.32912245662456,4.442012318588,4.55487749425247,4.66784654485166,4.78086579292607,
4.8941035087682,4.98725899882035,5.1006938369561,5.21392493052826,5.32704266355744,
5.44009193523297,5.55311754307617,5.66624733656245,5.77942776152503,5.89282532003093,
5.98471079858443,6.09814320678973,6.21137255611537,6.32448896567656,6.43753733727379,
6.55056247156036,6.66369246422572,6.77687346077531,6.89027220554026,6.98216259834849,
7.10604783685458,7.22955918790001,7.35249446618955,7.4059271132892),
 .UNSPECIFIED.);
#611=B_SPLINE_CURVE_WITH_KNOTS('',3,(#45926,#45927,#45928,#45929,#45930,
#45931,#45932,#45933,#45934,#45935),.UNSPECIFIED.,.F.,.F.,(4,1,1,1,1,1,
1,4),(-16.6583941348078,-15.9592287962251,-14.9617769964611,-13.964325196697,
-12.9668733969329,-11.9694215971689,-10.9719697974048,-10.3752088276283),
 .UNSPECIFIED.);
#612=B_SPLINE_CURVE_WITH_KNOTS('',3,(#45936,#45937,#45938,#45939,#45940,
#45941,#45942,#45943,#45944,#45945,#45946,#45947,#45948,#45949,#45950,#45951,
#45952,#45953,#45954,#45955,#45956,#45957,#45958,#45959,#45960,#45961,#45962,
#45963,#45964,#45965,#45966,#45967,#45968,#45969,#45970,#45971,#45972,#45973,
#45974,#45975,#45976,#45977,#45978,#45979,#45980,#45981,#45982,#45983,#45984,
#45985,#45986,#45987,#45988,#45989,#45990,#45991,#45992,#45993,#45994,#45995,
#45996,#45997,#45998,#45999,#46000,#46001,#46002,#46003,#46004,#46005,#46006,
#46007,#46008,#46009,#46010,#46011,#46012,#46013,#46014,#46015,#46016,#46017,
#46018,#46019,#46020,#46021,#46022,#46023,#46024,#46025,#46026,#46027,#46028,
#46029,#46030,#46031,#46032,#46033,#46034,#46035,#46036,#46037,#46038,#46039,
#46040,#46041,#46042,#46043,#46044,#46045,#46046,#46047,#46048,#46049,#46050,
#46051,#46052,#46053,#46054,#46055,#46056,#46057,#46058,#46059,#46060,#46061,
#46062,#46063,#46064,#46065,#46066,#46067,#46068,#46069,#46070,#46071,#46072,
#46073,#46074,#46075,#46076,#46077,#46078,#46079,#46080,#46081,#46082,#46083,
#46084,#46085,#46086,#46087,#46088,#46089,#46090,#46091,#46092,#46093,#46094,
#46095,#46096,#46097,#46098,#46099,#46100,#46101,#46102,#46103,#46104,#46105,
#46106,#46107),.UNSPECIFIED.,.F.,.F.,(4,3,3,3,3,3,3,3,3,3,3,3,3,3,3,3,3,
3,3,3,3,3,3,3,3,3,3,3,3,3,3,3,3,3,3,3,3,3,3,3,3,3,3,3,3,3,3,3,3,3,3,3,3,
3,3,3,3,4),(7.40592711364064,7.52121005042001,7.63668183552839,7.75224539306113,
7.86809182454605,7.97961439811257,8.09303015678759,8.20624218300847,8.31934087042466,
8.43237115264579,8.54537786162435,8.6584890519252,8.77165100746136,8.8850305562887,
8.97706619787664,9.09047984077282,9.20368979858075,9.31678644809962,9.42981472662471,
9.54281946982981,9.65592876979487,9.76908887367652,9.88246665916506,9.97451799764071,
10.0879271238153,10.2011324266134,10.3142243399969,10.4272478097423,10.5402476798992,
10.653352045565,10.7665071733445,10.8798799765599,10.9719697974048,11.0853819666047,
11.1985903765148,11.3116854339006,11.4247120789009,11.5377151499773,11.6508227308402,
11.7639810868815,11.8773570988817,11.9694215971689,12.0828332562848,12.1960411565483,
12.3091357049343,12.422161842498,12.5351644086174,12.6482714925108,12.7614293552009,
12.8748048862075,12.9668733969329,13.0792407947244,13.1914409444974,13.303520564868,
13.4155510689317,13.5275526454623,13.6396214903294,13.6891124208202),
 .UNSPECIFIED.);
#613=B_SPLINE_CURVE_WITH_KNOTS('',3,(#46112,#46113,#46114,#46115,#46116,
#46117,#46118,#46119,#46120,#46121,#46122,#46123,#46124,#46125,#46126,#46127,
#46128,#46129,#46130,#46131,#46132,#46133,#46134,#46135,#46136,#46137,#46138,
#46139,#46140,#46141,#46142,#46143,#46144,#46145,#46146,#46147,#46148,#46149,
#46150,#46151,#46152,#46153,#46154,#46155,#46156,#46157,#46158,#46159,#46160,
#46161,#46162,#46163,#46164,#46165,#46166,#46167,#46168,#46169,#46170,#46171,
#46172,#46173,#46174,#46175,#46176,#46177,#46178,#46179,#46180,#46181,#46182,
#46183,#46184,#46185,#46186,#46187,#46188,#46189,#46190,#46191,#46192,#46193,
#46194,#46195,#46196,#46197,#46198,#46199,#46200,#46201,#46202,#46203,#46204,
#46205,#46206,#46207,#46208,#46209,#46210,#46211,#46212,#46213,#46214,#46215,
#46216,#46217,#46218,#46219,#46220,#46221,#46222,#46223,#46224,#46225,#46226,
#46227,#46228,#46229,#46230,#46231,#46232,#46233,#46234,#46235,#46236,#46237,
#46238,#46239,#46240,#46241,#46242,#46243,#46244,#46245,#46246,#46247,#46248,
#46249,#46250,#46251,#46252,#46253,#46254,#46255,#46256,#46257,#46258,#46259,
#46260,#46261,#46262,#46263,#46264,#46265,#46266,#46267,#46268,#46269,#46270,
#46271,#46272,#46273,#46274,#46275,#46276,#46277,#46278,#46279,#46280,#46281,
#46282,#46283),.UNSPECIFIED.,.F.,.F.,(4,3,3,3,3,3,3,3,3,3,3,3,3,3,3,3,3,
3,3,3,3,3,3,3,3,3,3,3,3,3,3,3,3,3,3,3,3,3,3,3,3,3,3,3,3,3,3,3,3,3,3,3,3,
3,3,3,3,4),(-22.9415794419855,-22.8281641120224,-22.7149525583976,-22.6018543727819,
-22.4888246206922,-22.375818469337,-22.2627078130779,-22.1495464168245,
-22.0361672912024,-21.9439395948096,-21.8305281426948,-21.7173204588114,
-21.6042261323817,-21.4912002219535,-21.3781978877594,-21.265091041421,
-21.1519334197811,-21.0385581325795,-20.9464877950455,-20.8330763403247,
-20.7198686538157,-20.60677432475,-20.4937484116803,-20.3807460748438,-20.267639225883,
-20.1544816016273,-20.0411063118546,-19.9490359952814,-19.8356245481252,
-19.722416869167,-19.6093225476384,-19.4962966420793,-19.3832943127141,
-19.2701874711044,-19.1570298541452,-19.0436545714864,-18.9515841955173,
-18.8381727422958,-18.724965057378,-18.6118707299584,-18.4988448185861,
-18.385842483495,-18.2727356363388,-18.1595780139235,-18.0462027260256,
-17.9541323957533,-17.8407209262676,-17.7275132249132,-17.6144188809639,
-17.5013929529983,-17.3883906012796,-17.2752837375772,-17.1621260986338,
-17.0487507944498,-16.9566805959892,-16.81839297033,-16.6820945023375,-16.658394483377),
 .UNSPECIFIED.);
#614=B_SPLINE_CURVE_WITH_KNOTS('',3,(#46284,#46285,#46286,#46287,#46288,
#46289,#46290,#46291,#46292,#46293,#46294,#46295,#46296,#46297,#46298,#46299,
#46300,#46301,#46302,#46303,#46304,#46305,#46306,#46307,#46308,#46309,#46310,
#46311,#46312,#46313,#46314,#46315,#46316,#46317,#46318,#46319,#46320,#46321,
#46322,#46323,#46324,#46325,#46326,#46327,#46328,#46329,#46330,#46331,#46332,
#46333,#46334,#46335,#46336,#46337,#46338,#46339,#46340,#46341,#46342,#46343,
#46344,#46345,#46346,#46347,#46348,#46349,#46350,#46351,#46352,#46353,#46354,
#46355,#46356,#46357,#46358,#46359,#46360,#46361,#46362,#46363,#46364,#46365,
#46366,#46367,#46368,#46369,#46370,#46371,#46372,#46373,#46374,#46375,#46376,
#46377,#46378,#46379,#46380,#46381,#46382,#46383,#46384,#46385,#46386,#46387,
#46388,#46389,#46390,#46391,#46392,#46393,#46394,#46395,#46396,#46397,#46398,
#46399,#46400,#46401,#46402,#46403,#46404,#46405,#46406,#46407,#46408,#46409,
#46410,#46411,#46412,#46413,#46414,#46415,#46416,#46417,#46418,#46419,#46420,
#46421,#46422,#46423,#46424,#46425,#46426,#46427,#46428,#46429,#46430,#46431,
#46432,#46433,#46434,#46435,#46436,#46437,#46438,#46439,#46440,#46441,#46442,
#46443,#46444,#46445,#46446,#46447,#46448,#46449,#46450,#46451,#46452,#46453,
#46454,#46455),.UNSPECIFIED.,.F.,.F.,(4,3,3,3,3,3,3,3,3,3,3,3,3,3,3,3,3,
3,3,3,3,3,3,3,3,3,3,3,3,3,3,3,3,3,3,3,3,3,3,3,3,3,3,3,3,3,3,3,3,3,3,3,3,
3,3,3,3,4),(13.6891124212831,13.830426267103,13.964325196697,14.0777367610392,
14.1909445588691,14.304039000212,14.4170650263139,14.5300674767369,14.6431744392318,
14.7563321771748,14.869707579436,14.9617769964611,15.075188464516,15.1883961653478,
15.3014905093303,15.4145164378841,15.5275187907461,15.6406256564511,15.7537832978754,
15.8671586053055,15.9592287962251,16.0726402106002,16.1858478557609,16.2989421428955,
16.4119680135264,16.5249703074907,16.6380771132471,16.7512346940451,16.8646099404927,
16.9566805959892,17.0700920649716,17.1832997660237,17.2963941097936,17.4094200377023,
17.5224223894861,17.6355292534425,17.7486868927446,17.8620621974556,17.9541323957533,
18.067543848488,18.1807515330992,18.2938458603223,18.406871771608,18.5198741067224,
18.6329809540715,18.746138576774,18.8595138651107,18.9515841955174,19.064995643072,
19.1782033222769,19.2912976439594,19.40432354958,19.5173258789145,19.6304327203509,
19.7435903370575,19.8569656193363,19.9490359952814,19.9722977279999),
 .UNSPECIFIED.);
#615=B_SPLINE_CURVE_WITH_KNOTS('',3,(#46460,#46461,#46462,#46463,#46464,
#46465,#46466,#46467,#46468,#46469,#46470,#46471,#46472,#46473,#46474,#46475,
#46476,#46477,#46478,#46479,#46480,#46481,#46482,#46483,#46484,#46485,#46486,
#46487,#46488,#46489,#46490,#46491,#46492,#46493,#46494,#46495,#46496,#46497,
#46498,#46499,#46500,#46501,#46502,#46503,#46504,#46505,#46506,#46507,#46508,
#46509,#46510,#46511,#46512,#46513,#46514,#46515,#46516,#46517,#46518,#46519,
#46520,#46521,#46522,#46523,#46524,#46525,#46526,#46527,#46528,#46529,#46530,
#46531,#46532,#46533,#46534,#46535,#46536,#46537,#46538,#46539,#46540,#46541,
#46542,#46543,#46544,#46545,#46546,#46547,#46548,#46549,#46550,#46551,#46552,
#46553,#46554,#46555,#46556,#46557,#46558,#46559,#46560,#46561,#46562,#46563,
#46564,#46565,#46566,#46567,#46568,#46569,#46570,#46571,#46572,#46573,#46574,
#46575,#46576,#46577,#46578,#46579,#46580,#46581,#46582,#46583,#46584,#46585,
#46586,#46587,#46588,#46589,#46590,#46591,#46592,#46593,#46594,#46595,#46596,
#46597,#46598,#46599,#46600,#46601,#46602,#46603,#46604,#46605,#46606,#46607,
#46608,#46609,#46610,#46611,#46612,#46613,#46614,#46615,#46616,#46617,#46618,
#46619,#46620,#46621,#46622,#46623,#46624,#46625,#46626,#46627,#46628,#46629,
#46630,#46631),.UNSPECIFIED.,.F.,.F.,(4,3,3,3,3,3,3,3,3,3,3,3,3,3,3,3,3,
3,3,3,3,3,3,3,3,3,3,3,3,3,3,3,3,3,3,3,3,3,3,3,3,3,3,3,3,3,3,3,3,3,3,3,3,
3,3,3,3,4),(-29.2247643991025,-29.0886098418601,-28.9504612883211,-28.9261021931581,
-28.8126907409659,-28.6994830569944,-28.5863887304699,-28.4733628199404,
-28.360360485639,-28.2472536391849,-28.1340960174244,-28.0207207300958,
-27.928650393394,-27.815238941203,-27.7020312572328,-27.5889369307099,-27.4759110201822,
-27.3629086858827,-27.2498018394306,-27.1366442176723,-27.0232689303461,
-26.9311985936299,-26.8177871413807,-26.7045794573521,-26.5914851307706,
-26.4784592201845,-26.3654568858265,-26.2523500393167,-26.1391924175008,
-26.0258171301183,-25.9337467938658,-25.8203353417363,-25.7071276578268,
-25.5940333313641,-25.4810074208961,-25.3680050866555,-25.254898240261,
-25.1417406185593,-25.0283653312878,-24.9362949941018,-24.8228835419418,
-24.7096758580039,-24.5965815315139,-24.4835556210198,-24.3705532867545,
-24.2574464403373,-24.1442888186141,-24.0309135313233,-23.9388431943377,
-23.8254356156578,-23.7122317969665,-23.5991413251002,-23.486119251654,
-23.3731207299011,-23.2600176887708,-23.1468638370261,-23.0334923835988,
-22.9415794423358),.UNSPECIFIED.);
#616=B_SPLINE_CURVE_WITH_KNOTS('',3,(#46632,#46633,#46634,#46635,#46636,
#46637,#46638,#46639,#46640,#46641,#46642,#46643,#46644,#46645,#46646,#46647,
#46648,#46649,#46650,#46651,#46652,#46653,#46654,#46655,#46656,#46657,#46658,
#46659,#46660,#46661,#46662,#46663,#46664,#46665,#46666,#46667,#46668,#46669,
#46670,#46671,#46672,#46673,#46674,#46675,#46676,#46677,#46678,#46679,#46680,
#46681,#46682,#46683,#46684,#46685,#46686,#46687,#46688,#46689,#46690,#46691,
#46692,#46693,#46694,#46695,#46696,#46697,#46698,#46699,#46700,#46701,#46702,
#46703,#46704,#46705,#46706,#46707,#46708,#46709,#46710,#46711,#46712,#46713,
#46714,#46715,#46716,#46717,#46718,#46719,#46720,#46721,#46722,#46723,#46724,
#46725,#46726,#46727,#46728,#46729,#46730,#46731,#46732,#46733,#46734,#46735,
#46736,#46737,#46738,#46739,#46740,#46741,#46742,#46743,#46744,#46745,#46746,
#46747,#46748,#46749,#46750,#46751,#46752,#46753,#46754,#46755,#46756,#46757,
#46758,#46759,#46760,#46761,#46762,#46763,#46764,#46765,#46766,#46767,#46768,
#46769,#46770,#46771,#46772,#46773,#46774,#46775,#46776,#46777,#46778,#46779,
#46780,#46781,#46782,#46783,#46784,#46785,#46786,#46787,#46788,#46789,#46790,
#46791,#46792,#46793,#46794,#46795,#46796,#46797,#46798,#46799,#46800,#46801,
#46802,#46803),.UNSPECIFIED.,.F.,.F.,(4,3,3,3,3,3,3,3,3,3,3,3,3,3,3,3,3,
3,3,3,3,3,3,3,3,3,3,3,3,3,3,3,3,3,3,3,3,3,3,3,3,3,3,3,3,3,3,3,3,3,3,3,3,
3,3,3,3,4),(19.9722977286751,20.0852614447579,20.1980240325097,20.3106755095438,
20.4232615627257,20.5358277786643,20.6484999916156,20.7612277552495,20.8741653780159,
20.9464877950455,21.0598992471089,21.1731069309596,21.2862012573683,21.3992271677869,
21.5122295019828,21.6253363483408,21.7384939700102,21.8518692572571,21.9439395948096,
22.0573510464558,22.170558729865,22.2836530558175,22.3966789657663,22.5096812994795,
22.6227881453382,22.7359457664985,22.8493210532263,22.9413913945736,23.0548028471147,
23.1680105314422,23.2811048583265,23.394130769219,23.5071331038862,23.6202399507073,
23.7333975728362,23.8467728605304,23.9388431943377,24.0522546464927,24.1654623304275,
24.2785566569154,24.3915825674085,24.5045849016738,24.6176917480928,24.7308493698188,
24.8442246571138,24.9362949941018,25.049706446238,25.1629141301516,25.276008456617,
25.389034367086,25.502036701326,25.6151435477177,25.728301169415,25.84167645668,
25.9337467938658,26.0684010631508,26.2015071711322,26.2554830347735),
 .UNSPECIFIED.);
#617=B_SPLINE_CURVE_WITH_KNOTS('',3,(#46808,#46809,#46810,#46811,#46812,
#46813,#46814,#46815,#46816,#46817),.UNSPECIFIED.,.F.,.F.,(4,1,1,1,1,1,
1,4),(-35.5079500563466,-34.9108129917425,-33.9133611919784,-32.9159093922143,
-31.9184575924503,-30.9210057926862,-29.9235539929221,-29.2247647491671),
 .UNSPECIFIED.);
#618=B_SPLINE_CURVE_WITH_KNOTS('',3,(#46818,#46819,#46820,#46821,#46822,
#46823,#46824,#46825,#46826,#46827,#46828,#46829,#46830,#46831,#46832,#46833,
#46834,#46835,#46836,#46837,#46838,#46839,#46840,#46841,#46842,#46843,#46844,
#46845,#46846,#46847,#46848,#46849,#46850,#46851,#46852,#46853,#46854,#46855,
#46856,#46857,#46858,#46859,#46860,#46861,#46862,#46863,#46864,#46865,#46866,
#46867,#46868,#46869,#46870,#46871,#46872,#46873,#46874,#46875,#46876,#46877,
#46878,#46879,#46880,#46881,#46882,#46883,#46884,#46885,#46886,#46887,#46888,
#46889,#46890,#46891,#46892,#46893,#46894,#46895,#46896,#46897,#46898,#46899,
#46900,#46901,#46902,#46903,#46904,#46905,#46906,#46907,#46908,#46909,#46910,
#46911,#46912,#46913,#46914,#46915,#46916,#46917,#46918,#46919,#46920,#46921,
#46922,#46923,#46924,#46925,#46926,#46927,#46928,#46929,#46930,#46931,#46932,
#46933,#46934,#46935,#46936,#46937,#46938,#46939,#46940,#46941,#46942,#46943,
#46944,#46945,#46946,#46947,#46948,#46949,#46950,#46951,#46952,#46953,#46954,
#46955,#46956,#46957,#46958,#46959,#46960,#46961,#46962,#46963,#46964,#46965,
#46966,#46967,#46968,#46969,#46970,#46971,#46972,#46973,#46974,#46975,#46976,
#46977,#46978,#46979,#46980,#46981,#46982,#46983,#46984,#46985,#46986,#46987,
#46988,#46989),.UNSPECIFIED.,.F.,.F.,(4,3,3,3,3,3,3,3,3,3,3,3,3,3,3,3,3,
3,3,3,3,3,3,3,3,3,3,3,3,3,3,3,3,3,3,3,3,3,3,3,3,3,3,3,3,3,3,3,3,3,3,3,3,
3,3,3,3,4),(26.2554830351794,26.3682243124585,26.4809384286302,26.5937592235565,
26.7066280453205,26.8197294891619,26.9311985936299,27.0446100458205,27.1578177297904,
27.2709120563132,27.3839379668408,27.4969403011404,27.6100471475925,27.723204769351,
27.8365800566775,27.928650393394,28.0420618455871,28.1552695295592,28.268363856084,
28.3813897666136,28.4943921009147,28.6074989473684,28.7206565691285,28.8340318564562,
28.9261021931581,29.0395136453643,29.1527213293499,29.2658156558886,29.3788415664321,
29.4918439007475,29.6049507472155,29.71810836899,29.8314836563322,29.9235539929221,
30.0369654451204,30.1501731290981,30.2632674556285,30.3762933661638,30.4892957004709,
30.6024025469306,30.7155601686967,30.8289354560306,30.9210057926862,31.0344172448853,
31.1476249288639,31.2607192553953,31.3737451659315,31.4867475002398,31.5998543467004,
31.7130119684676,31.8263872558023,31.9184575924503,32.0328851634577,32.1471215288982,
32.2611933998447,32.375169438642,32.489104873967,32.538668342359),
 .UNSPECIFIED.);
#619=B_SPLINE_CURVE_WITH_KNOTS('',3,(#46994,#46995,#46996,#46997,#46998,
#46999,#47000,#47001,#47002,#47003,#47004,#47005,#47006,#47007,#47008,#47009,
#47010,#47011,#47012,#47013,#47014,#47015,#47016,#47017,#47018,#47019,#47020,
#47021,#47022,#47023,#47024,#47025,#47026,#47027,#47028,#47029,#47030,#47031,
#47032,#47033,#47034,#47035,#47036,#47037,#47038,#47039,#47040,#47041,#47042,
#47043,#47044,#47045,#47046,#47047,#47048,#47049,#47050,#47051,#47052,#47053,
#47054,#47055,#47056,#47057,#47058,#47059,#47060,#47061,#47062,#47063,#47064,
#47065,#47066,#47067,#47068,#47069,#47070,#47071,#47072,#47073,#47074,#47075,
#47076,#47077,#47078,#47079,#47080,#47081,#47082,#47083,#47084,#47085,#47086,
#47087,#47088,#47089,#47090,#47091,#47092,#47093,#47094,#47095,#47096,#47097,
#47098,#47099,#47100,#47101,#47102,#47103,#47104,#47105,#47106,#47107,#47108,
#47109,#47110,#47111,#47112,#47113,#47114,#47115,#47116,#47117,#47118,#47119,
#47120,#47121,#47122,#47123,#47124,#47125,#47126,#47127,#47128,#47129,#47130,
#47131,#47132,#47133,#47134,#47135,#47136,#47137,#47138,#47139,#47140,#47141,
#47142,#47143,#47144,#47145,#47146,#47147,#47148,#47149,#47150,#47151,#47152,
#47153,#47154,#47155,#47156,#47157,#47158,#47159,#47160,#47161,#47162,#47163,
#47164,#47165),.UNSPECIFIED.,.F.,.F.,(4,3,3,3,3,3,3,3,3,3,3,3,3,3,3,3,3,
3,3,3,3,3,3,3,3,3,3,3,3,3,3,3,3,3,3,3,3,3,3,3,3,3,3,3,3,3,3,3,3,3,3,3,3,
3,3,3,3,4),(-41.7911353630763,-41.6791839164827,-41.5674467917417,-41.4558025914072,
-41.3442043092205,-41.2320341794971,-41.1203170881086,-41.0079204392178,
-40.8955237903269,-40.7821123381277,-40.6689046541491,-40.5558103276177,
-40.4427844170814,-40.3297820827733,-40.2166752363126,-40.1035176145455,
-39.9901423272108,-39.8980719905628,-39.7846605383621,-39.671452854382,
-39.558358527849,-39.4453326173112,-39.3323302830015,-39.2192234365393,
-39.1060658147706,-38.9926905274342,-38.9006201907988,-38.7872087385991,
-38.67400105462,-38.560906728088,-38.4478808175513,-38.3348784832428,-38.2217716367815,
-38.108614015014,-37.9952387276787,-37.9031683910347,-37.7897569388349,
-37.6765492548556,-37.5634549283234,-37.4504290177865,-37.3374266834777,
-37.2243198370163,-37.1111622152485,-36.997786927913,-36.9057165912706,
-36.7923051390707,-36.6790974550913,-36.5660031285592,-36.4529772180219,
-36.3399748837131,-36.2268680372516,-36.1137104154836,-36.000335128148,
-35.9082647915066,-35.7824128954135,-35.657006136482,-35.5322949997494,
-35.507950489932),.UNSPECIFIED.);
#620=B_SPLINE_CURVE_WITH_KNOTS('',3,(#47166,#47167,#47168,#47169,#47170,
#47171,#47172,#47173,#47174,#47175),.UNSPECIFIED.,.F.,.F.,(4,1,1,1,1,1,
1,4),(32.5386754793687,32.9159093922144,33.9133611919784,34.9108129917425,
35.9082647915066,36.9057165912706,37.9031683910347,38.8218455523264),
 .UNSPECIFIED.);
#621=B_SPLINE_CURVE_WITH_KNOTS('',3,(#47180,#47181,#47182,#47183,#47184,
#47185,#47186,#47187,#47188,#47189,#47190,#47191,#47192,#47193,#47194,#47195,
#47196,#47197,#47198,#47199,#47200,#47201,#47202,#47203,#47204,#47205,#47206,
#47207,#47208,#47209,#47210,#47211,#47212,#47213,#47214,#47215,#47216,#47217,
#47218,#47219,#47220,#47221,#47222,#47223,#47224,#47225,#47226,#47227,#47228,
#47229,#47230,#47231,#47232,#47233,#47234,#47235,#47236,#47237,#47238,#47239,
#47240,#47241,#47242,#47243,#47244,#47245,#47246,#47247,#47248,#47249,#47250,
#47251,#47252,#47253,#47254,#47255,#47256,#47257,#47258,#47259,#47260,#47261,
#47262,#47263,#47264,#47265,#47266,#47267,#47268,#47269,#47270,#47271,#47272,
#47273,#47274,#47275,#47276,#47277,#47278,#47279,#47280,#47281,#47282,#47283,
#47284,#47285,#47286,#47287,#47288,#47289,#47290,#47291,#47292,#47293,#47294,
#47295,#47296,#47297,#47298,#47299,#47300,#47301,#47302,#47303,#47304,#47305,
#47306,#47307,#47308,#47309,#47310,#47311,#47312,#47313,#47314,#47315,#47316,
#47317,#47318,#47319,#47320,#47321,#47322,#47323,#47324,#47325,#47326,#47327,
#47328,#47329,#47330,#47331,#47332,#47333,#47334,#47335,#47336,#47337,#47338,
#47339,#47340,#47341,#47342,#47343,#47344,#47345,#47346,#47347,#47348,#47349,
#47350,#47351),.UNSPECIFIED.,.F.,.F.,(4,3,3,3,3,3,3,3,3,3,3,3,3,3,3,3,3,
3,3,3,3,3,3,3,3,3,3,3,3,3,3,3,3,3,3,3,3,3,3,3,3,3,3,3,3,3,3,3,3,3,3,3,3,
3,3,3,3,4),(-48.0743206707058,-47.9107513804871,-47.8776863886754,-47.7642749365203,
-47.6510672525854,-47.5379729260974,-47.4249470156042,-47.3119446813386,
-47.1988378349195,-47.0856802131936,-46.9723049258985,-46.8802345889113,
-46.7668231367748,-46.653615452861,-46.5405211263955,-46.4274952159263,
-46.3144928816861,-46.2013860352943,-46.0882284135968,-45.9748531263316,
-45.8827827891473,-45.7693713369007,-45.6561636528737,-45.5430693262933,
-45.4300434157076,-45.3170410813495,-45.2039342348387,-45.0907766130212,
-44.9774013256363,-44.8853309893832,-44.7719195371926,-44.6587118532226,
-44.5456175266998,-44.4325916161722,-44.3195892818726,-44.2064824354204,
-44.0933248136618,-43.9799495263352,-43.8878791896191,-43.7744677374261,
-43.661260053454,-43.5481657269291,-43.4351398163996,-43.3221374820982,
-43.2090306356445,-43.0958730138844,-42.9824977265567,-42.890427389855,
-42.7770159376488,-42.6638082536632,-42.5507139271245,-42.437688016581,
-42.3246856822654,-42.2115788357974,-42.0984212140229,-41.9850459266807,
-41.892975590091,-41.7911353635262),.UNSPECIFIED.);
#622=B_SPLINE_CURVE_WITH_KNOTS('',3,(#47352,#47353,#47354,#47355,#47356,
#47357,#47358,#47359,#47360,#47361,#47362,#47363,#47364,#47365,#47366,#47367,
#47368,#47369,#47370,#47371,#47372,#47373,#47374,#47375,#47376,#47377,#47378,
#47379,#47380,#47381,#47382,#47383,#47384,#47385,#47386,#47387,#47388,#47389,
#47390,#47391,#47392,#47393,#47394,#47395,#47396,#47397,#47398,#47399,#47400,
#47401,#47402,#47403,#47404,#47405,#47406,#47407,#47408,#47409,#47410,#47411,
#47412,#47413,#47414,#47415,#47416,#47417,#47418,#47419,#47420,#47421,#47422,
#47423,#47424,#47425,#47426,#47427,#47428,#47429,#47430,#47431,#47432,#47433,
#47434,#47435,#47436,#47437,#47438,#47439,#47440,#47441,#47442,#47443,#47444,
#47445,#47446,#47447,#47448,#47449,#47450,#47451,#47452,#47453,#47454,#47455,
#47456,#47457,#47458,#47459,#47460,#47461,#47462,#47463,#47464,#47465,#47466,
#47467,#47468,#47469,#47470,#47471,#47472,#47473,#47474,#47475,#47476,#47477,
#47478,#47479,#47480,#47481,#47482,#47483,#47484,#47485,#47486,#47487,#47488,
#47489,#47490,#47491,#47492,#47493,#47494,#47495,#47496,#47497,#47498,#47499,
#47500,#47501,#47502,#47503,#47504,#47505,#47506,#47507,#47508,#47509,#47510,
#47511,#47512,#47513,#47514,#47515,#47516,#47517,#47518,#47519,#47520,#47521,
#47522,#47523),.UNSPECIFIED.,.F.,.F.,(4,3,3,3,3,3,3,3,3,3,3,3,3,3,3,3,3,
3,3,3,3,3,3,3,3,3,3,3,3,3,3,3,3,3,3,3,3,3,3,3,3,3,3,3,3,3,3,3,3,3,3,3,3,
3,3,3,3,4),(38.8218536495386,38.9006201907988,39.0140316429996,39.1272393269797,
39.2403336535128,39.3533595640506,39.4663618983604,39.5794687448226,39.6926263665913,
39.8060016539276,39.8980719905628,40.0114834427619,40.1246911267404,40.2377854532718,
40.350811363808,40.4638136981161,40.5769205445768,40.6900781663439,40.8034534536787,
40.8955237903269,41.0089352425252,41.1221429265028,41.2352372530334,41.3482631635687,
41.4612654978759,41.5743723443357,41.6875299661018,41.8009052534357,41.892975590091,
42.0063870422976,42.1195947262836,42.2326890528224,42.345714963366,42.4587172976816,
42.5718241441495,42.6849817659238,42.7983570532657,42.8904273898551,43.0038388420472,
43.1170465260187,43.2301408525431,43.3431667630725,43.4561690973737,43.5692759438278,
43.6824335655883,43.7958088529168,43.8878791896191,44.0012906418101,44.1144983257803,
44.2275926523032,44.3406185628308,44.4536208971304,44.5667277435824,44.6798853653407,
44.7932606526669,44.8853309893832,45.0403742212961,45.1050389567181),
 .UNSPECIFIED.);
#623=B_SPLINE_CURVE_WITH_KNOTS('',3,(#47528,#47529,#47530,#47531,#47532,
#47533,#47534,#47535,#47536,#47537),.UNSPECIFIED.,.F.,.F.,(4,1,1,1,1,1,
1,4),(-54.3575057011833,-53.8623971872598,-52.8649453874958,-51.8674935877317,
-50.8700417879676,-49.8725899882035,-48.8751381884395,-48.0743241720579),
 .UNSPECIFIED.);
#624=B_SPLINE_CURVE_WITH_KNOTS('',3,(#47538,#47539,#47540,#47541,#47542,
#47543,#47544,#47545,#47546,#47547,#47548,#47549,#47550,#47551,#47552,#47553,
#47554,#47555,#47556,#47557,#47558,#47559,#47560,#47561,#47562,#47563,#47564,
#47565,#47566,#47567,#47568,#47569,#47570,#47571,#47572,#47573,#47574,#47575,
#47576,#47577,#47578,#47579,#47580,#47581,#47582,#47583,#47584,#47585,#47586,
#47587,#47588,#47589,#47590,#47591,#47592,#47593,#47594,#47595,#47596,#47597,
#47598,#47599,#47600,#47601,#47602,#47603,#47604,#47605,#47606,#47607,#47608,
#47609,#47610,#47611,#47612,#47613,#47614,#47615,#47616,#47617,#47618,#47619,
#47620,#47621,#47622,#47623,#47624,#47625,#47626,#47627,#47628,#47629,#47630,
#47631,#47632,#47633,#47634,#47635,#47636,#47637,#47638,#47639,#47640,#47641,
#47642,#47643,#47644,#47645,#47646,#47647,#47648,#47649,#47650,#47651,#47652,
#47653,#47654,#47655,#47656,#47657,#47658,#47659,#47660,#47661,#47662,#47663,
#47664,#47665,#47666,#47667,#47668,#47669,#47670,#47671,#47672,#47673,#47674,
#47675,#47676,#47677,#47678,#47679,#47680,#47681,#47682,#47683,#47684,#47685,
#47686,#47687,#47688,#47689,#47690,#47691,#47692,#47693,#47694,#47695,#47696,
#47697,#47698,#47699,#47700,#47701,#47702,#47703,#47704,#47705,#47706,#47707,
#47708,#47709),.UNSPECIFIED.,.F.,.F.,(4,3,3,3,3,3,3,3,3,3,3,3,3,3,3,3,3,
3,3,3,3,3,3,3,3,3,3,3,3,3,3,3,3,3,3,3,3,3,3,3,3,3,3,3,3,3,3,3,3,3,3,3,3,
3,3,3,3,4),(45.1050389572695,45.2166679109873,45.3282052498347,45.4396980981619,
45.5512757199758,45.662889531836,45.7747203023662,45.8827827891473,45.9961942412766,
46.1094019251858,46.2224962516483,46.3355221621161,46.4485244963565,46.5616313427509,
46.6747889644524,46.7881642517237,46.8802345889113,46.9936460410712,47.1068537250089,
47.2199480514988,47.3329739619927,47.4459762962578,47.5590831426749,47.6722407643979,
47.7856160516885,47.8776863886754,47.9910978412332,48.1043055255711,48.2173998524622,
48.3304257633577,48.443428098024,48.5565349448385,48.6696925669575,48.7830678546367,
48.8751381884395,48.9885496400318,49.1017573234071,49.214851649338,49.3278775592774,
49.4408798929934,49.5539867388737,49.6671443600661,49.7805196468428,49.8725899882036,
49.9860014403177,50.0992091242004,50.2123034506294,50.3253293610571,50.4383316952503,
50.551438541588,50.6645961632272,50.777971450428,50.8700417879676,50.9882858012164,
51.1061966176998,51.2239066097079,51.3413928306475,51.3882242638978),
 .UNSPECIFIED.);
#625=B_SPLINE_CURVE_WITH_KNOTS('',3,(#47714,#47715,#47716,#47717,#47718,
#47719,#47720,#47721,#47722,#47723,#47724,#47725,#47726,#47727,#47728,#47729,
#47730,#47731,#47732,#47733,#47734,#47735,#47736,#47737,#47738,#47739,#47740,
#47741,#47742,#47743,#47744,#47745,#47746,#47747,#47748,#47749,#47750,#47751,
#47752,#47753,#47754,#47755,#47756,#47757,#47758,#47759,#47760,#47761,#47762,
#47763,#47764,#47765,#47766,#47767,#47768,#47769,#47770,#47771,#47772,#47773,
#47774,#47775,#47776,#47777,#47778,#47779,#47780,#47781,#47782,#47783,#47784,
#47785,#47786,#47787,#47788,#47789,#47790,#47791,#47792,#47793,#47794,#47795,
#47796,#47797,#47798,#47799,#47800,#47801,#47802,#47803,#47804,#47805,#47806,
#47807,#47808,#47809,#47810,#47811,#47812,#47813,#47814,#47815,#47816,#47817,
#47818,#47819,#47820,#47821,#47822,#47823,#47824,#47825,#47826,#47827,#47828,
#47829,#47830,#47831,#47832,#47833,#47834,#47835,#47836,#47837,#47838,#47839,
#47840,#47841,#47842,#47843,#47844,#47845,#47846,#47847,#47848,#47849,#47850,
#47851,#47852,#47853,#47854,#47855,#47856,#47857,#47858,#47859,#47860,#47861,
#47862,#47863,#47864,#47865,#47866,#47867,#47868,#47869,#47870,#47871,#47872,
#47873,#47874,#47875,#47876,#47877,#47878,#47879,#47880,#47881,#47882,#47883,
#47884,#47885),.UNSPECIFIED.,.F.,.F.,(4,3,3,3,3,3,3,3,3,3,3,3,3,3,3,3,3,
3,3,3,3,3,3,3,3,3,3,3,3,3,3,3,3,3,3,3,3,3,3,3,3,3,3,3,3,3,3,3,3,3,3,3,3,
3,3,3,3,4),(-60.6406912844698,-60.5291209741293,-60.417650226069,-60.3062318016793,
-60.1914508477206,-60.0799232699748,-59.9635156279096,-59.8471079858443,
-59.7336963268614,-59.6204884267402,-59.5073938785023,-59.3943677410919,
-59.2813651751309,-59.1682580914026,-59.0551002288817,-58.9417246980488,
-58.8496561860802,-58.7362450335743,-58.6230376567668,-58.5099436417519,
-58.3969180465193,-58.2839160307492,-58.1708095053147,-58.0576522064656,
-57.9442772410778,-57.8522043863161,-57.7387928221874,-57.6255850245746,
-57.5124905834508,-57.3994645575697,-57.2864621073685,-57.1733551450959,
-57.0601974073755,-56.9468220053348,-56.854752586552,-56.7413411185027,
-56.6281334176777,-56.5150390737027,-56.4020131451571,-56.289010792304,
-56.1759039266089,-56.0627462851953,-55.9493709777767,-55.857300786788,
-55.7438893723472,-55.6306817271192,-55.5175874399162,-55.404561569216,
-55.2915592751816,-55.1784524693545,-55.0652948884853,-54.9519196419665,
-54.8598489870239,-54.7408090857764,-54.622127699113,-54.503666173285,-54.3854603615985,
-54.3575059778853),.UNSPECIFIED.);
#626=B_SPLINE_CURVE_WITH_KNOTS('',3,(#47886,#47887,#47888,#47889,#47890,
#47891,#47892,#47893,#47894,#47895,#47896,#47897,#47898,#47899,#47900,#47901,
#47902,#47903,#47904,#47905,#47906,#47907,#47908,#47909,#47910,#47911,#47912,
#47913,#47914,#47915,#47916,#47917,#47918,#47919,#47920,#47921,#47922,#47923,
#47924,#47925,#47926,#47927,#47928,#47929,#47930,#47931,#47932,#47933,#47934,
#47935,#47936,#47937,#47938,#47939,#47940,#47941,#47942,#47943,#47944,#47945,
#47946,#47947,#47948,#47949,#47950,#47951,#47952,#47953,#47954,#47955,#47956,
#47957,#47958,#47959,#47960,#47961,#47962,#47963,#47964,#47965,#47966,#47967,
#47968,#47969,#47970,#47971,#47972,#47973,#47974,#47975,#47976,#47977,#47978,
#47979,#47980,#47981,#47982,#47983,#47984,#47985,#47986,#47987,#47988,#47989,
#47990,#47991,#47992,#47993,#47994,#47995,#47996,#47997,#47998,#47999,#48000,
#48001,#48002,#48003,#48004,#48005,#48006,#48007,#48008,#48009,#48010,#48011,
#48012,#48013,#48014,#48015,#48016,#48017,#48018,#48019,#48020,#48021,#48022,
#48023,#48024,#48025,#48026,#48027,#48028,#48029,#48030,#48031,#48032,#48033,
#48034,#48035,#48036,#48037,#48038,#48039,#48040,#48041,#48042,#48043,#48044,
#48045,#48046,#48047,#48048,#48049,#48050,#48051,#48052,#48053,#48054,#48055,
#48056,#48057),.UNSPECIFIED.,.F.,.F.,(4,3,3,3,3,3,3,3,3,3,3,3,3,3,3,3,3,
3,3,3,3,3,3,3,3,3,3,3,3,3,3,3,3,3,3,3,3,3,3,3,3,3,3,3,3,3,3,3,3,3,3,3,3,
3,3,3,3,4),(51.388224264309,51.5080415951646,51.6277999255016,51.747986711116,
51.8674935877317,51.9809050348777,52.0941127138258,52.2072070353442,52.3202329408932,
52.4332352702484,52.5463421118483,52.6594997287978,52.7728750114472,52.8649453874958,
52.9783568407164,53.091564525633,53.2046588530513,53.3176847644222,53.430687099512,
53.5437939466665,53.6569515690802,53.7703268569763,53.8623971872599,53.9758086567831,
54.0890163581752,54.2021107021622,54.3151366301656,54.428138981922,54.5412458456617,
54.6544034846422,54.7677787888627,54.8598489870239,54.9732603983721,55.0864680416299,
55.1995623275488,55.3125881976491,55.4255904917669,55.5386972987355,55.6518548813328,
55.7652301305258,55.857300786788,55.9707122592066,56.0839199627815,56.1970143085166,
56.3100402378354,56.4230425904762,56.5361494544338,56.6493070932641,56.7626823967366,
56.8547525865521,56.96644110335,57.0779705555368,57.1893884864546,57.3007422449335,
57.4121297263007,57.5235379612258,57.6350798901998,57.6714095705593),
 .UNSPECIFIED.);
#627=B_SPLINE_CURVE_WITH_KNOTS('',3,(#48062,#48063,#48064,#48065,#48066,
#48067,#48068,#48069,#48070,#48071,#48072,#48073,#48074,#48075,#48076,#48077,
#48078,#48079,#48080,#48081,#48082,#48083,#48084,#48085,#48086,#48087,#48088,
#48089,#48090,#48091,#48092,#48093,#48094,#48095,#48096,#48097,#48098,#48099,
#48100,#48101,#48102,#48103,#48104,#48105,#48106,#48107,#48108,#48109,#48110,
#48111,#48112,#48113,#48114,#48115,#48116,#48117,#48118,#48119,#48120,#48121,
#48122,#48123,#48124,#48125,#48126,#48127,#48128,#48129,#48130,#48131,#48132,
#48133,#48134,#48135,#48136,#48137,#48138,#48139,#48140,#48141,#48142,#48143,
#48144,#48145,#48146,#48147,#48148,#48149,#48150,#48151,#48152,#48153,#48154,
#48155,#48156,#48157,#48158,#48159,#48160,#48161,#48162,#48163,#48164,#48165,
#48166,#48167,#48168,#48169,#48170,#48171,#48172,#48173,#48174,#48175,#48176,
#48177,#48178,#48179,#48180,#48181,#48182,#48183,#48184,#48185,#48186,#48187,
#48188,#48189,#48190,#48191,#48192,#48193,#48194,#48195,#48196,#48197,#48198,
#48199,#48200,#48201,#48202,#48203,#48204,#48205,#48206,#48207,#48208,#48209,
#48210,#48211,#48212,#48213,#48214,#48215,#48216,#48217,#48218,#48219,#48220,
#48221,#48222,#48223,#48224,#48225,#48226,#48227,#48228,#48229,#48230,#48231,
#48232,#48233),.UNSPECIFIED.,.F.,.F.,(4,3,3,3,3,3,3,3,3,3,3,3,3,3,3,3,3,
3,3,3,3,3,3,3,3,3,3,3,3,3,3,3,3,3,3,3,3,3,3,3,3,3,3,3,3,3,3,3,3,3,3,3,3,
3,3,3,3,4),(-66.9238765922446,-66.8292705841928,-66.7158357794347,-66.6026047197083,
-66.4894870207858,-66.3764377834166,-66.2634122100187,-66.150282450917,
-66.0371020603601,-65.9237045358565,-65.8318187844287,-65.7183863844429,
-65.6051570436917,-65.4920406429159,-65.3789922802997,-65.2659671551746,
-65.1528371718813,-65.0396561848354,-64.9262574496734,-64.8343669846646,
-64.7209731386006,-64.6077834563938,-64.4947073603155,-64.3816998763103,
-64.2687161323106,-64.155627982331,-64.0424891458818,-63.9291325519897,
-63.8369151849005,-63.7234994326658,-63.6102874129762,-63.4971887321421,
-63.384158456542,-63.2711517542119,-63.1580405705486,-63.0448786216547,
-62.9314990793927,-62.8394633851365,-62.726049743495,-62.6128397870048,
-62.4997431388413,-62.386714861707,-62.2737101199256,-62.1606008214247,
-62.0474407190319,-61.9340629350545,-61.8420115853724,-61.7286024564631,
-61.615397150865,-61.5023052346435,-61.3892817620273,-61.2762818889718,
-61.1631775203868,-61.0500223896721,-60.9366495835322,-60.8445597856083,
-60.683912590964,-60.640691285065),.UNSPECIFIED.);
#628=B_SPLINE_CURVE_WITH_KNOTS('',3,(#48234,#48235,#48236,#48237,#48238,
#48239,#48240,#48241,#48242,#48243,#48244,#48245,#48246,#48247,#48248,#48249,
#48250,#48251,#48252,#48253,#48254,#48255,#48256,#48257,#48258,#48259,#48260,
#48261,#48262,#48263,#48264,#48265,#48266,#48267,#48268,#48269,#48270,#48271,
#48272,#48273,#48274,#48275,#48276,#48277,#48278,#48279,#48280,#48281,#48282,
#48283,#48284,#48285,#48286,#48287,#48288,#48289,#48290,#48291,#48292,#48293,
#48294,#48295,#48296,#48297,#48298,#48299,#48300,#48301,#48302,#48303,#48304,
#48305,#48306,#48307,#48308,#48309,#48310,#48311,#48312,#48313,#48314,#48315,
#48316,#48317,#48318,#48319,#48320,#48321,#48322,#48323,#48324,#48325,#48326,
#48327,#48328,#48329,#48330,#48331,#48332,#48333,#48334,#48335,#48336,#48337,
#48338,#48339,#48340,#48341,#48342,#48343,#48344,#48345,#48346,#48347,#48348,
#48349,#48350,#48351,#48352,#48353,#48354,#48355,#48356,#48357,#48358,#48359,
#48360,#48361,#48362,#48363,#48364,#48365,#48366,#48367,#48368,#48369,#48370,
#48371,#48372,#48373,#48374,#48375,#48376,#48377,#48378,#48379,#48380,#48381,
#48382,#48383,#48384,#48385,#48386,#48387,#48388,#48389,#48390,#48391,#48392,
#48393,#48394,#48395,#48396,#48397,#48398,#48399,#48400,#48401,#48402,#48403,
#48404,#48405),.UNSPECIFIED.,.F.,.F.,(4,3,3,3,3,3,3,3,3,3,3,3,3,3,3,3,3,
3,3,3,3,3,3,3,3,3,3,3,3,3,3,3,3,3,3,3,3,3,3,3,3,3,3,3,3,3,3,3,3,3,3,3,3,
3,3,3,3,4),(57.6714095710774,57.8424716034082,57.8522043863161,57.96561551648,
58.0788228790694,58.1919168848318,58.3049424757643,58.4179444921801,58.5310510259175,
58.644208337316,58.7575833221,58.8496561860802,58.9630678826949,59.0762758065309,
59.1893703699776,59.3023965141141,59.4153990783317,59.5285061472084,59.6416639876074,
59.7550394846039,59.8471079858443,59.9605201596495,60.0737285724546,60.1868236316899,
60.2998502774975,60.4128533483403,60.5259609273589,60.6391192806626,60.752495288486,
60.8445597856084,60.9579687573358,61.0711739630446,61.1842658143953,61.2972892570663,
61.410289135053,61.5233935625653,61.6365487821517,61.7499217254423,61.8420115853724,
61.9554255397486,62.0686356933578,62.1817324679752,62.2947608010934,62.4077655284956,
62.5208747037191,62.6340346224343,62.7474121254151,62.8394633851365,62.9528790761637,
63.0660910598602,63.1791897201077,63.2922199904731,63.4052267028848,63.5183379202786,
63.6314999160311,63.7448795262153,63.8369151849006,63.9545948782569),
 .UNSPECIFIED.);
#629=B_SPLINE_CURVE_WITH_KNOTS('',3,(#48408,#48409,#48410,#48411,#48412,
#48413,#48414,#48415,#48416,#48417,#48418,#48419,#48420,#48421,#48422,#48423,
#48424,#48425,#48426,#48427,#48428,#48429,#48430,#48431,#48432,#48433,#48434,
#48435,#48436,#48437,#48438,#48439,#48440,#48441,#48442,#48443,#48444,#48445,
#48446,#48447,#48448,#48449,#48450,#48451,#48452,#48453,#48454,#48455,#48456,
#48457,#48458,#48459,#48460,#48461,#48462,#48463,#48464,#48465,#48466,#48467,
#48468,#48469,#48470,#48471,#48472,#48473,#48474,#48475,#48476,#48477,#48478,
#48479,#48480,#48481,#48482,#48483,#48484,#48485,#48486,#48487,#48488,#48489,
#48490,#48491,#48492,#48493,#48494,#48495,#48496,#48497,#48498,#48499,#48500,
#48501,#48502,#48503,#48504,#48505,#48506,#48507,#48508,#48509,#48510,#48511,
#48512,#48513,#48514,#48515,#48516,#48517,#48518,#48519,#48520,#48521,#48522,
#48523,#48524,#48525,#48526,#48527,#48528,#48529,#48530,#48531,#48532,#48533,
#48534,#48535,#48536,#48537,#48538,#48539,#48540,#48541,#48542,#48543,#48544,
#48545,#48546,#48547,#48548,#48549,#48550,#48551,#48552,#48553,#48554,#48555,
#48556,#48557,#48558,#48559,#48560,#48561,#48562,#48563,#48564,#48565,#48566,
#48567),.UNSPECIFIED.,.F.,.F.,(4,3,3,3,3,3,3,3,3,3,3,3,3,3,3,3,3,3,3,3,
3,3,3,3,3,3,3,3,3,3,3,3,3,3,3,3,3,3,3,3,3,3,3,3,3,3,3,3,3,3,3,3,3,4),(63.9545948787019,
64.0663283121786,64.1779267459133,64.2894374686781,64.4009076217729,64.5124655336905,
64.624063195758,64.7358746481165,64.8343669846646,64.9478019117417,65.0610328443785,
65.1741502653896,65.2871990781696,65.4002240842566,65.5133530677227,65.6265325663426,
65.7399290261141,65.8318187844287,65.9452523437199,66.0584826334375,66.1715998529507,
66.2846489006395,66.3976745735762,66.5108048794446,66.6239860649216,66.7373847835369,
66.8292705841928,66.9425447390915,67.0556149512323,67.1685717922222,67.2814604361248,
67.3943259551164,67.5072977677325,67.6203211180831,67.7335651001906,67.8267223839568,
67.9403424102071,68.0537571248511,68.1670573855848,68.2802877819635,68.3934928005795,
68.5067979340436,68.6201517182112,68.7337171970108,68.8241741837209,68.9390720244675,
69.0510940384473,69.16300915207,69.2748640897515,69.391987294737,69.5039323893411,
69.6159429374358,69.7281336005457,69.7433569096934),.UNSPECIFIED.);
#630=B_SPLINE_CURVE_WITH_KNOTS('',3,(#48570,#48571,#48572,#48573,#48574,
#48575,#48576,#48577),.UNSPECIFIED.,.F.,.F.,(4,1,1,1,1,4),(-71.8165295830131,
-70.819077783249,-69.821625983485,-68.8241741837209,-67.8267223839568,-66.9238856394982),
 .UNSPECIFIED.);
#631=B_SPLINE_CURVE_WITH_KNOTS('',3,(#48580,#48581,#48582,#48583,#48584,
#48585),.UNSPECIFIED.,.F.,.F.,(4,1,1,4),(76.8085816652527,77.4477585319289,
78.445210331693,78.5398163397448),.UNSPECIFIED.);
#632=B_SPLINE_CURVE_WITH_KNOTS('',3,(#48587,#48588,#48589,#48590,#48591,
#48592,#48593,#48594,#48595,#48596,#48597,#48598,#48599,#48600,#48601,#48602,
#48603,#48604,#48605,#48606,#48607,#48608,#48609,#48610,#48611,#48612,#48613,
#48614,#48615,#48616,#48617,#48618,#48619,#48620,#48621,#48622,#48623,#48624,
#48625,#48626,#48627,#48628,#48629,#48630,#48631,#48632,#48633,#48634,#48635,
#48636,#48637,#48638,#48639,#48640,#48641,#48642,#48643,#48644,#48645,#48646,
#48647,#48648,#48649,#48650,#48651,#48652,#48653,#48654,#48655,#48656,#48657,
#48658,#48659,#48660,#48661,#48662),.UNSPECIFIED.,.F.,.F.,(4,3,3,3,3,3,
3,3,3,3,3,3,3,3,3,3,3,3,3,3,3,3,3,3,3,4),(78.5398169174564,78.6578581631678,
78.7757424064956,78.8935252569696,79.0112621341111,79.1290951210731,79.2469767917089,
79.3650860989278,79.4426621314571,79.5673436064276,79.6870738654733,79.8066827764956,
79.9262228004682,80.0457462805851,80.165386573184,80.2850966099796,80.4050192989118,
80.4401139312211,80.5585544019957,80.6768236178663,80.7949767675224,80.9130688341455,
81.0312371578687,81.1494402209803,81.2678606949208,81.359267928529),
 .UNSPECIFIED.);
#633=B_SPLINE_CURVE_WITH_KNOTS('',3,(#48666,#48667,#48668,#48669,#48670,
#48671,#48672,#48673,#48674,#48675,#48676,#48677,#48678,#48679,#48680,#48681,
#48682,#48683,#48684,#48685,#48686,#48687,#48688,#48689,#48690,#48691,#48692,
#48693,#48694,#48695,#48696,#48697,#48698,#48699,#48700,#48701,#48702,#48703,
#48704,#48705),.UNSPECIFIED.,.F.,.F.,(4,3,3,3,3,3,3,3,3,3,3,3,3,4),(78.5398163397448,
78.659636125144,78.7796502246197,78.8997625732989,79.020191251719,79.1211139375573,
79.2457954125278,79.368520780898,79.4910833479872,79.6135264861919,79.7397862989743,
79.8621555193481,79.9903606283347,80.1185657373213),.UNSPECIFIED.);
#634=B_SPLINE_CURVE_WITH_KNOTS('',3,(#48706,#48707,#48708,#48709,#48710,
#48711,#48712,#48713,#48714,#48715,#48716,#48717,#48718,#48719,#48720,#48721,
#48722,#48723,#48724,#48725,#48726,#48727,#48728,#48729,#48730,#48731,#48732,
#48733,#48734,#48735,#48736,#48737,#48738,#48739,#48740,#48741,#48742,#48743,
#48744,#48745,#48746,#48747,#48748,#48749,#48750,#48751,#48752,#48753,#48754),
 .UNSPECIFIED.,.F.,.F.,(4,3,3,3,3,3,3,3,3,3,3,3,3,3,3,3,4),(76.8075006878804,
76.9271796581132,77.0470845181732,77.1262103380291,77.2508918129996,77.3705174501154,
77.4900255177582,77.6094686275862,77.7288992786733,77.8484533949029,77.9680810296881,
78.0879276324046,78.1236621377932,78.254454988324,78.3847951958607,78.5144734410687,
78.5398163389325),.UNSPECIFIED.);
#635=B_SPLINE_CURVE_WITH_KNOTS('',3,(#48759,#48760,#48761,#48762,#48763,
#48764,#48765,#48766,#48767,#48768,#48769,#48770,#48771,#48772,#48773,#48774,
#48775,#48776,#48777,#48778,#48779,#48780,#48781,#48782,#48783,#48784,#48785,
#48786,#48787,#48788,#48789,#48790,#48791,#48792,#48793,#48794,#48795,#48796,
#48797,#48798,#48799,#48800,#48801,#48802,#48803,#48804,#48805,#48806,#48807,
#48808,#48809,#48810,#48811,#48812,#48813,#48814,#48815,#48816,#48817,#48818,
#48819,#48820,#48821,#48822,#48823,#48824,#48825,#48826,#48827,#48828,#48829,
#48830,#48831,#48832,#48833,#48834,#48835,#48836,#48837),.UNSPECIFIED.,
 .F.,.F.,(4,3,3,3,3,3,3,3,3,3,3,3,3,3,3,3,3,3,3,3,3,3,3,3,3,3,4),(-0.272733684723234,
-0.263933091050529,-0.246609025869403,-0.237097850216621,-0.231283116386945,
-0.214097972171501,-0.199459807385004,-0.196214597656375,-0.179475273061678,
-0.163134910222118,-0.153693408780706,-0.149077859260717,-0.145944972824637,
-0.130068097350725,-0.12534056960152,-0.109094409153109,-0.101071207557617,
-0.0956993686354407,-0.0926136204289078,-0.0768607618484406,-0.0612146360061542,
-0.0532966001767691,-0.0475071880028156,-0.0447088814465312,-0.0296023839094069,
-0.0148011919547035,0.),.UNSPECIFIED.);
#636=B_SPLINE_CURVE_WITH_KNOTS('',3,(#48838,#48839,#48840,#48841,#48842,
#48843,#48844,#48845,#48846,#48847,#48848,#48849,#48850,#48851,#48852,#48853,
#48854,#48855,#48856,#48857,#48858,#48859,#48860,#48861,#48862,#48863,#48864,
#48865,#48866,#48867,#48868,#48869,#48870,#48871,#48872,#48873,#48874,#48875,
#48876,#48877,#48878,#48879,#48880,#48881,#48882,#48883,#48884,#48885,#48886,
#48887,#48888,#48889,#48890,#48891,#48892,#48893,#48894,#48895,#48896,#48897,
#48898,#48899,#48900,#48901,#48902,#48903,#48904,#48905,#48906,#48907,#48908,
#48909,#48910,#48911,#48912,#48913,#48914,#48915,#48916,#48917,#48918,#48919,
#48920,#48921,#48922),.UNSPECIFIED.,.F.,.F.,(4,3,3,3,3,3,3,3,3,3,3,3,3,
3,3,3,3,3,3,3,3,3,3,3,3,3,3,3,4),(-0.276631791712734,-0.267261996455995,
-0.252638662205674,-0.246312363040928,-0.242068560323364,-0.226785633742753,
-0.215996016587511,-0.212143694358535,-0.209338885277652,-0.193398609351846,
-0.177535603971384,-0.168251432662936,-0.162618668425473,-0.159671082387916,
-0.143143715898125,-0.140398918737591,-0.124353701295378,-0.116139469058262,
-0.111126710163082,-0.108002044299551,-0.0915419859739776,-0.0746030552852902,
-0.0650265681318801,-0.0590759629246126,-0.0560748708216743,-0.0528975941021778,
-0.0354276289851714,-0.0177138144925857,0.),.UNSPECIFIED.);
#637=B_SPLINE_CURVE_WITH_KNOTS('',3,(#49224,#49225,#49226,#49227),
 .UNSPECIFIED.,.F.,.F.,(4,4),(-0.026145581273058,0.),.UNSPECIFIED.);
#638=B_SPLINE_CURVE_WITH_KNOTS('',3,(#49228,#49229,#49230,#49231,#49232,
#49233,#49234,#49235,#49236,#49237,#49238,#49239,#49240,#49241,#49242,#49243,
#49244,#49245,#49246,#49247,#49248,#49249,#49250,#49251,#49252,#49253,#49254,
#49255,#49256,#49257,#49258,#49259,#49260,#49261,#49262,#49263,#49264,#49265,
#49266,#49267,#49268,#49269,#49270,#49271,#49272,#49273,#49274,#49275,#49276,
#49277,#49278,#49279,#49280,#49281,#49282,#49283,#49284,#49285,#49286,#49287,
#49288,#49289,#49290,#49291,#49292,#49293,#49294,#49295,#49296,#49297,#49298,
#49299,#49300,#49301,#49302,#49303,#49304,#49305,#49306,#49307,#49308,#49309),
 .UNSPECIFIED.,.F.,.F.,(4,3,3,3,3,3,3,3,3,3,3,3,3,3,3,3,3,3,3,3,3,3,3,3,
3,3,3,4),(-0.276631791712739,-0.267261996456003,-0.252555963292598,-0.246312378453633,
-0.242068565443008,-0.226785642088753,-0.21599602390543,-0.212143486540232,
-0.209338645876512,-0.193538398420259,-0.177483821941212,-0.168251250557197,
-0.162618632421756,-0.159671067091488,-0.143143700304065,-0.140398918737599,
-0.124285864682194,-0.111126709917846,-0.108002044065338,-0.0915419879252078,
-0.0746030592382071,-0.0650265697785082,-0.0590759664797879,-0.0560748754887655,
-0.0528975949305316,-0.035427631110524,-0.017713815555262,0.),
 .UNSPECIFIED.);
#639=B_SPLINE_CURVE_WITH_KNOTS('',3,(#49314,#49315,#49316,#49317,#49318,
#49319,#49320,#49321,#49322,#49323,#49324,#49325,#49326,#49327,#49328,#49329,
#49330,#49331,#49332,#49333,#49334,#49335,#49336,#49337,#49338,#49339,#49340,
#49341,#49342,#49343,#49344,#49345,#49346,#49347,#49348,#49349,#49350,#49351,
#49352,#49353,#49354,#49355,#49356,#49357,#49358,#49359,#49360,#49361,#49362,
#49363,#49364,#49365,#49366,#49367,#49368,#49369,#49370,#49371,#49372,#49373,
#49374,#49375,#49376,#49377,#49378,#49379,#49380,#49381,#49382,#49383,#49384,
#49385,#49386,#49387,#49388,#49389,#49390,#49391,#49392,#49393,#49394,#49395),
 .UNSPECIFIED.,.F.,.F.,(4,3,3,3,3,3,3,3,3,3,3,3,3,3,3,3,3,3,3,3,3,3,3,3,
3,3,3,4),(-0.272733710415022,-0.26393309105054,-0.246451516153048,-0.23709784863092,
-0.233168130330458,-0.215966889594249,-0.204638177861954,-0.1994597979912,
-0.196214581144175,-0.179475255804651,-0.163134888932547,-0.153693392769608,
-0.149077802760023,-0.145944936327465,-0.130068057058006,-0.125340569601517,
-0.108707156583976,-0.101071231081186,-0.095699368520472,-0.0926136207771124,
-0.0768306446800761,-0.0611558835737404,-0.0532966012025288,-0.0475071908126714,
-0.0447088840235041,-0.0296023913127002,-0.0148011956563501,0.),
 .UNSPECIFIED.);
#640=B_SPLINE_CURVE_WITH_KNOTS('',3,(#49697,#49698,#49699,#49700),
 .UNSPECIFIED.,.F.,.F.,(4,4),(-0.0264538357708102,0.),.UNSPECIFIED.);
#641=B_SPLINE_CURVE_WITH_KNOTS('',3,(#53054,#53055,#53056,#53057,#53058,
#53059,#53060),.UNSPECIFIED.,.F.,.F.,(4,3,4),(-0.0562125399722967,0.,0.0562125399722968),
 .UNSPECIFIED.);
#642=B_SPLINE_CURVE_WITH_KNOTS('',3,(#53062,#53063,#53064,#53065,#53066,
#53067),.UNSPECIFIED.,.F.,.F.,(4,2,4),(-0.961432950963571,-0.905220410991274,
-0.849007871018978),.UNSPECIFIED.);
#643=B_SPLINE_CURVE_WITH_KNOTS('',3,(#53077,#53078,#53079,#53080,#53081,
#53082,#53083),.UNSPECIFIED.,.F.,.F.,(4,3,4),(-0.0562125399722967,0.,0.0562125399722968),
 .UNSPECIFIED.);
#644=B_SPLINE_CURVE_WITH_KNOTS('',3,(#53085,#53086,#53087,#53088,#53089,
#53090),.UNSPECIFIED.,.F.,.F.,(4,2,4),(-0.961432950963571,-0.905220410991274,
-0.849007871018978),.UNSPECIFIED.);
#645=B_SPLINE_CURVE_WITH_KNOTS('',3,(#53163,#53164,#53165,#53166,#53167,
#53168,#53169,#53170,#53171,#53172,#53173,#53174,#53175,#53176,#53177,#53178,
#53179,#53180,#53181,#53182,#53183,#53184,#53185,#53186,#53187,#53188,#53189,
#53190,#53191,#53192,#53193,#53194,#53195,#53196,#53197,#53198,#53199,#53200,
#53201,#53202,#53203,#53204,#53205,#53206,#53207,#53208,#53209,#53210,#53211,
#53212,#53213,#53214,#53215,#53216,#53217,#53218,#53219,#53220,#53221,#53222,
#53223,#53224,#53225,#53226,#53227,#53228,#53229,#53230,#53231,#53232,#53233,
#53234,#53235,#53236,#53237,#53238,#53239,#53240,#53241,#53242,#53243,#53244,
#53245,#53246,#53247,#53248,#53249,#53250,#53251,#53252,#53253,#53254,#53255,
#53256,#53257,#53258,#53259,#53260,#53261,#53262,#53263,#53264,#53265,#53266,
#53267,#53268),.UNSPECIFIED.,.F.,.F.,(4,2,2,2,2,2,2,2,2,2,2,2,2,2,2,2,2,
2,2,2,2,2,2,2,2,2,2,2,2,2,2,2,2,2,2,2,2,2,2,2,2,2,2,2,2,2,2,2,2,2,2,2,4),
(-0.578057800930158,-0.576907658226536,-0.568154833588687,-0.561138999497065,
-0.552272437437979,-0.542064916508128,-0.517889363717969,-0.507443620840254,
-0.5026023411279,-0.498401345318794,-0.491060740642357,-0.469791252118237,
-0.451026489857121,-0.442347794318625,-0.435320724528266,-0.426342970288697,
-0.415944588322965,-0.390451736003233,-0.380837795881047,-0.376307614792867,
-0.371965237536568,-0.363532324173621,-0.350556965963959,-0.324775865056773,
-0.316215461473166,-0.309236126491577,-0.30027545529445,-0.289876340707482,
-0.264214578438879,-0.254775349788872,-0.250280578846039,-0.245883566264983,
-0.237234369709441,-0.223717989369306,-0.199058992042047,-0.190354569511272,
-0.1833018149302,-0.174278579622026,-0.163807016827302,-0.137775149213679,
-0.12869300762222,-0.124216054466084,-0.119638119348461,-0.109986931187581,
-0.0934027038767481,-0.0743184018899234,-0.0656129882769852,-0.0585836505909147,
-0.0494613038761158,-0.0260871743460905,-0.0069322348740228,-0.00303082776048378,
-0.00159986386543374),.UNSPECIFIED.);
#646=B_SPLINE_CURVE_WITH_KNOTS('',3,(#53271,#53272,#53273,#53274,#53275,
#53276,#53277,#53278,#53279,#53280,#53281,#53282,#53283,#53284,#53285,#53286,
#53287,#53288,#53289,#53290,#53291,#53292,#53293,#53294,#53295,#53296,#53297,
#53298,#53299,#53300,#53301,#53302,#53303,#53304,#53305,#53306,#53307,#53308,
#53309,#53310,#53311,#53312,#53313,#53314,#53315,#53316,#53317,#53318,#53319,
#53320,#53321,#53322,#53323,#53324,#53325,#53326,#53327,#53328,#53329,#53330,
#53331,#53332,#53333,#53334,#53335,#53336,#53337,#53338,#53339,#53340,#53341,
#53342,#53343,#53344),.UNSPECIFIED.,.F.,.F.,(4,2,2,2,2,2,2,2,2,2,2,2,2,
2,2,2,2,2,2,2,2,2,2,2,2,2,2,2,2,2,2,2,2,2,2,2,4),(-1.31816221225193,-1.31512894288896,
-1.31135704736811,-1.29605024055882,-1.27729638040057,-1.26581126211065,
-1.25797720490834,-1.2490398174757,-1.2250784758911,-1.20789126545402,-1.20072619108313,
-1.19494117273146,-1.19093691780624,-1.18558492912948,-1.16407570760206,
-1.14133523638755,-1.13327775490148,-1.12654658814491,-1.11792602250525,
-1.09490240366976,-1.07980411050715,-1.07323777199083,-1.06788103747146,
-1.06394552068814,-1.05828956237135,-1.03953710342389,-1.01571751125415,
-1.00661207639585,-0.999520056879496,-0.990771470388567,-0.97089804755582,
-0.954929106573042,-0.945466425191204,-0.940915981340912,-0.936417949046409,
-0.927487378930933,-0.911920807669219),.UNSPECIFIED.);
#647=B_SPLINE_CURVE_WITH_KNOTS('',3,(#53349,#53350,#53351,#53352,#53353,
#53354,#53355,#53356,#53357,#53358,#53359,#53360,#53361,#53362,#53363,#53364,
#53365,#53366,#53367,#53368,#53369,#53370,#53371,#53372,#53373,#53374,#53375,
#53376,#53377,#53378,#53379,#53380,#53381,#53382,#53383,#53384,#53385,#53386,
#53387,#53388,#53389,#53390,#53391,#53392,#53393,#53394,#53395,#53396,#53397,
#53398,#53399,#53400,#53401,#53402,#53403,#53404,#53405,#53406,#53407,#53408,
#53409,#53410,#53411,#53412,#53413,#53414,#53415,#53416,#53417,#53418,#53419,
#53420,#53421,#53422,#53423,#53424,#53425,#53426,#53427,#53428,#53429,#53430,
#53431,#53432,#53433,#53434,#53435,#53436,#53437,#53438,#53439,#53440,#53441,
#53442,#53443,#53444,#53445,#53446,#53447,#53448,#53449,#53450,#53451,#53452,
#53453,#53454,#53455,#53456,#53457,#53458,#53459,#53460,#53461,#53462,#53463,
#53464,#53465,#53466,#53467,#53468,#53469,#53470,#53471,#53472,#53473,#53474,
#53475,#53476,#53477,#53478,#53479,#53480,#53481,#53482,#53483,#53484,#53485,
#53486,#53487,#53488,#53489,#53490,#53491,#53492,#53493,#53494,#53495,#53496),
 .UNSPECIFIED.,.F.,.F.,(4,2,2,2,2,2,2,2,2,2,2,2,2,2,2,2,2,2,2,2,2,2,2,2,
2,2,2,2,2,2,2,2,2,2,2,2,2,2,2,2,2,2,2,2,2,2,2,2,2,2,2,2,2,2,2,2,2,2,2,2,
2,2,2,2,2,2,2,2,2,2,2,2,2,4),(-1.37994316952968,-1.37689311227225,-1.36682573652866,
-1.34228042207965,-1.33202475129869,-1.32313094817597,-1.31611795587767,
-1.30739915888195,-1.28345678192069,-1.26961972562278,-1.26086349964075,
-1.25645905792183,-1.25196785707959,-1.2426230896204,-1.22097924337118,
-1.2087485365401,-1.19879870812078,-1.19171700533154,-1.18367974843681,
-1.1651250047271,-1.14612917760861,-1.13877225267984,-1.13292305703663,
-1.12887646598579,-1.12323947896202,-1.10319838297259,-1.08670439419831,
-1.08108591203388,-1.07194741411961,-1.06492766049471,-1.05641623486836,
-1.03001574518196,-1.01736420210715,-1.00905268906645,-1.00471540075752,
-1.00014327199197,-0.990211241284662,-0.965107144749355,-0.954773421513134,
-0.94583592876078,-0.938822168802323,-0.930143076508692,-0.91133644834229,
-0.890012183713333,-0.882655960278845,-0.878459217734409,-0.873639573360281,
-0.862318089220826,-0.838779608238446,-0.828672057832893,-0.819861300618453,
-0.812847681281455,-0.804045278229529,-0.782707006762665,-0.767297417203463,
-0.760610652389874,-0.755136771563515,-0.751084486821065,-0.745045636921343,
-0.737339368803087,-0.716084657156016,-0.700217472411605,-0.692285062837235,
-0.685183498483941,-0.675005742963352,-0.66834101175725,-0.645395392510605,
-0.633855154214012,-0.628786809333242,-0.624674683771948,-0.617965940192248,
-0.613254767023967,-0.596707640675902,-0.578057800930158),.UNSPECIFIED.);
#648=B_SPLINE_CURVE_WITH_KNOTS('',3,(#53497,#53498,#53499,#53500,#53501,
#53502,#53503,#53504,#53505,#53506,#53507,#53508,#53509,#53510,#53511,#53512,
#53513,#53514,#53515,#53516,#53517,#53518,#53519,#53520,#53521,#53522,#53523,
#53524,#53525,#53526,#53527,#53528,#53529,#53530,#53531,#53532,#53533,#53534,
#53535,#53536,#53537,#53538,#53539,#53540,#53541,#53542,#53543,#53544,#53545,
#53546,#53547,#53548,#53549,#53550,#53551,#53552,#53553,#53554,#53555,#53556,
#53557,#53558,#53559,#53560,#53561,#53562,#53563,#53564,#53565,#53566,#53567,
#53568,#53569,#53570,#53571,#53572,#53573,#53574,#53575,#53576,#53577,#53578,
#53579,#53580,#53581,#53582,#53583,#53584,#53585,#53586,#53587,#53588,#53589,
#53590,#53591,#53592,#53593,#53594,#53595,#53596,#53597,#53598,#53599,#53600,
#53601,#53602,#53603,#53604,#53605,#53606,#53607,#53608,#53609,#53610,#53611,
#53612,#53613,#53614,#53615,#53616,#53617,#53618,#53619,#53620,#53621,#53622,
#53623,#53624,#53625,#53626,#53627,#53628,#53629,#53630,#53631,#53632,#53633,
#53634,#53635,#53636,#53637,#53638,#53639,#53640,#53641,#53642),
 .UNSPECIFIED.,.F.,.F.,(4,2,2,2,2,2,2,2,2,2,2,2,2,2,2,2,2,2,2,2,2,2,2,2,
2,2,2,2,2,2,2,2,2,2,2,2,2,2,2,2,2,2,2,2,2,2,2,2,2,2,2,2,2,2,2,2,2,2,2,2,
2,2,2,2,2,2,2,2,2,2,2,2,4),(-0.911920807669219,-0.90143765389995,-0.886745109987811,
-0.87905985210302,-0.871885995371558,-0.860765107176676,-0.834212388433582,
-0.824970278238165,-0.818140331658867,-0.814012239618955,-0.809013408073738,
-0.796547838803406,-0.774191110932913,-0.767613995717944,-0.757532710564437,
-0.750470423755175,-0.742567775145225,-0.725784833814838,-0.705083680534938,
-0.697460900871011,-0.691472842001079,-0.687435402051852,-0.682064717154924,
-0.659379246119088,-0.638518233901586,-0.629717651584906,-0.622695306396698,
-0.613856573362942,-0.603699302204386,-0.579837876380211,-0.569131574410963,
-0.564259621347492,-0.560074172934118,-0.552823844565205,-0.531588824368177,
-0.512603164050812,-0.503909708727391,-0.496894653818284,-0.487968840160277,
-0.477656051512273,-0.452752791453641,-0.442968809586499,-0.438234994374704,
-0.434001687320285,-0.426379261067704,-0.404707709530608,-0.386580270569894,
-0.377961326143986,-0.370950953858479,-0.361959900002634,-0.351525889175323,
-0.32570200703561,-0.316397229918055,-0.311913413010029,-0.307505901145109,
-0.298730296056676,-0.284840018172648,-0.261030113633416,-0.252304893487327,
-0.245290405886381,-0.236399180714257,-0.22614706440424,-0.201660461140628,
-0.191511997882101,-0.186716411225593,-0.18250846607308,-0.175076221179508,
-0.153660023347993,-0.135060083361694,-0.126397217303569,-0.119382399277055,
-0.110425404253977,-0.109945337718666),.UNSPECIFIED.);
#649=B_SPLINE_CURVE_WITH_KNOTS('',3,(#53648,#53649,#53650,#53651,#53652,
#53653,#53654,#53655,#53656,#53657,#53658,#53659,#53660,#53661,#53662,#53663,
#53664,#53665,#53666,#53667,#53668,#53669,#53670,#53671,#53672,#53673,#53674,
#53675,#53676,#53677,#53678,#53679,#53680,#53681,#53682,#53683,#53684,#53685,
#53686,#53687,#53688,#53689,#53690,#53691,#53692,#53693,#53694,#53695,#53696,
#53697,#53698,#53699,#53700,#53701,#53702,#53703,#53704,#53705,#53706,#53707,
#53708,#53709,#53710,#53711,#53712,#53713,#53714,#53715,#53716,#53717,#53718,
#53719,#53720,#53721,#53722,#53723,#53724,#53725,#53726,#53727,#53728,#53729,
#53730,#53731,#53732,#53733,#53734,#53735,#53736,#53737,#53738,#53739,#53740,
#53741,#53742,#53743,#53744,#53745,#53746,#53747,#53748,#53749,#53750,#53751,
#53752,#53753,#53754,#53755,#53756,#53757,#53758,#53759,#53760,#53761,#53762,
#53763,#53764,#53765,#53766,#53767,#53768,#53769,#53770,#53771,#53772,#53773,
#53774,#53775),.UNSPECIFIED.,.F.,.F.,(4,2,2,2,2,2,2,2,2,2,2,2,2,2,2,2,2,
2,2,2,2,2,2,2,2,2,2,2,2,2,2,2,2,2,2,2,2,2,2,2,2,2,2,2,2,2,2,2,2,2,2,2,2,
2,2,2,2,2,2,2,2,2,2,4),(-0.692748904775942,-0.676235309369303,-0.655372660470089,
-0.650315787459615,-0.646259718221949,-0.640812265724851,-0.634173194557436,
-0.618984651933166,-0.597360118129836,-0.588560296236878,-0.581547764742262,
-0.572737879990665,-0.562630022829078,-0.539120743771452,-0.527740193202501,
-0.522907197061913,-0.518716905154737,-0.511406980074506,-0.490157957161306,
-0.471257269792631,-0.4625702665497,-0.455555889274502,-0.446625224036467,
-0.436302467964124,-0.411315222304172,-0.401241893275841,-0.396650497196789,
-0.392325644017379,-0.384101172600747,-0.371673130043542,-0.344795779003007,
-0.336335971889365,-0.32931121992784,-0.320098782696567,-0.314408949318338,
-0.297552164027685,-0.278092449608793,-0.27244341390756,-0.268396189423533,
-0.262557550460827,-0.255221878535237,-0.236343058018277,-0.217665150549581,
-0.209627240224955,-0.20254426624099,-0.192592103284861,-0.180356641550837,
-0.158693095351688,-0.149324985386529,-0.144829869066863,-0.14042736650238,
-0.131688630949153,-0.117901398543954,-0.093898367928125,-0.0851856038670745,
-0.078170904286919,-0.0692664536942175,-0.0589912320322845,-0.0343493501421503,
-0.0243368999663489,-0.0195631100818421,-0.0157376569658423,-0.0113277168243253,
-0.000354962303461684),.UNSPECIFIED.);
#650=B_SPLINE_CURVE_WITH_KNOTS('',3,(#53776,#53777,#53778,#53779,#53780,
#53781,#53782,#53783,#53784,#53785,#53786,#53787,#53788,#53789,#53790,#53791,
#53792,#53793,#53794,#53795),.UNSPECIFIED.,.F.,.F.,(4,2,2,2,2,2,2,2,2,4),
(-1.48962364885331,-1.45799851151838,-1.44903501640883,-1.44202043222367,
-1.43336373572573,-1.41483556482368,-1.39335690597027,-1.38588751118161,
-1.38167498118498,-1.37994316952968),.UNSPECIFIED.);
#651=B_SPLINE_CURVE_WITH_KNOTS('',3,(#53797,#53798,#53799,#53800,#53801,
#53802,#53803,#53804,#53805,#53806,#53807,#53808,#53809,#53810,#53811,#53812,
#53813,#53814,#53815,#53816,#53817,#53818),.UNSPECIFIED.,.F.,.F.,(4,2,2,
2,2,2,2,2,2,2,4),(-0.109945337718666,-0.10005578303786,-0.0747324452225718,
-0.0649691927664568,-0.0604191866905936,-0.0560641058015071,-0.0476381350691081,
-0.0267483071399664,-0.00932637088096731,-0.00429109630289761,-0.000368170222445954),
 .UNSPECIFIED.);
#652=B_SPLINE_CURVE_WITH_KNOTS('',3,(#53819,#53820,#53821,#53822,#53823,
#53824,#53825,#53826,#53827,#53828,#53829,#53830,#53831,#53832,#53833,#53834,
#53835,#53836,#53837,#53838,#53839,#53840,#53841,#53842,#53843,#53844,#53845,
#53846,#53847,#53848,#53849,#53850,#53851,#53852,#53853,#53854,#53855,#53856,
#53857,#53858,#53859,#53860,#53861,#53862,#53863,#53864,#53865,#53866,#53867,
#53868,#53869,#53870,#53871,#53872,#53873,#53874,#53875,#53876,#53877,#53878,
#53879,#53880,#53881,#53882,#53883,#53884,#53885,#53886,#53887,#53888,#53889,
#53890,#53891,#53892,#53893,#53894,#53895,#53896,#53897,#53898,#53899,#53900,
#53901,#53902,#53903,#53904,#53905,#53906,#53907,#53908,#53909,#53910,#53911,
#53912,#53913,#53914,#53915,#53916,#53917,#53918,#53919,#53920,#53921,#53922,
#53923,#53924,#53925,#53926,#53927,#53928,#53929,#53930,#53931,#53932,#53933,
#53934,#53935,#53936,#53937,#53938,#53939,#53940,#53941,#53942),
 .UNSPECIFIED.,.F.,.F.,(4,2,2,2,2,2,2,2,2,2,2,2,2,2,2,2,2,2,2,2,2,2,2,2,
2,2,2,2,2,2,2,2,2,2,2,2,2,2,2,2,2,2,2,2,2,2,2,2,2,2,2,2,2,2,2,2,2,2,2,2,
2,4),(-1.60425228271969,-1.59886013992911,-1.59205050840229,-1.57668909305917,
-1.55163274571425,-1.54516388062916,-1.53981565161675,-1.53575173853546,
-1.52953672881361,-1.49971361789063,-1.48882279238098,-1.47957891257316,
-1.47255508515753,-1.46412392192429,-1.43695756392477,-1.42463775983764,
-1.41645729461622,-1.41214023795018,-1.4075422475674,-1.39740830220192,
-1.37252090057192,-1.3622183989205,-1.35329913441885,-1.34628765064055,
-1.33759730143691,-1.31863032565473,-1.29739385218365,-1.29010208755001,
-1.28591564218491,-1.28107972329177,-1.27063707299661,-1.24648612495446,
-1.23628861420684,-1.22742829918159,-1.22041800907575,-1.21167392727818,
-1.18819396703073,-1.17410960785412,-1.16526566989882,-1.16084904835453,
-1.15637469403923,-1.14714002177405,-1.12128598147573,-1.11085387246229,
-1.10186259577961,-1.09484992074297,-1.08622397677135,-1.0610803947368,
-1.04785444369528,-1.03932397932077,-1.03495446472101,-1.0304264937904,
-1.02115547325627,-0.999527691664109,-0.987315547425084,-0.977376206019699,
-0.97029781675934,-0.962260986410504,-0.943572063283242,-0.924684858362288,
-0.917347152536238,-0.911889189294514),.UNSPECIFIED.);
#653=B_SPLINE_CURVE_WITH_KNOTS('',3,(#53947,#53948,#53949,#53950,#53951,
#53952,#53953,#53954,#53955,#53956,#53957,#53958,#53959,#53960,#53961,#53962,
#53963,#53964,#53965,#53966,#53967,#53968,#53969,#53970,#53971,#53972,#53973,
#53974,#53975,#53976,#53977,#53978,#53979,#53980,#53981,#53982,#53983,#53984,
#53985,#53986,#53987,#53988,#53989,#53990,#53991,#53992,#53993,#53994,#53995,
#53996,#53997,#53998,#53999,#54000,#54001,#54002,#54003,#54004,#54005,#54006,
#54007,#54008,#54009,#54010,#54011,#54012,#54013,#54014,#54015,#54016,#54017,
#54018,#54019,#54020,#54021,#54022,#54023,#54024,#54025,#54026,#54027,#54028,
#54029,#54030,#54031,#54032,#54033,#54034,#54035,#54036,#54037,#54038,#54039,
#54040,#54041,#54042,#54043,#54044,#54045,#54046,#54047,#54048,#54049,#54050,
#54051,#54052,#54053,#54054,#54055,#54056,#54057,#54058,#54059,#54060,#54061,
#54062,#54063,#54064,#54065,#54066,#54067,#54068,#54069,#54070,#54071,#54072,
#54073,#54074,#54075,#54076,#54077,#54078,#54079,#54080,#54081,#54082,#54083,
#54084,#54085,#54086,#54087,#54088,#54089,#54090),.UNSPECIFIED.,.F.,.F.,
(4,2,2,2,2,2,2,2,2,2,2,2,2,2,2,2,2,2,2,2,2,2,2,2,2,2,2,2,2,2,2,2,2,2,2,
2,2,2,2,2,2,2,2,2,2,2,2,2,2,2,2,2,2,2,2,2,2,2,2,2,2,2,2,2,2,2,2,2,2,2,2,
4),(-1.49476463800755,-1.48836283425702,-1.47815618240204,-1.46928940850674,
-1.46227574437302,-1.45352914248273,-1.43002798940522,-1.41594785976451,
-1.40710406107762,-1.40268609286647,-1.39820862769885,-1.38896181796712,
-1.36311125633698,-1.35267711303315,-1.34368338708279,-1.33666748747283,
-1.32803561667801,-1.30291645266522,-1.2896715676271,-1.28113273027181,
-1.27676060817156,-1.27223100329919,-1.26295809711477,-1.24132188353044,
-1.22910655670356,-1.21916411766478,-1.21208258222925,-1.20404093868875,
-1.18522779054724,-1.16642677328903,-1.15910211910383,-1.15327044009174,
-1.14922358911303,-1.14356877698806,-1.12480200505867,-1.10141500565614,
-1.09228486896798,-1.08526435230261,-1.07674370509638,-1.05042155416237,
-1.03773291367076,-1.029406520026,-1.02506650580339,-1.02049633727313,-1.01058180054215,
-0.985458006045474,-0.975121199619371,-0.96618178387084,-0.959167407854628,
-0.950488622450764,-0.931694661572718,-0.910359596671632,-0.902996519478991,
-0.898798954452685,-0.893983371337442,-0.882678899523297,-0.85910920678493,
-0.848996118363765,-0.840182229711628,-0.833169552047423,-0.824373351557158,
-0.802189847399198,-0.781147227975423,-0.776102968175805,-0.772047802141666,
-0.766586745367916,-0.748623777043322,-0.722381009183814,-0.713858665508179,
-0.706906093943008,-0.69782471877296,-0.692748904775942),.UNSPECIFIED.);
#654=B_SPLINE_CURVE_WITH_KNOTS('',3,(#54091,#54092,#54093,#54094,#54095,
#54096,#54097,#54098,#54099,#54100,#54101,#54102,#54103,#54104,#54105,#54106,
#54107,#54108,#54109,#54110,#54111,#54112,#54113,#54114,#54115,#54116,#54117,
#54118,#54119,#54120,#54121,#54122,#54123,#54124,#54125,#54126,#54127,#54128,
#54129,#54130,#54131,#54132,#54133,#54134,#54135,#54136,#54137,#54138,#54139,
#54140,#54141,#54142,#54143,#54144,#54145,#54146,#54147,#54148,#54149,#54150,
#54151,#54152,#54153,#54154,#54155,#54156,#54157,#54158,#54159,#54160,#54161,
#54162,#54163,#54164,#54165,#54166,#54167,#54168,#54169,#54170,#54171,#54172,
#54173,#54174,#54175,#54176,#54177,#54178,#54179,#54180,#54181,#54182,#54183,
#54184,#54185,#54186,#54187,#54188,#54189,#54190,#54191,#54192,#54193,#54194,
#54195,#54196,#54197,#54198,#54199,#54200,#54201,#54202,#54203,#54204,#54205,
#54206,#54207,#54208,#54209,#54210,#54211,#54212,#54213,#54214,#54215,#54216,
#54217,#54218,#54219,#54220,#54221,#54222,#54223,#54224,#54225,#54226,#54227,
#54228,#54229,#54230,#54231,#54232),.UNSPECIFIED.,.F.,.F.,(4,2,2,2,2,2,
2,2,2,2,2,2,2,2,2,2,2,2,2,2,2,2,2,2,2,2,2,2,2,2,2,2,2,2,2,2,2,2,2,2,2,2,
2,2,2,2,2,2,2,2,2,2,2,2,2,2,2,2,2,2,2,2,2,2,2,2,2,2,2,2,4),(-0.911889189294514,
-0.911509021238188,-0.907463936454965,-0.901820872826992,-0.882103655125236,
-0.865432657612678,-0.859780367354239,-0.850607735719611,-0.843588278481432,
-0.835107194877428,-0.802257725779036,-0.789648542908412,-0.784638848655905,
-0.780511371089536,-0.77367121735012,-0.764396930434076,-0.737911044533359,
-0.726905439794408,-0.719774643262872,-0.712119822207256,-0.697483263531707,
-0.671707457677322,-0.662370562293857,-0.657880924998617,-0.653476747435654,
-0.644720012579152,-0.630880408782948,-0.60698447819079,-0.598267345681839,
-0.591255327990508,-0.582362763519045,-0.572107028998137,-0.547590577072453,
-0.537466800267108,-0.532676157949429,-0.528468360085987,-0.521031249194516,
-0.499609516124549,-0.481025527176616,-0.472364888537303,-0.465351039047699,
-0.456394174244022,-0.446023860311508,-0.420686670931562,-0.410942775532298,
-0.406395765569983,-0.402038832467301,-0.3935991511728,-0.380616214766329,
-0.354985428610164,-0.34640363022741,-0.340089024820618,-0.331461731902421,
-0.311556433860089,-0.287013662178649,-0.28176010244523,-0.277682212034723,
-0.271312588381915,-0.262979796614335,-0.236810207268542,-0.224616300761729,
-0.217259226853215,-0.209810514071386,-0.196906743140633,-0.17756139961699,
-0.162185110323441,-0.156490685368601,-0.15244452025261,-0.146655911311739,
-0.129475000774062,-0.109828012290715),.UNSPECIFIED.);
#655=B_SPLINE_CURVE_WITH_KNOTS('',3,(#54238,#54239,#54240,#54241,#54242,
#54243,#54244,#54245,#54246,#54247,#54248,#54249,#54250,#54251,#54252,#54253,
#54254,#54255,#54256,#54257,#54258,#54259,#54260,#54261,#54262,#54263,#54264,
#54265,#54266,#54267,#54268,#54269,#54270,#54271,#54272,#54273,#54274,#54275,
#54276,#54277,#54278,#54279,#54280,#54281,#54282,#54283,#54284,#54285,#54286,
#54287,#54288,#54289,#54290,#54291,#54292,#54293,#54294,#54295,#54296,#54297,
#54298,#54299,#54300,#54301,#54302,#54303,#54304,#54305,#54306,#54307,#54308,
#54309,#54310,#54311,#54312,#54313,#54314,#54315,#54316,#54317,#54318,#54319,
#54320,#54321,#54322,#54323,#54324,#54325,#54326,#54327,#54328,#54329,#54330,
#54331,#54332,#54333,#54334,#54335,#54336,#54337,#54338,#54339,#54340,#54341,
#54342,#54343,#54344,#54345,#54346,#54347,#54348,#54349,#54350,#54351,#54352,
#54353,#54354,#54355,#54356,#54357),.UNSPECIFIED.,.F.,.F.,(4,2,2,2,2,2,
2,2,2,2,2,2,2,2,2,2,2,2,2,2,2,2,2,2,2,2,2,2,2,2,2,2,2,2,2,2,2,2,2,2,2,2,
2,2,2,2,2,2,2,2,2,2,2,2,2,2,2,2,2,4),(-0.692980815119166,-0.685166320873275,
-0.680335305981931,-0.676143495922616,-0.668825199462455,-0.64756357223643,
-0.628679844563148,-0.619993388537569,-0.612978204666185,-0.604044878487092,
-0.593717982150457,-0.568706253487832,-0.558652593707495,-0.554063412592961,
-0.549736118811309,-0.541497731425997,-0.529035365321838,-0.502232072768898,
-0.493763353775518,-0.486738369859774,-0.477535834761316,-0.45764479787291,
-0.435017091219731,-0.429635808864119,-0.425580845449889,-0.419542627027357,
-0.411840026771538,-0.390626329152909,-0.374776344926731,-0.366816810972062,
-0.359713303272902,-0.349571500041958,-0.328261536242825,-0.309683941244289,
-0.304023235618637,-0.299975454537271,-0.294147216933534,-0.276605034792486,
-0.250865158023303,-0.242290923536331,-0.235338430058862,-0.226314935272215,
-0.215826701332353,-0.189606866256862,-0.180652720165412,-0.176217505888737,
-0.171755875055023,-0.162623290611988,-0.147709817722585,-0.12564556055034,
-0.116846925220763,-0.109831735811192,-0.101013975716215,-0.0908942254530899,
-0.067322851274371,-0.0559813973244607,-0.0511575166530446,-0.0469609964387052,
-0.0396151153015186,-0.000355547063539398),.UNSPECIFIED.);
#656=B_SPLINE_CURVE_WITH_KNOTS('',3,(#54358,#54359,#54360,#54361,#54362,
#54363,#54364,#54365,#54366,#54367,#54368,#54369,#54370,#54371,#54372,#54373,
#54374,#54375,#54376,#54377,#54378,#54379,#54380,#54381),.UNSPECIFIED.,
 .F.,.F.,(4,2,2,2,2,2,2,2,2,2,2,4),(-1.60439037716061,-1.59945122675283,
-1.59462474263139,-1.58821321942477,-1.57953987078498,-1.56057235854575,
-1.53930317729267,-1.53198957109054,-1.5277986145673,-1.52296607692686,
-1.51256007779002,-1.49476463800755),.UNSPECIFIED.);
#657=B_SPLINE_CURVE_WITH_KNOTS('',3,(#54383,#54384,#54385,#54386,#54387,
#54388,#54389,#54390,#54391,#54392,#54393,#54394,#54395,#54396,#54397,#54398,
#54399,#54400,#54401,#54402,#54403,#54404,#54405,#54406),.UNSPECIFIED.,
 .F.,.F.,(4,2,2,2,2,2,2,2,2,2,2,4),(-0.109828012290715,-0.103125880268508,
-0.0946120250454899,-0.0875913270661589,-0.078453506773865,-0.0550782175137834,
-0.0362647231901379,-0.0306079282228981,-0.0265611633896067,-0.0224960035305987,
-0.0162949183073028,-0.0003552119044235),.UNSPECIFIED.);
#658=B_SPLINE_CURVE_WITH_KNOTS('',3,(#54407,#54408,#54409,#54410,#54411,
#54412,#54413,#54414,#54415,#54416,#54417,#54418,#54419,#54420,#54421,#54422,
#54423,#54424,#54425,#54426,#54427,#54428,#54429,#54430,#54431,#54432,#54433,
#54434,#54435,#54436,#54437,#54438,#54439,#54440,#54441,#54442,#54443,#54444,
#54445,#54446,#54447,#54448,#54449,#54450,#54451,#54452,#54453,#54454,#54455,
#54456,#54457,#54458,#54459,#54460,#54461,#54462,#54463,#54464,#54465,#54466,
#54467,#54468,#54469,#54470,#54471,#54472,#54473,#54474,#54475,#54476,#54477,
#54478,#54479,#54480,#54481,#54482,#54483,#54484,#54485,#54486,#54487,#54488,
#54489,#54490,#54491,#54492,#54493,#54494,#54495,#54496,#54497,#54498,#54499,
#54500,#54501,#54502,#54503,#54504,#54505,#54506,#54507,#54508,#54509,#54510,
#54511,#54512,#54513,#54514,#54515,#54516,#54517,#54518,#54519,#54520,#54521,
#54522,#54523,#54524,#54525,#54526,#54527,#54528,#54529,#54530),
 .UNSPECIFIED.,.F.,.F.,(4,2,2,2,2,2,2,2,2,2,2,2,2,2,2,2,2,2,2,2,2,2,2,2,
2,2,2,2,2,2,2,2,2,2,2,2,2,2,2,2,2,2,2,2,2,2,2,2,2,2,2,2,2,2,2,2,2,2,2,2,
2,4),(-1.60450853446915,-1.58099180905865,-1.5741640089589,-1.56713939792466,
-1.55871752412026,-1.53174949229508,-1.51928866589299,-1.51105219965776,
-1.50672667142175,-1.50214046897003,-1.49209775827369,-1.46711358423613,
-1.45679739873521,-1.44787035341194,-1.44085844057041,-1.43217440865226,
-1.4132911845589,-1.39200871903329,-1.38468329509778,-1.38049199984088,
-1.37566688158213,-1.36530537971552,-1.34107119888107,-1.33086132124443,
-1.32199392559381,-1.31498323409782,-1.30624502641982,-1.28265190155576,
-1.2686288158881,-1.25980651665391,-1.25539298921942,-1.25091490543891,
-1.24165527928765,-1.21582764234192,-1.20539870632091,-1.19640907337983,
-1.18939619545903,-1.18076825971048,-1.15564300664585,-1.14240712476105,
-1.13387279165151,-1.12950258089611,-1.12497509223292,-1.11570809322809,
-1.09407805023255,-1.0818629800975,-1.07192199681267,-1.064843194393,-1.05680658619747,
-1.03815591414222,-1.01923797676905,-1.01189493822598,-1.0060538044972,
-1.00200849647931,-0.996367710829674,-0.976494308524129,-0.959911348274805,
-0.954275992030018,-0.945120733533117,-0.93810181209856,-0.929607066178783,
-0.912048462349294),.UNSPECIFIED.);
#659=B_SPLINE_CURVE_WITH_KNOTS('',3,(#54535,#54536,#54537,#54538,#54539,
#54540,#54541,#54542,#54543,#54544,#54545,#54546,#54547,#54548,#54549,#54550,
#54551,#54552,#54553,#54554,#54555,#54556,#54557,#54558,#54559,#54560,#54561,
#54562,#54563,#54564,#54565,#54566,#54567,#54568,#54569,#54570,#54571,#54572,
#54573,#54574,#54575,#54576,#54577,#54578,#54579,#54580,#54581,#54582,#54583,
#54584,#54585,#54586,#54587,#54588,#54589,#54590,#54591,#54592,#54593,#54594,
#54595,#54596,#54597,#54598,#54599,#54600,#54601,#54602,#54603,#54604,#54605,
#54606,#54607,#54608,#54609,#54610,#54611,#54612,#54613,#54614,#54615,#54616,
#54617,#54618,#54619,#54620,#54621,#54622,#54623,#54624,#54625,#54626,#54627,
#54628,#54629,#54630,#54631,#54632,#54633,#54634,#54635,#54636,#54637,#54638,
#54639,#54640,#54641,#54642,#54643,#54644,#54645,#54646,#54647,#54648,#54649,
#54650,#54651,#54652,#54653,#54654,#54655,#54656,#54657,#54658,#54659,#54660,
#54661,#54662,#54663,#54664,#54665,#54666,#54667,#54668,#54669,#54670,#54671,
#54672,#54673,#54674),.UNSPECIFIED.,.F.,.F.,(4,2,2,2,2,2,2,2,2,2,2,2,2,
2,2,2,2,2,2,2,2,2,2,2,2,2,2,2,2,2,2,2,2,2,2,2,2,2,2,2,2,2,2,2,2,2,2,2,2,
2,2,2,2,2,2,2,2,2,2,2,2,2,2,2,2,2,2,2,2,4),(-1.49497804194698,-1.49377195464921,
-1.48497036929973,-1.46340995305725,-1.44815265604888,-1.43890686622161,
-1.43443033816667,-1.43001345969881,-1.42117329002966,-1.39486737521192,
-1.3843759126987,-1.37535090415026,-1.36840089454909,-1.35983388144816,
-1.33401215177245,-1.31650686283038,-1.31068343962577,-1.30663722384223,
-1.30097604987968,-1.27613725998678,-1.26233461622457,-1.25162005754253,
-1.2444531036937,-1.23669429453869,-1.22108752706174,-1.1990978895747,-1.19128289441049,
-1.18518602246255,-1.18112926827002,-1.17579428831105,-1.14908934226767,
-1.13410421406953,-1.12453803673063,-1.11749152266626,-1.10926230799779,
-1.09293905901445,-1.07275516995505,-1.06520694413741,-1.0592535652122,
-1.05520400211965,-1.04976145591368,-1.02211595613978,-1.00876845741215,
-0.999004378077605,-0.991941117995587,-0.983817616971652,-0.953869524717951,
-0.937524458148364,-0.932408008225162,-0.928305601361065,-0.921687567099786,
-0.893160517076821,-0.882040654014953,-0.872672211123954,-0.865639450498399,
-0.857288980716925,-0.829358768559797,-0.811815809226221,-0.806655485712711,
-0.802561595530425,-0.796026524242121,-0.791496544735808,-0.776054627069269,
-0.754798161548612,-0.7459983635543,-0.738985060043492,-0.730173211738306,
-0.720062477091776,-0.696539000238583,-0.692980815119166),.UNSPECIFIED.);
#660=B_SPLINE_CURVE_WITH_KNOTS('',3,(#54675,#54676,#54677,#54678,#54679,
#54680,#54681,#54682,#54683,#54684,#54685,#54686,#54687,#54688,#54689,#54690,
#54691,#54692,#54693,#54694,#54695,#54696,#54697,#54698,#54699,#54700,#54701,
#54702,#54703,#54704,#54705,#54706,#54707,#54708,#54709,#54710,#54711,#54712,
#54713,#54714,#54715,#54716,#54717,#54718,#54719,#54720,#54721,#54722,#54723,
#54724,#54725,#54726,#54727,#54728,#54729,#54730,#54731,#54732,#54733,#54734,
#54735,#54736,#54737,#54738,#54739,#54740,#54741,#54742,#54743,#54744,#54745,
#54746,#54747,#54748,#54749,#54750,#54751,#54752,#54753,#54754,#54755,#54756,
#54757,#54758,#54759,#54760,#54761,#54762,#54763,#54764,#54765,#54766,#54767,
#54768,#54769,#54770,#54771,#54772,#54773,#54774,#54775,#54776,#54777,#54778,
#54779,#54780,#54781,#54782,#54783,#54784,#54785,#54786,#54787,#54788,#54789,
#54790,#54791,#54792,#54793,#54794,#54795,#54796,#54797,#54798,#54799,#54800,
#54801,#54802,#54803,#54804,#54805,#54806,#54807,#54808,#54809,#54810,#54811,
#54812,#54813,#54814,#54815,#54816,#54817,#54818,#54819,#54820,#54821,#54822),
 .UNSPECIFIED.,.F.,.F.,(4,2,2,2,2,2,2,2,2,2,2,2,2,2,2,2,2,2,2,2,2,2,2,2,
2,2,2,2,2,2,2,2,2,2,2,2,2,2,2,2,2,2,2,2,2,2,2,2,2,2,2,2,2,2,2,2,2,2,2,2,
2,2,2,2,2,2,2,2,2,2,2,2,2,4),(-0.912048462349294,-0.896787479541693,-0.887787252805348,
-0.881082056421924,-0.876970859194697,-0.87189978055317,-0.857601215483016,
-0.836619391417323,-0.826932624675712,-0.818361431293804,-0.811346248886324,
-0.802444281552055,-0.779149796069077,-0.759910889932576,-0.754261356548292,
-0.750215936334087,-0.744383568476121,-0.737058159169312,-0.718232648422221,
-0.699495194346949,-0.691459240057477,-0.684379613022506,-0.674435557334175,
-0.662213489616615,-0.640563554921123,-0.631282436702651,-0.626752510710786,
-0.622383498123253,-0.613859410053045,-0.600651412044106,-0.575508713103071,
-0.566885983404994,-0.559872175480125,-0.550874529020405,-0.54043000366026,
-0.514524808438672,-0.50530430098736,-0.500831460454452,-0.496411887490613,
-0.487552143587483,-0.473424108760431,-0.450057615849071,-0.44130968428607,
-0.434298088548766,-0.42543841115686,-0.415241315385748,-0.391130823378256,
-0.380611376633401,-0.375764561833978,-0.371581111540397,-0.364316991885263,
-0.343096210635845,-0.324106430740163,-0.315413171261473,-0.308400108134927,
-0.299479880692613,-0.289175185267792,-0.264315597332995,-0.254503511936039,
-0.249764492364517,-0.245530918965283,-0.237917195827653,-0.216255864773591,
-0.198101576875409,-0.189476678412823,-0.182461121057872,-0.173461239424339,
-0.163014121479963,-0.137102459672032,-0.127879756796657,-0.12340582189053,
-0.118985177997877,-0.110123264679583,-0.110052644177883),.UNSPECIFIED.);
#661=B_SPLINE_CURVE_WITH_KNOTS('',3,(#54828,#54829,#54830,#54831,#54832,
#54833,#54834,#54835,#54836,#54837,#54838,#54839,#54840,#54841,#54842,#54843,
#54844,#54845,#54846,#54847,#54848,#54849,#54850,#54851,#54852,#54853,#54854,
#54855,#54856,#54857,#54858,#54859,#54860,#54861,#54862,#54863,#54864,#54865,
#54866,#54867,#54868,#54869,#54870,#54871,#54872,#54873,#54874,#54875,#54876,
#54877,#54878,#54879,#54880,#54881,#54882,#54883,#54884,#54885,#54886,#54887,
#54888,#54889,#54890,#54891,#54892,#54893,#54894,#54895,#54896,#54897,#54898,
#54899,#54900,#54901,#54902,#54903,#54904,#54905,#54906,#54907,#54908,#54909,
#54910,#54911,#54912,#54913,#54914,#54915,#54916,#54917,#54918,#54919,#54920,
#54921,#54922,#54923,#54924,#54925,#54926,#54927,#54928,#54929,#54930,#54931,
#54932,#54933,#54934,#54935,#54936,#54937,#54938,#54939,#54940,#54941,#54942,
#54943,#54944,#54945,#54946,#54947,#54948,#54949),.UNSPECIFIED.,.F.,.F.,
(4,2,2,2,2,2,2,2,2,2,2,2,2,2,2,2,2,2,2,2,2,2,2,2,2,2,2,2,2,2,2,2,2,2,2,
2,2,2,2,2,2,2,2,2,2,2,2,2,2,2,2,2,2,2,2,2,2,2,2,2,4),(-0.692979258838884,
-0.67118995559551,-0.660866191665037,-0.651947318622327,-0.644970789635518,
-0.636378600644057,-0.60727614293275,-0.591512805470871,-0.586376026649255,
-0.582294060180516,-0.575795283599456,-0.553673671159206,-0.534265136420348,
-0.525531505302177,-0.518506056740535,-0.509590314510271,-0.499297170215878,
-0.474501837439696,-0.464694785347564,-0.459951122221414,-0.455704806824037,
-0.448031472572048,-0.425570280093862,-0.406534368994663,-0.398490632978779,
-0.391405509701558,-0.38145487535463,-0.369225695848239,-0.347565766891165,
-0.338273844980115,-0.333740773740727,-0.329373350516715,-0.32085914220195,
-0.307678112406119,-0.282468280722237,-0.273850874445708,-0.266838378502827,
-0.257839628417611,-0.24739307469677,-0.221482207085166,-0.212252537828199,
-0.207778796289508,-0.203359391533404,-0.194509561142105,-0.180413163659739,
-0.156976605719048,-0.14822795622256,-0.141211741118464,-0.132339867458766,
-0.122123580196769,-0.0978938520951423,-0.0874944227269537,-0.0826613397690077,
-0.0784679677917035,-0.071145027051044,-0.049875874748182,-0.0292982719334265,
-0.021178040717596,-0.0143023234670417,-0.00788979083151709,-0.000367801731532991),
 .UNSPECIFIED.);
#662=B_SPLINE_CURVE_WITH_KNOTS('',3,(#54950,#54951,#54952,#54953,#54954,
#54955,#54956,#54957,#54958,#54959,#54960,#54961,#54962,#54963,#54964,#54965,
#54966,#54967,#54968,#54969),.UNSPECIFIED.,.F.,.F.,(4,2,2,2,2,2,2,2,2,4),
(-1.60445172345304,-1.57087287035435,-1.56356495273178,-1.55937554915346,
-1.55454319912385,-1.54316751778459,-1.51968740073871,-1.5095887286719,
-1.50078343146496,-1.49497804194698),.UNSPECIFIED.);
#663=B_SPLINE_CURVE_WITH_KNOTS('',3,(#54971,#54972,#54973,#54974,#54975,
#54976,#54977,#54978,#54979,#54980,#54981,#54982,#54983,#54984,#54985,#54986,
#54987,#54988,#54989,#54990),.UNSPECIFIED.,.F.,.F.,(4,2,2,2,2,2,2,2,2,4),
(-0.110052644177883,-0.0959917623713727,-0.0726194674722937,-0.0638694112349162,
-0.0568561358282353,-0.0479943818297274,-0.037794935835177,-0.0146164749566909,
-0.00527669761352651,-0.000466613313815364),.UNSPECIFIED.);
#664=B_SPLINE_CURVE_WITH_KNOTS('',3,(#54991,#54992,#54993,#54994,#54995,
#54996,#54997,#54998,#54999,#55000,#55001,#55002,#55003,#55004,#55005,#55006,
#55007,#55008,#55009,#55010,#55011,#55012,#55013,#55014,#55015,#55016,#55017,
#55018,#55019,#55020,#55021,#55022,#55023,#55024,#55025,#55026,#55027,#55028,
#55029,#55030,#55031,#55032,#55033,#55034,#55035,#55036,#55037,#55038,#55039,
#55040,#55041,#55042,#55043,#55044,#55045,#55046,#55047,#55048,#55049,#55050,
#55051,#55052,#55053,#55054,#55055,#55056,#55057,#55058,#55059,#55060,#55061,
#55062,#55063,#55064,#55065,#55066,#55067,#55068,#55069,#55070,#55071,#55072,
#55073,#55074,#55075,#55076,#55077,#55078,#55079,#55080,#55081,#55082,#55083,
#55084,#55085,#55086,#55087,#55088,#55089,#55090,#55091,#55092,#55093,#55094,
#55095,#55096,#55097,#55098,#55099,#55100,#55101,#55102,#55103,#55104,#55105,
#55106,#55107,#55108,#55109,#55110,#55111,#55112),.UNSPECIFIED.,.F.,.F.,
(4,2,2,2,2,2,2,2,2,2,2,2,2,2,2,2,2,2,2,2,2,2,2,2,2,2,2,2,2,2,2,2,2,2,2,
2,2,2,2,2,2,2,2,2,2,2,2,2,2,2,2,2,2,2,2,2,2,2,2,2,4),(0.692945632510061,
0.701098988438348,0.725132570721244,0.745998105385564,0.751049440209536,
0.75510289302239,0.760547994319789,0.779389231545661,0.804529776262318,
0.813157989608204,0.820172689985033,0.829167560916291,0.839605347779739,
0.865502248436985,0.87469308324559,0.879162020220886,0.883586501275583,
0.892480291136297,0.906704758420185,0.929935863909063,0.938693251348128,
0.945703972588875,0.954551776009108,0.964726465256555,0.988716782702821,
0.999327278601534,1.00418418488939,1.008362128598,1.01559230609395,1.03687743233692,
1.05589371707847,1.06458793006142,1.07159922945832,1.08051378430896,1.09080779966496,
1.11563242884667,1.12544384119935,1.1301820351341,1.13441431598638,1.1420247916423,
1.16369368387706,1.18187472676576,1.19050111867402,1.19751519322408,1.20650973554747,
1.21694670810894,1.24282929574475,1.25204297954118,1.25651490592208,1.26093552223229,
1.26980250123599,1.28395001924971,1.307324402572,1.31607576538116,1.32308720435612,
1.33194298256497,1.35611708796313,1.37454359712428,1.38020969133085,1.38295740097097,
1.38531635665395),.UNSPECIFIED.);
#665=B_SPLINE_CURVE_WITH_KNOTS('',3,(#55116,#55117,#55118,#55119,#55120,
#55121,#55122,#55123,#55124,#55125,#55126,#55127,#55128,#55129,#55130,#55131,
#55132,#55133,#55134,#55135,#55136,#55137,#55138,#55139,#55140,#55141,#55142,
#55143,#55144,#55145,#55146,#55147,#55148,#55149,#55150,#55151,#55152,#55153,
#55154,#55155,#55156,#55157,#55158,#55159,#55160,#55161,#55162,#55163,#55164,
#55165,#55166,#55167,#55168,#55169,#55170,#55171,#55172,#55173),
 .UNSPECIFIED.,.F.,.F.,(4,3,3,3,3,3,3,3,3,3,3,3,3,3,3,3,3,3,3,4),(-4.04123713824997,
-3.94225244711282,-3.83273628999188,-3.72323042065973,-3.61400708733206,
-3.50484939767286,-3.39571794529748,-3.28596079280676,-3.17669944235086,
-3.06669438884274,-2.95668933533462,-2.84758449988576,-2.73866222057574,
-2.62984168483314,-2.52108273415307,-2.41234529469343,-2.30351145552693,
-2.19463277712453,-2.08555027678977,-1.98505081481724),.UNSPECIFIED.);
#666=B_SPLINE_CURVE_WITH_KNOTS('',3,(#55177,#55178,#55179,#55180,#55181),
 .UNSPECIFIED.,.F.,.F.,(4,1,4),(0.,0.985563111778209,1.08537753955771),
 .UNSPECIFIED.);
#667=B_SPLINE_CURVE_WITH_KNOTS('',3,(#55183,#55184,#55185,#55186,#55187,
#55188,#55189,#55190,#55191,#55192,#55193,#55194,#55195,#55196,#55197,#55198,
#55199,#55200,#55201,#55202,#55203,#55204,#55205,#55206,#55207,#55208,#55209,
#55210,#55211,#55212,#55213,#55214,#55215,#55216,#55217,#55218,#55219,#55220,
#55221,#55222,#55223,#55224,#55225,#55226,#55227,#55228,#55229,#55230,#55231,
#55232,#55233,#55234,#55235,#55236,#55237,#55238,#55239,#55240,#55241,#55242,
#55243,#55244,#55245,#55246,#55247,#55248,#55249,#55250,#55251,#55252,#55253,
#55254,#55255,#55256,#55257,#55258,#55259,#55260,#55261,#55262,#55263,#55264,
#55265,#55266,#55267,#55268,#55269,#55270,#55271,#55272,#55273,#55274,#55275,
#55276,#55277,#55278,#55279,#55280,#55281,#55282,#55283,#55284,#55285,#55286,
#55287,#55288,#55289,#55290,#55291,#55292,#55293,#55294,#55295,#55296,#55297,
#55298,#55299,#55300,#55301,#55302,#55303,#55304,#55305,#55306,#55307,#55308,
#55309,#55310,#55311,#55312,#55313,#55314,#55315,#55316,#55317,#55318,#55319,
#55320,#55321,#55322,#55323,#55324,#55325,#55326,#55327,#55328,#55329,#55330,
#55331,#55332,#55333,#55334,#55335,#55336,#55337,#55338,#55339,#55340,#55341,
#55342,#55343,#55344,#55345,#55346,#55347,#55348,#55349,#55350,#55351,#55352,
#55353,#55354,#55355,#55356,#55357),.UNSPECIFIED.,.F.,.F.,(4,3,3,3,3,3,
3,3,3,3,3,3,3,3,3,3,3,3,3,3,3,3,3,3,3,3,3,3,3,3,3,3,3,3,3,3,3,3,3,3,3,3,
3,3,3,3,3,3,3,3,3,3,3,3,3,3,3,3,4),(1.08537753955771,1.19609612505755,1.30308901533939,
1.40999021783501,1.51684224978507,1.62368754240906,1.73063567937683,1.83764628072714,
1.94483380370644,1.97112622355641,2.08051853033858,2.19003988096308,2.29913778678197,
2.40816980702691,2.51717555233518,2.62705399808504,2.73619094067904,2.84644013800683,
2.95668933533462,3.06618855596474,3.17569654235825,3.28491288691593,3.39406733753621,
3.50319929489951,3.61296258295283,3.72223356492953,3.83224300602117,3.94225244711282,
4.05148995552414,4.161030655945,4.26997382470323,4.37885158765571,4.48770382649441,
4.59773175959356,4.70671885335743,4.81726720612423,4.92781555889103,5.03716800382292,
5.14669433717871,5.25575579897979,5.3647527746709,5.47372494165427,5.58363837390801,
5.69274576144384,5.80306221605654,5.91337867066923,6.02273158896768,6.13225786315265,
6.24132068816919,6.3503193589255,6.45929355088761,6.56920560877757,6.67831581327472,
6.78862879786108,6.89894178244744,7.01634704840949,7.13200788731664,7.25028536680614,
7.36856284629564),.UNSPECIFIED.);
#668=B_SPLINE_CURVE_WITH_KNOTS('',3,(#55359,#55360,#55361,#55362,#55363,
#55364,#55365,#55366,#55367,#55368,#55369,#55370,#55371,#55372,#55373,#55374,
#55375,#55376,#55377,#55378,#55379,#55380,#55381,#55382,#55383,#55384,#55385,
#55386,#55387,#55388,#55389,#55390,#55391,#55392,#55393,#55394,#55395,#55396,
#55397,#55398,#55399,#55400,#55401,#55402,#55403,#55404,#55405,#55406,#55407,
#55408,#55409,#55410,#55411,#55412,#55413,#55414,#55415,#55416,#55417,#55418,
#55419,#55420,#55421,#55422,#55423,#55424,#55425,#55426,#55427,#55428,#55429,
#55430,#55431,#55432,#55433,#55434,#55435,#55436,#55437,#55438,#55439,#55440,
#55441,#55442,#55443,#55444,#55445,#55446,#55447,#55448,#55449,#55450,#55451,
#55452,#55453,#55454,#55455,#55456,#55457,#55458,#55459,#55460,#55461,#55462,
#55463,#55464,#55465,#55466,#55467,#55468,#55469,#55470,#55471,#55472,#55473,
#55474,#55475,#55476,#55477,#55478,#55479,#55480,#55481,#55482,#55483,#55484,
#55485,#55486,#55487,#55488,#55489,#55490,#55491,#55492,#55493,#55494,#55495,
#55496,#55497,#55498,#55499,#55500,#55501,#55502,#55503,#55504,#55505,#55506,
#55507,#55508,#55509,#55510,#55511,#55512,#55513,#55514,#55515,#55516,#55517,
#55518,#55519,#55520,#55521,#55522,#55523,#55524,#55525,#55526,#55527,#55528,
#55529,#55530,#55531,#55532,#55533),.UNSPECIFIED.,.F.,.F.,(4,3,3,3,3,3,
3,3,3,3,3,3,3,3,3,3,3,3,3,3,3,3,3,3,3,3,3,3,3,3,3,3,3,3,3,3,3,3,3,3,3,3,
3,3,3,3,3,3,3,3,3,3,3,3,3,3,3,3,4),(7.3685628467373,7.48153885872925,7.59477484966834,
7.7081490758396,7.82180510018963,7.88450489422564,7.9938449101036,8.10337279709113,
8.21242191116621,8.3214066065219,8.43036658246054,8.54029193834637,8.6493874997913,
8.75972775289758,8.87006800600385,8.97940661138203,9.08893467468203,9.19798242504892,
9.30696577840231,9.41592443647842,9.52585110680433,9.63494542566003,9.74528827172105,
9.85563111778206,9.96496690329824,10.074495319081,10.183540107565,10.2925204542086,
10.4014760658998,10.5114056068149,10.6204968171082,10.7308455233342,10.8411942295603,
10.9505318783152,11.0600600611931,11.1691067785061,11.2780890730194,11.387046648252,
11.4969743215237,11.6060675109473,11.7164124261429,11.8267573413385,11.9360946581711,
12.0456228825393,12.1546692664882,12.2636512280816,12.3726084714257,12.4825364668485,
12.5916293308537,12.7019748919852,12.8123204531167,12.9200463210862,13.0276280771467,
13.1351078843213,13.2425277495154,13.3499863415123,13.4574600064483,13.5650841670389,
13.6517481535604),.UNSPECIFIED.);
#669=B_SPLINE_CURVE_WITH_KNOTS('',3,(#55535,#55536,#55537,#55538,#55539,
#55540,#55541,#55542,#55543,#55544,#55545,#55546,#55547,#55548,#55549,#55550,
#55551,#55552,#55553,#55554,#55555,#55556,#55557,#55558,#55559,#55560,#55561,
#55562,#55563,#55564,#55565,#55566,#55567,#55568,#55569,#55570,#55571,#55572,
#55573,#55574,#55575,#55576,#55577,#55578,#55579,#55580,#55581,#55582,#55583,
#55584,#55585,#55586,#55587,#55588,#55589,#55590,#55591,#55592,#55593,#55594,
#55595,#55596,#55597,#55598,#55599,#55600,#55601,#55602,#55603,#55604,#55605,
#55606,#55607,#55608,#55609,#55610,#55611,#55612,#55613,#55614,#55615,#55616,
#55617,#55618,#55619,#55620,#55621,#55622,#55623,#55624,#55625,#55626,#55627,
#55628,#55629,#55630,#55631,#55632,#55633,#55634,#55635,#55636,#55637,#55638,
#55639,#55640,#55641,#55642,#55643,#55644,#55645,#55646,#55647,#55648,#55649,
#55650,#55651,#55652,#55653,#55654,#55655,#55656,#55657,#55658,#55659,#55660,
#55661,#55662,#55663,#55664,#55665,#55666,#55667,#55668,#55669,#55670,#55671,
#55672,#55673,#55674,#55675,#55676,#55677,#55678,#55679,#55680,#55681,#55682,
#55683,#55684,#55685,#55686,#55687,#55688,#55689,#55690,#55691,#55692,#55693,
#55694,#55695,#55696,#55697,#55698,#55699,#55700,#55701,#55702,#55703,#55704,
#55705,#55706),.UNSPECIFIED.,.F.,.F.,(4,3,3,3,3,3,3,3,3,3,3,3,3,3,3,3,3,
3,3,3,3,3,3,3,3,3,3,3,3,3,3,3,3,3,3,3,3,3,3,3,3,3,3,3,3,3,3,3,3,3,3,3,3,
3,3,3,3,4),(13.6517481539169,13.7978835648949,13.9072208386646,14.0167490684156,
14.1257954027862,14.2347773124886,14.3437345017137,14.4536625454536,14.5627553504665,
14.6731010135698,14.7834466766731,14.8927838932927,15.0023121301875,15.1113584064312,
15.2203402578103,15.3292973886179,15.4392254885762,15.5483182356278,15.6586640120395,
15.7690097884513,15.8783469822886,15.9878752220312,16.0969214740007,16.2059033006146,
16.3148604062078,16.4247885297132,16.5338812507372,16.6442270754833,16.7545729002295,
16.8639101200874,16.9734383565774,17.0824846356086,17.1914664895968,17.3004236228299,
17.4103517201243,17.5194444691187,17.6297902405632,17.7401360120077,17.8494732232515,
17.9590014608183,18.06804773103,18.1770295761472,18.2859867004733,18.3959148063015,
18.5050075464051,18.6153533350955,18.7256991237859,18.8350363334543,18.944564571218,
19.0536108397158,19.1625926830721,19.271549805593,19.3814779130857,19.4905706512962,
19.6009164434301,19.7112622355641,19.8572147419281,19.9349334610965),
 .UNSPECIFIED.);
#670=B_SPLINE_CURVE_WITH_KNOTS('',3,(#55708,#55709,#55710,#55711,#55712,
#55713,#55714,#55715,#55716,#55717,#55718,#55719,#55720,#55721,#55722,#55723,
#55724,#55725,#55726,#55727,#55728,#55729,#55730,#55731,#55732,#55733,#55734,
#55735,#55736,#55737,#55738,#55739,#55740,#55741,#55742,#55743,#55744,#55745,
#55746,#55747,#55748,#55749,#55750,#55751,#55752,#55753,#55754,#55755,#55756,
#55757,#55758,#55759,#55760,#55761,#55762,#55763,#55764,#55765,#55766,#55767,
#55768,#55769,#55770,#55771,#55772,#55773,#55774,#55775,#55776,#55777,#55778,
#55779,#55780,#55781,#55782,#55783,#55784,#55785,#55786,#55787,#55788,#55789,
#55790,#55791,#55792,#55793,#55794,#55795,#55796,#55797,#55798,#55799,#55800,
#55801,#55802,#55803,#55804,#55805,#55806,#55807,#55808,#55809,#55810,#55811,
#55812,#55813,#55814,#55815,#55816,#55817,#55818,#55819,#55820,#55821,#55822,
#55823,#55824,#55825,#55826,#55827,#55828,#55829,#55830,#55831,#55832,#55833,
#55834,#55835,#55836,#55837,#55838,#55839,#55840,#55841,#55842,#55843,#55844,
#55845,#55846,#55847,#55848,#55849,#55850,#55851,#55852,#55853,#55854,#55855,
#55856,#55857,#55858,#55859,#55860,#55861,#55862,#55863,#55864,#55865,#55866,
#55867,#55868,#55869,#55870,#55871,#55872,#55873,#55874,#55875,#55876,#55877,
#55878,#55879,#55880,#55881,#55882),.UNSPECIFIED.,.F.,.F.,(4,3,3,3,3,3,
3,3,3,3,3,3,3,3,3,3,3,3,3,3,3,3,3,3,3,3,3,3,3,3,3,3,3,3,3,3,3,3,3,3,3,3,
3,3,3,3,3,3,3,3,3,3,3,3,3,3,3,3,4),(19.9349334614217,20.0426247475374,20.15023541793,
20.2578072367367,20.3675617643881,20.4752466720914,20.5860360097169,20.6968253473423,
20.8061625587225,20.9156907962723,21.0247370665719,21.1337189117587,21.2426760361357,
21.3526041418819,21.4616968819895,21.572042670555,21.6823884591205,21.7917256704712,
21.9012539080246,22.0103001782835,22.1192820234254,22.2282391477534,22.3381672535397,
22.4472599935889,22.5576057822438,22.6679515708987,22.7772887825285,22.886817020047,
22.9958632905997,23.10484513604,23.2138022606707,23.3237303661722,23.4328231065306,
23.5431688946038,23.6535146826769,23.7628518941414,23.8723801316806,23.9814264020619,
24.0904082473291,24.1993653717851,24.3092934774526,24.4183862176348,24.5287320060449,
24.6390777944551,24.7484150060951,24.8579432436124,24.9669895141692,25.0759713596114,
25.1849284842416,25.2948565897395,25.4039493300921,25.5142951181627,25.6246409062333,
25.7354821569353,25.8461429057937,25.9566374510624,26.0670349562016,26.1773739290343,
26.2181187682761),.UNSPECIFIED.);
#671=B_SPLINE_CURVE_WITH_KNOTS('',3,(#55884,#55885,#55886,#55887,#55888,
#55889,#55890,#55891,#55892,#55893,#55894,#55895,#55896,#55897,#55898,#55899,
#55900,#55901,#55902,#55903,#55904,#55905,#55906,#55907,#55908,#55909,#55910,
#55911,#55912,#55913,#55914,#55915,#55916,#55917,#55918,#55919,#55920,#55921,
#55922,#55923,#55924,#55925,#55926,#55927,#55928,#55929,#55930,#55931,#55932,
#55933,#55934,#55935,#55936,#55937,#55938,#55939,#55940,#55941,#55942,#55943,
#55944,#55945,#55946,#55947,#55948,#55949,#55950,#55951,#55952,#55953,#55954,
#55955,#55956,#55957,#55958,#55959,#55960,#55961,#55962,#55963,#55964,#55965,
#55966,#55967,#55968,#55969,#55970,#55971,#55972,#55973,#55974,#55975,#55976,
#55977,#55978,#55979,#55980,#55981,#55982,#55983,#55984,#55985,#55986,#55987,
#55988,#55989,#55990,#55991,#55992,#55993,#55994,#55995,#55996,#55997,#55998,
#55999,#56000,#56001,#56002,#56003,#56004,#56005,#56006,#56007,#56008,#56009,
#56010,#56011,#56012,#56013,#56014,#56015,#56016,#56017,#56018,#56019,#56020,
#56021,#56022,#56023,#56024,#56025,#56026,#56027,#56028,#56029,#56030,#56031,
#56032,#56033,#56034,#56035,#56036,#56037,#56038,#56039,#56040,#56041,#56042,
#56043,#56044,#56045,#56046,#56047,#56048,#56049,#56050,#56051,#56052,#56053,
#56054,#56055,#56056,#56057,#56058),.UNSPECIFIED.,.F.,.F.,(4,3,3,3,3,3,
3,3,3,3,3,3,3,3,3,3,3,3,3,3,3,3,3,3,3,3,3,3,3,3,3,3,3,3,3,3,3,3,3,3,3,3,
3,3,3,3,3,3,3,3,3,3,3,3,3,3,3,3,4),(26.2181187686548,26.3384959137195,26.4593174082803,
26.5806968286956,26.6102040180115,26.7195412294059,26.8290694669539,26.9381157372594,
27.047097582449,27.1560547068255,27.2659828125666,27.3750755526661,27.4854213412279,
27.5957671297898,27.7051043424275,27.81463257982,27.9236788513792,28.0326606978225,
28.141617823451,28.2515459279802,28.3606386693125,28.4709844554403,28.581330241568,
28.6906674510535,28.8001956888401,28.9092419572624,29.0182238005836,29.1271809231098,
29.2371090306689,29.3462017689833,29.4565475611647,29.5668933533462,29.676230564775,
29.7857588023187,29.8948050726067,30.0037869177593,30.1127440420799,30.222672147841,
30.3317648878394,30.4421106764819,30.5524564651244,30.6617936853272,30.7713219217741,
30.8803682009476,30.9893500550019,31.0983071882249,31.2082352853943,31.3173280341927,
31.4276738055476,31.5380195769026,31.6469506371475,31.7556960802581,31.8643381430127,
31.9729172904604,32.0814739006531,32.1901241097691,32.2988188835178,32.4077120677762,
32.5013040751382),.UNSPECIFIED.);
#672=B_SPLINE_CURVE_WITH_KNOTS('',3,(#56060,#56061,#56062,#56063,#56064,
#56065,#56066,#56067,#56068,#56069,#56070,#56071,#56072,#56073,#56074,#56075,
#56076,#56077,#56078,#56079,#56080,#56081,#56082,#56083,#56084,#56085,#56086,
#56087,#56088,#56089,#56090,#56091,#56092,#56093,#56094,#56095,#56096,#56097,
#56098,#56099,#56100,#56101,#56102,#56103,#56104,#56105,#56106,#56107,#56108,
#56109,#56110,#56111,#56112,#56113,#56114,#56115,#56116,#56117,#56118,#56119,
#56120,#56121,#56122,#56123,#56124,#56125,#56126,#56127,#56128,#56129,#56130,
#56131,#56132,#56133,#56134,#56135,#56136,#56137,#56138,#56139,#56140,#56141,
#56142,#56143,#56144,#56145,#56146,#56147,#56148,#56149,#56150,#56151,#56152,
#56153,#56154,#56155,#56156,#56157,#56158,#56159,#56160,#56161,#56162,#56163,
#56164,#56165,#56166,#56167,#56168,#56169,#56170,#56171,#56172,#56173,#56174,
#56175,#56176,#56177,#56178,#56179,#56180,#56181,#56182,#56183,#56184,#56185,
#56186,#56187,#56188,#56189,#56190,#56191,#56192,#56193,#56194,#56195,#56196,
#56197,#56198,#56199,#56200,#56201,#56202,#56203,#56204,#56205,#56206,#56207,
#56208,#56209,#56210,#56211,#56212,#56213,#56214,#56215,#56216,#56217,#56218,
#56219,#56220,#56221,#56222,#56223,#56224,#56225,#56226,#56227,#56228,#56229,
#56230,#56231,#56232,#56233,#56234),.UNSPECIFIED.,.F.,.F.,(4,3,3,3,3,3,
3,3,3,3,3,3,3,3,3,3,3,3,3,3,3,3,3,3,3,3,3,3,3,3,3,3,3,3,3,3,3,3,3,3,3,3,
3,3,3,3,3,3,3,3,3,3,3,3,3,3,3,3,4),(32.5013040754556,32.5235826886808,32.6329199073593,
32.7424481439968,32.8514944210897,32.9604762728626,33.0694334036092,33.1793615028216,
33.2884542487017,33.3988000245803,33.509145800459,33.6184830760487,33.7280113055722,
33.8370576406939,33.9460395507448,34.0549967399167,34.1649247829968,34.274017586975,
34.3843632496061,34.4947089122372,34.6040459492957,34.7135742086356,34.8226203053257,
34.9316019776638,35.0405589302422,35.1504872036855,35.2595797765364,35.3699259002759,
35.4802720240154,35.5896093619076,35.6991375836433,35.8081839762799,35.9171659419024,
36.0261231846247,36.136051172417,36.2451440244415,36.3554895801176,36.4658351357936,
36.5751727899969,36.6847009721938,36.7937476917544,36.9027299873101,37.0116875623818,
37.1216152336793,37.2307084200033,37.3410533337875,37.4513982475718,37.5607339329457,
37.6702623612463,37.779307108419,37.8882874359025,37.9972430505506,38.1071726277504,
38.216263895013,38.3266126271815,38.43696135935,38.5625537048142,38.6871198019977,
38.7844893822274),.UNSPECIFIED.);
#673=B_SPLINE_CURVE_WITH_KNOTS('',3,(#56236,#56237,#56238,#56239,#56240,
#56241,#56242,#56243,#56244,#56245,#56246,#56247,#56248,#56249,#56250,#56251,
#56252,#56253,#56254,#56255,#56256,#56257,#56258,#56259,#56260,#56261,#56262,
#56263,#56264,#56265,#56266,#56267,#56268,#56269,#56270,#56271,#56272,#56273,
#56274,#56275,#56276,#56277,#56278,#56279,#56280,#56281,#56282,#56283,#56284,
#56285,#56286,#56287,#56288,#56289,#56290,#56291,#56292,#56293,#56294,#56295,
#56296,#56297,#56298,#56299,#56300,#56301,#56302,#56303,#56304,#56305,#56306,
#56307,#56308,#56309,#56310,#56311,#56312,#56313,#56314,#56315,#56316,#56317,
#56318,#56319,#56320,#56321,#56322,#56323,#56324,#56325,#56326,#56327,#56328,
#56329,#56330,#56331,#56332,#56333,#56334,#56335,#56336,#56337,#56338,#56339,
#56340,#56341,#56342,#56343,#56344,#56345,#56346,#56347,#56348,#56349,#56350,
#56351,#56352,#56353,#56354,#56355,#56356,#56357,#56358,#56359,#56360,#56361,
#56362,#56363,#56364,#56365,#56366,#56367,#56368,#56369,#56370,#56371,#56372,
#56373,#56374,#56375,#56376,#56377,#56378,#56379,#56380,#56381,#56382,#56383,
#56384,#56385,#56386,#56387,#56388,#56389,#56390,#56391,#56392,#56393,#56394,
#56395,#56396,#56397,#56398,#56399,#56400,#56401,#56402,#56403,#56404,#56405,
#56406,#56407,#56408,#56409,#56410),.UNSPECIFIED.,.F.,.F.,(4,3,3,3,3,3,
3,3,3,3,3,3,3,3,3,3,3,3,3,3,3,3,3,3,3,3,3,3,3,3,3,3,3,3,3,3,3,3,3,3,3,3,
3,3,3,3,3,3,3,3,3,3,3,3,3,3,3,3,4),(38.7844893826353,38.8937562439304,39.0030205291665,
39.1124040424951,39.2218467620058,39.3315047765829,39.4225244711282,39.531864446128,
39.6413923382253,39.7504414354374,39.8594261229724,39.9683861001188,40.0783114708157,
40.1874070555165,40.2977473192114,40.4080875829064,40.5174118990146,40.6269417484733,
40.7359751200007,40.8449441019264,40.9538884202333,41.0638289888461,41.1729092104048,
41.2832799525447,41.3936506946846,41.5030054920437,41.6125315313461,41.7215951314652,
41.8305941616126,41.9395682978918,42.0494796750345,42.1585888103856,42.2689013084242,
42.3792138064628,42.4885651699356,42.5980916384737,42.707152654175,42.816149423017,
42.9251216220356,43.035035446087,43.1441434489396,43.2544601835903,43.364776918241,
43.4740090834525,43.5835504517734,43.6924914154099,43.8013681540031,43.9102205474251,
44.0202504180736,44.1292405486958,44.2397902893575,44.3503400300192,44.4588741857476,
44.5672556291874,44.6755255492681,44.7837478551205,44.891939875013,45.0001948129805,
45.0676746898148),.UNSPECIFIED.);
#674=B_SPLINE_CURVE_WITH_KNOTS('',3,(#56412,#56413,#56414,#56415,#56416,
#56417,#56418,#56419,#56420,#56421,#56422,#56423,#56424,#56425,#56426,#56427,
#56428,#56429,#56430,#56431,#56432,#56433,#56434,#56435,#56436,#56437,#56438,
#56439,#56440,#56441,#56442,#56443,#56444,#56445),.UNSPECIFIED.,.F.,.F.,
(4,3,3,3,3,3,3,3,3,3,3,4),(45.0676746902223,45.203625675157,45.3359031417975,
45.4450078827114,45.5539300697693,45.6627505143036,45.7715093749702,45.8802467257635,
45.9890804881181,46.0979590906992,46.2070415430544,46.3075704370366),
 .UNSPECIFIED.);
#675=B_SPLINE_CURVE_WITH_KNOTS('',3,(#56449,#56450,#56451,#56452,#56453,
#56454,#56455),.UNSPECIFIED.,.F.,.F.,(4,3,4),(-48.2925924771321,-48.1551961866216,
-48.0235345953958),.UNSPECIFIED.);
#676=B_SPLINE_CURVE_WITH_KNOTS('',3,(#56457,#56458,#56459,#56460,#56461,
#56462,#56463,#56464,#56465,#56466),.UNSPECIFIED.,.F.,.F.,(4,1,1,1,1,1,
1,4),(-48.0235342885071,-47.3070293653539,-46.3214662535757,-45.3359031417975,
-44.3503400300192,-43.364776918241,-42.3792138064628,-41.7403489813275),
 .UNSPECIFIED.);
#677=B_SPLINE_CURVE_WITH_KNOTS('',3,(#56468,#56469,#56470,#56471,#56472,
#56473,#56474,#56475,#56476,#56477,#56478,#56479,#56480,#56481,#56482,#56483,
#56484,#56485,#56486,#56487,#56488,#56489,#56490,#56491,#56492,#56493,#56494,
#56495,#56496,#56497,#56498,#56499,#56500,#56501,#56502,#56503,#56504,#56505,
#56506,#56507,#56508,#56509,#56510,#56511,#56512,#56513,#56514,#56515,#56516,
#56517,#56518,#56519,#56520,#56521,#56522,#56523,#56524,#56525,#56526,#56527,
#56528,#56529,#56530,#56531,#56532,#56533,#56534,#56535,#56536,#56537,#56538,
#56539,#56540,#56541,#56542,#56543,#56544,#56545,#56546,#56547,#56548,#56549,
#56550,#56551,#56552,#56553,#56554,#56555,#56556,#56557,#56558,#56559,#56560,
#56561,#56562,#56563,#56564,#56565,#56566,#56567,#56568,#56569,#56570,#56571,
#56572,#56573,#56574,#56575,#56576,#56577,#56578,#56579,#56580,#56581,#56582,
#56583,#56584,#56585,#56586,#56587,#56588,#56589,#56590,#56591,#56592,#56593,
#56594,#56595,#56596,#56597,#56598,#56599,#56600,#56601,#56602,#56603,#56604,
#56605,#56606,#56607,#56608,#56609,#56610,#56611,#56612,#56613,#56614,#56615,
#56616,#56617,#56618,#56619,#56620,#56621,#56622,#56623,#56624,#56625,#56626,
#56627,#56628,#56629,#56630,#56631,#56632,#56633,#56634,#56635,#56636,#56637,
#56638,#56639,#56640,#56641,#56642),.UNSPECIFIED.,.F.,.F.,(4,3,3,3,3,3,
3,3,3,3,3,3,3,3,3,3,3,3,3,3,3,3,3,3,3,3,3,3,3,3,3,3,3,3,3,3,3,3,3,3,3,3,
3,3,3,3,3,3,3,3,3,3,3,3,3,3,3,3,4),(-41.7403485560519,-41.615840513558,
-41.4902535416044,-41.3936506946846,-41.284325628528,-41.1747958728253,
-41.0657621949742,-40.9567930737688,-40.8478487829612,-40.7379084829475,
-40.628828696172,-40.5184581395392,-40.4080875829064,-40.2987475649647,
-40.1892196782351,-40.0801705620444,-39.9711858645597,-39.8622258864825,
-39.7523005326439,-39.6432049690615,-39.5328647200948,-39.4225244711282,
-39.3131858654622,-39.2036578021981,-39.0946100515161,-38.9856266978384,
-38.8766680394291,-38.7667413694093,-38.6576470502025,-38.5473042047762,
-38.43696135935,-38.3276255745887,-38.2180971587116,-38.1090523710127,-38.0000720251634,
-37.8911164142742,-37.7811868725986,-37.6720956631173,-37.5617469553446,
-37.4513982475718,-37.3420605984726,-37.2325324156377,-37.1234856979709,
-37.0145034031013,-36.9055458275105,-36.7956181545813,-36.6865249647992,
-36.5761800502964,-36.4658351357936,-36.3564978189441,-36.246969594578,
-36.1379232106088,-36.0289412489942,-35.9199840056274,-35.8100560102244,
-35.700963146194,-35.5906175851047,-35.4802720240154,-35.4571636741479),
 .UNSPECIFIED.);
#678=B_SPLINE_CURVE_WITH_KNOTS('',3,(#56644,#56645,#56646,#56647,#56648,
#56649,#56650,#56651,#56652,#56653,#56654,#56655,#56656,#56657,#56658,#56659,
#56660,#56661,#56662,#56663,#56664,#56665,#56666,#56667,#56668,#56669,#56670,
#56671,#56672,#56673,#56674,#56675,#56676,#56677,#56678,#56679,#56680,#56681,
#56682,#56683,#56684,#56685,#56686,#56687,#56688,#56689,#56690,#56691,#56692,
#56693,#56694,#56695,#56696,#56697,#56698,#56699,#56700,#56701,#56702,#56703,
#56704,#56705,#56706,#56707,#56708,#56709,#56710,#56711,#56712,#56713,#56714,
#56715,#56716,#56717,#56718,#56719,#56720,#56721,#56722,#56723,#56724,#56725,
#56726,#56727,#56728,#56729,#56730,#56731,#56732,#56733,#56734,#56735,#56736,
#56737,#56738,#56739,#56740,#56741,#56742,#56743,#56744,#56745,#56746,#56747,
#56748,#56749,#56750,#56751,#56752,#56753,#56754,#56755,#56756,#56757,#56758,
#56759,#56760,#56761,#56762,#56763,#56764,#56765,#56766,#56767,#56768,#56769,
#56770,#56771,#56772,#56773,#56774,#56775,#56776,#56777,#56778,#56779,#56780,
#56781,#56782,#56783,#56784,#56785,#56786,#56787,#56788,#56789,#56790,#56791,
#56792,#56793,#56794,#56795,#56796,#56797,#56798,#56799,#56800,#56801,#56802,
#56803,#56804,#56805,#56806,#56807,#56808,#56809,#56810,#56811,#56812,#56813,
#56814,#56815,#56816,#56817,#56818),.UNSPECIFIED.,.F.,.F.,(4,3,3,3,3,3,
3,3,3,3,3,3,3,3,3,3,3,3,3,3,3,3,3,3,3,3,3,3,3,3,3,3,3,3,3,3,3,3,3,3,3,3,
3,3,3,3,3,3,3,3,3,3,3,3,3,3,3,3,4),(-35.4571636738398,-35.3482509468301,
-35.2395222303795,-35.1308958950177,-35.0223314563655,-34.9137885159107,
-34.8051505167586,-34.696467014166,-34.5875841193446,-34.4947089122372,
-34.3853716384126,-34.2758434086684,-34.1667970742412,-34.0578151644816,
-33.948857975199,-33.838929931514,-33.7298371264434,-33.6194914634512,-33.509145800459,
-33.3998085838417,-33.2902803469466,-33.1812340707049,-33.0722522193277,
-32.9632950885218,-32.8533669885615,-32.7442742415114,-32.6339284650961,
-32.5235826886808,-32.4142454948571,-32.3047172551128,-32.1956710031575,
-32.0866891765581,-31.9777320709795,-31.8678039474603,-31.7587112264511,
-31.6483654016769,-31.5380195769026,-31.4286823570365,-31.3191541205475,
-31.2101078415077,-31.1011259875108,-30.9921688542689,-30.8822407569828,
-30.7731480079796,-30.662802236552,-30.5524564651244,-30.4431192538816,
-30.3335910163147,-30.2245447461042,-30.1155629009879,-30.0066057766627,
-29.8966776708336,-29.7875849307311,-29.6772391420386,-29.5668933533462,
-29.4456706023087,-29.3248472979377,-29.2046599751121,-29.1739783673454),
 .UNSPECIFIED.);
#679=B_SPLINE_CURVE_WITH_KNOTS('',3,(#56820,#56821,#56822,#56823,#56824,
#56825,#56826,#56827,#56828,#56829,#56830,#56831,#56832,#56833,#56834,#56835,
#56836,#56837,#56838,#56839,#56840,#56841,#56842,#56843,#56844,#56845,#56846,
#56847,#56848,#56849,#56850,#56851,#56852,#56853,#56854,#56855,#56856,#56857,
#56858,#56859,#56860,#56861,#56862,#56863,#56864,#56865,#56866,#56867,#56868,
#56869,#56870,#56871,#56872,#56873,#56874,#56875,#56876,#56877,#56878,#56879,
#56880,#56881,#56882,#56883,#56884,#56885,#56886,#56887,#56888,#56889,#56890,
#56891,#56892,#56893,#56894,#56895,#56896,#56897,#56898,#56899,#56900,#56901,
#56902,#56903,#56904,#56905,#56906,#56907,#56908,#56909,#56910,#56911,#56912,
#56913,#56914,#56915,#56916,#56917,#56918,#56919,#56920,#56921,#56922,#56923,
#56924,#56925,#56926,#56927,#56928,#56929,#56930,#56931,#56932,#56933,#56934,
#56935,#56936,#56937,#56938,#56939,#56940,#56941,#56942,#56943,#56944,#56945,
#56946,#56947,#56948,#56949,#56950,#56951,#56952,#56953,#56954,#56955,#56956,
#56957,#56958,#56959,#56960,#56961,#56962,#56963,#56964,#56965,#56966,#56967,
#56968,#56969,#56970,#56971,#56972,#56973,#56974,#56975,#56976,#56977,#56978,
#56979,#56980,#56981,#56982,#56983,#56984,#56985,#56986,#56987,#56988,#56989,
#56990,#56991,#56992,#56993,#56994),.UNSPECIFIED.,.F.,.F.,(4,3,3,3,3,3,
3,3,3,3,3,3,3,3,3,3,3,3,3,3,3,3,3,3,3,3,3,3,3,3,3,3,3,3,3,3,3,3,3,3,3,3,
3,3,3,3,3,3,3,3,3,3,3,3,3,3,3,3,4),(-29.1739783669683,-29.0636179975722,
-28.9532180437743,-28.8426593424289,-28.732009659386,-28.6211452081831,
-28.581330241568,-28.4719930289838,-28.3624647915845,-28.2534185200467,
-28.1444366736126,-28.0354795479814,-27.9255514434335,-27.8164587020689,
-27.7061129159293,-27.5957671297898,-27.4864299184101,-27.3769016808603,
-27.2678554105611,-27.1588735653748,-27.0499164409984,-26.9399883352517,
-26.8308955951446,-26.7205498065781,-26.6102040180116,-26.5008668066609,
-26.3913385691074,-26.2822922988486,-26.1733104537067,-26.0643533293788,
-25.9544252235924,-25.8453324835434,-25.7349866948883,-25.6246409062333,
-25.5153036946033,-25.4057754570848,-25.2967291865319,-25.1877473410915,
-25.0787902164607,-24.9688621109593,-24.8597693706007,-24.7494235825279,
-24.6390777944551,-24.5297405829907,-24.4202123454515,-24.3111660750705,
-24.2021842298035,-24.0932271053477,-23.98329899968,-23.8742062594979,-23.7638604710874,
-23.6535146826769,-23.545626041452,-23.4378850553064,-23.3302497285488,
-23.2203855614481,-23.112800792144,-23.0017969261448,-22.8907930601457),
 .UNSPECIFIED.);
#680=B_SPLINE_CURVE_WITH_KNOTS('',3,(#56996,#56997,#56998,#56999,#57000,
#57001,#57002,#57003,#57004,#57005,#57006,#57007,#57008,#57009,#57010,#57011,
#57012,#57013,#57014,#57015,#57016,#57017,#57018,#57019,#57020,#57021,#57022,
#57023,#57024,#57025,#57026,#57027,#57028,#57029,#57030,#57031,#57032,#57033,
#57034,#57035,#57036,#57037,#57038,#57039,#57040,#57041,#57042,#57043,#57044,
#57045,#57046,#57047,#57048,#57049,#57050,#57051,#57052,#57053,#57054,#57055,
#57056,#57057,#57058,#57059,#57060,#57061,#57062,#57063,#57064,#57065,#57066,
#57067,#57068,#57069,#57070,#57071,#57072,#57073,#57074,#57075,#57076,#57077,
#57078,#57079,#57080,#57081,#57082,#57083,#57084,#57085,#57086,#57087,#57088,
#57089,#57090,#57091,#57092,#57093,#57094,#57095,#57096,#57097,#57098,#57099,
#57100,#57101,#57102,#57103,#57104,#57105,#57106,#57107,#57108,#57109,#57110,
#57111,#57112,#57113,#57114,#57115,#57116,#57117,#57118,#57119,#57120,#57121,
#57122,#57123,#57124,#57125,#57126,#57127,#57128,#57129,#57130,#57131,#57132,
#57133,#57134,#57135,#57136,#57137,#57138,#57139,#57140,#57141,#57142,#57143,
#57144,#57145,#57146,#57147,#57148,#57149,#57150,#57151,#57152,#57153,#57154,
#57155,#57156,#57157,#57158,#57159,#57160,#57161,#57162,#57163,#57164,#57165,
#57166,#57167),.UNSPECIFIED.,.F.,.F.,(4,3,3,3,3,3,3,3,3,3,3,3,3,3,3,3,3,
3,3,3,3,3,3,3,3,3,3,3,3,3,3,3,3,3,3,3,3,3,3,3,3,3,3,3,3,3,3,3,3,3,3,3,3,
3,3,3,3,4),(-22.8907930597887,-22.7446120253379,-22.6679515708987,-22.5586143595699,
-22.4490861220137,-22.3400398517639,-22.2310580066262,-22.1221008822976,
-22.0121727765033,-21.9030800364417,-21.7927342477811,-21.6823884591205,
-21.5730512477264,-21.4635230101784,-21.3544767398733,-21.2454948946841,
-21.136537770308,-21.0266096645666,-20.9175169244675,-20.8071711359049,
-20.6968253473423,-20.5874881347035,-20.477959897311,-20.3689136257507,
-20.2599317793062,-20.1509746536766,-20.0410465491485,-19.9319538078151,
-19.8216080216896,-19.7112622355641,-19.6019250260803,-19.4923967882935,
-19.3833505198729,-19.2743686765534,-19.1654115540288,-19.0554834464681,
-18.9463907081554,-18.8360449159706,-18.7256991237859,-18.6163619123579,
-18.5068336748142,-18.3977874045272,-18.2888055593755,-18.1798484350559,
-18.0699203292938,-17.9608275892965,-17.8504818006521,-17.7401360120077,
-17.6307987917964,-17.5212705553506,-17.4122242761684,-17.3032424221055,
-17.1942852888741,-17.0843571917129,-16.9752644429062,-16.8649186715678,
-16.7545729002295,-16.6076077526092),.UNSPECIFIED.);
#681=B_SPLINE_CURVE_WITH_KNOTS('',3,(#57169,#57170,#57171,#57172,#57173,
#57174,#57175,#57176,#57177,#57178,#57179,#57180,#57181,#57182,#57183,#57184,
#57185,#57186,#57187,#57188,#57189,#57190,#57191,#57192,#57193,#57194,#57195,
#57196,#57197,#57198,#57199,#57200,#57201,#57202,#57203,#57204,#57205,#57206,
#57207,#57208,#57209,#57210,#57211,#57212,#57213,#57214,#57215,#57216,#57217,
#57218,#57219,#57220,#57221,#57222,#57223,#57224,#57225,#57226,#57227,#57228,
#57229,#57230,#57231,#57232,#57233,#57234,#57235,#57236,#57237,#57238,#57239,
#57240,#57241,#57242,#57243,#57244,#57245,#57246,#57247,#57248,#57249,#57250,
#57251,#57252,#57253,#57254,#57255,#57256,#57257,#57258,#57259,#57260,#57261,
#57262,#57263,#57264,#57265,#57266,#57267,#57268,#57269,#57270,#57271,#57272,
#57273,#57274,#57275,#57276,#57277,#57278,#57279,#57280,#57281,#57282,#57283,
#57284,#57285,#57286,#57287,#57288,#57289,#57290,#57291,#57292,#57293,#57294,
#57295,#57296,#57297,#57298,#57299,#57300,#57301,#57302,#57303,#57304,#57305,
#57306,#57307,#57308,#57309,#57310,#57311,#57312,#57313,#57314,#57315,#57316,
#57317,#57318,#57319,#57320,#57321,#57322,#57323,#57324,#57325,#57326,#57327,
#57328,#57329,#57330,#57331,#57332,#57333,#57334,#57335,#57336,#57337,#57338,
#57339,#57340,#57341,#57342,#57343),.UNSPECIFIED.,.F.,.F.,(4,3,3,3,3,3,
3,3,3,3,3,3,3,3,3,3,3,3,3,3,3,3,3,3,3,3,3,3,3,3,3,3,3,3,3,3,3,3,3,3,3,3,
3,3,3,3,3,3,3,3,3,3,3,3,3,3,3,3,4),(-16.6076077522586,-16.4999871317891,
-16.3924795284533,-16.2850428992939,-16.1776353106626,-16.0701415239761,
-15.9626061582257,-15.8548783947035,-15.7690097884513,-15.6596725697738,
-15.5501443331362,-15.4410980560447,-15.3321162042733,-15.2231590735284,
-15.1132309743146,-15.0041382284364,-14.8937924525548,-14.7834466766731,
-14.6741094010268,-14.5645811715103,-14.4555348363317,-14.3465529262237,
-14.2375957369949,-14.1276676939699,-14.0185748899357,-13.9082292274153,
-13.7978835648949,-13.6885465279501,-13.579018268596,-13.4699721720189,
-13.3609904997933,-13.2520335473263,-13.1421052737739,-13.0330127010316,
-12.9226665770742,-12.8123204531167,-12.7029831151977,-12.5934548934653,
-12.4844085008043,-12.3754265351588,-12.2664692924144,-12.1565413046455,
-12.0474484526016,-11.93710289697,-11.8267573413385,-11.7174196867805,-11.6078915046279,
-11.4988447847093,-11.3898624887953,-11.2809049133659,-11.1709772424145,
-11.061884055738,-10.9515391426491,-10.8411942295603,-10.7275265913945,
-10.6141543120805,-10.5009590036298,-10.3879603830256,-10.3244224454296),
 .UNSPECIFIED.);
#682=B_SPLINE_CURVE_WITH_KNOTS('',3,(#57344,#57345,#57346,#57347,#57348,
#57349,#57350,#57351,#57352,#57353,#57354,#57355,#57356,#57357,#57358,#57359,
#57360,#57361,#57362,#57363,#57364,#57365,#57366,#57367,#57368,#57369,#57370,
#57371,#57372,#57373,#57374,#57375,#57376,#57377,#57378,#57379,#57380,#57381,
#57382,#57383,#57384,#57385,#57386,#57387,#57388,#57389,#57390,#57391,#57392,
#57393,#57394,#57395,#57396,#57397,#57398,#57399,#57400,#57401,#57402,#57403,
#57404,#57405,#57406,#57407,#57408,#57409,#57410,#57411,#57412,#57413,#57414,
#57415,#57416,#57417,#57418,#57419,#57420,#57421,#57422,#57423,#57424,#57425,
#57426,#57427,#57428,#57429,#57430,#57431,#57432,#57433,#57434,#57435,#57436,
#57437,#57438,#57439,#57440,#57441,#57442,#57443,#57444,#57445,#57446,#57447,
#57448,#57449,#57450,#57451,#57452,#57453,#57454,#57455,#57456,#57457,#57458,
#57459,#57460,#57461,#57462,#57463,#57464,#57465,#57466,#57467,#57468,#57469,
#57470,#57471,#57472,#57473,#57474,#57475,#57476,#57477,#57478,#57479,#57480,
#57481,#57482,#57483,#57484,#57485,#57486,#57487,#57488,#57489,#57490,#57491,
#57492,#57493,#57494,#57495,#57496,#57497,#57498,#57499,#57500,#57501,#57502,
#57503,#57504,#57505,#57506,#57507,#57508,#57509,#57510,#57511,#57512,#57513,
#57514,#57515,#57516,#57517,#57518),.UNSPECIFIED.,.F.,.F.,(4,3,3,3,3,3,
3,3,3,3,3,3,3,3,3,3,3,3,3,3,3,3,3,3,3,3,3,3,3,3,3,3,3,3,3,3,3,3,3,3,3,3,
3,3,3,3,3,3,3,3,3,3,3,3,3,3,3,3,4),(-10.3244224449722,-10.2072246131747,
-10.09165085566,-9.97364098672105,-9.85563111778205,-9.74629230873417,-9.63676427089288,
-9.52771643631158,-9.41873304372302,-9.30977439132236,-9.19984779499273,
-9.09075359148984,-8.98041079874685,-8.87006800600385,-8.76072802889233,
-8.651200137059,-8.5421510377115,-8.43316634803825,-8.32420636875443,-8.21428100012223,
-8.10518541331124,-7.99484515376844,-7.88450489422564,-7.7751805834152,
-7.66565073329423,-7.55661736705702,-7.44764839040374,-7.33870407734288,
-7.22876350361902,-7.11968328718189,-7.00931253481466,-6.89894178244744,
-6.78958698223486,-6.68006094328916,-6.57099734040682,-6.46199830753732,
-6.35302416858155,-6.24311279410347,-6.13400365621582,-6.02369116344252,
-5.91337867066923,-5.80402729489106,-5.69450082789106,-5.58543979974154,
-5.47644301843349,-5.36747080695317,-5.25755699493764,-5.14844897977771,
-5.03813226933437,-4.92781555889103,-4.81699325636299,-4.70927521869757,
-4.60165774558959,-4.49409900115545,-4.3865572407147,-4.27893084714527,
-4.17125183227785,-4.06341456574977,-4.04123713866671),.UNSPECIFIED.);
#683=B_SPLINE_CURVE_WITH_KNOTS('',3,(#57521,#57522,#57523,#57524,#57525,
#57526,#57527,#57528,#57529,#57530,#57531,#57532,#57533,#57534,#57535,#57536,
#57537,#57538,#57539,#57540,#57541,#57542,#57543,#57544,#57545,#57546,#57547,
#57548,#57549,#57550,#57551,#57552,#57553,#57554,#57555,#57556,#57557,#57558,
#57559,#57560,#57561,#57562,#57563,#57564,#57565,#57566,#57567,#57568,#57569,
#57570,#57571,#57572,#57573,#57574,#57575,#57576,#57577,#57578,#57579,#57580,
#57581,#57582,#57583,#57584,#57585,#57586,#57587,#57588,#57589,#57590,#57591,
#57592,#57593,#57594,#57595,#57596,#57597,#57598,#57599,#57600,#57601,#57602,
#57603,#57604,#57605,#57606,#57607,#57608,#57609,#57610,#57611,#57612,#57613,
#57614,#57615,#57616,#57617,#57618,#57619,#57620,#57621,#57622,#57623,#57624,
#57625,#57626,#57627,#57628,#57629,#57630,#57631,#57632,#57633,#57634,#57635,
#57636,#57637,#57638,#57639,#57640,#57641,#57642,#57643,#57644,#57645,#57646,
#57647,#57648),.UNSPECIFIED.,.F.,.F.,(4,2,2,2,2,2,2,2,2,2,2,2,2,2,2,2,2,
2,2,2,2,2,2,2,2,2,2,2,2,2,2,2,2,2,2,2,2,2,2,2,2,2,2,2,2,2,2,2,2,2,2,2,2,
2,2,2,2,2,2,2,2,2,2,4),(0.00160705595523008,0.00303069816735615,0.00693180054122098,
0.0260766323320663,0.049420593346507,0.0585609139609525,0.0656560107037017,
0.0743798200061914,0.0937641513165261,0.110101325445735,0.116979872190794,
0.122577131094358,0.12669519364253,0.131828585845873,0.150504578641132,
0.171476070898076,0.181712855199548,0.188854962153091,0.196843599860368,
0.212713122807251,0.234001272043188,0.241725383518611,0.247779851098417,
0.251833409216635,0.257185321475974,0.279991783609909,0.300899892154916,
0.309621683637536,0.316596312965283,0.325374349979552,0.347715335888014,
0.362524271249563,0.366943856318463,0.373364630364573,0.377399670873743,
0.382562133593276,0.407999153711683,0.422135731944411,0.43300947728638,
0.440204992883985,0.447938215265115,0.463241281223814,0.485457419866072,
0.493300190134225,0.499414348024838,0.503479248067671,0.508826310319265,
0.520139301900781,0.542675515758242,0.549285889728129,0.559413689495879,
0.566515011404271,0.574479153561681,0.590378227251692,0.61154715707313,
0.619242701470622,0.625276697613685,0.629328686156107,0.634703608039514,
0.661162014958273,0.676255444956648,0.685857530307112,0.692902189979643,
0.692945632510061),.UNSPECIFIED.);
#684=B_SPLINE_CURVE_WITH_KNOTS('',3,(#57651,#57652,#57653,#57654,#57655,
#57656,#57657,#57658,#57659,#57660,#57661,#57662,#57663,#57664,#57665,#57666,
#57667,#57668,#57669,#57670,#57671,#57672,#57673,#57674,#57675,#57676,#57677,
#57678,#57679,#57680,#57681,#57682,#57683,#57684,#57685,#57686,#57687,#57688,
#57689,#57690,#57691,#57692,#57693,#57694,#57695,#57696,#57697,#57698,#57699,
#57700,#57701,#57702,#57703,#57704,#57705,#57706,#57707,#57708,#57709,#57710,
#57711,#57712,#57713,#57714,#57715,#57716,#57717,#57718,#57719,#57720,#57721,
#57722,#57723,#57724,#57725,#57726,#57727,#57728,#57729,#57730,#57731,#57732,
#57733,#57734,#57735,#57736,#57737,#57738,#57739,#57740,#57741,#57742,#57743,
#57744,#57745,#57746),.UNSPECIFIED.,.F.,.F.,(4,2,2,2,2,2,2,2,2,2,2,2,2,
2,2,2,2,2,2,2,2,2,2,2,2,2,2,2,2,2,2,2,2,2,2,2,2,2,2,2,2,2,2,2,2,2,2,4),
(-1.21411811178252,-1.2110857626649,-1.20731545990233,-1.19202931788252,
-1.17330458064623,-1.16179203960238,-1.15395453653068,-1.14502478488769,
-1.12157541088363,-1.10401260242507,-1.09677384268193,-1.09094703605413,
-1.08731588903907,-1.08218585926128,-1.05768297439084,-1.03820959597564,
-1.02983271989945,-1.02311177806054,-1.01470975413155,-0.987446417451232,
-0.969965930718606,-0.964241892128248,-0.960312323131805,-0.955083467613174,
-0.930824734090043,-0.910628930123118,-0.901912198549083,-0.895527290220546,
-0.88680947190823,-0.867508963456092,-0.851083530299997,-0.844187046522863,
-0.83858083305714,-0.834463814367659,-0.829339717316834,-0.809974114266387,
-0.793130709011167,-0.787441919427184,-0.77821947502899,-0.771161585226906,
-0.762622592226985,-0.736096321326291,-0.723439689399553,-0.715117650593693,
-0.71077175182725,-0.706217361616685,-0.696338002095026,-0.692979258838884),
 .UNSPECIFIED.);
#685=B_SPLINE_CURVE_WITH_KNOTS('',3,(#57751,#57752,#57753,#57754,#57755,
#57756,#57757,#57758,#57759,#57760,#57761,#57762,#57763,#57764,#57765,#57766,
#57767,#57768,#57769,#57770,#57771,#57772,#57773,#57774,#57775,#57776,#57777,
#57778,#57779,#57780,#57781,#57782,#57783,#57784,#57785,#57786,#57787,#57788,
#57789,#57790,#57791,#57792,#57793,#57794,#57795,#57796,#57797,#57798,#57799,
#57800,#57801,#57802,#57803,#57804,#57805,#57806,#57807,#57808,#57809,#57810,
#57811,#57812,#57813,#57814,#57815,#57816,#57817,#57818,#57819,#57820,#57821,
#57822,#57823,#57824,#57825,#57826,#57827,#57828,#57829),.UNSPECIFIED.,
 .F.,.F.,(4,3,3,3,3,3,3,3,3,3,3,3,3,3,3,3,3,3,3,3,3,3,3,3,3,3,4),(-0.295872322228609,
-0.295800390457621,-0.276373981843977,-0.263250378750487,-0.258528391455822,
-0.239527378274684,-0.226792705152952,-0.222168728339882,-0.218676032022988,
-0.200352145245616,-0.182496347188838,-0.171319424938723,-0.161265355966744,
-0.15793468747543,-0.140841510700994,-0.137688493100165,-0.120125890536754,
-0.104799833849173,-0.101813032456204,-0.0849744272046009,-0.0684432950696122,
-0.0520509361631049,-0.0483399571277156,-0.032301942455842,-0.0162639277839685,
-0.00121618693710043,0.),.UNSPECIFIED.);
#686=B_SPLINE_CURVE_WITH_KNOTS('',3,(#57831,#57832,#57833,#57834),
 .UNSPECIFIED.,.F.,.F.,(4,4),(0.,0.00985912010464335),.UNSPECIFIED.);
#687=B_SPLINE_CURVE_WITH_KNOTS('',3,(#57835,#57836,#57837,#57838,#57839,
#57840,#57841,#57842,#57843,#57844,#57845,#57846,#57847,#57848,#57849,#57850,
#57851,#57852,#57853,#57854,#57855,#57856,#57857,#57858,#57859,#57860,#57861,
#57862,#57863,#57864,#57865,#57866,#57867,#57868,#57869,#57870,#57871,#57872,
#57873,#57874,#57875,#57876,#57877,#57878,#57879,#57880,#57881,#57882,#57883,
#57884,#57885,#57886,#57887,#57888,#57889,#57890,#57891,#57892,#57893,#57894,
#57895,#57896,#57897,#57898,#57899,#57900,#57901,#57902,#57903,#57904,#57905,
#57906,#57907,#57908,#57909,#57910,#57911,#57912,#57913,#57914,#57915,#57916,
#57917,#57918,#57919),.UNSPECIFIED.,.F.,.F.,(4,3,3,3,3,3,3,3,3,3,3,3,3,
3,3,3,3,3,3,3,3,3,3,3,3,3,3,3,4),(-0.300067541140097,-0.298264687041868,
-0.283066149434729,-0.274573360236698,-0.270084926663162,-0.266149262121986,
-0.250029687161801,-0.240714412789918,-0.236187237775089,-0.219496198515433,
-0.202395854960078,-0.191718287929847,-0.186414128238179,-0.183367582668388,
-0.165564985377019,-0.159558822602046,-0.142340885891246,-0.133217270038284,
-0.128037713880546,-0.12353774143095,-0.105513692533452,-0.086987532383811,
-0.0684672685495456,-0.0648082422231501,-0.0612577277857387,-0.0420101474320933,
-0.0227205645652813,-0.00360078115333159,0.),.UNSPECIFIED.);
#688=B_SPLINE_CURVE_WITH_KNOTS('',3,(#58129,#58130,#58131,#58132),
 .UNSPECIFIED.,.F.,.F.,(4,4),(-0.0228279319091498,0.),.UNSPECIFIED.);
#689=B_SPLINE_CURVE_WITH_KNOTS('',3,(#58134,#58135,#58136,#58137,#58138,
#58139,#58140,#58141,#58142,#58143,#58144,#58145,#58146,#58147,#58148,#58149,
#58150,#58151,#58152,#58153,#58154,#58155,#58156,#58157,#58158,#58159,#58160,
#58161,#58162,#58163,#58164,#58165,#58166,#58167,#58168,#58169,#58170,#58171,
#58172,#58173,#58174,#58175,#58176,#58177,#58178,#58179,#58180,#58181,#58182,
#58183,#58184,#58185,#58186,#58187,#58188,#58189,#58190,#58191,#58192,#58193,
#58194,#58195,#58196,#58197,#58198,#58199,#58200,#58201,#58202,#58203,#58204,
#58205,#58206,#58207,#58208,#58209,#58210,#58211,#58212,#58213,#58214,#58215,
#58216,#58217,#58218),.UNSPECIFIED.,.F.,.F.,(4,3,3,3,3,3,3,3,3,3,3,3,3,
3,3,3,3,3,3,3,3,3,3,3,3,3,3,3,4),(-0.300067541140124,-0.298264687041895,
-0.28306614612428,-0.274573356605969,-0.270084902423893,-0.266149257077711,
-0.250012130634623,-0.240714394402588,-0.236187236421063,-0.219545451825803,
-0.202445276722714,-0.191718285618554,-0.186414122583878,-0.183367577486661,
-0.165564980231119,-0.159558822602065,-0.14234088543558,-0.133217269957808,
-0.128037714183407,-0.123537741563047,-0.105564719399351,-0.0870159929477358,
-0.0684672664961207,-0.0648082516194149,-0.0612577300642884,-0.0419353127656361,
-0.022623645419663,-0.00360078661868575,0.),.UNSPECIFIED.);
#690=B_SPLINE_CURVE_WITH_KNOTS('',3,(#58219,#58220,#58221,#58222),
 .UNSPECIFIED.,.F.,.F.,(4,4),(-0.0098305480153634,0.),.UNSPECIFIED.);
#691=B_SPLINE_CURVE_WITH_KNOTS('',3,(#58227,#58228,#58229,#58230,#58231,
#58232,#58233,#58234,#58235,#58236,#58237,#58238,#58239,#58240,#58241,#58242,
#58243,#58244,#58245,#58246,#58247,#58248,#58249,#58250,#58251,#58252,#58253,
#58254,#58255,#58256,#58257,#58258,#58259,#58260,#58261,#58262,#58263,#58264,
#58265,#58266,#58267,#58268,#58269,#58270,#58271,#58272,#58273,#58274,#58275,
#58276,#58277,#58278,#58279,#58280,#58281,#58282,#58283,#58284,#58285,#58286,
#58287,#58288,#58289,#58290,#58291,#58292,#58293,#58294,#58295,#58296,#58297,
#58298,#58299,#58300,#58301,#58302,#58303,#58304,#58305),.UNSPECIFIED.,
 .F.,.F.,(4,3,3,3,3,3,3,3,3,3,3,3,3,3,3,3,3,3,3,3,3,3,3,3,3,3,4),(-0.295872351833489,
-0.295800390457537,-0.276036403287862,-0.263250379555454,-0.258528391470647,
-0.239521878863702,-0.226792705643256,-0.222168753783715,-0.21867604574408,
-0.200368561394637,-0.18251252301445,-0.171319438031604,-0.1612653787683,
-0.157934691378101,-0.140841517786507,-0.137688493100138,-0.120477431462621,
-0.104799834548055,-0.101813033019031,-0.0849850954960385,-0.0683039566266225,
-0.0520509292305863,-0.0483399545671687,-0.0325278496633223,-0.0162639248316611,
-0.00121617927212471,0.),.UNSPECIFIED.);
#692=B_SPLINE_CURVE_WITH_KNOTS('',3,(#58515,#58516,#58517,#58518),
 .UNSPECIFIED.,.F.,.F.,(4,4),(-0.0228763908153357,0.),.UNSPECIFIED.);
#693=B_SPLINE_CURVE_WITH_KNOTS('',3,(#59389,#59390,#59391,#59392,#59393,
#59394,#59395,#59396,#59397,#59398,#59399,#59400,#59401,#59402,#59403,#59404,
#59405,#59406,#59407,#59408,#59409,#59410,#59411,#59412,#59413,#59414,#59415,
#59416,#59417,#59418,#59419,#59420,#59421,#59422,#59423,#59424,#59425,#59426,
#59427,#59428,#59429,#59430,#59431,#59432,#59433,#59434,#59435,#59436,#59437,
#59438,#59439,#59440,#59441,#59442,#59443,#59444,#59445,#59446,#59447,#59448,
#59449,#59450,#59451,#59452,#59453,#59454,#59455,#59456,#59457,#59458,#59459,
#59460,#59461,#59462,#59463,#59464,#59465,#59466,#59467,#59468,#59469,#59470,
#59471,#59472,#59473,#59474,#59475,#59476,#59477,#59478,#59479,#59480,#59481,
#59482,#59483,#59484,#59485,#59486,#59487,#59488,#59489,#59490,#59491,#59492,
#59493,#59494,#59495,#59496,#59497,#59498,#59499,#59500,#59501,#59502,#59503,
#59504,#59505,#59506,#59507,#59508,#59509,#59510,#59511,#59512,#59513,#59514,
#59515),.UNSPECIFIED.,.F.,.F.,(4,3,3,3,3,3,3,3,3,3,3,3,3,3,3,3,3,3,3,3,
3,3,3,3,3,3,3,3,3,3,3,3,3,3,3,3,3,3,3,3,3,3,4),(10.3244224454295,10.3347762602768,
10.4523755104341,10.5697567932924,10.687017805337,10.8042083393309,10.921378073836,
11.0386591521697,11.1560016504262,11.273559681505,11.3324641798094,11.4501570625527,
11.5676398197509,11.6850070752187,11.8023084152573,11.9195933182444,12.0369952827684,
12.1544620980084,12.2721483369573,12.3301520993421,12.4475267014295,12.5646823078878,
12.6817172043898,12.7986816223694,12.9156256782421,13.032683561123,13.1498039510826,
13.2671442032613,13.3278400188747,13.4453614082309,13.5626664785529,13.6798523713343,
13.7969690317053,13.9140662920102,14.0312776252005,14.1485518345722,14.2660446675354,
14.3255279384074,14.4430457990983,14.5603521333803,14.6775359904871,14.7946582937227,
14.8497137389722),.UNSPECIFIED.);
#694=B_SPLINE_CURVE_WITH_KNOTS('',3,(#59518,#59519,#59520,#59521,#59522,
#59523,#59524,#59525,#59526,#59527,#59528,#59529,#59530,#59531,#59532,#59533,
#59534,#59535,#59536,#59537,#59538,#59539,#59540,#59541,#59542,#59543,#59544,
#59545,#59546,#59547,#59548,#59549,#59550,#59551,#59552,#59553,#59554,#59555,
#59556,#59557,#59558,#59559,#59560,#59561,#59562,#59563,#59564,#59565,#59566,
#59567,#59568,#59569,#59570,#59571,#59572,#59573,#59574,#59575,#59576,#59577,
#59578,#59579,#59580,#59581,#59582,#59583,#59584,#59585,#59586,#59587,#59588,
#59589,#59590,#59591,#59592,#59593,#59594,#59595,#59596,#59597,#59598,#59599,
#59600,#59601,#59602,#59603,#59604,#59605),.UNSPECIFIED.,.F.,.F.,(4,3,3,
3,3,3,3,3,3,3,3,3,3,3,3,3,3,3,3,3,3,3,3,3,3,3,3,3,3,4),(11.6667261296989,
11.7914371196405,11.9115078206976,12.0315495137313,12.1516029751615,12.27170898462,
12.3920043210467,12.5124089010735,12.6330580926368,12.6644140492316,12.7808766559592,
12.8970982188996,13.0131860262978,13.1291919200962,13.2451676019825,13.3612494874271,
13.4773878723687,13.5937483072809,13.6621019687642,13.7797013220772,13.8970827102571,
14.014343828866,14.1315344704521,14.2487043133647,14.3659855004597,14.4833281078319,
14.6008862472843,14.6597898882969,14.7774514636229,14.8502992189952),
 .UNSPECIFIED.);
#695=B_SPLINE_CURVE_WITH_KNOTS('',3,(#59611,#59612,#59613,#59614,#59615,
#59616,#59617,#59618,#59619,#59620,#59621,#59622,#59623,#59624,#59625,#59626,
#59627,#59628,#59629,#59630,#59631,#59632,#59633,#59634,#59635,#59636,#59637,
#59638,#59639,#59640,#59641,#59642,#59643,#59644,#59645,#59646,#59647,#59648,
#59649,#59650,#59651,#59652,#59653,#59654,#59655,#59656,#59657,#59658,#59659,
#59660,#59661,#59662,#59663,#59664,#59665,#59666,#59667,#59668,#59669,#59670,
#59671,#59672,#59673,#59674,#59675,#59676,#59677,#59678,#59679,#59680,#59681,
#59682,#59683,#59684,#59685,#59686,#59687,#59688,#59689,#59690,#59691,#59692,
#59693,#59694,#59695,#59696,#59697,#59698,#59699,#59700,#59701,#59702,#59703,
#59704,#59705,#59706,#59707,#59708,#59709,#59710,#59711,#59712,#59713,#59714,
#59715,#59716,#59717,#59718,#59719,#59720,#59721,#59722,#59723,#59724,#59725,
#59726,#59727,#59728,#59729,#59730,#59731,#59732,#59733,#59734,#59735,#59736,
#59737,#59738,#59739,#59740,#59741,#59742,#59743,#59744,#59745,#59746,#59747,
#59748,#59749,#59750,#59751,#59752,#59753,#59754,#59755,#59756,#59757,#59758),
 .UNSPECIFIED.,.F.,.F.,(4,3,3,3,3,3,3,3,3,3,3,3,3,3,3,3,3,3,3,3,3,3,3,3,
3,3,3,3,3,3,3,3,3,3,3,3,3,3,3,3,3,3,3,3,3,3,3,3,3,4),(15.7079632679489,
15.826189752956,15.9498682590852,16.0683010825115,16.1868385915478,16.3056105526879,
16.3209037774727,16.4384084206739,16.5556968022436,16.6728660565512,16.7899661610164,
16.9070469803279,17.0242421798739,17.1415004071429,17.2589776838822,17.3185916970053,
17.4360947212145,17.5533815374925,17.6705492611684,17.787647872645,17.9047272396398,
18.0219210605523,18.1391779491447,18.2566539655226,18.3162796165379,18.4337783817821,
18.5510608066487,18.6682240606424,18.785318132747,18.9023928991528,19.0195820630453,
19.1368342556321,19.2543055705415,19.3139675360706,19.4314690346998,19.5487542516085,
19.6659203315695,19.7830172581319,19.9000949020984,20.0172869556911,20.134542049137,
20.2520162480687,20.3116554556032,20.4291191392111,20.5464069655919,20.663569125986,
20.78077716451,20.8978784283634,21.0151398542227,21.132401280082),
 .UNSPECIFIED.);
#696=B_SPLINE_CURVE_WITH_KNOTS('',3,(#59759,#59760,#59761,#59762,#59763,
#59764,#59765,#59766,#59767,#59768,#59769,#59770,#59771,#59772,#59773,#59774,
#59775,#59776,#59777,#59778,#59779,#59780),.UNSPECIFIED.,.F.,.F.,(4,3,3,
3,3,3,3,4),(14.8497137389722,14.9680892687142,15.0853285498675,15.2042722039037,
15.32321585794,15.4550717956996,15.5859966424603,15.7079632672096),
 .UNSPECIFIED.);
#697=B_SPLINE_CURVE_WITH_KNOTS('',3,(#59782,#59783,#59784,#59785,#59786,
#59787,#59788,#59789,#59790,#59791,#59792,#59793,#59794,#59795,#59796,#59797,
#59798,#59799,#59800,#59801,#59802,#59803,#59804,#59805,#59806),
 .UNSPECIFIED.,.F.,.F.,(4,3,3,3,3,3,3,3,4),(14.8502992189952,14.967704568568,
15.0850251599573,15.2023105050779,15.3196994923041,15.4371364444717,15.5548075604255,
15.6574778078295,15.707963267949),.UNSPECIFIED.);
#698=B_SPLINE_CURVE_WITH_KNOTS('',3,(#59807,#59808,#59809,#59810,#59811,
#59812,#59813,#59814,#59815,#59816,#59817,#59818,#59819,#59820,#59821,#59822,
#59823,#59824,#59825,#59826,#59827,#59828,#59829,#59830,#59831,#59832,#59833,
#59834,#59835,#59836,#59837,#59838,#59839,#59840,#59841,#59842,#59843,#59844,
#59845,#59846,#59847,#59848,#59849,#59850,#59851,#59852,#59853,#59854,#59855,
#59856,#59857,#59858,#59859,#59860,#59861,#59862,#59863,#59864,#59865,#59866,
#59867,#59868,#59869,#59870,#59871,#59872,#59873,#59874,#59875,#59876,#59877,
#59878,#59879,#59880,#59881,#59882,#59883,#59884,#59885,#59886,#59887,#59888,
#59889,#59890,#59891,#59892,#59893,#59894,#59895,#59896,#59897,#59898,#59899,
#59900,#59901,#59902,#59903,#59904,#59905,#59906,#59907,#59908,#59909,#59910,
#59911,#59912,#59913,#59914,#59915,#59916,#59917,#59918,#59919,#59920,#59921,
#59922,#59923,#59924,#59925,#59926,#59927,#59928,#59929,#59930,#59931,#59932,
#59933,#59934,#59935,#59936,#59937,#59938),.UNSPECIFIED.,.F.,.F.,(4,2,2,
2,2,2,2,2,2,2,2,2,2,2,2,2,2,2,2,2,2,2,2,2,2,2,2,2,2,2,2,2,2,2,2,2,2,2,2,
2,2,2,2,2,2,2,2,2,2,2,2,2,2,2,2,2,2,2,2,2,2,2,2,2,2,4),(-1.60493377957124,
-1.59987050848402,-1.57873903548264,-1.5648359244767,-1.55461258883571,
-1.54874460226824,-1.54328239853955,-1.53555119059207,-1.51169698163715,
-1.49725423878715,-1.48864381489348,-1.4848726374927,-1.48176283324838,
-1.47715240856349,-1.45189900306032,-1.43756837907325,-1.42713333431231,
-1.42119940320615,-1.4156983768377,-1.40793791028021,-1.38588980103349,
-1.37045291892543,-1.36151402510944,-1.35767587646358,-1.35455596745909,
-1.34996766518868,-1.32452284345291,-1.31030162976917,-1.29992164311062,
-1.29400218866262,-1.288506604496,-1.28074346759365,-1.25749367219419,-1.24276389961884,
-1.23405212812915,-1.23025149730065,-1.2271349817491,-1.22252046117701,
-1.19733279743846,-1.18298886558583,-1.17255509215521,-1.16663137082758,
-1.161147151725,-1.15342827229919,-1.12924645011164,-1.11509233685587,-1.10657725173874,
-1.10280684884489,-1.09968391211381,-1.09501762992913,-1.07028877408506,
-1.05573899165196,-1.04521151415666,-1.03926822881994,-1.03378261817331,
-1.02608890605539,-1.00149665014118,-0.987597931946931,-0.97917098091361,
-0.975410759328862,-0.972282483199418,-0.96758493485304,-0.943147114271868,
-0.928468919189071,-0.917885814304118,-0.912322913525635),.UNSPECIFIED.);
#699=B_SPLINE_CURVE_WITH_KNOTS('',3,(#59944,#59945,#59946,#59947,#59948,
#59949,#59950,#59951,#59952,#59953),.UNSPECIFIED.,.F.,.F.,(4,1,1,1,1,1,
1,4),(21.9911547274662,22.3070312946685,23.3047192142012,24.3024071337338,
25.3000950532664,26.2977829727991,27.2954708923317,27.4168377020878),
 .UNSPECIFIED.);
#700=B_SPLINE_CURVE_WITH_KNOTS('',3,(#59954,#59955,#59956,#59957,#59958,
#59959,#59960,#59961,#59962,#59963,#59964,#59965,#59966,#59967,#59968,#59969,
#59970,#59971,#59972,#59973,#59974,#59975,#59976,#59977,#59978),
 .UNSPECIFIED.,.F.,.F.,(4,3,3,3,3,3,3,3,4),(21.132401280082,21.24987516791,
21.3093433751359,21.4264262274341,21.543322914988,21.6600916557656,21.7767813160478,
21.8934986553372,21.9911485751285),.UNSPECIFIED.);
#701=B_SPLINE_CURVE_WITH_KNOTS('',3,(#59979,#59980,#59981,#59982,#59983,
#59984,#59985,#59986,#59987,#59988,#59989,#59990,#59991,#59992,#59993,#59994,
#59995,#59996,#59997,#59998,#59999,#60000,#60001,#60002,#60003,#60004,#60005,
#60006,#60007,#60008,#60009,#60010,#60011,#60012,#60013,#60014,#60015,#60016,
#60017,#60018,#60019,#60020,#60021,#60022,#60023,#60024,#60025,#60026,#60027,
#60028,#60029,#60030,#60031,#60032,#60033,#60034,#60035,#60036,#60037,#60038,
#60039,#60040,#60041,#60042,#60043,#60044,#60045,#60046,#60047,#60048,#60049,
#60050,#60051,#60052,#60053,#60054,#60055,#60056,#60057,#60058,#60059,#60060,
#60061,#60062,#60063,#60064,#60065,#60066,#60067,#60068,#60069,#60070,#60071,
#60072,#60073,#60074,#60075,#60076,#60077,#60078,#60079,#60080,#60081,#60082,
#60083,#60084,#60085,#60086,#60087,#60088,#60089,#60090,#60091,#60092,#60093,
#60094,#60095,#60096,#60097,#60098,#60099,#60100,#60101,#60102,#60103,#60104,
#60105,#60106,#60107,#60108,#60109,#60110,#60111,#60112,#60113,#60114,#60115,
#60116,#60117,#60118,#60119,#60120,#60121,#60122,#60123,#60124,#60125,#60126,
#60127,#60128,#60129,#60130,#60131,#60132,#60133,#60134),.UNSPECIFIED.,
 .F.,.F.,(4,2,2,2,2,2,2,2,2,2,2,2,2,2,2,2,2,2,2,2,2,2,2,2,2,2,2,2,2,2,2,
2,2,2,2,2,2,2,2,2,2,2,2,2,2,2,2,2,2,2,2,2,2,2,2,2,2,2,2,2,2,2,2,2,2,2,2,
2,2,2,2,2,2,2,2,2,2,4),(-0.912322913525635,-0.911934213429162,-0.906453142965189,
-0.898787260140372,-0.879414340197368,-0.858265688943076,-0.851153416297868,
-0.847603568824797,-0.844442247367097,-0.83930043026472,-0.820203687819216,
-0.802826045528258,-0.791154694853652,-0.785032783277211,-0.779599803321779,
-0.772326703986733,-0.749367388765553,-0.727078572155622,-0.722152171413902,
-0.719024174275046,-0.71539076438579,-0.707779059166838,-0.696050432795616,
-0.666943894355935,-0.659817099380472,-0.65438565197958,-0.648253517458123,
-0.636518001640174,-0.61896776714075,-0.600080746878765,-0.594948576159234,
-0.591788718033106,-0.588234959186982,-0.581099904991374,-0.559933117993286,
-0.540654512818056,-0.532995259329514,-0.527515290701031,-0.521561513614715,
-0.510965354953334,-0.496256999783314,-0.471830933835663,-0.467128044760812,
-0.463999773517692,-0.460244777094813,-0.451847253290902,-0.438031839855466,
-0.413316089936075,-0.405633971576458,-0.400151068729167,-0.394206016891429,
-0.383662826190182,-0.369075146164618,-0.344381314246961,-0.339707249571018,
-0.336582537398261,-0.332812105706658,-0.324309442893067,-0.310192603935533,
-0.286007069481154,-0.278290719175982,-0.272803145618507,-0.266870405857176,
-0.256402921158967,-0.241986607365549,-0.216907104545424,-0.212274690725974,
-0.209154858986032,-0.205361231085055,-0.19669793812975,-0.182109284583203,
-0.158703230132587,-0.150951523297094,-0.145459124057986,-0.13953890466759,
-0.129147838899375,-0.114902840850451,-0.110035658503537),.UNSPECIFIED.);
#702=B_SPLINE_CURVE_WITH_KNOTS('',3,(#60140,#60141,#60142,#60143,#60144,
#60145,#60146,#60147,#60148,#60149,#60150,#60151,#60152,#60153,#60154,#60155,
#60156,#60157,#60158,#60159,#60160,#60161,#60162,#60163,#60164,#60165,#60166,
#60167,#60168,#60169,#60170,#60171,#60172,#60173,#60174,#60175,#60176,#60177,
#60178,#60179,#60180,#60181,#60182,#60183,#60184,#60185,#60186,#60187,#60188,
#60189,#60190,#60191,#60192,#60193,#60194,#60195,#60196,#60197,#60198,#60199,
#60200,#60201,#60202,#60203,#60204,#60205,#60206,#60207,#60208,#60209,#60210,
#60211,#60212,#60213,#60214,#60215,#60216,#60217,#60218,#60219,#60220,#60221,
#60222,#60223,#60224,#60225,#60226,#60227,#60228,#60229,#60230,#60231,#60232,
#60233,#60234,#60235,#60236,#60237,#60238,#60239,#60240,#60241,#60242,#60243,
#60244,#60245,#60246,#60247,#60248,#60249,#60250,#60251,#60252,#60253,#60254,
#60255,#60256,#60257,#60258,#60259,#60260,#60261,#60262,#60263,#60264,#60265,
#60266,#60267,#60268,#60269,#60270,#60271,#60272,#60273,#60274,#60275,#60276,
#60277,#60278,#60279,#60280,#60281,#60282,#60283,#60284,#60285,#60286,#60287,
#60288,#60289,#60290),.UNSPECIFIED.,.F.,.F.,(4,3,3,3,3,3,3,3,3,3,3,3,3,
3,3,3,3,3,3,3,3,3,3,3,3,3,3,3,3,3,3,3,3,3,3,3,3,3,3,3,3,3,3,3,3,3,3,3,3,
3,4),(28.2743338823081,28.2931588118644,28.4106596979302,28.5279442948967,
28.6451097508825,28.7622060506395,28.8792830661675,28.996474493875,29.1137289619717,
29.2312025437845,29.290846731397,29.4083476154735,29.5256322104213,29.642797664372,
29.7598939620814,29.8769709755534,29.9941624012081,30.1114168672509,30.2288904470325,
30.2885346509297,30.4060355346255,30.5233201291716,30.6404855827079,30.7575818799911,
30.8746588930257,30.9918503182297,31.1091047838135,31.2265783631284,31.2862225704623,
31.4037234548693,31.5210080501455,31.638173504423,31.755269802457,31.8723468162507,
31.9895382422202,32.1067927085743,32.2242662886579,32.283910489995,32.4014113741103,
32.5186959690898,32.6358614230678,32.7529577208,32.8700347342901,32.987226159956,
33.104480626006,33.2219542057883,33.2815984095276,33.399060761611,33.5163536756721,
33.633518003233,33.6995974475487),.UNSPECIFIED.);
#703=B_SPLINE_CURVE_WITH_KNOTS('',3,(#60291,#60292,#60293,#60294),
 .UNSPECIFIED.,.F.,.F.,(4,4),(27.4168377020878,28.27433136801),
 .UNSPECIFIED.);
#704=B_SPLINE_CURVE_WITH_KNOTS('',3,(#60296,#60297,#60298,#60299,#60300,
#60301,#60302,#60303,#60304,#60305,#60306,#60307,#60308,#60309,#60310,#60311,
#60312,#60313,#60314,#60315,#60316,#60317,#60318,#60319,#60320,#60321),
 .UNSPECIFIED.,.F.,.F.,(4,2,2,2,2,2,2,2,2,2,2,2,4),(-0.110035658503537,
-0.0894303473050645,-0.0848411241296203,-0.0817261029194477,-0.0779073952651996,
-0.0690669192919908,-0.0472928151504454,-0.0292032109585574,-0.0223105991302409,
-0.0169104081760242,-0.0118102046580991,-0.00662420233944239,-0.000375289463787094),
 .UNSPECIFIED.);
#705=B_SPLINE_CURVE_WITH_KNOTS('',3,(#60322,#60323,#60324,#60325,#60326,
#60327,#60328,#60329,#60330,#60331),.UNSPECIFIED.,.F.,.F.,(4,1,1,1,1,1,
1,4),(28.2743410485279,28.6274207617539,29.6251086812865,30.6227966008192,
31.6204845203518,32.6181724398845,33.6158603594171,33.6998501991794),
 .UNSPECIFIED.);
#706=B_SPLINE_CURVE_WITH_KNOTS('',3,(#60337,#60338,#60339,#60340,#60341,
#60342,#60343,#60344,#60345),.UNSPECIFIED.,.F.,.F.,(4,1,1,1,1,1,4),(34.5575191894877,
35.2769742485929,36.2746621681255,37.2723500876582,38.2700380071908,39.2677259267235,
39.9816638270269),.UNSPECIFIED.);
#707=B_SPLINE_CURVE_WITH_KNOTS('',3,(#60346,#60347,#60348,#60349,#60350,
#60351,#60352,#60353,#60354,#60355,#60356,#60357,#60358,#60359,#60360,#60361,
#60362,#60363,#60364,#60365,#60366,#60367),.UNSPECIFIED.,.F.,.F.,(4,3,3,
3,3,3,3,4),(33.6995974475487,33.8166767415956,33.9338547022906,34.0510762006772,
34.1685337552212,34.2792863290602,34.4251381581413,34.5575191894877),
 .UNSPECIFIED.);
#708=B_SPLINE_CURVE_WITH_KNOTS('',3,(#60369,#60370,#60371,#60372),
 .UNSPECIFIED.,.F.,.F.,(4,4),(33.6998501991794,34.5575124975197),
 .UNSPECIFIED.);
#709=B_SPLINE_CURVE_WITH_KNOTS('',3,(#60373,#60374,#60375,#60376,#60377,
#60378,#60379,#60380,#60381,#60382,#60383,#60384,#60385,#60386,#60387,#60388,
#60389,#60390,#60391,#60392,#60393,#60394,#60395,#60396,#60397,#60398,#60399,
#60400,#60401,#60402,#60403,#60404,#60405,#60406,#60407,#60408,#60409,#60410,
#60411,#60412,#60413,#60414,#60415,#60416,#60417,#60418,#60419,#60420,#60421,
#60422,#60423,#60424,#60425,#60426,#60427,#60428,#60429,#60430,#60431,#60432,
#60433,#60434,#60435,#60436,#60437,#60438,#60439,#60440,#60441,#60442,#60443,
#60444,#60445,#60446,#60447,#60448,#60449,#60450,#60451,#60452,#60453,#60454,
#60455,#60456,#60457,#60458,#60459,#60460,#60461,#60462,#60463,#60464,#60465,
#60466,#60467,#60468,#60469,#60470,#60471,#60472,#60473,#60474,#60475,#60476,
#60477,#60478,#60479,#60480,#60481,#60482,#60483,#60484,#60485,#60486,#60487,
#60488,#60489,#60490,#60491,#60492,#60493,#60494,#60495,#60496,#60497,#60498,
#60499,#60500,#60501,#60502,#60503,#60504,#60505,#60506,#60507,#60508,#60509,
#60510),.UNSPECIFIED.,.F.,.F.,(4,2,2,2,2,2,2,2,2,2,2,2,2,2,2,2,2,2,2,2,
2,2,2,2,2,2,2,2,2,2,2,2,2,2,2,2,2,2,2,2,2,2,2,2,2,2,2,2,2,2,2,2,2,2,2,2,
2,2,2,2,2,2,2,2,2,2,2,2,4),(-1.60459719055946,-1.60178300272715,-1.59909075093962,
-1.59628461001764,-1.59236418356326,-1.5833727425585,-1.5722137340225,-1.55111601522325,
-1.54075620618843,-1.53484335691492,-1.52935184120328,-1.52159118596671,
-1.49857215188127,-1.4837211004988,-1.47497180794081,-1.47116706137049,
-1.46805121871521,-1.46344367854927,-1.43820349813744,-1.42389164310272,
-1.41347210593244,-1.40754925737045,-1.40206130202897,-1.39432808903217,
-1.37046814396921,-1.35614401031577,-1.34757135725019,-1.34379175533296,
-1.34067063425579,-1.3360182526735,-1.31118737489542,-1.29669394191008,
-1.28619358587361,-1.28025730799103,-1.27477405070355,-1.26707709862348,
-1.24256716076334,-1.22862131963994,-1.22017908177656,-1.21641834587374,
-1.21329281820254,-1.20860514426719,-1.18409967261904,-1.16945948900438,
-1.15889436100026,-1.15294727887949,-1.14746751063494,-1.13979855686478,
-1.1105184887593,-1.0995710482709,-1.0922829839777,-1.08870398743655,-1.08555668711595,
-1.08049892228391,-1.06041648563823,-1.04356751459763,-1.0320968106417,
-1.02600645043121,-1.02056807886404,-1.01323587052882,-0.985107442701769,
-0.972946762200217,-0.965164547068087,-0.961504382705103,-0.958386055406396,
-0.953524227222894,-0.930646036895216,-0.915256780825494,-0.912207559110817),
 .UNSPECIFIED.);
#710=B_SPLINE_CURVE_WITH_KNOTS('',3,(#60516,#60517,#60518,#60519,#60520,
#60521,#60522,#60523,#60524,#60525,#60526,#60527,#60528,#60529,#60530,#60531,
#60532,#60533,#60534,#60535,#60536,#60537,#60538,#60539,#60540,#60541,#60542,
#60543,#60544,#60545,#60546,#60547,#60548,#60549,#60550,#60551,#60552,#60553,
#60554,#60555,#60556,#60557,#60558,#60559,#60560,#60561,#60562,#60563,#60564,
#60565,#60566,#60567,#60568,#60569,#60570,#60571,#60572,#60573,#60574,#60575,
#60576,#60577,#60578,#60579,#60580,#60581,#60582,#60583,#60584,#60585,#60586,
#60587,#60588,#60589,#60590,#60591,#60592,#60593,#60594,#60595,#60596,#60597,
#60598,#60599,#60600,#60601,#60602,#60603,#60604,#60605,#60606,#60607,#60608,
#60609,#60610,#60611,#60612,#60613,#60614,#60615,#60616,#60617,#60618,#60619,
#60620,#60621,#60622,#60623,#60624,#60625,#60626,#60627,#60628,#60629,#60630,
#60631,#60632,#60633,#60634,#60635,#60636,#60637,#60638,#60639,#60640,#60641,
#60642,#60643,#60644,#60645,#60646,#60647,#60648,#60649),.UNSPECIFIED.,
 .F.,.F.,(4,2,2,2,2,2,2,2,2,2,2,2,2,2,2,2,2,2,2,2,2,2,2,2,2,2,2,2,2,2,2,
2,2,2,2,2,2,2,2,2,2,2,2,2,2,2,2,2,2,2,2,2,2,2,2,2,2,2,2,2,2,2,2,2,2,2,4),
(-0.692954581112378,-0.690107125872129,-0.686278982582345,-0.677373495051638,
-0.662046489541168,-0.639752470891751,-0.631985260140913,-0.626489929875214,
-0.620573383190546,-0.610208902127747,-0.596023681417976,-0.570414862652245,
-0.565840706522337,-0.562726803929921,-0.558897581131768,-0.549984389854336,
-0.534633358682857,-0.512373323730011,-0.504606311021614,-0.499110991348438,
-0.493194343690737,-0.482829345411824,-0.468643009062657,-0.443036561584647,
-0.438462109864493,-0.435348166185292,-0.431519097085452,-0.422607085052476,
-0.407259789393917,-0.384994282016187,-0.377227200757971,-0.371731854577023,
-0.36581519746099,-0.355450240397643,-0.341264029676267,-0.315657064695619,
-0.311082642573696,-0.307968691858849,-0.304139579431889,-0.29522732708495,
-0.279879328197489,-0.257614650002929,-0.249847545373831,-0.244352178954194,
-0.238435496831611,-0.228070486209916,-0.213884190487116,-0.188277197981138,
-0.183702750285698,-0.180588786759347,-0.176759664444986,-0.167847412637021,
-0.152499463549225,-0.130234545281643,-0.122467409702783,-0.116972022015258,
-0.111055317542599,-0.100690269437631,-0.0865039244304431,-0.0608968211554993,
-0.056322357259471,-0.0532083819119233,-0.0493792440502393,-0.0404669520209199,
-0.0251189252975217,-0.00796884978255691,-0.000386348129261924),
 .UNSPECIFIED.);
#711=B_SPLINE_CURVE_WITH_KNOTS('',3,(#60650,#60651,#60652,#60653,#60654),
 .UNSPECIFIED.,.F.,.F.,(4,1,4),(39.9816638270269,40.2654138462561,40.8407044966673),
 .UNSPECIFIED.);
#712=B_SPLINE_CURVE_WITH_KNOTS('',3,(#60655,#60656,#60657,#60658,#60659,
#60660,#60661,#60662,#60663,#60664,#60665,#60666,#60667,#60668,#60669,#60670,
#60671,#60672,#60673,#60674,#60675,#60676,#60677,#60678,#60679,#60680,#60681,
#60682,#60683,#60684,#60685,#60686,#60687,#60688,#60689,#60690,#60691,#60692,
#60693,#60694,#60695,#60696,#60697,#60698,#60699,#60700,#60701,#60702,#60703,
#60704,#60705,#60706,#60707,#60708,#60709,#60710,#60711,#60712,#60713,#60714,
#60715,#60716,#60717,#60718,#60719,#60720,#60721,#60722,#60723,#60724,#60725,
#60726,#60727,#60728,#60729,#60730,#60731,#60732,#60733,#60734,#60735,#60736,
#60737,#60738,#60739,#60740,#60741,#60742,#60743,#60744,#60745,#60746,#60747,
#60748,#60749,#60750,#60751,#60752,#60753,#60754,#60755,#60756,#60757,#60758,
#60759,#60760,#60761,#60762,#60763,#60764,#60765,#60766,#60767,#60768,#60769,
#60770,#60771,#60772,#60773,#60774,#60775,#60776,#60777,#60778,#60779,#60780,
#60781,#60782,#60783,#60784,#60785,#60786,#60787,#60788,#60789,#60790,#60791,
#60792,#60793,#60794,#60795,#60796,#60797,#60798,#60799,#60800,#60801,#60802,
#60803,#60804,#60805,#60806,#60807,#60808,#60809,#60810),.UNSPECIFIED.,
 .F.,.F.,(4,2,2,2,2,2,2,2,2,2,2,2,2,2,2,2,2,2,2,2,2,2,2,2,2,2,2,2,2,2,2,
2,2,2,2,2,2,2,2,2,2,2,2,2,2,2,2,2,2,2,2,2,2,2,2,2,2,2,2,2,2,2,2,2,2,2,2,
2,2,2,2,2,2,2,2,2,2,4),(-0.912207559110817,-0.904370165018042,-0.898370552967401,
-0.892906950896839,-0.885368518653862,-0.859004877746807,-0.846026001349283,
-0.837931341722297,-0.834222107250463,-0.831082361507067,-0.826290219671332,
-0.802745556480474,-0.781907852870987,-0.774180285949588,-0.768691256216211,
-0.762762661445065,-0.752320124607763,-0.737959821906094,-0.712753076978956,
-0.708134615440343,-0.705016407763125,-0.701214897319066,-0.692496119353534,
-0.677741073643799,-0.654596569845275,-0.646837505688292,-0.641344129898751,
-0.635426541025622,-0.625051280915556,-0.610841403772924,-0.585288240426161,
-0.580708109696272,-0.577594080775163,-0.573769985347027,-0.564890782074043,
-0.5496450193943,-0.527232792518649,-0.519465674065646,-0.513971162216523,
-0.508056312617709,-0.497697863482222,-0.483525402616645,-0.457884935306767,
-0.453314591437652,-0.450201581226279,-0.446371545490143,-0.437449679017519,
-0.422070873728227,-0.399848281471212,-0.392082141709777,-0.386587747014567,
-0.380672524523701,-0.37031191181269,-0.356134682483944,-0.330505082013807,
-0.32593348053507,-0.322820327675395,-0.318991027074598,-0.310074542004067,
-0.294712639716686,-0.272465930605739,-0.264699561163723,-0.259205115734093,
-0.253289935586837,-0.242929690592456,-0.228753315889827,-0.20312147323728,
-0.198550092769763,-0.195436951782767,-0.191607488944604,-0.182689913914197,
-0.167324653862376,-0.145082514942491,-0.137316149014768,-0.131821685233644,
-0.125906467248585,-0.115546101238224,-0.109987797047057),.UNSPECIFIED.);
#713=B_SPLINE_CURVE_WITH_KNOTS('',3,(#60815,#60816,#60817,#60818,#60819,
#60820,#60821,#60822,#60823,#60824,#60825,#60826,#60827,#60828,#60829,#60830,
#60831,#60832,#60833,#60834,#60835,#60836,#60837,#60838,#60839,#60840,#60841,
#60842,#60843,#60844,#60845,#60846,#60847,#60848,#60849,#60850,#60851,#60852,
#60853,#60854,#60855,#60856,#60857,#60858,#60859,#60860,#60861,#60862,#60863,
#60864,#60865,#60866,#60867,#60868,#60869,#60870,#60871,#60872,#60873,#60874,
#60875,#60876,#60877,#60878,#60879,#60880,#60881,#60882,#60883,#60884,#60885,
#60886,#60887,#60888,#60889,#60890,#60891,#60892,#60893,#60894,#60895,#60896,
#60897,#60898,#60899,#60900,#60901,#60902,#60903,#60904,#60905,#60906,#60907,
#60908,#60909,#60910,#60911,#60912,#60913,#60914,#60915,#60916,#60917,#60918,
#60919,#60920,#60921,#60922,#60923,#60924,#60925,#60926,#60927,#60928,#60929,
#60930,#60931,#60932,#60933,#60934,#60935,#60936,#60937,#60938,#60939,#60940,
#60941,#60942,#60943,#60944,#60945,#60946,#60947,#60948,#60949,#60950,#60951,
#60952,#60953,#60954,#60955,#60956,#60957,#60958,#60959,#60960,#60961,#60962,
#60963,#60964,#60965,#60966,#60967,#60968,#60969,#60970),.UNSPECIFIED.,
 .F.,.F.,(4,2,2,2,2,2,2,2,2,2,2,2,2,2,2,2,2,2,2,2,2,2,2,2,2,2,2,2,2,2,2,
2,2,2,2,2,2,2,2,2,2,2,2,2,2,2,2,2,2,2,2,2,2,2,2,2,2,2,2,2,2,2,2,2,2,2,2,
2,2,2,2,2,2,2,2,2,2,4),(-1.49501924537234,-1.4813148627293,-1.4680560708403,
-1.45985967772397,-1.45613571858057,-1.45300108845073,-1.44824188592874,
-1.42441831558675,-1.40947559509268,-1.39877973307688,-1.39281157526604,
-1.38733914050731,-1.37972551975406,-1.36135837627754,-1.3392218732596,
-1.33204697502592,-1.32848721336543,-1.32533156571223,-1.3202210330441,
-1.30334686340635,-1.28450939122364,-1.27232355275591,-1.26612681232264,
-1.26070911642611,-1.25370128228088,-1.223683914122,-1.21231884988458,-1.20485647270919,
-1.20124821922491,-1.19811194125785,-1.19312727429328,-1.16698170234289,
-1.14721464618892,-1.1402747148536,-1.13487197761727,-1.12855288409598,
-1.11549579071886,-1.09015955699211,-1.0845256833055,-1.07735056944568,
-1.07379032513158,-1.07063398630341,-1.06552193230557,-1.04852546653233,
-1.02976380151225,-1.01760252893791,-1.01140849831093,-1.00598913462564,
-0.998973454584765,-0.968999378925303,-0.957612454266797,-0.950140546560794,
-0.946530264797707,-0.94339388808695,-0.93841158710968,-0.916919533769083,
-0.900843325589779,-0.895540675846777,-0.887302561368203,-0.881737349025378,
-0.875957444673054,-0.866415137657659,-0.836302707806108,-0.824285207096203,
-0.820102754030312,-0.817013494298257,-0.812957478266099,-0.802620066898701,
-0.781287309984028,-0.764815006180216,-0.757981913640745,-0.752583991849499,
-0.746183167213547,-0.732509174772806,-0.708505726807608,-0.69705333904176,
-0.693221201266409,-0.692954581112378),.UNSPECIFIED.);
#714=B_SPLINE_CURVE_WITH_KNOTS('',3,(#60972,#60973,#60974,#60975,#60976,
#60977,#60978,#60979,#60980,#60981,#60982,#60983,#60984,#60985,#60986,#60987,
#60988,#60989,#60990,#60991,#60992,#60993,#60994,#60995),.UNSPECIFIED.,
 .F.,.F.,(4,2,2,2,2,2,2,2,2,2,2,4),(-0.109987797047057,-0.101369495396899,
-0.075737941276712,-0.0711664964469346,-0.0680533374928693,-0.0642238855499439,
-0.0553064687578774,-0.0311046932610105,-0.0150614501695526,-0.00846605047845859,
-0.00415225361026194,-0.000375256628440777),.UNSPECIFIED.);
#715=B_SPLINE_CURVE_WITH_KNOTS('',3,(#60996,#60997,#60998,#60999,#61000,
#61001,#61002,#61003,#61004,#61005,#61006,#61007,#61008,#61009,#61010,#61011,
#61012,#61013,#61014,#61015,#61016,#61017,#61018,#61019,#61020,#61021,#61022,
#61023,#61024,#61025,#61026,#61027,#61028,#61029,#61030,#61031,#61032,#61033,
#61034,#61035,#61036,#61037,#61038,#61039,#61040,#61041,#61042,#61043,#61044,
#61045,#61046,#61047,#61048,#61049,#61050,#61051,#61052,#61053,#61054,#61055,
#61056,#61057,#61058,#61059,#61060,#61061,#61062,#61063,#61064,#61065,#61066,
#61067,#61068,#61069,#61070,#61071,#61072,#61073,#61074,#61075,#61076,#61077,
#61078,#61079,#61080,#61081,#61082,#61083,#61084,#61085,#61086,#61087,#61088,
#61089,#61090,#61091,#61092,#61093,#61094,#61095,#61096,#61097,#61098,#61099,
#61100,#61101,#61102,#61103,#61104,#61105,#61106,#61107,#61108,#61109,#61110,
#61111,#61112,#61113,#61114,#61115,#61116,#61117,#61118,#61119,#61120,#61121,
#61122,#61123,#61124,#61125,#61126,#61127,#61128,#61129),.UNSPECIFIED.,
 .F.,.F.,(4,2,2,2,2,2,2,2,2,2,2,2,2,2,2,2,2,2,2,2,2,2,2,2,2,2,2,2,2,2,2,
2,2,2,2,2,2,2,2,2,2,2,2,2,2,2,2,2,2,2,2,2,2,2,2,2,2,2,2,2,2,2,2,2,2,2,4),
(-1.60449821208469,-1.60117471261476,-1.5964950956904,-1.57927261005758,
-1.55964101744956,-1.55073034444578,-1.54690289634666,-1.54379106829042,
-1.5392214159838,-1.51363830730631,-1.49947413214974,-1.48912065473405,
-1.48320849903881,-1.47771605866567,-1.46995134538992,-1.44716422048722,
-1.43215693757249,-1.42335600900917,-1.41954376404826,-1.41642901785842,
-1.41183336949047,-1.38647980163793,-1.37221523595865,-1.36181650035951,
-1.35589671095472,-1.35040691634006,-1.34266296414325,-1.31903487511374,
-1.30456705053649,-1.29594528770798,-1.29215839630123,-1.28903848600272,
-1.28439822543246,-1.25944944744898,-1.24500617328139,-1.23452766812593,
-1.22859461485906,-1.22310952751012,-1.21540170343605,-1.19105122703047,
-1.1770120704431,-1.16853703489118,-1.16477128929525,-1.16164658806205,
-1.15696730819572,-1.13237787336056,-1.11777328673824,-1.10722343391458,
-1.10127850483346,-1.09579736075833,-1.08812072654645,-1.06330042126066,
-1.04952425952151,-1.04114113150227,-1.03738875342865,-1.03426069615257,
-1.02955558930728,-1.00520370460247,-0.990490798635368,-0.979893298103208,
-0.973940345202394,-0.968461572877665,-0.960804945540949,-0.941597207766749,
-0.920368754853509,-0.913200300898691,-0.91205896481613),.UNSPECIFIED.);
#716=B_SPLINE_CURVE_WITH_KNOTS('',3,(#61135,#61136,#61137,#61138,#61139,
#61140,#61141,#61142,#61143,#61144,#61145,#61146,#61147,#61148,#61149,#61150,
#61151,#61152,#61153,#61154,#61155,#61156,#61157,#61158,#61159,#61160,#61161,
#61162,#61163,#61164,#61165,#61166,#61167,#61168,#61169,#61170,#61171,#61172,
#61173,#61174,#61175,#61176,#61177,#61178,#61179,#61180,#61181,#61182,#61183,
#61184,#61185,#61186,#61187,#61188,#61189,#61190,#61191,#61192,#61193,#61194,
#61195,#61196,#61197,#61198,#61199,#61200,#61201,#61202,#61203,#61204,#61205,
#61206,#61207,#61208,#61209,#61210,#61211,#61212,#61213,#61214,#61215,#61216,
#61217,#61218,#61219,#61220,#61221,#61222,#61223,#61224,#61225,#61226,#61227,
#61228,#61229,#61230,#61231,#61232,#61233,#61234,#61235,#61236,#61237,#61238,
#61239,#61240,#61241,#61242,#61243,#61244,#61245,#61246,#61247,#61248,#61249,
#61250,#61251,#61252,#61253,#61254,#61255,#61256,#61257,#61258,#61259,#61260,
#61261,#61262,#61263,#61264,#61265,#61266,#61267,#61268),.UNSPECIFIED.,
 .F.,.F.,(4,2,2,2,2,2,2,2,2,2,2,2,2,2,2,2,2,2,2,2,2,2,2,2,2,2,2,2,2,2,2,
2,2,2,2,2,2,2,2,2,2,2,2,2,2,2,2,2,2,2,2,2,2,2,2,2,2,2,2,2,2,2,2,2,2,2,4),
(-0.693092190322639,-0.69015751324097,-0.683629814231713,-0.678135474982164,
-0.672219676221536,-0.66185585975289,-0.647671272007037,-0.622063065460699,
-0.617489398199346,-0.614375868776239,-0.610547105340709,-0.601636182823502,
-0.586291488509274,-0.564025137267241,-0.556258413123572,-0.550763259234434,
-0.544846718803061,-0.534481498986856,-0.520294010175215,-0.494696856336391,
-0.490121956830987,-0.487008036423791,-0.483179390638319,-0.474269339850772,
-0.458927345536385,-0.436657672917112,-0.428891116117865,-0.423396145940555,
-0.417479898096204,-0.407115695748478,-0.392930632900304,-0.367324168061133,
-0.362750151519772,-0.359636451799163,-0.355807641911074,-0.346896099110626,
-0.331549403124372,-0.309285851925463,-0.30151931723584,-0.296024383199857,
-0.290108201420297,-0.279744208456879,-0.265559527413953,-0.239952679004846,
-0.235378741065102,-0.232265027776118,-0.228436081640495,-0.219523849181067,
-0.204175110058433,-0.181914328415961,-0.174147724031108,-0.168652691117248,
-0.1627363451117,-0.152371828144423,-0.138186047639759,-0.112582005190155,
-0.108007722257923,-0.104893934068742,-0.101065105805702,-0.0921537708571086,
-0.0768078722055855,-0.0545429654360646,-0.0467763330896944,-0.0412813060508978,
-0.0353649943164301,-0.0291760048854813,-0.000377328695443869),
 .UNSPECIFIED.);
#717=B_SPLINE_CURVE_WITH_KNOTS('',3,(#61269,#61270,#61271,#61272,#61273,
#61274,#61275,#61276,#61277,#61278,#61279,#61280,#61281,#61282,#61283,#61284,
#61285,#61286,#61287,#61288,#61289,#61290,#61291,#61292,#61293,#61294),
 .UNSPECIFIED.,.F.,.F.,(4,2,2,2,2,2,2,2,2,2,2,2,4),(-1.6044068850231,-1.58965030014154,
-1.58600505033392,-1.58313059790593,-1.57997861077168,-1.57488842166979,
-1.55622031234691,-1.53687287755627,-1.52612913631752,-1.5201536495453,
-1.51468433454594,-1.5070915873584,-1.49501924537234),.UNSPECIFIED.);
#718=B_SPLINE_CURVE_WITH_KNOTS('',3,(#61295,#61296,#61297,#61298,#61299,
#61300,#61301,#61302,#61303,#61304,#61305,#61306,#61307,#61308,#61309,#61310,
#61311,#61312,#61313,#61314,#61315,#61316,#61317,#61318,#61319,#61320,#61321,
#61322,#61323,#61324,#61325,#61326,#61327,#61328,#61329,#61330,#61331,#61332,
#61333,#61334,#61335,#61336,#61337,#61338,#61339,#61340,#61341,#61342,#61343,
#61344,#61345,#61346,#61347,#61348,#61349,#61350,#61351,#61352,#61353,#61354,
#61355,#61356,#61357,#61358,#61359,#61360,#61361,#61362,#61363,#61364,#61365,
#61366,#61367,#61368,#61369,#61370,#61371,#61372,#61373,#61374,#61375,#61376,
#61377,#61378,#61379,#61380,#61381,#61382,#61383,#61384,#61385,#61386,#61387,
#61388,#61389,#61390,#61391,#61392,#61393,#61394,#61395,#61396,#61397,#61398,
#61399,#61400,#61401,#61402,#61403,#61404,#61405,#61406,#61407,#61408,#61409,
#61410,#61411,#61412,#61413,#61414,#61415,#61416,#61417,#61418,#61419,#61420,
#61421,#61422,#61423,#61424,#61425,#61426,#61427,#61428,#61429,#61430,#61431,
#61432,#61433,#61434,#61435,#61436,#61437,#61438,#61439,#61440,#61441,#61442,
#61443,#61444,#61445,#61446,#61447,#61448,#61449,#61450),.UNSPECIFIED.,
 .F.,.F.,(4,2,2,2,2,2,2,2,2,2,2,2,2,2,2,2,2,2,2,2,2,2,2,2,2,2,2,2,2,2,2,
2,2,2,2,2,2,2,2,2,2,2,2,2,2,2,2,2,2,2,2,2,2,2,2,2,2,2,2,2,2,2,2,2,2,2,2,
2,2,2,2,2,2,2,2,2,2,4),(-0.91205896481613,-0.909641274075211,-0.906484757659767,
-0.901370813566233,-0.883580462577556,-0.865336335945879,-0.853353310013507,
-0.847185477149381,-0.841762079830826,-0.834703030030153,-0.802386647355041,
-0.788162487199457,-0.78368682748423,-0.780582916630038,-0.776692340219932,
-0.7673210843246,-0.750468369436933,-0.730191570429174,-0.722488183294921,
-0.717002468854449,-0.711065268165521,-0.700569900903023,-0.686090510172526,
-0.661154549454114,-0.656506695364241,-0.653385135258693,-0.649600352511887,
-0.640998333487524,-0.626591103568252,-0.602893192725773,-0.59515264780876,
-0.589661864442072,-0.583737896584683,-0.573323485776892,-0.559026165743644,
-0.533675502827674,-0.529072911650881,-0.525956483314419,-0.522145786804655,
-0.513361985762053,-0.498409770813735,-0.475566300732396,-0.467801680461069,
-0.462307564151859,-0.456391951088547,-0.446028567705263,-0.431845053560707,
-0.406230905898853,-0.40165767015328,-0.398544387244274,-0.394716183375895,
-0.385807319102666,-0.37046908015249,-0.348189297192809,-0.340422788135625,
-0.334928386813119,-0.329013379124437,-0.318653814887083,-0.304478820778654,
-0.278844633442578,-0.274273621962933,-0.27116054542505,-0.267330907141639,
-0.258411916877638,-0.243042049144117,-0.22080730784035,-0.213041109021085,
-0.207546705730238,-0.201631496399774,-0.191270958101461,-0.177093877680558,
-0.151464194025713,-0.146892634147559,-0.143779507584902,-0.139950258764867,
-0.131033882126756,-0.115672220255292,-0.109848755237784),.UNSPECIFIED.);
#719=B_SPLINE_CURVE_WITH_KNOTS('',3,(#61455,#61456,#61457,#61458,#61459,
#61460,#61461,#61462,#61463,#61464,#61465,#61466,#61467,#61468,#61469,#61470,
#61471,#61472,#61473,#61474,#61475,#61476,#61477,#61478,#61479,#61480,#61481,
#61482,#61483,#61484,#61485,#61486,#61487,#61488,#61489,#61490,#61491,#61492,
#61493,#61494,#61495,#61496,#61497,#61498,#61499,#61500,#61501,#61502,#61503,
#61504,#61505,#61506,#61507,#61508,#61509,#61510,#61511,#61512,#61513,#61514,
#61515,#61516,#61517,#61518,#61519,#61520,#61521,#61522,#61523,#61524,#61525,
#61526,#61527,#61528,#61529,#61530,#61531,#61532,#61533,#61534,#61535,#61536,
#61537,#61538,#61539,#61540,#61541,#61542,#61543,#61544,#61545,#61546,#61547,
#61548,#61549,#61550,#61551,#61552,#61553,#61554,#61555,#61556,#61557,#61558,
#61559,#61560,#61561,#61562,#61563,#61564,#61565,#61566,#61567,#61568,#61569,
#61570,#61571,#61572,#61573,#61574,#61575,#61576,#61577,#61578,#61579,#61580,
#61581,#61582,#61583,#61584,#61585,#61586,#61587,#61588,#61589,#61590,#61591,
#61592,#61593,#61594,#61595,#61596,#61597,#61598,#61599,#61600,#61601,#61602,
#61603,#61604),.UNSPECIFIED.,.F.,.F.,(4,2,2,2,2,2,2,2,2,2,2,2,2,2,2,2,2,
2,2,2,2,2,2,2,2,2,2,2,2,2,2,2,2,2,2,2,2,2,2,2,2,2,2,2,2,2,2,2,2,2,2,2,2,
2,2,2,2,2,2,2,2,2,2,2,2,2,2,2,2,2,2,2,2,2,4),(-1.49514144568264,-1.47438857105786,
-1.46045849771916,-1.45022305357444,-1.44435288172889,-1.43889105456154,
-1.43116435290765,-1.40722401557869,-1.39283837472975,-1.38424761820676,
-1.38047920020778,-1.37736852119829,-1.37275211016375,-1.34755948942701,
-1.3332063100285,-1.32276142634397,-1.31682570935194,-1.31132487155196,
-1.30356762536673,-1.28058029495704,-1.26579136510866,-1.25706287817131,
-1.25325415294809,-1.25012853345904,-1.24548894090294,-1.22051819483855,
-1.20609396748146,-1.1956236845839,-1.18968929617281,-1.18419905470653,
-1.17647659214743,-1.15227168670788,-1.1381312685222,-1.12961958896452,
-1.1258477102684,-1.12272495591843,-1.11805801926491,-1.09336125123812,
-1.07880424687313,-1.06827635035556,-1.06233706940999,-1.05685815177955,
-1.04918041937155,-1.02437341766863,-1.01057935952288,-1.00219012882368,
-0.998438102967066,-0.995310611511707,-0.990608829365062,-0.966217676459732,
-0.951520438289615,-0.940928504456857,-0.934974506764387,-0.929492180425934,
-0.921825366122576,-0.902404848674383,-0.881301853283018,-0.874215287049936,
-0.870668989897699,-0.867504006166135,-0.862343635961059,-0.842881735424566,
-0.825765477070716,-0.814192386661388,-0.808084946221302,-0.802647876831401,
-0.795342854681945,-0.772617796786585,-0.750144313039306,-0.745236044253845,
-0.742110626730573,-0.738469454742124,-0.730808221723706,-0.718954873859401,
-0.693092190322639),.UNSPECIFIED.);
#720=B_SPLINE_CURVE_WITH_KNOTS('',3,(#61606,#61607,#61608,#61609,#61610,
#61611,#61612,#61613,#61614,#61615,#61616,#61617,#61618,#61619,#61620,#61621,
#61622,#61623,#61624,#61625,#61626,#61627,#61628,#61629,#61630,#61631),
 .UNSPECIFIED.,.F.,.F.,(4,2,2,2,2,2,2,2,2,2,2,2,4),(-0.109848755237784,
-0.0934252676034876,-0.0856589675731766,-0.0801646032460511,-0.0742495478951926,
-0.0643588753228271,-0.0439802194508923,-0.025130067662574,-0.0200474136688195,
-0.016895840425231,-0.0140198172539918,-0.0103707398875634,-0.0003752626807542),
 .UNSPECIFIED.);
#721=B_SPLINE_CURVE_WITH_KNOTS('',3,(#61632,#61633,#61634,#61635,#61636,
#61637,#61638,#61639,#61640,#61641,#61642,#61643,#61644,#61645,#61646,#61647,
#61648,#61649,#61650,#61651,#61652,#61653,#61654,#61655,#61656,#61657,#61658,
#61659,#61660,#61661,#61662,#61663,#61664,#61665,#61666,#61667,#61668,#61669,
#61670,#61671,#61672,#61673,#61674,#61675,#61676,#61677,#61678,#61679,#61680,
#61681,#61682,#61683,#61684,#61685,#61686,#61687,#61688,#61689,#61690,#61691,
#61692,#61693,#61694,#61695,#61696,#61697,#61698,#61699,#61700,#61701,#61702,
#61703,#61704,#61705,#61706,#61707,#61708,#61709,#61710,#61711,#61712,#61713,
#61714,#61715,#61716,#61717,#61718,#61719,#61720,#61721,#61722,#61723,#61724,
#61725,#61726,#61727,#61728,#61729,#61730,#61731,#61732,#61733,#61734,#61735,
#61736,#61737,#61738,#61739,#61740,#61741,#61742,#61743,#61744,#61745,#61746,
#61747,#61748,#61749,#61750,#61751,#61752,#61753,#61754,#61755,#61756,#61757,
#61758,#61759,#61760,#61761,#61762,#61763,#61764,#61765,#61766,#61767,#61768,
#61769,#61770,#61771,#61772,#61773,#61774,#61775,#61776,#61777,#61778,#61779),
 .UNSPECIFIED.,.F.,.F.,(4,3,3,3,3,3,3,3,3,3,3,3,3,3,3,3,3,3,3,3,3,3,3,3,
3,3,3,3,3,3,3,3,3,3,3,3,3,3,3,3,3,3,3,3,3,3,3,3,3,4),(59.6902604187055,
59.8059365886586,59.9214749790758,60.0369282464819,60.1523488894859,60.2678696341567,
60.3834462962811,60.4992335231002,60.5534341867985,60.6709356877518,60.7882209063099,
60.9053869875018,61.0224839148767,61.1395615592371,61.2567536125899,61.3740087054347,
61.491482903214,61.5511221063311,61.6686207302785,61.7859030669755,61.9030662657053,
62.0201603153612,62.1372350920866,62.2544243155958,62.3716765959422,62.4891480410998,
62.5488100258638,62.6663133455865,62.7836003454799,62.9007681834644,63.0178668401377,
63.1349461833192,63.2521398766191,63.3693965783365,63.4868723183997,63.5464979453964,
63.6640025093476,63.7812908428973,63.8984600685255,64.0155601635914,64.1326409927496,
64.2498362310647,64.3670945136204,64.4845718705366,64.5441858649291,64.6616585799595,
64.7789258711664,64.8960709870156,65.0131746409143,65.1150562521972),
 .UNSPECIFIED.);
#722=B_SPLINE_CURVE_WITH_KNOTS('',3,(#61783,#61784,#61785,#61786,#61787,
#61788,#61789,#61790,#61791,#61792,#61793,#61794,#61795,#61796,#61797,#61798,
#61799,#61800,#61801,#61802,#61803,#61804,#61805,#61806,#61807,#61808,#61809,
#61810,#61811,#61812,#61813,#61814,#61815,#61816,#61817,#61818,#61819,#61820,
#61821,#61822,#61823,#61824,#61825,#61826,#61827,#61828,#61829,#61830,#61831,
#61832,#61833,#61834,#61835,#61836,#61837,#61838,#61839,#61840,#61841,#61842,
#61843),.UNSPECIFIED.,.F.,.F.,(4,3,3,3,3,3,3,3,3,3,3,3,3,3,3,3,3,3,3,3,
4),(-4.04123713824999,-3.99075167813058,-3.88138448277551,-3.77034439225331,
-3.66127980526779,-3.55228313954551,-3.44331469571073,-3.33075196143253,
-3.22165200987809,-3.10735788423801,-2.99306375859793,-2.88381609209196,
-2.77276106046363,-2.66380817130367,-2.5549200056019,-2.44605671409851,
-2.33338649534021,-2.22438227090265,-2.10987905498397,-1.99537583906529,
-1.98502202421796),.UNSPECIFIED.);
#723=B_SPLINE_CURVE_WITH_KNOTS('',3,(#61847,#61848,#61849,#61850,#61851),
 .UNSPECIFIED.,.F.,.F.,(4,1,4),(0.,0.997687919532644,1.08537753955778),
 .UNSPECIFIED.);
#724=B_SPLINE_CURVE_WITH_KNOTS('',3,(#61853,#61854,#61855,#61856,#61857,
#61858,#61859,#61860,#61861,#61862,#61863,#61864,#61865,#61866,#61867,#61868,
#61869,#61870,#61871,#61872,#61873,#61874,#61875,#61876,#61877,#61878,#61879,
#61880,#61881,#61882,#61883,#61884,#61885,#61886,#61887,#61888,#61889,#61890,
#61891,#61892,#61893,#61894,#61895,#61896,#61897,#61898,#61899,#61900,#61901,
#61902,#61903,#61904,#61905,#61906,#61907,#61908,#61909,#61910,#61911,#61912,
#61913,#61914,#61915,#61916,#61917,#61918,#61919,#61920,#61921,#61922,#61923,
#61924,#61925,#61926,#61927,#61928,#61929,#61930,#61931,#61932,#61933,#61934,
#61935,#61936,#61937,#61938,#61939,#61940,#61941,#61942,#61943,#61944,#61945,
#61946,#61947,#61948,#61949,#61950,#61951,#61952,#61953,#61954,#61955,#61956,
#61957,#61958,#61959,#61960,#61961,#61962,#61963,#61964,#61965,#61966,#61967,
#61968,#61969,#61970,#61971,#61972,#61973,#61974,#61975,#61976,#61977,#61978,
#61979,#61980,#61981,#61982,#61983,#61984,#61985,#61986,#61987,#61988,#61989,
#61990,#61991,#61992,#61993,#61994,#61995,#61996,#61997,#61998,#61999,#62000,
#62001,#62002,#62003,#62004,#62005,#62006,#62007,#62008,#62009,#62010,#62011,
#62012,#62013,#62014,#62015,#62016,#62017,#62018,#62019,#62020,#62021,#62022,
#62023,#62024,#62025,#62026,#62027,#62028,#62029,#62030),.UNSPECIFIED.,
 .F.,.F.,(4,3,3,3,3,3,3,3,3,3,3,3,3,3,3,3,3,3,3,3,3,3,3,3,3,3,3,3,3,3,3,
3,3,3,3,3,3,3,3,3,3,3,3,3,3,3,3,3,3,3,3,3,3,3,3,3,3,3,3,4),(1.08537753955778,
1.19234574493029,1.29913105914354,1.40581587747835,1.51244291764453,1.61905479404571,
1.72576691819386,1.83253406091469,1.93949157832785,1.99537583906529,2.10463715419484,
2.21569047974523,2.32464897406955,2.43353974323111,2.54240264139813,2.65506792069808,
2.7640643232495,2.87856404092371,2.99306375859793,3.10241206764536,3.21345451895602,
3.32251126192849,3.43150420770341,3.54047304919539,3.65304270642919,3.76215325291235,
3.87645246552146,3.99075167813058,4.09980427302158,4.21088368860178,4.3196319345462,
4.42831248282007,4.53696553861079,4.64983405337389,4.75862402872994,4.86749101609525,
4.97653965670554,4.98843959766322,5.09762857242077,5.20869094051765,5.3175794422449,
5.42640130271024,5.5351964991536,5.64792925366416,5.75686180175626,5.87149465947606,
5.98612751719586,6.0953168100183,6.20637913835707,6.31526902205822,6.42409265844288,
6.53289002301757,6.64562137644531,6.75455705278224,6.86918624475538,6.98381543672851,
7.10632262234372,7.22836033829121,7.34964575624075,7.36856284629316),
 .UNSPECIFIED.);
#725=B_SPLINE_CURVE_WITH_KNOTS('',3,(#62032,#62033,#62034,#62035,#62036,
#62037,#62038,#62039,#62040,#62041,#62042,#62043,#62044,#62045,#62046,#62047,
#62048,#62049,#62050,#62051,#62052,#62053,#62054,#62055,#62056,#62057,#62058,
#62059,#62060,#62061,#62062,#62063,#62064,#62065,#62066,#62067,#62068,#62069,
#62070,#62071,#62072,#62073,#62074,#62075,#62076,#62077,#62078,#62079,#62080,
#62081,#62082,#62083,#62084,#62085,#62086,#62087,#62088,#62089,#62090,#62091,
#62092,#62093,#62094,#62095,#62096,#62097,#62098,#62099,#62100,#62101,#62102,
#62103,#62104,#62105,#62106,#62107,#62108,#62109,#62110,#62111,#62112,#62113,
#62114,#62115,#62116,#62117,#62118,#62119,#62120,#62121,#62122,#62123,#62124,
#62125,#62126,#62127,#62128,#62129,#62130,#62131,#62132,#62133,#62134,#62135,
#62136,#62137,#62138,#62139,#62140,#62141,#62142,#62143,#62144,#62145,#62146,
#62147,#62148,#62149,#62150,#62151,#62152,#62153,#62154,#62155,#62156,#62157,
#62158,#62159,#62160,#62161,#62162,#62163,#62164,#62165,#62166,#62167,#62168,
#62169,#62170,#62171,#62172,#62173,#62174,#62175,#62176,#62177,#62178,#62179,
#62180,#62181,#62182,#62183,#62184,#62185,#62186,#62187,#62188,#62189,#62190,
#62191,#62192,#62193,#62194,#62195,#62196,#62197,#62198,#62199,#62200,#62201,
#62202,#62203,#62204,#62205,#62206),.UNSPECIFIED.,.F.,.F.,(4,3,3,3,3,3,
3,3,3,3,3,3,3,3,3,3,3,3,3,3,3,3,3,3,3,3,3,3,3,3,3,3,3,3,3,3,3,3,3,3,3,3,
3,3,3,3,3,3,3,3,3,3,3,3,3,3,3,3,4),(7.36856284673735,7.4784069249757,7.58827792776978,
7.69829983037369,7.8084040130256,7.91873166272418,7.98150335626115,8.09067677218719,
8.20174108513802,8.31061410652896,8.41942055999989,8.5282004487066,8.64094815547839,
8.74986582499829,8.86452855039604,8.97919127579379,9.08836318751633,9.19942768849259,
9.30829928229541,9.41710434087364,9.5258828698046,9.63863195118506,9.7475483651341,
9.86221378023027,9.97687919532644,10.0860471500499,10.1971121456511,10.3059795915811,
10.4147804426623,10.523554711276,10.6363078121718,10.7452198829806,10.8598934989198,
10.9745671148591,11.0837376091672,11.1948022873202,11.3036723575658,11.4124758572139,
11.5212527943222,11.6340033543396,11.7429181124569,11.8575865734243,11.9722550343917,
12.0814251445948,12.192489870761,12.3013595589726,12.410162678443,12.5189392378677,
12.6316901668819,12.7406045580105,12.8552737559675,12.9699429539244,13.078724484454,
13.1873437619597,13.2958416021516,13.4042699324801,13.5126593842041,13.621079592138,
13.651748153917),.UNSPECIFIED.);
#726=B_SPLINE_CURVE_WITH_KNOTS('',3,(#62208,#62209,#62210,#62211,#62212,
#62213,#62214,#62215,#62216,#62217,#62218,#62219,#62220,#62221,#62222,#62223,
#62224,#62225,#62226,#62227,#62228,#62229,#62230,#62231,#62232,#62233,#62234,
#62235,#62236,#62237,#62238,#62239,#62240,#62241,#62242,#62243,#62244,#62245,
#62246,#62247,#62248,#62249,#62250,#62251,#62252,#62253,#62254,#62255,#62256,
#62257,#62258,#62259,#62260,#62261,#62262,#62263,#62264,#62265,#62266,#62267,
#62268,#62269,#62270,#62271,#62272,#62273,#62274,#62275,#62276,#62277,#62278,
#62279,#62280,#62281,#62282,#62283,#62284,#62285,#62286,#62287,#62288,#62289,
#62290,#62291,#62292,#62293,#62294,#62295,#62296,#62297,#62298,#62299,#62300,
#62301,#62302,#62303,#62304,#62305,#62306,#62307,#62308,#62309,#62310,#62311,
#62312,#62313,#62314,#62315,#62316,#62317,#62318,#62319,#62320,#62321,#62322,
#62323,#62324,#62325,#62326,#62327,#62328,#62329,#62330,#62331,#62332,#62333,
#62334,#62335,#62336,#62337,#62338,#62339,#62340,#62341,#62342,#62343,#62344,
#62345,#62346,#62347,#62348,#62349,#62350,#62351,#62352,#62353,#62354,#62355,
#62356,#62357,#62358,#62359,#62360,#62361,#62362,#62363,#62364,#62365,#62366,
#62367,#62368,#62369,#62370,#62371,#62372,#62373,#62374,#62375,#62376,#62377,
#62378,#62379),.UNSPECIFIED.,.F.,.F.,(4,3,3,3,3,3,3,3,3,3,3,3,3,3,3,3,3,
3,3,3,3,3,3,3,3,3,3,3,3,3,3,3,3,3,3,3,3,3,3,3,3,3,3,3,3,3,3,3,3,3,3,3,3,
3,3,3,3,4),(13.6517481543043,13.7804829473712,13.9108082109149,13.967630873457,
14.0768008840177,14.1878656226392,14.2967352004234,14.4055382057466,14.5143146474821,
14.627065683859,14.7359799497759,14.8506493713828,14.9653187929896,15.0744887311938,
15.1855534788599,15.2944229835671,15.4032259157507,15.5120022844056,15.6247533914348,
15.7336675852756,15.8483371488989,15.9630067125223,16.0721766057685,16.1832413590543,
16.2921108162111,16.4009137000096,16.5096900195225,16.6224411726556,16.7313553160279,
16.8460249740414,16.9606946320549,17.0698645681445,17.1809293160749,17.2897988176718,
17.3986017463818,17.5073781112041,17.6201292213,17.7290434104513,17.8437129810194,
17.9583825515876,18.0675524756807,18.1786172251106,18.2874867144961,18.3962896309488,
18.5050659834882,18.6178171053962,18.7267312823442,18.8414008767322,18.9560704711202,
19.0648897450418,19.1736452095118,19.2821672095361,19.3906233509149,19.4990541980267,
19.6080240137205,19.7165924406379,19.8257629507199,19.9349334608019),
 .UNSPECIFIED.);
#727=B_SPLINE_CURVE_WITH_KNOTS('',3,(#62381,#62382,#62383,#62384,#62385,
#62386,#62387,#62388,#62389,#62390,#62391,#62392,#62393,#62394,#62395,#62396,
#62397,#62398,#62399,#62400,#62401,#62402,#62403,#62404,#62405,#62406,#62407,
#62408,#62409,#62410,#62411,#62412,#62413,#62414,#62415,#62416,#62417,#62418,
#62419,#62420,#62421,#62422,#62423,#62424,#62425,#62426,#62427,#62428,#62429,
#62430,#62431,#62432,#62433,#62434,#62435,#62436,#62437,#62438,#62439,#62440,
#62441,#62442,#62443,#62444,#62445,#62446,#62447,#62448,#62449,#62450,#62451,
#62452,#62453,#62454,#62455,#62456,#62457,#62458,#62459,#62460,#62461,#62462,
#62463,#62464,#62465,#62466,#62467,#62468,#62469,#62470,#62471,#62472,#62473,
#62474,#62475,#62476,#62477,#62478,#62479,#62480,#62481,#62482,#62483,#62484,
#62485,#62486,#62487,#62488,#62489,#62490,#62491,#62492,#62493,#62494,#62495,
#62496,#62497,#62498,#62499,#62500,#62501,#62502,#62503,#62504,#62505,#62506,
#62507,#62508,#62509,#62510,#62511,#62512,#62513,#62514,#62515,#62516,#62517,
#62518,#62519,#62520,#62521,#62522,#62523,#62524,#62525,#62526,#62527,#62528,
#62529,#62530,#62531,#62532,#62533,#62534,#62535,#62536,#62537,#62538,#62539,
#62540,#62541,#62542,#62543,#62544,#62545,#62546,#62547,#62548,#62549,#62550,
#62551,#62552),.UNSPECIFIED.,.F.,.F.,(4,3,3,3,3,3,3,3,3,3,3,3,3,3,3,3,3,
3,3,3,3,3,3,3,3,3,3,3,3,3,3,3,3,3,3,3,3,3,3,3,3,3,3,3,3,3,3,3,3,3,3,3,3,
3,3,3,3,4),(19.9349334610966,19.9537583906529,20.0629283158291,20.1739930651237,
20.2828625555163,20.391665472945,20.5004418264274,20.6131929473669,20.722107125164,
20.8367767176748,20.9514463101855,21.0606162335135,21.1716809830391,21.280550471541,
21.3893533870683,21.4981297386421,21.6108808614111,21.7197950373033,21.8344646335107,
21.9491342297182,22.0583041526924,22.1693689022622,22.2782383903802,22.3870413055133,
22.4958176566833,22.6085687798252,22.7174829552942,22.8321525522725,22.9468221492508,
23.0559920728858,23.167056822373,23.2759263111791,23.3847292270085,23.4935055788819,
23.6062567013573,23.7151708775393,23.8298404731614,23.9445100687835,24.0536799921475,
24.1647447416686,24.2736142301963,24.3824171457456,24.4911934973373,24.603944620082,
24.7128587959821,24.8275283921491,24.9421979883161,25.0513679116608,25.1624326611843,
25.2713021496898,25.3801050652158,25.4888814167832,25.6016325395496,25.7105467154231,
25.8252163116359,25.9398859078487,26.0790023378198,26.2181187677909),
 .UNSPECIFIED.);
#728=B_SPLINE_CURVE_WITH_KNOTS('',3,(#62554,#62555,#62556,#62557,#62558,
#62559,#62560,#62561,#62562,#62563,#62564,#62565,#62566,#62567,#62568,#62569,
#62570,#62571,#62572,#62573,#62574,#62575,#62576,#62577,#62578,#62579,#62580,
#62581,#62582,#62583,#62584,#62585,#62586,#62587,#62588,#62589,#62590,#62591,
#62592,#62593,#62594,#62595,#62596,#62597,#62598,#62599,#62600,#62601,#62602,
#62603,#62604,#62605,#62606,#62607,#62608,#62609,#62610,#62611,#62612,#62613,
#62614,#62615,#62616,#62617,#62618,#62619,#62620,#62621,#62622,#62623,#62624,
#62625,#62626,#62627,#62628,#62629,#62630,#62631,#62632,#62633,#62634,#62635,
#62636,#62637,#62638,#62639,#62640,#62641,#62642,#62643,#62644,#62645,#62646,
#62647,#62648,#62649,#62650,#62651,#62652,#62653,#62654,#62655,#62656,#62657,
#62658,#62659,#62660,#62661,#62662,#62663,#62664,#62665,#62666,#62667,#62668,
#62669,#62670,#62671,#62672,#62673,#62674,#62675,#62676,#62677,#62678,#62679,
#62680,#62681,#62682,#62683,#62684,#62685,#62686,#62687,#62688,#62689,#62690,
#62691,#62692,#62693,#62694,#62695,#62696,#62697,#62698,#62699,#62700,#62701,
#62702,#62703,#62704,#62705,#62706,#62707,#62708,#62709,#62710,#62711,#62712,
#62713,#62714,#62715,#62716,#62717,#62718,#62719,#62720,#62721,#62722,#62723,
#62724,#62725,#62726,#62727,#62728),.UNSPECIFIED.,.F.,.F.,(4,3,3,3,3,3,
3,3,3,3,3,3,3,3,3,3,3,3,3,3,3,3,3,3,3,3,3,3,3,3,3,3,3,3,3,3,3,3,3,3,3,3,
3,3,3,3,3,3,3,3,3,3,3,3,3,3,3,3,4),(26.2181187682761,26.3260314065148,26.4338895648003,
26.5417345758493,26.6496837906648,26.7576875372505,26.8658900149683,26.9375738273814,
27.0467437507667,27.1578085002851,27.2666779888336,27.3754809044032,27.484257256015,
27.5970083787398,27.7059225546589,27.8205921507864,27.935261746914,28.0444316703009,
28.1554964198191,28.264365908369,28.3731688239399,28.4819451755529,28.5946962982764,
28.7036104741963,28.8182800703215,28.9329496664467,29.0421195898417,29.1531843393589,
29.2620538279173,29.3708567434968,29.4796330951187,29.5923842178338,29.7012983937628,
29.8159679898711,29.9306375859793,30.0398075093685,30.1508722588864,30.2597417474389,
30.3685446630125,30.4773210146281,30.5900721373491,30.6989863132719,30.8136559093919,
30.928325505512,31.0374954289073,31.1485601784245,31.2574296669829,31.3662325825624,
31.4750089341842,31.5877600568993,31.6966742328281,31.8113438289363,31.9260134250446,
32.037541760806,32.1534823394684,32.2646132694227,32.3756310959963,32.4865598326513,
32.5013040754557),.UNSPECIFIED.);
#729=B_SPLINE_CURVE_WITH_KNOTS('',3,(#62730,#62731,#62732,#62733,#62734,
#62735,#62736,#62737,#62738,#62739,#62740,#62741,#62742,#62743,#62744,#62745,
#62746,#62747,#62748,#62749,#62750,#62751,#62752,#62753,#62754,#62755,#62756,
#62757,#62758,#62759,#62760,#62761,#62762,#62763,#62764,#62765,#62766,#62767,
#62768,#62769,#62770,#62771,#62772,#62773,#62774,#62775,#62776,#62777,#62778,
#62779,#62780,#62781,#62782,#62783,#62784,#62785,#62786,#62787,#62788,#62789,
#62790,#62791,#62792,#62793,#62794,#62795,#62796,#62797,#62798,#62799,#62800,
#62801,#62802,#62803,#62804,#62805,#62806,#62807,#62808,#62809,#62810,#62811,
#62812,#62813,#62814,#62815,#62816,#62817,#62818,#62819,#62820,#62821,#62822,
#62823,#62824,#62825,#62826,#62827,#62828,#62829,#62830,#62831,#62832,#62833,
#62834,#62835,#62836,#62837,#62838,#62839,#62840,#62841,#62842,#62843,#62844,
#62845,#62846,#62847,#62848,#62849,#62850,#62851,#62852,#62853,#62854,#62855,
#62856,#62857,#62858,#62859,#62860,#62861,#62862,#62863,#62864,#62865,#62866,
#62867,#62868,#62869,#62870,#62871,#62872,#62873,#62874,#62875,#62876,#62877,
#62878,#62879,#62880,#62881,#62882,#62883,#62884,#62885,#62886,#62887,#62888,
#62889,#62890,#62891,#62892,#62893,#62894,#62895,#62896,#62897,#62898,#62899,
#62900,#62901),.UNSPECIFIED.,.F.,.F.,(4,3,3,3,3,3,3,3,3,3,3,3,3,3,3,3,3,
3,3,3,3,3,3,3,3,3,3,3,3,3,3,3,3,3,3,3,3,3,3,3,3,3,3,3,3,3,3,3,3,3,3,3,3,
3,3,3,3,4),(32.5013040758074,32.6198608438911,32.7387777837186,32.858217674201,
32.9237013445772,33.0328712679628,33.1439360174812,33.2528055060299,33.3616084215996,
33.4703847732114,33.583135895936,33.692050071855,33.8067196679824,33.9213892641099,
34.0305591875354,34.1416239370488,34.2504934256376,34.3592963412474,34.4680726928993,
34.5808238155851,34.6897379915434,34.804407587593,34.9190771836425,35.0282471069821,
35.1393118565063,35.2481813450097,35.3569842605347,35.4657606121023,35.5785117348705,
35.6874259107468,35.802095506961,35.9167651031752,36.025935026543,36.1369997760636,
36.2458692645929,36.3546721801429,36.4634485317346,36.5761996544779,36.6851138303758,
36.7997834265418,36.9144530227078,37.0236229463545,37.1346876958402,37.2435571846511,
37.3523601004828,37.461136452356,37.5738875748271,37.6828017510026,37.7974713466216,
37.9121409422405,38.021184497235,38.1286405836999,38.2359927120742,38.343283022873,
38.4535846127039,38.5609344442578,38.6727119132271,38.7844893821964),
 .UNSPECIFIED.);
#730=B_SPLINE_CURVE_WITH_KNOTS('',3,(#62903,#62904,#62905,#62906,#62907,
#62908,#62909,#62910,#62911,#62912,#62913,#62914,#62915,#62916,#62917,#62918,
#62919,#62920,#62921,#62922,#62923,#62924,#62925,#62926,#62927,#62928,#62929,
#62930,#62931,#62932,#62933,#62934,#62935,#62936,#62937,#62938,#62939,#62940,
#62941,#62942,#62943,#62944,#62945,#62946,#62947,#62948,#62949,#62950,#62951,
#62952,#62953,#62954,#62955,#62956,#62957,#62958,#62959,#62960,#62961,#62962,
#62963,#62964,#62965,#62966,#62967,#62968,#62969,#62970,#62971,#62972,#62973,
#62974,#62975,#62976,#62977,#62978,#62979,#62980,#62981,#62982,#62983,#62984,
#62985,#62986,#62987,#62988,#62989,#62990,#62991,#62992,#62993,#62994,#62995,
#62996,#62997,#62998,#62999,#63000,#63001,#63002,#63003,#63004,#63005,#63006,
#63007,#63008,#63009,#63010,#63011,#63012,#63013,#63014,#63015,#63016,#63017,
#63018,#63019,#63020,#63021,#63022,#63023,#63024,#63025,#63026,#63027,#63028,
#63029,#63030,#63031,#63032,#63033,#63034,#63035,#63036,#63037,#63038,#63039,
#63040,#63041,#63042,#63043,#63044,#63045,#63046,#63047,#63048,#63049,#63050,
#63051,#63052,#63053,#63054,#63055,#63056,#63057,#63058,#63059,#63060,#63061,
#63062,#63063,#63064,#63065,#63066,#63067,#63068,#63069,#63070,#63071),
 .UNSPECIFIED.,.F.,.F.,(4,3,3,3,3,3,3,3,3,3,3,3,3,3,3,3,3,3,3,3,3,3,3,3,
3,3,3,3,3,3,3,3,3,3,3,3,3,3,3,3,3,3,3,3,3,3,3,3,3,3,3,3,3,3,3,3,4),(38.7844893826353,
38.9098288617731,39.0189987851414,39.130063534662,39.2389330231807,39.3477359387159,
39.4565122902888,39.569263413043,39.6781775889125,39.7928471851092,39.9075167813058,
40.0166867065533,40.1277514558389,40.2366209462611,40.3454238637035,40.4542002171843,
40.5669513380978,40.6758655158546,40.7905351083465,40.9052047008384,41.0143746203194,
41.1254393703258,41.2343088549957,41.3431117667068,41.4518881144863,41.5646392409575,
41.6735534131527,41.7882230167618,41.902892620371,42.0120625448578,42.1231272942385,
42.2319967837874,42.3407997003176,42.4495760528488,42.5623271746126,42.6712413513396,
42.7859109456216,42.9005805399037,43.0097504763836,43.1208152242651,43.2296847260242,
43.338487654811,43.4472640196252,43.560015129578,43.6689293185101,43.7835988889732,
43.8982684594363,44.007438350286,44.1185031038713,44.2273725600332,44.3361754433597,
44.4449517629223,44.557702916934,44.6666170616515,44.7812867203103,44.895956378969,
45.0676746898149),.UNSPECIFIED.);
#731=B_SPLINE_CURVE_WITH_KNOTS('',3,(#63073,#63074,#63075,#63076,#63077,
#63078,#63079,#63080,#63081,#63082,#63083,#63084,#63085,#63086,#63087,#63088,
#63089,#63090,#63091,#63092,#63093,#63094,#63095,#63096,#63097,#63098,#63099,
#63100,#63101,#63102,#63103,#63104,#63105,#63106,#63107,#63108,#63109,#63110,
#63111,#63112,#63113,#63114,#63115,#63116,#63117,#63118,#63119,#63120,#63121,
#63122,#63123,#63124,#63125,#63126,#63127,#63128,#63129,#63130,#63131,#63132,
#63133,#63134,#63135,#63136,#63137,#63138,#63139,#63140,#63141,#63142,#63143,
#63144,#63145,#63146,#63147,#63148,#63149,#63150,#63151,#63152,#63153,#63154,
#63155,#63156,#63157,#63158,#63159,#63160,#63161,#63162,#63163,#63164,#63165,
#63166,#63167,#63168,#63169,#63170,#63171,#63172,#63173,#63174,#63175,#63176,
#63177,#63178,#63179,#63180,#63181,#63182,#63183,#63184,#63185,#63186,#63187,
#63188,#63189,#63190,#63191,#63192,#63193,#63194,#63195,#63196,#63197,#63198,
#63199,#63200,#63201,#63202,#63203,#63204,#63205,#63206,#63207,#63208,#63209,
#63210,#63211,#63212,#63213,#63214,#63215,#63216,#63217,#63218,#63219,#63220,
#63221,#63222,#63223,#63224,#63225,#63226,#63227,#63228,#63229,#63230,#63231,
#63232,#63233,#63234,#63235,#63236,#63237,#63238,#63239,#63240,#63241,#63242,
#63243,#63244),.UNSPECIFIED.,.F.,.F.,(4,3,3,3,3,3,3,3,3,3,3,3,3,3,3,3,3,
3,3,3,3,3,3,3,3,3,3,3,3,3,3,3,3,3,3,3,3,3,3,3,3,3,3,3,3,3,3,3,3,3,3,3,3,
3,3,3,3,4),(45.0676746901124,45.1750417725799,45.282302053759,45.3894977918574,
45.4966711412374,45.6039382377035,45.7112531460519,45.8187617443077,45.8936442985016,
46.002814310719,46.1138790491335,46.2227486276055,46.331551633255,46.4403280749561,
46.5530791107256,46.6619933757127,46.7766627968735,46.8913322180343,47.000501877111,
47.111566659668,47.2204358846347,47.3292385376104,47.4380146280312,47.5507660054152,
47.6596799266104,47.7743500320886,47.8890201375669,47.9981902797867,48.1092550019508,
48.2181247034541,48.3269278292316,48.4357043879899,48.5484553052673,48.6573696784251,
48.7720388677623,48.8867080570995,48.995878553069,49.1069432310144,49.2158133019497,
49.3246168019251,49.4333937389989,49.5461442984073,49.6550590555919,49.7697275161121,
49.8843959766322,49.9935638013074,50.1046288131645,50.2134962051043,50.322297030565,
50.4310713018833,50.5438244504537,50.6527365942569,50.7674102452109,50.8820838961648,
50.999277921294,51.1153231035882,51.2330915501348,51.3508599966814),
 .UNSPECIFIED.);
#732=B_SPLINE_CURVE_WITH_KNOTS('',3,(#63246,#63247,#63248,#63249,#63250,
#63251,#63252,#63253,#63254,#63255,#63256,#63257,#63258,#63259,#63260,#63261,
#63262,#63263,#63264,#63265,#63266,#63267,#63268,#63269,#63270,#63271,#63272,
#63273,#63274,#63275,#63276,#63277,#63278,#63279,#63280,#63281,#63282,#63283,
#63284,#63285,#63286,#63287,#63288,#63289,#63290,#63291,#63292,#63293,#63294,
#63295,#63296,#63297,#63298,#63299,#63300,#63301,#63302,#63303,#63304,#63305,
#63306,#63307,#63308,#63309,#63310,#63311,#63312,#63313,#63314,#63315,#63316,
#63317,#63318,#63319,#63320,#63321,#63322,#63323,#63324,#63325,#63326,#63327,
#63328,#63329,#63330,#63331,#63332,#63333,#63334,#63335,#63336,#63337,#63338,
#63339,#63340,#63341,#63342,#63343,#63344,#63345,#63346,#63347,#63348,#63349,
#63350,#63351,#63352,#63353,#63354,#63355,#63356,#63357,#63358,#63359,#63360,
#63361,#63362,#63363,#63364,#63365,#63366,#63367,#63368,#63369,#63370,#63371,
#63372,#63373,#63374,#63375,#63376,#63377,#63378,#63379,#63380,#63381,#63382,
#63383,#63384,#63385,#63386,#63387,#63388,#63389,#63390,#63391,#63392,#63393,
#63394,#63395,#63396,#63397,#63398,#63399,#63400,#63401,#63402,#63403,#63404,
#63405,#63406,#63407,#63408,#63409,#63410,#63411,#63412,#63413,#63414,#63415,
#63416,#63417,#63418,#63419,#63420),.UNSPECIFIED.,.F.,.F.,(4,3,3,3,3,3,
3,3,3,3,3,3,3,3,3,3,3,3,3,3,3,3,3,3,3,3,3,3,3,3,3,3,3,3,3,3,3,3,3,3,3,3,
3,3,3,3,3,3,3,3,3,3,3,3,3,3,3,3,4),(51.3508599969945,51.4634741467203,51.5763443922042,
51.6893483676939,51.8026435838821,51.8797718156975,51.988945155237,52.1000094777362,
52.2088824674154,52.3176889058393,52.4264687961371,52.5392165309103,52.6481342433072,
52.7627969892686,52.8774597352301,52.9866133635763,53.0976801499746,53.2065333314141,
53.3153199798818,53.4240801302457,53.536847011375,53.6457453351107,53.7604464949367,
53.8751476547628,53.9843392307382,54.0954012736828,54.2042921051629,54.3131161911514,
54.421913507944,54.5346440245319,54.6435784190957,54.7582069966955,54.8728355742954,
54.9820232591834,55.093085788514,55.2019737547881,55.3107953612392,55.4195905846614,
55.5323238119531,55.6412570841702,55.7558902889992,55.8705234938281,55.9795699161335,
56.0906501032869,56.199395785453,56.3080751149658,56.4167282948664,56.52959907449,
56.638392510654,56.747264113805,56.8563189544076,56.8682114133607,56.9761882052863,
57.0840128847663,57.1917273855887,57.3023068652351,57.4099598206258,57.5220025623999,
57.6340453041741),.UNSPECIFIED.);
#733=B_SPLINE_CURVE_WITH_KNOTS('',3,(#63422,#63423,#63424,#63425,#63426,
#63427,#63428,#63429,#63430,#63431,#63432,#63433,#63434,#63435,#63436,#63437,
#63438,#63439,#63440,#63441,#63442,#63443,#63444,#63445,#63446,#63447,#63448,
#63449,#63450,#63451,#63452,#63453,#63454,#63455,#63456,#63457,#63458),
 .UNSPECIFIED.,.F.,.F.,(4,3,3,3,3,3,3,3,3,3,3,3,4),(57.6340453045496,57.779619983922,
57.8658993328933,57.9751468990343,58.0862019432083,58.1951547315241,58.3040427964902,
58.4129059875357,58.5255763037583,58.6345804296199,58.7490838410229,58.863587252426,
58.8739410672733),.UNSPECIFIED.);
#734=B_SPLINE_CURVE_WITH_KNOTS('',3,(#63462,#63463,#63464,#63465,#63466,
#63467,#63468),.UNSPECIFIED.,.F.,.F.,(4,3,4),(-60.8589630914912,-60.7203125906016,
-60.5899052282396),.UNSPECIFIED.);
#735=B_SPLINE_CURVE_WITH_KNOTS('',3,(#63470,#63471,#63472,#63473,#63474,
#63475,#63476,#63477,#63478,#63479),.UNSPECIFIED.,.F.,.F.,(4,1,1,1,1,1,
1,4),(-60.5899049028663,-59.8612751719586,-58.863587252426,-57.8658993328933,
-56.8682114133607,-55.8705234938281,-54.8728355742954,-54.3067195956867),
 .UNSPECIFIED.);
#736=B_SPLINE_CURVE_WITH_KNOTS('',3,(#63481,#63482,#63483,#63484,#63485,
#63486,#63487,#63488,#63489,#63490,#63491,#63492,#63493,#63494,#63495,#63496,
#63497,#63498,#63499,#63500,#63501,#63502,#63503,#63504,#63505,#63506,#63507,
#63508,#63509,#63510,#63511,#63512,#63513,#63514,#63515,#63516,#63517,#63518,
#63519,#63520,#63521,#63522,#63523,#63524,#63525,#63526,#63527,#63528,#63529,
#63530,#63531,#63532,#63533,#63534,#63535,#63536,#63537,#63538,#63539,#63540,
#63541,#63542,#63543,#63544,#63545,#63546,#63547,#63548,#63549,#63550,#63551,
#63552,#63553,#63554,#63555,#63556,#63557,#63558,#63559,#63560,#63561,#63562,
#63563,#63564,#63565,#63566,#63567,#63568,#63569,#63570,#63571,#63572,#63573,
#63574,#63575,#63576,#63577,#63578,#63579,#63580,#63581,#63582,#63583,#63584,
#63585,#63586,#63587,#63588,#63589,#63590,#63591,#63592,#63593,#63594,#63595,
#63596,#63597,#63598,#63599,#63600,#63601,#63602,#63603,#63604,#63605,#63606,
#63607,#63608,#63609,#63610,#63611,#63612,#63613,#63614,#63615,#63616,#63617,
#63618,#63619,#63620,#63621,#63622,#63623,#63624,#63625,#63626,#63627,#63628,
#63629,#63630,#63631,#63632,#63633,#63634,#63635,#63636,#63637,#63638,#63639,
#63640,#63641,#63642,#63643,#63644,#63645,#63646,#63647,#63648,#63649,#63650,
#63651,#63652),.UNSPECIFIED.,.F.,.F.,(4,3,3,3,3,3,3,3,3,3,3,3,3,3,3,3,3,
3,3,3,3,3,3,3,3,3,3,3,3,3,3,3,3,3,3,3,3,3,3,3,3,3,3,3,3,3,3,3,3,3,3,3,3,
3,3,3,3,4),(-54.3067192612381,-54.1887395011815,-54.0704302450224,-53.9516185764346,
-53.8751476547628,-53.7659931173469,-53.6549264445823,-53.5460728899735,
-53.437286068191,-53.3285259440385,-53.2157593918364,-53.1068615894403,
-52.9921606623352,-52.8774597352301,-52.7682863165904,-52.6572220039788,
-52.5483489798132,-52.4395425235527,-52.3307626320459,-52.2180149279588,
-52.1090972556454,-51.9944345356715,-51.8797718156975,-51.7705999034038,
-51.6595354024989,-51.5506638080811,-51.4418587488731,-51.3330802192985,
-51.2203311385151,-51.1114147238957,-50.9967493100302,-50.8820838961648,
-50.772915942593,-50.6618509468479,-50.5529835021134,-50.4441826522408,
-50.3354083848465,-50.222655282793,-50.1137432132176,-49.9990695949249,
-49.8843959766322,-49.7752254818367,-49.6641608037445,-49.5552907329995,
-49.4464872328491,-49.3377102952362,-49.224959735702,-49.1160449770806,
-49.0013765170901,-48.8867080570995,-48.7788113360781,-48.6713935084339,
-48.5640801570707,-48.4568290977937,-48.3485053955774,-48.2411984952054,
-48.1323663920669,-48.0235342889285),.UNSPECIFIED.);
#737=B_SPLINE_CURVE_WITH_KNOTS('',3,(#63654,#63655,#63656,#63657,#63658,
#63659,#63660,#63661,#63662,#63663,#63664,#63665,#63666,#63667,#63668,#63669,
#63670,#63671,#63672,#63673,#63674,#63675,#63676,#63677,#63678,#63679,#63680,
#63681,#63682,#63683,#63684,#63685,#63686,#63687,#63688,#63689,#63690,#63691,
#63692,#63693,#63694,#63695,#63696,#63697,#63698,#63699,#63700,#63701,#63702,
#63703,#63704,#63705,#63706,#63707,#63708,#63709,#63710,#63711,#63712,#63713,
#63714,#63715,#63716,#63717,#63718,#63719,#63720,#63721,#63722,#63723,#63724,
#63725,#63726,#63727,#63728,#63729,#63730,#63731,#63732,#63733,#63734,#63735,
#63736,#63737,#63738,#63739,#63740,#63741,#63742,#63743,#63744,#63745,#63746,
#63747,#63748,#63749,#63750,#63751,#63752,#63753,#63754,#63755,#63756,#63757,
#63758,#63759,#63760,#63761,#63762,#63763,#63764,#63765,#63766,#63767,#63768,
#63769,#63770,#63771,#63772,#63773,#63774,#63775,#63776,#63777,#63778,#63779,
#63780,#63781,#63782,#63783,#63784,#63785,#63786,#63787,#63788,#63789,#63790,
#63791,#63792,#63793,#63794,#63795,#63796,#63797,#63798,#63799,#63800,#63801,
#63802,#63803,#63804,#63805,#63806,#63807,#63808,#63809,#63810,#63811,#63812,
#63813,#63814,#63815,#63816,#63817,#63818,#63819,#63820,#63821,#63822),
 .UNSPECIFIED.,.F.,.F.,(4,3,3,3,3,3,3,3,3,3,3,3,3,3,3,3,3,3,3,3,3,3,3,3,
3,3,3,3,3,3,3,3,3,3,3,3,3,3,3,3,3,3,3,3,3,3,3,3,3,3,3,3,3,3,3,3,4),(-48.0235342885071,
-47.8890201375669,-47.7798504607805,-47.6687856804372,-47.5599164482297,
-47.4511137919178,-47.3423377020588,-47.2295863310527,-47.12067242009,-47.0060023190621,
-46.8913322180343,-46.7821622073899,-46.6710974687789,-46.5622278909087,
-46.453424885499,-46.3446484436765,-46.2318974073827,-46.1229831413787,
-46.0083137199401,-45.8936442985016,-45.7844743602938,-45.6734096126282,
-45.5645401079166,-45.4557371757283,-45.3469608070684,-45.2342097000436,
-45.1252955061971,-45.0106259425831,-44.895956378969,-44.7867864857488,
-44.6757217324597,-44.56685227533,-44.4580493915589,-44.3492730720737,-44.2365219189143,
-44.1276077755701,-44.0129381175032,-43.8982684594363,-43.789098523333,
-43.6780337754043,-43.5691642737932,-43.460361345069,-43.3515849802323,
-43.2388338701502,-43.1299196809845,-43.0152501104441,-42.9005805399037,
-42.7914106158111,-42.6803458663811,-42.571476376996,-42.4626734605437,
-42.3538971080047,-42.2411459860962,-42.1322318091485,-42.0175622147598,
-41.902892620371,-41.7403489813275),.UNSPECIFIED.);
#738=B_SPLINE_CURVE_WITH_KNOTS('',3,(#63824,#63825,#63826,#63827,#63828,
#63829,#63830,#63831,#63832,#63833,#63834,#63835,#63836,#63837,#63838,#63839,
#63840,#63841,#63842,#63843,#63844,#63845,#63846,#63847,#63848,#63849,#63850,
#63851,#63852,#63853,#63854,#63855,#63856,#63857,#63858,#63859,#63860,#63861,
#63862,#63863,#63864,#63865,#63866,#63867,#63868,#63869,#63870,#63871,#63872,
#63873,#63874,#63875,#63876,#63877,#63878,#63879,#63880,#63881,#63882,#63883,
#63884,#63885,#63886,#63887,#63888,#63889,#63890,#63891,#63892,#63893,#63894,
#63895,#63896,#63897,#63898,#63899,#63900,#63901,#63902,#63903,#63904,#63905,
#63906,#63907,#63908,#63909,#63910,#63911,#63912,#63913,#63914,#63915,#63916,
#63917,#63918,#63919,#63920,#63921,#63922,#63923,#63924,#63925,#63926,#63927,
#63928,#63929,#63930,#63931,#63932,#63933,#63934,#63935,#63936,#63937,#63938,
#63939,#63940,#63941,#63942,#63943,#63944,#63945,#63946,#63947,#63948,#63949,
#63950,#63951,#63952,#63953,#63954,#63955,#63956,#63957,#63958,#63959,#63960,
#63961,#63962,#63963,#63964,#63965,#63966,#63967,#63968,#63969,#63970,#63971,
#63972,#63973,#63974,#63975,#63976,#63977,#63978,#63979,#63980,#63981,#63982,
#63983,#63984,#63985,#63986,#63987,#63988,#63989,#63990,#63991,#63992,#63993,
#63994,#63995),.UNSPECIFIED.,.F.,.F.,(4,3,3,3,3,3,3,3,3,3,3,3,3,3,3,3,3,
3,3,3,3,3,3,3,3,3,3,3,3,3,3,3,3,3,3,3,3,3,3,3,3,3,3,3,3,3,3,3,3,3,3,3,3,
3,3,3,3,4),(-41.7403489809942,-41.6329694234406,-41.5257002609243,-41.4184992250767,
-41.3113241566121,-41.204057916278,-41.0967470791135,-40.9892397008504,
-40.9052047008384,-40.7960347756599,-40.6849700263657,-40.5761005359707,
-40.4672976185397,-40.3585212650549,-40.2457701441176,-40.1368559663182,
-40.0221863738119,-39.9075167813057,-39.798346857978,-39.6872821084524,
-39.5784126199507,-39.4696097044238,-39.3608333528504,-39.2480822300811,
-39.1391680541892,-39.0244984579812,-38.9098288617731,-38.8006589387994,
-38.6895941892295,-38.580724701112,-38.4719217859793,-38.3631454348099,
-38.2503943116676,-38.1414801361991,-38.0268105392198,-37.9121409422405,
-37.8029710186051,-37.691906269118,-37.5830367803116,-37.4742338644818,
-37.3654575126082,-37.2527063901331,-37.1437922139506,-37.0291226183292,
-36.9144530227078,-36.8052830993439,-36.6942183498228,-36.5853488612952,
-36.4765459457459,-36.3677695941543,-36.2550184714095,-36.1461042955095,
-36.0314346993424,-35.9167651031752,-35.7999067404385,-35.6833251833026,
-35.5671586433901,-35.4571636745501),.UNSPECIFIED.);
#739=B_SPLINE_CURVE_WITH_KNOTS('',3,(#63997,#63998,#63999,#64000,#64001,
#64002,#64003,#64004,#64005,#64006,#64007,#64008,#64009,#64010,#64011,#64012,
#64013,#64014,#64015,#64016,#64017,#64018,#64019,#64020,#64021,#64022,#64023,
#64024,#64025,#64026,#64027,#64028,#64029,#64030,#64031,#64032,#64033,#64034,
#64035,#64036,#64037,#64038,#64039,#64040,#64041,#64042,#64043,#64044,#64045,
#64046,#64047,#64048,#64049,#64050,#64051,#64052,#64053,#64054,#64055,#64056,
#64057,#64058,#64059,#64060,#64061,#64062,#64063,#64064,#64065,#64066,#64067,
#64068,#64069,#64070,#64071,#64072,#64073,#64074,#64075,#64076,#64077,#64078,
#64079,#64080,#64081,#64082,#64083,#64084,#64085,#64086,#64087,#64088,#64089,
#64090,#64091,#64092,#64093,#64094,#64095,#64096,#64097,#64098,#64099,#64100,
#64101,#64102,#64103,#64104,#64105,#64106,#64107,#64108,#64109,#64110,#64111,
#64112,#64113,#64114,#64115,#64116,#64117,#64118,#64119,#64120,#64121,#64122,
#64123,#64124,#64125,#64126,#64127,#64128,#64129,#64130,#64131,#64132,#64133,
#64134,#64135,#64136,#64137,#64138,#64139,#64140,#64141,#64142,#64143,#64144,
#64145,#64146,#64147,#64148,#64149,#64150,#64151,#64152,#64153,#64154,#64155,
#64156,#64157,#64158,#64159,#64160,#64161,#64162,#64163,#64164,#64165,#64166,
#64167,#64168),.UNSPECIFIED.,.F.,.F.,(4,3,3,3,3,3,3,3,3,3,3,3,3,3,3,3,3,
3,3,3,3,3,3,3,3,3,3,3,3,3,3,3,3,3,3,3,3,3,3,3,3,3,3,3,3,3,3,3,3,3,3,3,3,
3,3,3,3,4),(-35.4571636741479,-35.344912853165,-35.2324236048642,-35.1198119929548,
-35.0069133599008,-34.9190771836425,-34.8099072602187,-34.6988425107051,
-34.5899730221171,-34.4811701065077,-34.3723937548559,-34.2596426321694,
-34.1507284562101,-34.03605886016,-33.9213892641099,-33.8122193407245,-33.7011545912061,
-33.5922851026576,-33.4834821870879,-33.374705835476,-33.2619547127513,
-33.1530405368323,-33.0383709407047,-32.9237013445772,-32.8145314211901,
-32.7034666716719,-32.5945971831221,-32.4857942675512,-32.3770179159381,
-32.2642667932148,-32.1553526172948,-32.0406830211697,-31.9260134250446,
-31.8168435016496,-31.7057787521324,-31.5969092635741,-31.4881063479944,
-31.3793299963728,-31.2665788736576,-31.1576646977287,-31.0429951016203,
-30.9283255055119,-30.8191555821226,-30.7080908326047,-30.5992213440521,
-30.4904184284786,-30.3816420768629,-30.268890954142,-30.1599767782191,
-30.0453071820992,-29.9306375859793,-29.8228320190155,-29.7151785918317,
-29.6076351924948,-29.4992209861132,-29.3917393866121,-29.2828588767902,
-29.1739783669683),.UNSPECIFIED.);
#740=B_SPLINE_CURVE_WITH_KNOTS('',3,(#64170,#64171,#64172,#64173,#64174,
#64175,#64176,#64177,#64178,#64179,#64180,#64181,#64182,#64183,#64184,#64185,
#64186,#64187,#64188,#64189,#64190,#64191,#64192,#64193,#64194,#64195,#64196,
#64197,#64198,#64199,#64200,#64201,#64202,#64203,#64204,#64205,#64206,#64207,
#64208,#64209,#64210,#64211,#64212,#64213,#64214,#64215,#64216,#64217,#64218,
#64219,#64220,#64221,#64222,#64223,#64224,#64225,#64226,#64227,#64228,#64229,
#64230,#64231,#64232,#64233,#64234,#64235,#64236,#64237,#64238,#64239,#64240,
#64241,#64242,#64243,#64244,#64245,#64246,#64247,#64248,#64249,#64250,#64251,
#64252,#64253,#64254,#64255,#64256,#64257,#64258,#64259,#64260,#64261,#64262,
#64263,#64264,#64265,#64266,#64267,#64268,#64269,#64270,#64271,#64272,#64273,
#64274,#64275,#64276,#64277,#64278,#64279,#64280,#64281,#64282,#64283,#64284,
#64285,#64286,#64287,#64288,#64289,#64290,#64291,#64292,#64293,#64294,#64295,
#64296,#64297,#64298,#64299,#64300,#64301,#64302,#64303,#64304,#64305,#64306,
#64307,#64308,#64309,#64310,#64311,#64312,#64313,#64314,#64315,#64316,#64317,
#64318,#64319,#64320,#64321,#64322,#64323,#64324,#64325,#64326,#64327,#64328,
#64329,#64330,#64331,#64332,#64333,#64334,#64335,#64336,#64337,#64338,#64339,
#64340,#64341),.UNSPECIFIED.,.F.,.F.,(4,3,3,3,3,3,3,3,3,3,3,3,3,3,3,3,3,
3,3,3,3,3,3,3,3,3,3,3,3,3,3,3,3,3,3,3,3,3,3,3,3,3,3,3,3,3,3,3,3,3,3,3,3,
3,3,3,3,4),(-29.1739783666309,-29.0306086412345,-28.9329496664467,-28.8237797430603,
-28.712714993542,-28.6038455049923,-28.4950425894213,-28.3862662378082,
-28.2735151150846,-28.1646009391642,-28.0499313430391,-27.935261746914,
-27.8260918235285,-27.7150270740101,-27.6061575854616,-27.497354669892,
-27.3885783182803,-27.2758271955556,-27.1669130196368,-27.0522434235091,
-26.9375738273814,-26.8284039039558,-26.7173391544424,-26.6084696658535,
-26.4996667502436,-26.3908903985916,-26.2781392759059,-26.1692250999475,
-26.0545555038981,-25.9398859078487,-25.8307159845091,-25.719651234985,
-25.6107817464816,-25.5019788309567,-25.3932024793892,-25.2804513566209,
-25.1715371807446,-25.0568675845304,-24.9421979883161,-24.8330280649484,
-24.7219633154277,-24.6130938268984,-24.5042909113485,-24.3955145597569,
-24.2827634370135,-24.1738492611156,-24.0591796649495,-23.9445100687834,
-23.8353401451363,-23.7242753956507,-23.6154059068394,-23.5066029910073,
-23.3978266391338,-23.2850755166631,-23.1761613404872,-23.061491744869,
-22.9468221492508,-22.8907930597887),.UNSPECIFIED.);
#741=B_SPLINE_CURVE_WITH_KNOTS('',3,(#64343,#64344,#64345,#64346,#64347,
#64348,#64349,#64350,#64351,#64352,#64353,#64354,#64355,#64356,#64357,#64358,
#64359,#64360,#64361,#64362,#64363,#64364,#64365,#64366,#64367,#64368,#64369,
#64370,#64371,#64372,#64373,#64374,#64375,#64376,#64377,#64378,#64379,#64380,
#64381,#64382,#64383,#64384,#64385,#64386,#64387,#64388,#64389,#64390,#64391,
#64392,#64393,#64394,#64395,#64396,#64397,#64398,#64399,#64400,#64401,#64402,
#64403,#64404,#64405,#64406,#64407,#64408,#64409,#64410,#64411,#64412,#64413,
#64414,#64415,#64416,#64417,#64418,#64419,#64420,#64421,#64422,#64423,#64424,
#64425,#64426,#64427,#64428,#64429,#64430,#64431,#64432,#64433,#64434,#64435,
#64436,#64437,#64438,#64439,#64440,#64441,#64442,#64443,#64444,#64445,#64446,
#64447,#64448,#64449,#64450,#64451,#64452,#64453,#64454,#64455,#64456,#64457,
#64458,#64459,#64460,#64461,#64462,#64463,#64464,#64465,#64466,#64467,#64468,
#64469,#64470,#64471,#64472,#64473,#64474,#64475,#64476,#64477,#64478,#64479,
#64480,#64481,#64482,#64483,#64484,#64485,#64486,#64487,#64488,#64489,#64490,
#64491,#64492,#64493,#64494,#64495,#64496,#64497,#64498,#64499,#64500,#64501,
#64502,#64503,#64504,#64505,#64506,#64507,#64508,#64509,#64510,#64511,#64512,
#64513,#64514),.UNSPECIFIED.,.F.,.F.,(4,3,3,3,3,3,3,3,3,3,3,3,3,3,3,3,3,
3,3,3,3,3,3,3,3,3,3,3,3,3,3,3,3,3,3,3,3,3,3,3,3,3,3,3,3,3,3,3,3,3,3,3,3,
3,3,3,3,4),(-22.8907930594412,-22.7825589193295,-22.6745058528515,-22.5665527900898,
-22.4586583131073,-22.3507810903025,-22.2428041434464,-22.1347762876769,
-22.026550528337,-21.9491342297182,-21.8399643063501,-21.7288995568295,
-21.620030068311,-21.511227152776,-21.4024508012033,-21.2896996784488,-21.1807855025796,
-21.0661159063825,-20.9514463101855,-20.8422763849356,-20.7312116356503,
-20.6223421452257,-20.5135392277807,-20.4047628742975,-20.2920117533864,
-20.1830975756272,-20.0684279831401,-19.9537583906529,-19.8445884711759,
-19.733523721169,-19.624654236503,-19.5158513247957,-19.40707497702,-19.2943238505451,
-19.1854096783537,-19.0707400747369,-18.9560704711202,-18.8469005466336,
-18.7358357972529,-18.6269663077043,-18.5181633911742,-18.4093870386433,
-18.2966359168794,-18.1877217401528,-18.0730521458702,-17.9583825515876,
-17.8492126150935,-17.7381478672137,-17.6292783654402,-17.520475436639,
-17.4116990718104,-17.2989479618716,-17.1900337729252,-17.0753642024901,
-16.9606946320549,-16.8349352911367,-16.7102672428761,-16.6076077530603),
 .UNSPECIFIED.);
#742=B_SPLINE_CURVE_WITH_KNOTS('',3,(#64516,#64517,#64518,#64519,#64520,
#64521,#64522,#64523,#64524,#64525,#64526,#64527,#64528,#64529,#64530,#64531,
#64532,#64533,#64534,#64535,#64536,#64537,#64538,#64539,#64540,#64541,#64542,
#64543,#64544,#64545,#64546,#64547,#64548,#64549,#64550,#64551,#64552,#64553,
#64554,#64555,#64556,#64557,#64558,#64559,#64560,#64561,#64562,#64563,#64564,
#64565,#64566,#64567,#64568,#64569,#64570,#64571,#64572,#64573,#64574,#64575,
#64576,#64577,#64578,#64579,#64580,#64581,#64582,#64583,#64584,#64585,#64586,
#64587,#64588,#64589,#64590,#64591,#64592,#64593,#64594,#64595,#64596,#64597,
#64598,#64599,#64600,#64601,#64602,#64603,#64604,#64605,#64606,#64607,#64608,
#64609,#64610,#64611,#64612,#64613,#64614,#64615,#64616,#64617,#64618,#64619,
#64620,#64621,#64622,#64623,#64624,#64625,#64626,#64627,#64628,#64629,#64630,
#64631,#64632,#64633,#64634,#64635,#64636,#64637,#64638,#64639,#64640,#64641,
#64642,#64643,#64644,#64645,#64646,#64647,#64648,#64649,#64650,#64651,#64652,
#64653,#64654,#64655,#64656,#64657,#64658,#64659,#64660,#64661,#64662,#64663,
#64664,#64665,#64666,#64667,#64668,#64669,#64670,#64671,#64672,#64673,#64674,
#64675,#64676,#64677,#64678,#64679,#64680,#64681,#64682,#64683,#64684,#64685,
#64686,#64687),.UNSPECIFIED.,.F.,.F.,(4,3,3,3,3,3,3,3,3,3,3,3,3,3,3,3,3,
3,3,3,3,3,3,3,3,3,3,3,3,3,3,3,3,3,3,3,3,3,3,3,3,3,3,3,3,3,3,3,3,3,3,3,3,
3,3,3,3,4),(-16.6076077526092,-16.4984911608107,-16.3893763320133,-16.2801378311394,
-16.1708390750773,-16.0613160672559,-15.9630067125223,-15.8538367706882,
-15.7427720234759,-15.6339025172588,-15.5250995843561,-15.4163232157718,
-15.3035721100763,-15.1946579182654,-15.0799883556275,-14.9653187929897,
-14.8561487806862,-14.7450840422826,-14.6362144637235,-14.5274114579869,
-14.4186350161989,-14.3058839805135,-14.1969697154406,-14.0823002944488,
-13.967630873457,-13.8584612145722,-13.7473964319912,-13.6385272072156,
-13.5297245544302,-13.4209484641989,-13.3081970866303,-13.1992831656195,
-13.084613059772,-12.9699429539244,-12.8607728116244,-12.7497080894703,
-12.6408383878908,-12.5320352620388,-12.4232587032078,-12.3105077860037,
-12.2015934127785,-12.0869242235851,-11.9722550343917,-11.8630845379244,
-11.7520198600413,-11.6431497886023,-11.5343462881227,-11.4255693505448,
-11.3128187916234,-11.2039040339403,-11.0892355743997,-10.9745671148591,
-10.8651519782074,-10.7559060984897,-10.6467953979075,-10.5377672062601,
-10.428744585677,-10.3244224454296),.UNSPECIFIED.);
#743=B_SPLINE_CURVE_WITH_KNOTS('',3,(#64688,#64689,#64690,#64691,#64692,
#64693,#64694,#64695,#64696,#64697,#64698,#64699,#64700,#64701,#64702,#64703,
#64704,#64705,#64706,#64707,#64708,#64709,#64710,#64711,#64712,#64713,#64714,
#64715,#64716,#64717,#64718,#64719,#64720,#64721,#64722,#64723,#64724,#64725,
#64726,#64727,#64728,#64729,#64730,#64731,#64732,#64733,#64734,#64735,#64736,
#64737,#64738,#64739,#64740,#64741,#64742,#64743,#64744,#64745,#64746,#64747,
#64748,#64749,#64750,#64751,#64752,#64753,#64754,#64755,#64756,#64757,#64758,
#64759,#64760,#64761,#64762,#64763,#64764,#64765,#64766,#64767,#64768,#64769,
#64770,#64771,#64772,#64773,#64774,#64775,#64776,#64777,#64778,#64779,#64780,
#64781,#64782,#64783,#64784,#64785,#64786,#64787,#64788,#64789,#64790,#64791,
#64792,#64793,#64794,#64795,#64796,#64797,#64798,#64799,#64800,#64801,#64802,
#64803,#64804,#64805,#64806,#64807,#64808,#64809,#64810,#64811,#64812,#64813,
#64814,#64815,#64816,#64817,#64818,#64819,#64820,#64821,#64822,#64823,#64824,
#64825,#64826,#64827,#64828,#64829,#64830,#64831,#64832,#64833,#64834,#64835,
#64836,#64837,#64838,#64839,#64840,#64841,#64842,#64843,#64844,#64845,#64846,
#64847,#64848,#64849,#64850,#64851,#64852,#64853,#64854,#64855,#64856,#64857,
#64858,#64859),.UNSPECIFIED.,.F.,.F.,(4,3,3,3,3,3,3,3,3,3,3,3,3,3,3,3,3,
3,3,3,3,3,3,3,3,3,3,3,3,3,3,3,3,3,3,3,3,3,3,3,3,3,3,3,3,3,3,3,3,3,3,3,3,
3,3,3,3,4),(-10.3244224449824,-10.1993916813248,-10.0731708785139,-9.97687919532644,
-9.86770700904284,-9.75664254238671,-9.64777083422229,-9.5389657210407,
-9.43018719717089,-9.31743821682662,-9.20852195600055,-9.09385661589717,
-8.9791912757938,-8.87001793349893,-8.7589536113442,-8.65008061887294,-8.54127417765129,
-8.43249428455432,-8.31974655248103,-8.21082883731402,-8.09616609678758,
-7.98150335626115,-7.87234973519855,-7.76128294788979,-7.65242977373111,
-7.54364313252348,-7.4348829893877,-7.3221161012229,-7.21321778455413,-7.09851661064132,
-6.98381543672851,-6.87462385635979,-6.7635618139643,-6.65467097820688,
-6.54584688799528,-6.43704956703977,-6.32431905457879,-6.21538465604731,
-6.10075608662159,-5.98612751719586,-5.87693981736238,-5.76587728989998,
-5.65698930848159,-5.5481676868544,-5.43937244824885,-5.32663923560244,
-5.21770594836024,-5.10307277301173,-4.98843959766322,-4.88022583904749,
-4.77220199698845,-4.66428364169945,-4.55642929382362,-4.44859756765392,
-4.34067235294103,-4.23270085154882,-4.12453357256264,-4.04123713858576),
 .UNSPECIFIED.);
#744=B_SPLINE_CURVE_WITH_KNOTS('',3,(#64862,#64863,#64864,#64865,#64866,
#64867,#64868,#64869,#64870,#64871,#64872,#64873,#64874,#64875,#64876,#64877,
#64878,#64879,#64880,#64881,#64882,#64883,#64884,#64885,#64886),
 .UNSPECIFIED.,.F.,.F.,(4,3,3,3,3,3,3,3,4),(65.1150562521972,65.2322256069618,
65.3494523200733,65.4669033672003,65.5418737844617,65.669718746099,65.7971813969394,
65.9240711597633,65.9734457248706),.UNSPECIFIED.);
#745=B_SPLINE_CURVE_WITH_KNOTS('',3,(#64888,#64889,#64890,#64891,#64892,
#64893,#64894,#64895,#64896,#64897,#64898,#64899,#64900,#64901,#64902,#64903,
#64904,#64905,#64906,#64907,#64908,#64909,#64910,#64911,#64912,#64913,#64914,
#64915,#64916,#64917,#64918,#64919,#64920,#64921,#64922,#64923,#64924,#64925,
#64926,#64927,#64928,#64929,#64930,#64931,#64932,#64933,#64934,#64935,#64936,
#64937,#64938,#64939,#64940,#64941,#64942,#64943,#64944,#64945,#64946,#64947,
#64948,#64949,#64950,#64951,#64952,#64953,#64954,#64955,#64956,#64957,#64958,
#64959,#64960,#64961,#64962,#64963,#64964,#64965,#64966,#64967,#64968,#64969,
#64970,#64971,#64972,#64973,#64974,#64975,#64976,#64977,#64978,#64979,#64980,
#64981,#64982,#64983,#64984,#64985,#64986,#64987,#64988,#64989,#64990,#64991,
#64992,#64993,#64994,#64995,#64996,#64997,#64998,#64999,#65000,#65001,#65002,
#65003,#65004,#65005,#65006,#65007,#65008,#65009,#65010,#65011,#65012,#65013,
#65014),.UNSPECIFIED.,.F.,.F.,(4,3,3,3,3,3,3,3,3,3,3,3,3,3,3,3,3,3,3,3,
3,3,3,3,3,3,3,3,3,3,3,3,3,3,3,3,3,3,3,3,3,3,4),(65.9734457253856,66.0931803203325,
66.2131255046649,66.3331795104007,66.453526391453,66.5395617039943,66.6570817211347,
66.7743859463503,66.8915713205084,67.0086877877879,67.1257851800162,67.2429971337764,
67.3602722427648,67.4777663961338,67.537249623527,67.6546175408908,67.7717689826245,
67.8888012744095,68.0057646433112,68.1227092034736,68.239769929466,68.356894496607,
68.4742409440685,68.5349375430596,68.65265075336,68.7701461217343,68.8875212053768,
69.0048256039178,69.1221088027688,69.2395019098775,69.3569557779961,69.4746229182873,
69.5326254625923,69.650210022574,69.7675822346185,69.8848376574316,70.0020260737922,
70.1191971568852,70.2364847930213,70.3538368252063,70.4714088735417,70.5303133821249,
70.5406671969722),.UNSPECIFIED.);
#746=B_SPLINE_CURVE_WITH_KNOTS('',3,(#65018,#65019,#65020,#65021,#65022,
#65023,#65024,#65025,#65026,#65027,#65028,#65029,#65030,#65031,#65032,#65033,
#65034,#65035,#65036,#65037,#65038,#65039,#65040,#65041,#65042,#65043,#65044,
#65045,#65046,#65047,#65048,#65049,#65050,#65051,#65052,#65053,#65054,#65055,
#65056,#65057,#65058,#65059,#65060,#65061,#65062,#65063,#65064,#65065,#65066,
#65067,#65068,#65069,#65070,#65071,#65072,#65073,#65074,#65075,#65076,#65077,
#65078,#65079,#65080,#65081,#65082,#65083,#65084,#65085,#65086,#65087,#65088,
#65089,#65090,#65091,#65092,#65093,#65094,#65095,#65096,#65097,#65098,#65099,
#65100,#65101,#65102,#65103,#65104,#65105),.UNSPECIFIED.,.F.,.F.,(4,3,3,
3,3,3,3,3,3,3,3,3,3,3,3,3,3,3,3,3,3,3,3,3,3,3,3,3,3,4),(65.9734457260144,
66.1301294810741,66.2052997541048,66.3228842060623,66.4402563097625,66.5575116241308,
66.6746999321573,66.7918709072384,66.9091584367217,67.0265103628761,67.1440823074026,
67.2029876736375,67.3193780628697,67.4355547744305,67.5516145993876,67.6676093259448,
67.7835906279157,67.8997035752663,68.0158874444454,68.1323155233877,68.2006755931701,
68.3253865831117,68.4457795259765,68.5660152672273,68.6861349469942,68.8061795199567,
68.9262260304059,69.0462720762451,69.1664064774643,69.1983635127028),
 .UNSPECIFIED.);
#747=B_SPLINE_CURVE_WITH_KNOTS('',3,(#65106,#65107,#65108,#65109,#65110,
#65111,#65112,#65113,#65114,#65115,#65116,#65117,#65118,#65119,#65120,#65121,
#65122,#65123,#65124,#65125,#65126,#65127,#65128,#65129,#65130,#65131),
 .UNSPECIFIED.,.F.,.F.,(4,2,2,2,2,2,2,2,2,2,2,2,4),(-1.60477775251229,-1.58384253663988,
-1.57768502680862,-1.57259023840276,-1.56713336014366,-1.55999142624319,
-1.53082582288673,-1.51900551052497,-1.51135046950296,-1.50770451735264,
-1.5045888071128,-1.49970347412066,-1.49514144568264),.UNSPECIFIED.);
#748=B_SPLINE_CURVE_WITH_KNOTS('',3,(#65136,#65137,#65138,#65139,#65140,
#65141,#65142,#65143,#65144,#65145,#65146,#65147,#65148,#65149,#65150,#65151,
#65152,#65153,#65154,#65155,#65156,#65157,#65158,#65159,#65160,#65161,#65162,
#65163,#65164,#65165,#65166,#65167,#65168,#65169,#65170,#65171,#65172,#65173,
#65174,#65175,#65176,#65177,#65178,#65179,#65180,#65181,#65182,#65183,#65184,
#65185,#65186,#65187,#65188,#65189,#65190,#65191,#65192,#65193,#65194,#65195,
#65196,#65197,#65198,#65199,#65200,#65201,#65202,#65203,#65204,#65205,#65206,
#65207,#65208,#65209,#65210,#65211),.UNSPECIFIED.,.F.,.F.,(4,3,3,3,3,3,
3,3,3,3,3,3,3,3,3,3,3,3,3,3,3,3,3,3,3,4),(-0.295806539842427,-0.276346651201055,
-0.259153393254382,-0.254907740575419,-0.235952882819617,-0.223306156021738,
-0.218631602919718,-0.200333195629182,-0.182499890135021,-0.171713515924353,
-0.162763868116522,-0.158783796512119,-0.141685011629867,-0.139512866501546,
-0.121939884475205,-0.106697398915805,-0.103668917575034,-0.0868295933515879,
-0.0702531503661989,-0.0538124404507125,-0.0507919491436113,-0.0475503654479505,
-0.0317536154610128,-0.0158768077305064,-0.000838403874092872,0.),
 .UNSPECIFIED.);
#749=B_SPLINE_CURVE_WITH_KNOTS('',3,(#65212,#65213,#65214,#65215,#65216,
#65217,#65218,#65219,#65220,#65221,#65222,#65223,#65224,#65225,#65226,#65227,
#65228,#65229,#65230,#65231,#65232,#65233,#65234,#65235,#65236,#65237,#65238,
#65239,#65240,#65241,#65242,#65243,#65244,#65245,#65246,#65247,#65248,#65249,
#65250,#65251,#65252,#65253,#65254,#65255,#65256,#65257,#65258,#65259,#65260,
#65261,#65262,#65263,#65264,#65265,#65266,#65267,#65268,#65269,#65270,#65271,
#65272,#65273,#65274,#65275,#65276,#65277,#65278,#65279,#65280,#65281,#65282,
#65283,#65284,#65285,#65286,#65287,#65288,#65289,#65290),.UNSPECIFIED.,
 .F.,.F.,(4,3,3,3,3,3,3,3,3,3,3,3,3,3,3,3,3,3,3,3,3,3,3,3,3,3,4),(-0.300067541140094,
-0.284765732859265,-0.273496979675118,-0.269500054551934,-0.253423326962788,
-0.241927110787518,-0.238274241091951,-0.221422988791485,-0.204571736491019,
-0.193777643808902,-0.184331465755972,-0.181440948090128,-0.16362648013299,
-0.161395365762553,-0.144213237170065,-0.134885024745118,-0.128123522255208,
-0.123524962845352,-0.1055412340923,-0.086985134185087,-0.0684290342778744,
-0.0649136170042364,-0.0612783534074245,-0.0420227137929396,-0.0227330075651508,
-0.00361430569105197,0.),.UNSPECIFIED.);
#750=B_SPLINE_CURVE_WITH_KNOTS('',3,(#65548,#65549,#65550,#65551),
 .UNSPECIFIED.,.F.,.F.,(4,4),(-0.0234767871018056,0.),.UNSPECIFIED.);
#751=B_SPLINE_CURVE_WITH_KNOTS('',3,(#65552,#65553,#65554,#65555,#65556,
#65557,#65558,#65559,#65560,#65561,#65562,#65563,#65564,#65565,#65566,#65567,
#65568,#65569,#65570,#65571,#65572,#65573,#65574,#65575,#65576,#65577,#65578,
#65579,#65580,#65581,#65582,#65583,#65584,#65585,#65586,#65587,#65588,#65589,
#65590,#65591,#65592,#65593,#65594,#65595,#65596,#65597,#65598,#65599,#65600,
#65601,#65602,#65603,#65604,#65605,#65606,#65607,#65608,#65609,#65610,#65611,
#65612,#65613,#65614,#65615,#65616,#65617,#65618,#65619,#65620,#65621,#65622,
#65623,#65624,#65625,#65626,#65627,#65628,#65629,#65630),.UNSPECIFIED.,
 .F.,.F.,(4,3,3,3,3,3,3,3,3,3,3,3,3,3,3,3,3,3,3,3,3,3,3,3,3,3,4),(-0.300067541140075,
-0.284903775252137,-0.273496984748414,-0.269500055156834,-0.253431644196808,
-0.241927109392526,-0.238274239829673,-0.221422986437265,-0.204571733044858,
-0.193777641224282,-0.184331461696163,-0.181440940855814,-0.163626472874271,
-0.161395365762553,-0.144213236819044,-0.134885024154862,-0.128123521102825,
-0.12352496320423,-0.105490429091212,-0.0870510242177805,-0.0684290325616374,
-0.0649136213287457,-0.0612783543927973,-0.0420227138085096,-0.0227330091795879,
-0.00361430957713989,-2.23591124697115E-15),.UNSPECIFIED.);
#752=B_SPLINE_CURVE_WITH_KNOTS('',3,(#65635,#65636,#65637,#65638,#65639,
#65640,#65641,#65642,#65643,#65644,#65645,#65646,#65647,#65648,#65649,#65650,
#65651,#65652,#65653,#65654,#65655,#65656,#65657,#65658,#65659,#65660,#65661,
#65662,#65663,#65664,#65665,#65666,#65667,#65668,#65669,#65670,#65671,#65672,
#65673,#65674,#65675,#65676,#65677,#65678,#65679,#65680,#65681,#65682,#65683,
#65684,#65685,#65686,#65687,#65688,#65689,#65690,#65691,#65692,#65693,#65694,
#65695,#65696,#65697,#65698,#65699,#65700,#65701,#65702,#65703,#65704,#65705,
#65706,#65707,#65708,#65709,#65710),.UNSPECIFIED.,.F.,.F.,(4,3,3,3,3,3,
3,3,3,3,3,3,3,3,3,3,3,3,3,3,3,3,3,3,3,4),(-0.295806546771922,-0.276346658132916,
-0.259153396697353,-0.254907741902912,-0.235934549609346,-0.223306160924828,
-0.21863160323213,-0.200313417110245,-0.182506801147177,-0.171713519137717,
-0.162763872690389,-0.158783797445154,-0.141685015599876,-0.139512866501534,
-0.121934206365092,-0.106697398496199,-0.103668916910145,-0.0868283976391997,
-0.0701246001375039,-0.0538124336143781,-0.0507919606835372,-0.0475503673793636,
-0.0317536141940222,-0.0162960065267044,-0.000838398859386542,0.),
 .UNSPECIFIED.);
#753=B_SPLINE_CURVE_WITH_KNOTS('',3,(#65968,#65969,#65970,#65971),
 .UNSPECIFIED.,.F.,.F.,(4,4),(-0.0234767213281991,0.),.UNSPECIFIED.);
#754=B_SPLINE_CURVE_WITH_KNOTS('',3,(#66842,#66843,#66844,#66845,#66846,
#66847,#66848,#66849,#66850,#66851,#66852,#66853,#66854,#66855,#66856,#66857,
#66858,#66859,#66860,#66861,#66862,#66863,#66864,#66865,#66866,#66867,#66868,
#66869,#66870,#66871,#66872,#66873,#66874,#66875,#66876,#66877,#66878,#66879,
#66880,#66881,#66882,#66883,#66884,#66885,#66886,#66887,#66888,#66889,#66890,
#66891,#66892,#66893,#66894,#66895,#66896,#66897,#66898,#66899,#66900,#66901,
#66902,#66903,#66904,#66905,#66906,#66907,#66908,#66909,#66910,#66911,#66912,
#66913,#66914,#66915,#66916,#66917,#66918,#66919,#66920,#66921,#66922,#66923,
#66924,#66925,#66926,#66927,#66928,#66929,#66930,#66931,#66932,#66933,#66934,
#66935,#66936,#66937,#66938,#66939,#66940,#66941,#66942,#66943,#66944,#66945,
#66946,#66947,#66948,#66949,#66950,#66951,#66952,#66953,#66954,#66955,#66956,
#66957,#66958,#66959,#66960,#66961,#66962,#66963,#66964,#66965,#66966,#66967,
#66968,#66969,#66970,#66971,#66972,#66973,#66974,#66975,#66976,#66977,#66978,
#66979,#66980,#66981,#66982,#66983,#66984,#66985,#66986,#66987,#66988,#66989,
#66990,#66991),.UNSPECIFIED.,.F.,.F.,(4,2,2,2,2,2,2,2,2,2,2,2,2,2,2,2,2,
2,2,2,2,2,2,2,2,2,2,2,2,2,2,2,2,2,2,2,2,2,2,2,2,2,2,2,2,2,2,2,2,2,2,2,2,
2,2,2,2,2,2,2,2,2,2,2,2,2,2,2,2,2,2,2,2,2,4),(-0.57814561136758,-0.576296413092534,
-0.573641255529324,-0.570575982215014,-0.565100054282956,-0.539917695991999,
-0.517394447378374,-0.513602331908594,-0.511741570723418,-0.510242310430281,
-0.508340948528616,-0.504346832441546,-0.498825097755031,-0.482729724369596,
-0.457683189040658,-0.452468380911234,-0.449158815326736,-0.44649911229893,
-0.443438658618413,-0.437998831205895,-0.420540876202223,-0.396348568164452,
-0.388039555375418,-0.385470635862254,-0.383865857222333,-0.382305956175603,
-0.379915741966088,-0.372455557398866,-0.358639298966442,-0.329684380929608,
-0.324675436110595,-0.321438891082664,-0.31880269342991,-0.315730719856977,
-0.310163725739934,-0.291420708773143,-0.262555131157506,-0.258796386401061,
-0.256948163636404,-0.25545280771485,-0.253551211796978,-0.249556076524077,
-0.244035210720099,-0.227979871153349,-0.202571226003975,-0.197332498520712,
-0.194009001551785,-0.191338924841252,-0.188267212494532,-0.182807842087583,
-0.165030475351221,-0.139231601339638,-0.132653249078248,-0.130320744596009,
-0.1288153480515,-0.127227747985358,-0.124700541689401,-0.116313972219858,
-0.0993334415849082,-0.0765628114683407,-0.0713569283432376,-0.0680324326380281,
-0.0653451663167553,-0.0622341911963431,-0.0566479026914896,-0.0370860220512205,
-0.017582256991236,-0.0174599552727001,-0.0173504481393084,-0.0172524828413307,
-0.0117389265183658,-0.00594267422071392,-0.00373663500168019,-0.00222440479797267,
-0.00170432960837967),.UNSPECIFIED.);
#755=B_SPLINE_CURVE_WITH_KNOTS('',3,(#66994,#66995,#66996,#66997,#66998,
#66999,#67000,#67001,#67002,#67003,#67004,#67005,#67006,#67007,#67008,#67009,
#67010,#67011,#67012,#67013,#67014,#67015,#67016,#67017,#67018,#67019,#67020,
#67021,#67022,#67023,#67024,#67025,#67026,#67027,#67028,#67029,#67030,#67031,
#67032,#67033,#67034,#67035,#67036,#67037,#67038,#67039,#67040,#67041,#67042,
#67043,#67044,#67045,#67046,#67047,#67048,#67049,#67050,#67051,#67052,#67053,
#67054,#67055,#67056,#67057,#67058,#67059,#67060,#67061,#67062,#67063,#67064,
#67065,#67066,#67067,#67068,#67069,#67070,#67071,#67072,#67073,#67074,#67075,
#67076,#67077,#67078,#67079,#67080,#67081,#67082,#67083,#67084,#67085,#67086,
#67087,#67088,#67089,#67090,#67091,#67092,#67093,#67094,#67095),
 .UNSPECIFIED.,.F.,.F.,(4,2,2,2,2,2,2,2,2,2,2,2,2,2,2,2,2,2,2,2,2,2,2,2,
2,2,2,2,2,2,2,2,2,2,2,2,2,2,2,2,2,2,2,2,2,2,2,2,2,2,4),(-1.318649661076,
-1.31743164617652,-1.31596386436676,-1.31264394085227,-1.29594709662516,
-1.28122934432088,-1.26838464214962,-1.26496788072465,-1.26168833677219,
-1.25870792832702,-1.25486579200619,-1.24618731091111,-1.21648393904188,
-1.20318656193115,-1.19816844726018,-1.19454224790336,-1.19301372216914,
-1.19149228574573,-1.1898443744577,-1.18691776961928,-1.17008318442145,
-1.14747114229976,-1.1394250167213,-1.13330473980141,-1.13019933198268,
-1.12766982200797,-1.12472587504508,-1.11956287795595,-1.08684999296772,
-1.0740249365971,-1.0669291365151,-1.06464970615256,-1.0631437366511,-1.06174272516908,
-1.05978387397002,-1.05448060749719,-1.02076562574725,-1.00652926771878,
-1.00219769891924,-0.999348512279982,-0.996615935546906,-0.992744443746673,
-0.983330401145941,-0.952120651371644,-0.941214068805748,-0.938480088912673,
-0.936816205379131,-0.935259751531581,-0.932908357310751,-0.926522568567024,
-0.912197827138135),.UNSPECIFIED.);
#756=B_SPLINE_CURVE_WITH_KNOTS('',3,(#67100,#67101,#67102,#67103,#67104,
#67105,#67106,#67107,#67108,#67109,#67110,#67111,#67112,#67113,#67114,#67115,
#67116,#67117,#67118,#67119,#67120,#67121,#67122,#67123,#67124,#67125,#67126,
#67127,#67128,#67129,#67130,#67131,#67132,#67133,#67134,#67135,#67136,#67137,
#67138,#67139,#67140,#67141,#67142,#67143,#67144,#67145,#67146,#67147,#67148,
#67149,#67150,#67151,#67152,#67153,#67154,#67155,#67156,#67157,#67158,#67159,
#67160,#67161,#67162,#67163,#67164,#67165,#67166,#67167,#67168,#67169,#67170,
#67171,#67172,#67173,#67174,#67175,#67176,#67177,#67178,#67179,#67180,#67181,
#67182,#67183,#67184,#67185,#67186,#67187,#67188,#67189,#67190,#67191,#67192,
#67193,#67194,#67195,#67196,#67197,#67198,#67199,#67200,#67201,#67202,#67203,
#67204,#67205,#67206,#67207,#67208,#67209,#67210,#67211,#67212,#67213,#67214,
#67215,#67216,#67217,#67218,#67219,#67220,#67221,#67222,#67223,#67224,#67225,
#67226,#67227,#67228,#67229,#67230,#67231,#67232,#67233,#67234,#67235,#67236,
#67237,#67238,#67239,#67240,#67241,#67242,#67243,#67244,#67245,#67246,#67247,
#67248,#67249,#67250,#67251,#67252,#67253,#67254,#67255,#67256,#67257,#67258,
#67259,#67260,#67261,#67262,#67263,#67264,#67265,#67266,#67267,#67268,#67269,
#67270,#67271,#67272,#67273,#67274,#67275,#67276,#67277,#67278,#67279,#67280,
#67281,#67282,#67283,#67284,#67285,#67286,#67287,#67288,#67289,#67290,#67291,
#67292,#67293,#67294,#67295,#67296,#67297,#67298,#67299,#67300,#67301,#67302,
#67303,#67304,#67305,#67306,#67307,#67308,#67309,#67310,#67311),
 .UNSPECIFIED.,.F.,.F.,(4,2,2,2,2,2,2,2,2,2,2,2,2,2,2,2,2,2,2,2,2,2,2,2,
2,2,2,2,2,2,2,2,2,2,2,2,2,2,2,2,2,2,2,2,2,2,2,2,2,2,2,2,2,2,2,2,2,2,2,2,
2,2,2,2,2,2,2,2,2,2,2,2,2,2,2,2,2,2,2,2,2,2,2,2,2,2,2,2,2,2,2,2,2,2,2,2,
2,2,2,2,2,2,2,2,2,4),(-1.38023582942697,-1.36727393991216,-1.35371560626455,
-1.34758612233084,-1.343921800107,-1.34061316589332,-1.34053112229902,-1.34043931642608,
-1.3403365203079,-1.34022134355601,-1.34016271070482,-1.34005242700723,
-1.3398468093432,-1.33815809251505,-1.3352377643514,-1.33045180817441,-1.30897662302457,
-1.29157501945926,-1.28356639925018,-1.27834115990851,-1.27623369214961,
-1.27471833837372,-1.2730058302725,-1.27001812086406,-1.25111770200688,
-1.23630570255573,-1.22495364593259,-1.21701636660591,-1.2134933524464,
-1.21081513541201,-1.20788795402808,-1.20306977280792,-1.18130948763523,
-1.16531976172926,-1.15249883204994,-1.14968381557519,-1.14802568515435,
-1.14650719484141,-1.14428686846135,-1.13870173312281,-1.11507890758532,
-1.09356250686361,-1.0881856924398,-1.08514186799305,-1.08248619566579,
-1.07916826209924,-1.07391367594643,-1.05284974270858,-1.03360977196564,
-1.02908537693002,-1.02372351079304,-1.02159526136499,-1.02007689873916,
-1.01837468805536,-1.01535478228218,-0.996529384285813,-0.981837080157525,
-0.970362461890046,-0.962365079993149,-0.958832057740846,-0.956152418464221,
-0.953229721601869,-0.948433077774452,-0.926850209827973,-0.909849783859956,
-0.897749210878761,-0.894973132600081,-0.89332330855354,-0.891799870665586,
-0.889554584404612,-0.883818167363212,-0.860336468657881,-0.838906369534903,
-0.833529741113932,-0.830485237382186,-0.827828474640885,-0.82450847685547,
-0.819249072614846,-0.796357484571786,-0.774587966790706,-0.769099095389485,
-0.766951592457606,-0.765430332989124,-0.763738186037086,-0.760761742328727,
-0.745207332653177,-0.712064927175208,-0.706929528343931,-0.703647324266641,
-0.70099576924898,-0.697929682490364,-0.692438811248146,-0.688696612541937,
-0.677483780053588,-0.66254578946903,-0.644895009679777,-0.641016489589638,
-0.639141075648444,-0.6376458447114,-0.635770121516414,-0.63189410665383,
-0.626587603279061,-0.611607150850109,-0.584751885349557,-0.579588767808115,
-0.57814561136758),.UNSPECIFIED.);
#757=B_SPLINE_CURVE_WITH_KNOTS('',3,(#67312,#67313,#67314,#67315,#67316,
#67317,#67318,#67319,#67320,#67321,#67322,#67323,#67324,#67325,#67326,#67327,
#67328,#67329,#67330,#67331,#67332,#67333,#67334,#67335,#67336,#67337,#67338,
#67339,#67340,#67341,#67342,#67343,#67344,#67345,#67346,#67347,#67348,#67349,
#67350,#67351,#67352,#67353,#67354,#67355,#67356,#67357,#67358,#67359,#67360,
#67361,#67362,#67363,#67364,#67365,#67366,#67367,#67368,#67369,#67370,#67371,
#67372,#67373,#67374,#67375,#67376,#67377,#67378,#67379,#67380,#67381,#67382,
#67383,#67384,#67385,#67386,#67387,#67388,#67389,#67390,#67391,#67392,#67393,
#67394,#67395,#67396,#67397,#67398,#67399,#67400,#67401,#67402,#67403,#67404,
#67405,#67406,#67407,#67408,#67409,#67410,#67411,#67412,#67413,#67414,#67415,
#67416,#67417,#67418,#67419,#67420,#67421,#67422,#67423,#67424,#67425,#67426,
#67427,#67428,#67429,#67430,#67431,#67432,#67433,#67434,#67435,#67436,#67437,
#67438,#67439,#67440,#67441,#67442,#67443,#67444,#67445,#67446,#67447,#67448,
#67449,#67450,#67451,#67452,#67453,#67454,#67455,#67456,#67457,#67458,#67459,
#67460,#67461,#67462,#67463,#67464,#67465,#67466,#67467,#67468,#67469,#67470,
#67471,#67472,#67473,#67474,#67475,#67476,#67477,#67478,#67479,#67480,#67481,
#67482,#67483,#67484,#67485,#67486,#67487,#67488,#67489,#67490,#67491,#67492,
#67493,#67494,#67495,#67496,#67497,#67498,#67499,#67500,#67501,#67502,#67503,
#67504,#67505,#67506,#67507,#67508,#67509,#67510,#67511,#67512,#67513),
 .UNSPECIFIED.,.F.,.F.,(4,2,2,2,2,2,2,2,2,2,2,2,2,2,2,2,2,2,2,2,2,2,2,2,
2,2,2,2,2,2,2,2,2,2,2,2,2,2,2,2,2,2,2,2,2,2,2,2,2,2,2,2,2,2,2,2,2,2,2,2,
2,2,2,2,2,2,2,2,2,2,2,2,2,2,2,2,2,2,2,2,2,2,2,2,2,2,2,2,2,2,2,2,2,2,2,2,
2,2,2,2,4),(-0.912197827138135,-0.900546199742846,-0.882740080166755,-0.877276848729105,
-0.87420458867794,-0.871534938336999,-0.868213171824111,-0.862979623827371,
-0.837294669421898,-0.821399737697169,-0.813292325056683,-0.810819299780855,
-0.80923232690993,-0.807836500252428,-0.805894466986116,-0.800715257100852,
-0.776732509135995,-0.761472510343384,-0.754898003265771,-0.749603032302451,
-0.746587085452515,-0.743945875155078,-0.740633716807298,-0.73536514512806,
-0.714333990831212,-0.694904842353685,-0.690355086583755,-0.684978663816953,
-0.682856691221549,-0.681344773564849,-0.679647540897774,-0.676651654041828,
-0.659567615862423,-0.630502651288208,-0.623210744390032,-0.619794566198917,
-0.617125366538986,-0.614134142471098,-0.609026791915333,-0.602763321734904,
-0.588717224411485,-0.567800480516633,-0.558812807840408,-0.556173769635394,
-0.554550706351212,-0.552988099678455,-0.550623966689748,-0.543493671585025,
-0.521319091753183,-0.499125206562843,-0.494346049589137,-0.491426211160512,
-0.488744113011381,-0.485200319950247,-0.477143785509341,-0.465548377900303,
-0.450939542629863,-0.432147184684293,-0.429128115647081,-0.427425965017967,
-0.425908121779637,-0.423780793358204,-0.418420538617579,-0.413897923689911,
-0.394664734957041,-0.373611549271333,-0.368362614572839,-0.36504734986907,
-0.362393387126308,-0.359351140731567,-0.353976464165174,-0.350340390713623,
-0.344436566516383,-0.321981988903486,-0.30472263868096,-0.301726802314854,
-0.300030506500816,-0.298510672817766,-0.296372371615432,-0.29094522638229,
-0.286342433098,-0.266490459338093,-0.244342140841239,-0.239561670201648,
-0.236641836214504,-0.233960285335861,-0.230418016471577,-0.222368375240227,
-0.210784316703314,-0.196186938439091,-0.177412056360276,-0.174428152598249,
-0.172716017721806,-0.171199851310539,-0.169089469839861,-0.163847025814943,
-0.155802938334471,-0.125431168164938,-0.11525581156426,-0.111303140211141,
-0.109929022958247),.UNSPECIFIED.);
#758=B_SPLINE_CURVE_WITH_KNOTS('',3,(#67519,#67520,#67521,#67522,#67523,
#67524,#67525,#67526,#67527,#67528),.UNSPECIFIED.,.F.,.F.,(4,1,1,1,1,1,
1,4),(21.9911545791849,22.3044925686794,23.3019991506414,24.2995057326034,
25.2970123145654,26.2945188965274,27.2920254784894,27.4168483341474),
 .UNSPECIFIED.);
#759=B_SPLINE_CURVE_WITH_KNOTS('',3,(#67529,#67530,#67531,#67532,#67533,
#67534,#67535,#67536,#67537,#67538,#67539,#67540,#67541,#67542,#67543,#67544,
#67545,#67546,#67547,#67548,#67549,#67550,#67551,#67552,#67553,#67554,#67555,
#67556,#67557,#67558,#67559,#67560),.UNSPECIFIED.,.F.,.F.,(4,2,2,2,2,2,
2,2,2,2,2,2,2,2,2,4),(-1.48989964064444,-1.47872022988109,-1.47217755902933,
-1.46929575414241,-1.46681092895138,-1.46413326237901,-1.46067282223444,
-1.45288472447889,-1.43040071064657,-1.40874861758075,-1.40514874379073,
-1.4032474542522,-1.40175146608248,-1.3998993055758,-1.39614539370723,-1.38023582942697),
 .UNSPECIFIED.);
#760=B_SPLINE_CURVE_WITH_KNOTS('',3,(#67562,#67563,#67564,#67565,#67566,
#67567,#67568,#67569,#67570,#67571,#67572,#67573,#67574,#67575,#67576,#67577,
#67578,#67579,#67580,#67581,#67582,#67583,#67584,#67585,#67586,#67587,#67588,
#67589,#67590,#67591,#67592,#67593,#67594,#67595,#67596,#67597,#67598,#67599,
#67600,#67601,#67602,#67603,#67604,#67605),.UNSPECIFIED.,.F.,.F.,(4,2,2,
2,2,2,2,2,2,2,2,2,2,2,2,2,2,2,2,2,2,4),(-0.109929022958247,-0.108827709523117,
-0.106248753533545,-0.106095865042436,-0.105952645963057,-0.105816458283612,
-0.105685184526301,-0.105557054470989,-0.105430525151244,-0.105304193208834,
-0.100925002687213,-0.0956454561187019,-0.0849423192460175,-0.0694325087816073,
-0.0514614323326723,-0.0475756570868673,-0.0456981019448579,-0.0442024164935431,
-0.0423276341335334,-0.0402635563262763,-0.0367985916153872,-0.000389969001955371),
 .UNSPECIFIED.);
#761=B_SPLINE_CURVE_WITH_KNOTS('',3,(#67606,#67607,#67608,#67609,#67610,
#67611,#67612,#67613,#67614,#67615,#67616,#67617,#67618,#67619,#67620,#67621,
#67622,#67623,#67624,#67625,#67626,#67627,#67628,#67629,#67630,#67631,#67632,
#67633,#67634,#67635,#67636,#67637,#67638,#67639,#67640,#67641,#67642,#67643,
#67644,#67645,#67646,#67647,#67648,#67649,#67650,#67651,#67652,#67653,#67654,
#67655,#67656,#67657,#67658,#67659,#67660,#67661,#67662,#67663,#67664,#67665,
#67666,#67667,#67668,#67669,#67670,#67671,#67672,#67673,#67674,#67675,#67676,
#67677,#67678,#67679,#67680,#67681,#67682,#67683,#67684,#67685,#67686,#67687,
#67688,#67689,#67690,#67691,#67692,#67693,#67694,#67695,#67696,#67697,#67698,
#67699,#67700,#67701,#67702,#67703,#67704,#67705,#67706,#67707,#67708,#67709,
#67710,#67711,#67712,#67713,#67714,#67715,#67716,#67717,#67718,#67719,#67720,
#67721,#67722,#67723,#67724,#67725,#67726,#67727,#67728,#67729,#67730,#67731,
#67732,#67733,#67734,#67735,#67736,#67737,#67738,#67739,#67740,#67741,#67742,
#67743,#67744,#67745,#67746,#67747,#67748,#67749,#67750,#67751,#67752,#67753,
#67754,#67755,#67756,#67757,#67758,#67759,#67760,#67761,#67762,#67763,#67764,
#67765,#67766,#67767,#67768,#67769,#67770,#67771,#67772,#67773,#67774,#67775,
#67776,#67777,#67778,#67779,#67780,#67781),.UNSPECIFIED.,.F.,.F.,(4,2,2,
2,2,2,2,2,2,2,2,2,2,2,2,2,2,2,2,2,2,2,2,2,2,2,2,2,2,2,2,2,2,2,2,2,2,2,2,
2,2,2,2,2,2,2,2,2,2,2,2,2,2,2,2,2,2,2,2,2,2,2,2,2,2,2,2,2,2,2,2,2,2,2,2,
2,2,2,2,2,2,2,2,2,2,2,2,4),(-1.60461143394934,-1.59295583522918,-1.58969687259461,
-1.58713600117349,-1.58451749098691,-1.58149594130956,-1.57635988095943,
-1.55789254442106,-1.53793233666413,-1.52799106328758,-1.52446079448715,
-1.52256847341829,-1.52107323202754,-1.51921418095462,-1.51542278630807,
-1.49295974405678,-1.47525451432197,-1.46808444180388,-1.46246476417511,
-1.45941196083208,-1.45749341864908,-1.45456735868366,-1.44975155583518,
-1.42814941060129,-1.40790908203135,-1.40325759170159,-1.40060691652397,
-1.39696135527566,-1.39513067587716,-1.39363427417778,-1.39170975578545,
-1.38771530778068,-1.36256333362951,-1.34692128107798,-1.3402419467513,
-1.33487658102878,-1.33183556894149,-1.32918028494435,-1.32586012847097,
-1.32059644333714,-1.29962069938713,-1.2803288228966,-1.27579792561704,
-1.27043101560275,-1.26830231871488,-1.26678420378276,-1.26508299821651,
-1.26206630302482,-1.24331580779254,-1.22875190546966,-1.2171608299765,
-1.20910765074542,-1.20556623807487,-1.20288623849692,-1.19996899848059,
-1.19519499774944,-1.17386657817923,-1.15334122879147,-1.1486545687781,
-1.14316002326754,-1.14101223813451,-1.13949113827345,-1.13779867465427,
-1.1348229722397,-1.11931676464173,-1.09624305828531,-1.08329387931814,
-1.07911748213852,-1.07632425774352,-1.07361263495037,-1.06971616812769,
-1.0599397115774,-1.03356449037147,-1.01873843399882,-1.01502843688923,
-1.01318511128668,-1.01183862153077,-1.0100068733807,-1.00635586413724,
-0.976963805699658,-0.958363358717214,-0.952935416933458,-0.949881461472766,
-0.947227494290107,-0.943925476865805,-0.938724461420196,-0.912842892704958,
-0.912048192097026),.UNSPECIFIED.);
#762=B_SPLINE_CURVE_WITH_KNOTS('',3,(#67787,#67788,#67789,#67790,#67791,
#67792,#67793,#67794,#67795,#67796,#67797,#67798,#67799,#67800,#67801,#67802,
#67803,#67804,#67805,#67806,#67807,#67808,#67809,#67810,#67811,#67812,#67813,
#67814,#67815,#67816,#67817,#67818,#67819,#67820,#67821,#67822,#67823,#67824,
#67825,#67826,#67827,#67828,#67829,#67830,#67831,#67832,#67833,#67834,#67835,
#67836,#67837,#67838,#67839,#67840,#67841,#67842,#67843,#67844,#67845,#67846,
#67847,#67848,#67849,#67850,#67851,#67852,#67853,#67854,#67855,#67856,#67857,
#67858,#67859,#67860,#67861,#67862,#67863,#67864,#67865,#67866,#67867,#67868,
#67869,#67870,#67871,#67872,#67873,#67874,#67875,#67876,#67877,#67878,#67879,
#67880,#67881,#67882,#67883,#67884,#67885,#67886,#67887,#67888,#67889,#67890,
#67891,#67892,#67893,#67894,#67895,#67896,#67897,#67898,#67899,#67900,#67901,
#67902,#67903,#67904,#67905,#67906,#67907,#67908,#67909,#67910,#67911,#67912,
#67913,#67914,#67915,#67916,#67917,#67918,#67919,#67920,#67921,#67922,#67923,
#67924,#67925,#67926,#67927,#67928,#67929,#67930,#67931,#67932,#67933,#67934,
#67935,#67936,#67937),.UNSPECIFIED.,.F.,.F.,(4,3,3,3,3,3,3,3,3,3,3,3,3,
3,3,3,3,3,3,3,3,3,3,3,3,3,3,3,3,3,3,3,3,3,3,3,3,3,3,3,3,3,3,3,3,3,3,3,3,
3,4),(28.274333882308,28.2895320604514,28.4070356534716,28.5243230424993,
28.641491343524,28.758590535659,28.8756704853353,28.9928648252044,29.1101222354136,
29.2275986095123,29.2870386424133,29.4045422337205,29.5218296210103,29.6389979202831,
29.7560971106555,29.8731770585619,29.9903713966644,30.1076288051063,30.2251051774572,
30.2845452243753,30.402048815337,30.5193362022627,30.6365045011601,30.7536036911465,
30.8706836386574,30.9878779763524,31.1051353843795,31.2226117563091,31.2820518063373,
31.3995553979145,31.516842785472,31.6340110850108,31.7511102756471,31.8681902238148,
31.9853845621724,32.1026419708661,32.220118343461,32.2795583882993,32.3970619796289,
32.5143493669347,32.6315176662193,32.7486168565995,32.8656968045097,32.9828911426097,
33.1001485510454,33.2176249233846,33.2770649702613,33.3945293996392,33.5118245182542,
33.6289923657488,33.6995813315044),.UNSPECIFIED.);
#763=B_SPLINE_CURVE_WITH_KNOTS('',3,(#67938,#67939,#67940,#67941),
 .UNSPECIFIED.,.F.,.F.,(4,4),(27.4168483341474,28.2743318237622),
 .UNSPECIFIED.);
#764=B_SPLINE_CURVE_WITH_KNOTS('',3,(#67942,#67943,#67944,#67945,#67946,
#67947,#67948,#67949,#67950,#67951,#67952,#67953,#67954,#67955,#67956,#67957,
#67958,#67959,#67960,#67961,#67962,#67963,#67964,#67965,#67966,#67967,#67968,
#67969,#67970,#67971,#67972,#67973,#67974,#67975,#67976,#67977,#67978,#67979,
#67980,#67981,#67982,#67983,#67984,#67985,#67986,#67987,#67988,#67989,#67990,
#67991,#67992,#67993,#67994,#67995,#67996,#67997,#67998,#67999,#68000,#68001,
#68002,#68003,#68004,#68005,#68006,#68007,#68008,#68009,#68010,#68011,#68012,
#68013,#68014,#68015,#68016,#68017,#68018,#68019,#68020,#68021,#68022,#68023,
#68024,#68025,#68026,#68027,#68028,#68029,#68030,#68031,#68032,#68033,#68034,
#68035,#68036,#68037,#68038,#68039,#68040,#68041,#68042,#68043,#68044,#68045,
#68046,#68047,#68048,#68049,#68050,#68051,#68052,#68053,#68054,#68055,#68056,
#68057,#68058,#68059,#68060,#68061,#68062,#68063,#68064,#68065,#68066,#68067,
#68068,#68069,#68070,#68071,#68072,#68073,#68074,#68075,#68076,#68077,#68078,
#68079,#68080,#68081,#68082,#68083,#68084,#68085,#68086,#68087,#68088,#68089,
#68090,#68091,#68092,#68093,#68094,#68095,#68096,#68097,#68098,#68099,#68100,
#68101,#68102,#68103,#68104,#68105,#68106,#68107,#68108,#68109,#68110,#68111,
#68112,#68113,#68114,#68115,#68116,#68117,#68118,#68119,#68120,#68121,#68122,
#68123,#68124,#68125,#68126,#68127,#68128,#68129,#68130,#68131,#68132,#68133,
#68134,#68135,#68136,#68137,#68138,#68139,#68140,#68141,#68142,#68143,#68144,
#68145,#68146,#68147,#68148,#68149,#68150,#68151,#68152,#68153,#68154,#68155,
#68156,#68157,#68158,#68159,#68160,#68161,#68162,#68163,#68164,#68165,#68166,
#68167,#68168,#68169,#68170,#68171,#68172,#68173,#68174,#68175,#68176,#68177),
 .UNSPECIFIED.,.F.,.F.,(4,2,2,2,2,2,2,2,2,2,2,2,2,2,2,2,2,2,2,2,2,2,2,2,
2,2,2,2,2,2,2,2,2,2,2,2,2,2,2,2,2,2,2,2,2,2,2,2,2,2,2,2,2,2,2,2,2,2,2,2,
2,2,2,2,2,2,2,2,2,2,2,2,2,2,2,2,2,2,2,2,2,2,2,2,2,2,2,2,2,2,2,2,2,2,2,2,
2,2,2,2,2,2,2,2,2,2,2,2,2,2,2,2,2,2,2,2,2,4),(-0.912048192097026,-0.897193903287954,
-0.891757102115713,-0.887811118919318,-0.885922525591254,-0.884427183118311,
-0.88256419929221,-0.878752693007088,-0.850190635474282,-0.836498509102547,
-0.827479694830447,-0.823787281105917,-0.821084199625904,-0.818569687361485,
-0.814391705207285,-0.802414353835596,-0.779607145104645,-0.762851750132384,
-0.7598577723789,-0.758161361658475,-0.756641500768136,-0.754502139473377,
-0.749064550920135,-0.74444826372594,-0.724483251978669,-0.702499382731449,
-0.697719977415738,-0.694801478857277,-0.692121624438214,-0.688582337773265,
-0.680543390283385,-0.668979946117005,-0.654359167188749,-0.635569575467892,
-0.632551594375238,-0.630850023407637,-0.629331811870553,-0.627203361849867,
-0.621838686723182,-0.617311109419045,-0.598038984964131,-0.577067020851179,
-0.571809318759909,-0.568490700330377,-0.56583530328618,-0.562792697539817,
-0.557420605019109,-0.553787263814848,-0.547889788586742,-0.525473155924292,
-0.508198632944983,-0.505202328971343,-0.50350533819836,-0.501985511723585,
-0.499846959060263,-0.494415466537649,-0.489806777428288,-0.469903386628048,
-0.447836519810407,-0.44305742056549,-0.440138840658775,-0.437458738378408,
-0.433918867993808,-0.425877396242107,-0.414309130225609,-0.399691403202778,
-0.380902685852573,-0.377884550080002,-0.376182865732762,-0.374664532663339,
-0.372535885587055,-0.367170577308199,-0.362642384942705,-0.343366735527645,
-0.322396451717294,-0.317137973073629,-0.313818991267101,-0.311163381019295,
-0.308120615355241,-0.302748470388934,-0.299115177246632,-0.293217966750355,
-0.270804648438807,-0.253522142301399,-0.250525578724478,-0.248828450724155,
-0.247308508850699,-0.245169803805127,-0.23973797677519,-0.235129035217801,
-0.215224924478593,-0.193155313723836,-0.188375855415121,-0.18545705244339,
-0.182776742868282,-0.179236595040061,-0.17119447587694,-0.159625261368032,
-0.145006469060257,-0.126229055672179,-0.123238412258239,-0.121525367815816,
-0.120055790287089,-0.120024690568117,-0.119993873759491,-0.119963297723458,
-0.119932922280232,-0.119902709036972,-0.119872621203619,-0.119842623226302,
-0.119812680682742,-0.119782760123177,-0.119752828823599,-0.119722854653954,
-0.117625590987786,-0.115048214893327,-0.110212516818048,-0.109970659150362),
 .UNSPECIFIED.);
#765=B_SPLINE_CURVE_WITH_KNOTS('',3,(#68183,#68184,#68185,#68186,#68187,
#68188,#68189,#68190,#68191,#68192,#68193,#68194,#68195,#68196,#68197,#68198,
#68199,#68200,#68201,#68202,#68203,#68204,#68205,#68206,#68207,#68208,#68209,
#68210,#68211,#68212,#68213,#68214,#68215,#68216,#68217,#68218,#68219,#68220,
#68221,#68222,#68223,#68224,#68225,#68226,#68227,#68228,#68229,#68230,#68231,
#68232,#68233,#68234,#68235,#68236,#68237,#68238,#68239,#68240,#68241,#68242,
#68243,#68244,#68245,#68246,#68247,#68248,#68249,#68250,#68251,#68252,#68253,
#68254,#68255,#68256,#68257,#68258,#68259,#68260,#68261,#68262,#68263,#68264,
#68265,#68266,#68267,#68268,#68269,#68270,#68271,#68272,#68273,#68274,#68275,
#68276,#68277,#68278,#68279,#68280,#68281,#68282,#68283,#68284,#68285,#68286,
#68287,#68288,#68289,#68290,#68291,#68292,#68293,#68294,#68295,#68296,#68297,
#68298,#68299,#68300,#68301,#68302,#68303,#68304,#68305,#68306,#68307,#68308,
#68309,#68310,#68311,#68312,#68313,#68314,#68315,#68316,#68317,#68318,#68319,
#68320,#68321,#68322,#68323,#68324,#68325,#68326,#68327,#68328,#68329,#68330,
#68331,#68332,#68333,#68334,#68335,#68336,#68337,#68338,#68339,#68340,#68341,
#68342,#68343,#68344,#68345,#68346,#68347,#68348,#68349,#68350,#68351,#68352,
#68353,#68354,#68355,#68356,#68357,#68358,#68359,#68360,#68361,#68362,#68363,
#68364,#68365,#68366,#68367,#68368,#68369,#68370,#68371,#68372,#68373,#68374,
#68375,#68376,#68377,#68378,#68379,#68380,#68381,#68382,#68383,#68384,#68385,
#68386,#68387,#68388,#68389,#68390),.UNSPECIFIED.,.F.,.F.,(4,2,2,2,2,2,
2,2,2,2,2,2,2,2,2,2,2,2,2,2,2,2,2,2,2,2,2,2,2,2,2,2,2,2,2,2,2,2,2,2,2,2,
2,2,2,2,2,2,2,2,2,2,2,2,2,2,2,2,2,2,2,2,2,2,2,2,2,2,2,2,2,2,2,2,2,2,2,2,
2,2,2,2,2,2,2,2,2,2,2,2,2,2,2,2,2,2,2,2,2,2,2,2,2,4),(-0.693066393259155,
-0.674906229938858,-0.669695437266216,-0.666390072292241,-0.663735182271511,
-0.660682084047088,-0.655260976408456,-0.648490228107516,-0.632483582971117,
-0.607027920981691,-0.603539708069288,-0.60171810338321,-0.600370683697547,
-0.598515383348405,-0.594745496399711,-0.579381515359838,-0.55142437542294,
-0.543304037998711,-0.540014044368528,-0.537299532118133,-0.534508079932375,
-0.530343570696701,-0.517522269532378,-0.494928775281844,-0.47876086670957,
-0.475771234080074,-0.474075444722218,-0.472554735866463,-0.470412193829133,
-0.464955793622309,-0.46031697425351,-0.44017427137986,-0.418475759716522,
-0.413662641585343,-0.410736487363225,-0.408057883529762,-0.404532424216253,
-0.396581116946435,-0.385198662333336,-0.370389535867719,-0.351483909403705,
-0.348496175341454,-0.346783637871101,-0.345268161446529,-0.343160519728219,
-0.337934638715828,-0.329926235081169,-0.31265927996927,-0.291108173467055,
-0.286312740235186,-0.283390244756187,-0.280710430450574,-0.277176655060345,
-0.26917546318399,-0.257690932346598,-0.242984492870763,-0.224144302180962,
-0.221123943979906,-0.219421521998448,-0.217902888230671,-0.215774257034712,
-0.210411162278677,-0.205886022501703,-0.186635319604914,-0.165623919848117,
-0.160369570075876,-0.157051343434937,-0.154395180834349,-0.154174079737939,
-0.154055433945555,-0.153992186195788,-0.153876447869909,-0.153773081919531,
-0.153680678727045,-0.153597999905942,-0.153523957238636,-0.153457593715937,
-0.153398066757247,-0.153344633533162,-0.153296638187705,-0.153253500756339,
-0.15321470760693,-0.15317980316396,-0.153148382734162,-0.153120086296268,
-0.149541605852723,-0.140967508289976,-0.128183370529552,-0.102955114776677,
-0.0957076419459197,-0.0932565679957738,-0.0918335628704321,-0.0902758157150152,
-0.0886796347272504,-0.0843793562968723,-0.0689392068738299,-0.044875813738082,
-0.0346653684092674,-0.030707667992101,-0.0282312462253062,-0.0257169962615631,
-0.0230399161961442,-0.0194315076543716,-0.000374860171283078),
 .UNSPECIFIED.);
#766=B_SPLINE_CURVE_WITH_KNOTS('',3,(#68391,#68392,#68393,#68394,#68395,
#68396,#68397,#68398,#68399,#68400,#68401,#68402,#68403,#68404,#68405,#68406,
#68407,#68408,#68409,#68410,#68411,#68412),.UNSPECIFIED.,.F.,.F.,(4,3,3,
3,3,3,3,4),(33.6995813315044,33.8166629614849,33.9338446683203,34.0510716663033,
34.168532981513,34.2745715522233,34.4195088297933,34.557519189051),
 .UNSPECIFIED.);
#767=B_SPLINE_CURVE_WITH_KNOTS('',3,(#68414,#68415,#68416,#68417,#68418,
#68419,#68420,#68421,#68422,#68423,#68424,#68425,#68426,#68427,#68428,#68429,
#68430,#68431,#68432,#68433,#68434,#68435),.UNSPECIFIED.,.F.,.F.,(4,2,2,
2,2,2,2,2,2,2,4),(-0.109970659150362,-0.0881264654925452,-0.0658920433884551,
-0.0610673507265949,-0.0581389916306896,-0.0554614768900394,-0.0519420341948714,
-0.0440255142552692,-0.0327138928635081,-0.0179861676643662,-0.000375331772795134),
 .UNSPECIFIED.);
#768=B_SPLINE_CURVE_WITH_KNOTS('',3,(#68436,#68437,#68438,#68439,#68440,
#68441,#68442,#68443,#68444,#68445,#68446,#68447,#68448,#68449,#68450,#68451,
#68452,#68453,#68454,#68455,#68456,#68457,#68458,#68459,#68460,#68461,#68462,
#68463,#68464,#68465,#68466,#68467,#68468,#68469,#68470,#68471,#68472,#68473,
#68474,#68475,#68476,#68477,#68478,#68479,#68480,#68481,#68482,#68483,#68484,
#68485,#68486,#68487,#68488,#68489,#68490,#68491,#68492,#68493,#68494,#68495,
#68496,#68497,#68498,#68499,#68500,#68501,#68502,#68503,#68504,#68505,#68506,
#68507,#68508,#68509,#68510,#68511,#68512,#68513,#68514,#68515,#68516,#68517,
#68518,#68519,#68520,#68521,#68522,#68523,#68524,#68525,#68526,#68527,#68528,
#68529,#68530,#68531,#68532,#68533,#68534,#68535,#68536,#68537,#68538,#68539,
#68540,#68541,#68542,#68543,#68544,#68545,#68546,#68547,#68548,#68549,#68550,
#68551,#68552,#68553,#68554,#68555,#68556,#68557,#68558,#68559,#68560,#68561,
#68562,#68563,#68564,#68565,#68566,#68567,#68568,#68569,#68570,#68571,#68572,
#68573,#68574,#68575,#68576,#68577,#68578,#68579,#68580,#68581,#68582,#68583,
#68584,#68585,#68586,#68587,#68588,#68589,#68590,#68591,#68592,#68593,#68594,
#68595,#68596,#68597,#68598,#68599,#68600,#68601,#68602,#68603,#68604,#68605,
#68606,#68607,#68608,#68609,#68610,#68611,#68612,#68613),.UNSPECIFIED.,
 .F.,.F.,(4,2,2,2,2,2,2,2,2,2,2,2,2,2,2,2,2,2,2,2,2,2,2,2,2,2,2,2,2,2,2,
2,2,2,2,2,2,2,2,2,2,2,2,2,2,2,2,2,2,2,2,2,2,2,2,2,2,2,2,2,2,2,2,2,2,2,2,
2,2,2,2,2,2,2,2,2,2,2,2,2,2,2,2,2,2,2,2,2,4),(-1.60470189091564,-1.60095296946403,
-1.59939692088769,-1.59798940636926,-1.59636898833446,-1.59372612825631,
-1.58456665102568,-1.55978920851748,-1.5439158864618,-1.53853080173819,
-1.53548568883745,-1.53283081567452,-1.52951641732134,-1.52427270745507,
-1.50351491174043,-1.48402315765339,-1.47792196713859,-1.4749089175248,
-1.47302320633092,-1.47130543585475,-1.47014973497877,-1.46833082152723,
-1.46485381500265,-1.43936845750963,-1.42340057789767,-1.41344590430104,
-1.409620351403,-1.40689432887467,-1.40440892972212,-1.4003946874682,-1.38976272433269,
-1.35972748074174,-1.34803177816093,-1.34528019380035,-1.34363605206564,
-1.34211094764519,-1.33985282440251,-1.33403117898286,-1.31061400033734,
-1.28919254965368,-1.28382908980427,-1.28078824474108,-1.27813258973901,
-1.2748112880841,-1.26954437090681,-1.24859297383053,-1.2292822783375,-1.22474869996889,
-1.21937938066883,-1.21725015513871,-1.21573180788214,-1.21403050204633,
-1.21101397507488,-1.19227787196204,-1.17774379359185,-1.16612242505057,
-1.15805428939221,-1.15451014228935,-1.15182947945072,-1.14891287937641,
-1.14414308683646,-1.12289296271921,-1.10521218902712,-1.09721589268933,
-1.09199644049164,-1.08989009137095,-1.08837514244797,-1.08666272030503,
-1.08367435703639,-1.06474582095933,-1.04960625416472,-1.03845921299609,
-1.03473264958251,-1.02925778352664,-1.02619393570368,-1.02354052724862,
-1.02025106870403,-1.01509398528379,-0.988145335134789,-0.973213482996621,
-0.967916857538369,-0.964046995923919,-0.962172691461779,-0.960677244249893,
-0.958799786534675,-0.954913358189951,-0.936681336444259,-0.914454034042733,
-0.912213000320031),.UNSPECIFIED.);
#769=B_SPLINE_CURVE_WITH_KNOTS('',3,(#68618,#68619,#68620,#68621,#68622,
#68623,#68624,#68625,#68626,#68627,#68628,#68629,#68630,#68631,#68632,#68633,
#68634,#68635,#68636,#68637,#68638,#68639,#68640,#68641,#68642,#68643,#68644,
#68645,#68646,#68647,#68648,#68649,#68650,#68651,#68652,#68653,#68654,#68655,
#68656,#68657,#68658,#68659,#68660,#68661,#68662,#68663,#68664,#68665,#68666,
#68667,#68668,#68669,#68670,#68671,#68672,#68673,#68674,#68675,#68676,#68677,
#68678,#68679,#68680,#68681,#68682,#68683,#68684,#68685,#68686,#68687,#68688,
#68689,#68690,#68691,#68692,#68693,#68694,#68695,#68696,#68697,#68698,#68699,
#68700,#68701,#68702,#68703,#68704,#68705,#68706,#68707,#68708,#68709,#68710,
#68711,#68712,#68713,#68714,#68715,#68716,#68717,#68718,#68719,#68720,#68721,
#68722,#68723,#68724,#68725,#68726,#68727,#68728,#68729,#68730,#68731,#68732,
#68733,#68734,#68735,#68736,#68737,#68738,#68739,#68740,#68741,#68742,#68743,
#68744,#68745,#68746,#68747,#68748,#68749,#68750,#68751,#68752,#68753,#68754,
#68755,#68756,#68757,#68758,#68759,#68760,#68761,#68762,#68763,#68764,#68765,
#68766,#68767,#68768,#68769,#68770,#68771,#68772,#68773,#68774,#68775,#68776,
#68777,#68778,#68779,#68780,#68781,#68782,#68783,#68784,#68785,#68786,#68787,
#68788,#68789,#68790,#68791,#68792,#68793,#68794,#68795,#68796,#68797,#68798,
#68799,#68800,#68801,#68802,#68803,#68804,#68805,#68806,#68807,#68808,#68809,
#68810,#68811,#68812,#68813,#68814,#68815,#68816,#68817,#68818,#68819,#68820,
#68821,#68822,#68823,#68824,#68825,#68826,#68827),.UNSPECIFIED.,.F.,.F.,
(4,2,2,2,2,2,2,2,2,2,2,2,2,2,2,2,2,2,2,2,2,2,2,2,2,2,2,2,2,2,2,2,2,2,2,
2,2,2,2,2,2,2,2,2,2,2,2,2,2,2,2,2,2,2,2,2,2,2,2,2,2,2,2,2,2,2,2,2,2,2,2,
2,2,2,2,2,2,2,2,2,2,2,2,2,2,2,2,2,2,2,2,2,2,2,2,2,2,2,2,2,2,2,2,2,4),(-1.49506358435903,
-1.49459316852251,-1.49295987179869,-1.49154761020416,-1.48962849527195,
-1.48551958585863,-1.46046986416288,-1.44482595301145,-1.43814582163569,
-1.43277974809073,-1.42973818189258,-1.42708230725347,-1.42376125009147,
-1.41849573727524,-1.39753559702045,-1.37823521492406,-1.37370308742887,
-1.36833490836962,-1.36620574026705,-1.36468728335974,-1.3629856394231,
-1.35996799539036,-1.34120155414277,-1.32660700712414,-1.31504458880383,
-1.30700497676871,-1.30346531738608,-1.30078506395088,-1.29786599430001,
-1.29308533386462,-1.27101074170306,-1.25108718660959,-1.24647507935482,
-1.2410411040156,-1.23890203920943,-1.23738204310009,-1.23568497927446,
-1.2326888299206,-1.21529497939766,-1.19300466725329,-1.18712646617886,
-1.18350184059288,-1.1781388591753,-1.17509792701522,-1.17244197261471,
-1.16911998099,-1.16385125390158,-1.14292542497544,-1.12360274830032,-1.11906770775998,
-1.11369711877518,-1.11156758305447,-1.11004906650738,-1.10834758789171,
-1.10533073310359,-1.08658844294957,-1.07203881844943,-1.06043475903791,
-1.05237497387356,-1.04883199938223,-1.04615127770301,-1.04323367904321,
-1.03846003478107,-1.01567016700984,-0.996298126047144,-0.991756634007073,
-0.986380699161068,-0.984250339448056,-0.982731681019322,-0.981030554158052,
-0.9780154135377,-0.959327927490739,-0.944888424427529,-0.933184684646064,
-0.925076761712725,-0.921525888972868,-0.918844029195806,-0.915929870677276,
-0.911172694588434,-0.890231472159465,-0.869370980182679,-0.864643600490223,
-0.86196101666687,-0.858282821276543,-0.856445487354999,-0.855098928911026,
-0.85326049452433,-0.84969181577703,-0.825081844443449,-0.802669500212144,
-0.797234870802052,-0.793865129126414,-0.791204984213659,-0.788195458326038,
-0.782983957580618,-0.757313399843094,-0.734785802988896,-0.730994798142771,
-0.729135461641677,-0.727639632896396,-0.725746069217201,-0.721775278484118,
-0.716293897360636,-0.700409747126883,-0.693066393259155),.UNSPECIFIED.);
#770=B_SPLINE_CURVE_WITH_KNOTS('',3,(#68828,#68829,#68830,#68831,#68832,
#68833,#68834,#68835,#68836,#68837,#68838,#68839,#68840,#68841,#68842,#68843,
#68844,#68845,#68846,#68847,#68848,#68849,#68850,#68851,#68852,#68853,#68854,
#68855,#68856,#68857,#68858,#68859,#68860,#68861,#68862,#68863,#68864,#68865,
#68866,#68867,#68868,#68869,#68870,#68871,#68872,#68873,#68874,#68875,#68876,
#68877,#68878,#68879,#68880,#68881,#68882,#68883,#68884,#68885,#68886,#68887,
#68888,#68889,#68890,#68891,#68892,#68893,#68894,#68895,#68896,#68897,#68898,
#68899,#68900,#68901,#68902,#68903,#68904,#68905,#68906,#68907,#68908,#68909,
#68910,#68911,#68912,#68913,#68914,#68915,#68916,#68917,#68918,#68919,#68920,
#68921,#68922,#68923,#68924,#68925,#68926,#68927,#68928,#68929,#68930,#68931,
#68932,#68933,#68934,#68935,#68936,#68937,#68938,#68939,#68940,#68941,#68942,
#68943,#68944,#68945,#68946,#68947,#68948,#68949,#68950,#68951,#68952,#68953,
#68954,#68955,#68956,#68957,#68958,#68959,#68960,#68961,#68962,#68963,#68964,
#68965,#68966,#68967,#68968,#68969,#68970,#68971,#68972,#68973,#68974,#68975,
#68976,#68977,#68978,#68979,#68980,#68981,#68982,#68983,#68984,#68985,#68986,
#68987,#68988,#68989,#68990,#68991,#68992,#68993,#68994,#68995,#68996,#68997,
#68998,#68999,#69000,#69001,#69002,#69003,#69004,#69005,#69006,#69007,#69008,
#69009,#69010,#69011,#69012,#69013,#69014,#69015,#69016,#69017,#69018,#69019,
#69020,#69021,#69022,#69023,#69024,#69025,#69026,#69027,#69028,#69029,#69030,
#69031,#69032,#69033,#69034,#69035),.UNSPECIFIED.,.F.,.F.,(4,2,2,2,2,2,
2,2,2,2,2,2,2,2,2,2,2,2,2,2,2,2,2,2,2,2,2,2,2,2,2,2,2,2,2,2,2,2,2,2,2,2,
2,2,2,2,2,2,2,2,2,2,2,2,2,2,2,2,2,2,2,2,2,2,2,2,2,2,2,2,2,2,2,2,2,2,2,2,
2,2,2,2,2,2,2,2,2,2,2,2,2,2,2,2,2,2,2,2,2,2,2,2,2,4),(-0.912213000320031,
-0.904185423138655,-0.900317621453881,-0.897583697094516,-0.895105821397266,
-0.891771599658252,-0.883373245940542,-0.855674846088848,-0.840393111228322,
-0.836632359294594,-0.834778978194245,-0.83343184280948,-0.831609016922357,
-0.828114371926604,-0.802747979360156,-0.780655750146395,-0.775386105046824,
-0.772063877217642,-0.769407992278481,-0.766367435977363,-0.76100606058388,
-0.754332480936613,-0.731470781708606,-0.713230871208786,-0.709343001741131,
-0.707465204914766,-0.705969674854692,-0.704095500623492,-0.70022664158367,
-0.694932836332411,-0.68001305162414,-0.653087045578872,-0.647931078922335,
-0.644641816397422,-0.641988270290673,-0.638923933862759,-0.633447353207738,
-0.629718945058427,-0.618563751311103,-0.603406768578255,-0.584458957476656,
-0.581470020876322,-0.579757389404236,-0.578242301674307,-0.576135894239818,
-0.570916648870514,-0.562922445546916,-0.545340521356904,-0.524037115108987,
-0.519263324649768,-0.516345708352359,-0.513665017725299,-0.510122185999156,
-0.502063748135204,-0.49046085173145,-0.475878189141995,-0.457107752539287,
-0.454090021396908,-0.452388338554731,-0.450869839211915,-0.448740729155319,
-0.443373053732892,-0.438842153232241,-0.419546980548521,-0.398603840424228,
-0.393341804662594,-0.390021650092343,-0.387365757321423,-0.384323381401009,
-0.378953868555389,-0.375323062539216,-0.352806882741564,-0.331041127461899,
-0.327245160261254,-0.32538486817583,-0.323889076332513,-0.321996624786792,
-0.318031747338709,-0.312561416596615,-0.296736860055886,-0.27113719570378,
-0.26592825929231,-0.262623433317465,-0.259968605248771,-0.256915189675632,
-0.251492511506997,-0.244719280205865,-0.228703630202243,-0.203251925941467,
-0.199762220196112,-0.197940303071016,-0.196592920664014,-0.194738055494788,
-0.190970402351699,-0.17562791302048,-0.147739595214316,-0.139545989277664,
-0.136244228670731,-0.13363872417429,-0.131130223575698,-0.128417538892109,
-0.124710172973325,-0.118469338295433,-0.110007165866594),.UNSPECIFIED.);
#771=B_SPLINE_CURVE_WITH_KNOTS('',3,(#69041,#69042,#69043,#69044,#69045,
#69046,#69047,#69048,#69049,#69050,#69051,#69052,#69053,#69054,#69055,#69056,
#69057,#69058,#69059,#69060,#69061,#69062,#69063,#69064,#69065,#69066,#69067,
#69068,#69069,#69070,#69071,#69072,#69073,#69074,#69075,#69076,#69077,#69078,
#69079,#69080,#69081,#69082,#69083,#69084,#69085,#69086,#69087,#69088,#69089,
#69090,#69091,#69092,#69093,#69094,#69095,#69096,#69097,#69098,#69099,#69100,
#69101,#69102,#69103,#69104,#69105,#69106,#69107,#69108,#69109,#69110,#69111,
#69112,#69113,#69114,#69115,#69116,#69117,#69118,#69119,#69120,#69121,#69122,
#69123,#69124,#69125,#69126,#69127,#69128,#69129,#69130,#69131,#69132,#69133,
#69134,#69135,#69136,#69137,#69138,#69139,#69140,#69141,#69142,#69143,#69144,
#69145,#69146,#69147,#69148,#69149,#69150,#69151,#69152,#69153,#69154,#69155,
#69156,#69157,#69158,#69159,#69160,#69161,#69162,#69163,#69164,#69165,#69166,
#69167,#69168,#69169,#69170,#69171,#69172,#69173,#69174,#69175,#69176,#69177,
#69178,#69179,#69180,#69181,#69182,#69183,#69184,#69185,#69186,#69187,#69188,
#69189,#69190,#69191,#69192,#69193,#69194,#69195,#69196,#69197,#69198,#69199,
#69200,#69201,#69202,#69203,#69204,#69205,#69206,#69207,#69208,#69209,#69210,
#69211,#69212,#69213,#69214,#69215,#69216,#69217,#69218,#69219,#69220,#69221,
#69222),.UNSPECIFIED.,.F.,.F.,(4,2,2,2,2,2,2,2,2,2,2,2,2,2,2,2,2,2,2,2,
2,2,2,2,2,2,2,2,2,2,2,2,2,2,2,2,2,2,2,2,2,2,2,2,2,2,2,2,2,2,2,2,2,2,2,2,
2,2,2,2,2,2,2,2,2,2,2,2,2,2,2,2,2,2,2,2,2,2,2,2,2,2,2,2,2,2,2,2,2,2,4),
(-0.692976027751027,-0.690677018759155,-0.67607130447192,-0.657289354510635,
-0.654305699491911,-0.652594027778611,-0.651078206133527,-0.648968571102928,
-0.643730147392798,-0.635694444396294,-0.604956671733111,-0.600515487569622,
-0.593586963882524,-0.59023955066128,-0.587581085193234,-0.584556430275175,
-0.579273628352794,-0.554770843352943,-0.530999517730569,-0.527332048054737,
-0.52549660458651,-0.524149656932507,-0.5223085422684,-0.518612169647566,
-0.503913952439148,-0.477897660548173,-0.467760697986265,-0.463813346606405,
-0.461338762878883,-0.458599929607237,-0.454708557941114,-0.444265211086943,
-0.426993496985563,-0.403687880719116,-0.399990519196653,-0.398149190010454,
-0.396802416097306,-0.394967212275677,-0.391301078978969,-0.388630827177835,
-0.383933295963051,-0.363314832917524,-0.342122444417286,-0.337354427756351,
-0.334437562698699,-0.33175574471474,-0.328208700088314,-0.320127680685125,
-0.308478835162429,-0.293945782556724,-0.275201555131824,-0.272184190010179,
-0.270482330080033,-0.268963364564397,-0.266833126430772,-0.261460020954143,
-0.256922903642597,-0.237581456219421,-0.214771826489122,-0.210003316459699,
-0.207086302125691,-0.204404445719564,-0.200857497082934,-0.192777387695453,
-0.181130547859992,-0.166594637629413,-0.149280265482203,-0.145396393218514,
-0.143519047756513,-0.143149369139958,-0.141661755510349,-0.13963305064656,
-0.137286949418663,-0.133083790273205,-0.122934175346161,-0.0886229696348173,
-0.0832480468122925,-0.080173330431059,-0.0775452588392117,-0.0742800389403422,
-0.0679988256869937,-0.0653883053324759,-0.0389927124813264,-0.0236378442675931,
-0.0186759487146624,-0.0167512895609681,-0.015218376560855,-0.0138244657348888,
-0.0121928527065857,-0.00981889569000219,-0.000374665579676547),
 .UNSPECIFIED.);
#772=B_SPLINE_CURVE_WITH_KNOTS('',3,(#69223,#69224,#69225,#69226,#69227,
#69228,#69229,#69230,#69231,#69232,#69233,#69234,#69235,#69236,#69237,#69238,
#69239,#69240,#69241,#69242,#69243,#69244,#69245,#69246,#69247,#69248),
 .UNSPECIFIED.,.F.,.F.,(4,2,2,2,2,2,2,2,2,2,2,2,4),(-1.60472169846197,-1.57239004611136,
-1.56559352016807,-1.56167378571222,-1.55812169644377,-1.55543974735561,
-1.55252629288628,-1.54777211810372,-1.52692702746105,-1.51024911685062,
-1.50136262048626,-1.49750125048159,-1.49506358435903),.UNSPECIFIED.);
#773=B_SPLINE_CURVE_WITH_KNOTS('',3,(#69250,#69251,#69252,#69253,#69254,
#69255,#69256,#69257,#69258,#69259,#69260,#69261,#69262,#69263,#69264,#69265,
#69266,#69267,#69268,#69269,#69270,#69271,#69272,#69273,#69274,#69275,#69276,
#69277,#69278,#69279,#69280,#69281),.UNSPECIFIED.,.F.,.F.,(4,2,2,2,2,2,
2,2,2,2,2,2,2,2,2,4),(-0.110007165866594,-0.104507449886709,-0.0838701566740523,
-0.0743878709420968,-0.0717087400849561,-0.070080137279803,-0.0685271391723869,
-0.0662040699472125,-0.0594070965096256,-0.0271399959987747,-0.0136759747962797,
-0.0094316992061634,-0.00659078795257742,-0.0040613220566676,-0.00213809552869001,
-0.000374875370209125),.UNSPECIFIED.);
#774=B_SPLINE_CURVE_WITH_KNOTS('',3,(#69282,#69283,#69284,#69285,#69286,
#69287,#69288,#69289,#69290,#69291,#69292,#69293,#69294,#69295,#69296,#69297,
#69298,#69299,#69300,#69301,#69302,#69303,#69304,#69305,#69306,#69307,#69308,
#69309,#69310,#69311,#69312,#69313,#69314,#69315,#69316,#69317,#69318,#69319,
#69320,#69321,#69322,#69323,#69324,#69325,#69326,#69327,#69328,#69329,#69330,
#69331,#69332,#69333,#69334,#69335,#69336,#69337,#69338,#69339,#69340,#69341,
#69342,#69343,#69344,#69345,#69346,#69347,#69348,#69349,#69350,#69351,#69352,
#69353,#69354,#69355,#69356,#69357,#69358,#69359,#69360,#69361,#69362,#69363,
#69364,#69365,#69366,#69367,#69368,#69369,#69370,#69371,#69372,#69373,#69374,
#69375,#69376,#69377,#69378,#69379,#69380,#69381,#69382,#69383,#69384,#69385,
#69386,#69387,#69388,#69389,#69390,#69391,#69392,#69393,#69394,#69395,#69396,
#69397,#69398,#69399,#69400,#69401,#69402,#69403,#69404,#69405,#69406,#69407,
#69408,#69409,#69410,#69411,#69412,#69413,#69414,#69415,#69416,#69417,#69418,
#69419,#69420,#69421,#69422,#69423,#69424,#69425,#69426,#69427,#69428,#69429,
#69430,#69431,#69432,#69433,#69434,#69435,#69436,#69437,#69438,#69439,#69440,
#69441,#69442,#69443,#69444,#69445,#69446,#69447,#69448,#69449,#69450,#69451,
#69452,#69453,#69454,#69455,#69456,#69457,#69458,#69459,#69460,#69461,#69462,
#69463,#69464,#69465,#69466,#69467,#69468,#69469),.UNSPECIFIED.,.F.,.F.,
(4,2,2,2,2,2,2,2,2,2,2,2,2,2,2,2,2,2,2,2,2,2,2,2,2,2,2,2,2,2,2,2,2,2,2,
2,2,2,2,2,2,2,2,2,2,2,2,2,2,2,2,2,2,2,2,2,2,2,2,2,2,2,2,2,2,2,2,2,2,2,2,
2,2,2,2,2,2,2,2,2,2,2,2,2,2,2,2,2,2,2,2,2,2,4),(-1.60452966110218,-1.60139615323569,
-1.59616027114913,-1.56214671608205,-1.55475260021891,-1.55132820008312,
-1.54855456450182,-1.54690569049585,-1.5453831863967,-1.54313905556618,
-1.53740448052939,-1.51391364726702,-1.50993883305555,-1.49735969596893,
-1.48883954439345,-1.48601194681116,-1.48583118372699,-1.48565234088406,
-1.48546628960481,-1.48526013381114,-1.48501062067329,-1.48465960553332,
-1.48430764242497,-1.48172843252811,-1.4785606293793,-1.47286449254571,
-1.45188293756239,-1.4325561589479,-1.42802054955213,-1.42264960637224,
-1.42052017864715,-1.4190018392707,-1.41730071655422,-1.41428488655772,
-1.39556802960809,-1.38107110745189,-1.36941682586789,-1.36133287342369,
-1.35778621133186,-1.35510526685074,-1.35218992934655,-1.34742584068909,
-1.32628988116273,-1.30847623438016,-1.30048590753895,-1.29526923715334,
-1.29316335962203,-1.29164851785947,-1.28993594881599,-1.28694677947623,
-1.26799407701781,-1.25313665781787,-1.24184119467159,-1.23393194577901,
-1.23041408233831,-1.22773709605892,-1.22480864945179,-1.21998228990476,
-1.19687346179318,-1.17782592331505,-1.1733269434758,-1.16798626922089,
-1.16586139991853,-1.16434373602964,-1.1626404142586,-1.15961434941508,
-1.14060822875449,-1.12571158699456,-1.11447183778685,-1.10658996355613,
-1.10307662914097,-1.10040022105723,-1.09746958854071,-1.09263296286064,
-1.07041839422467,-1.05068522648163,-1.04609718990203,-1.04068304386393,
-1.0385470867333,-1.03702771353008,-1.03532957428315,-1.03232783478608,
-1.014245127035,-0.983252200262885,-0.977814412117494,-0.97475835951896,
-0.972104490284592,-0.968805094204545,-0.963613320763827,-0.937452959056019,
-0.921995285602853,-0.916595328301845,-0.912669276484203,-0.912009248555571),
 .UNSPECIFIED.);
#775=B_SPLINE_CURVE_WITH_KNOTS('',3,(#69474,#69475,#69476,#69477,#69478,
#69479,#69480,#69481,#69482,#69483,#69484,#69485,#69486,#69487,#69488,#69489,
#69490,#69491,#69492,#69493,#69494,#69495,#69496,#69497,#69498,#69499,#69500,
#69501,#69502,#69503,#69504,#69505,#69506,#69507,#69508,#69509,#69510,#69511,
#69512,#69513,#69514,#69515,#69516,#69517,#69518,#69519,#69520,#69521,#69522,
#69523,#69524,#69525,#69526,#69527,#69528,#69529,#69530,#69531,#69532,#69533,
#69534,#69535,#69536,#69537,#69538,#69539,#69540,#69541,#69542,#69543,#69544,
#69545,#69546,#69547,#69548,#69549,#69550,#69551,#69552,#69553,#69554,#69555,
#69556,#69557,#69558,#69559,#69560,#69561,#69562,#69563,#69564,#69565,#69566,
#69567,#69568,#69569,#69570,#69571,#69572,#69573,#69574,#69575,#69576,#69577,
#69578,#69579,#69580,#69581,#69582,#69583,#69584,#69585,#69586,#69587,#69588,
#69589,#69590,#69591,#69592,#69593,#69594,#69595,#69596,#69597,#69598,#69599,
#69600,#69601,#69602,#69603,#69604,#69605,#69606,#69607,#69608,#69609,#69610,
#69611,#69612,#69613,#69614,#69615,#69616,#69617,#69618,#69619,#69620,#69621,
#69622,#69623,#69624,#69625,#69626,#69627,#69628,#69629,#69630,#69631,#69632,
#69633,#69634,#69635,#69636,#69637,#69638,#69639,#69640,#69641,#69642,#69643,
#69644,#69645,#69646,#69647,#69648,#69649,#69650,#69651,#69652,#69653,#69654,
#69655,#69656,#69657,#69658,#69659,#69660,#69661,#69662,#69663,#69664,#69665,
#69666,#69667,#69668,#69669,#69670,#69671,#69672,#69673,#69674,#69675),
 .UNSPECIFIED.,.F.,.F.,(4,2,2,2,2,2,2,2,2,2,2,2,2,2,2,2,2,2,2,2,2,2,2,2,
2,2,2,2,2,2,2,2,2,2,2,2,2,2,2,2,2,2,2,2,2,2,2,2,2,2,2,2,2,2,2,2,2,2,2,2,
2,2,2,2,2,2,2,2,2,2,2,2,2,2,2,2,2,2,2,2,2,2,2,2,2,2,2,2,2,2,2,2,2,2,2,2,
2,2,2,2,4),(-1.49507327327653,-1.48719252098069,-1.48294770072824,-1.4820471916439,
-1.48178889420644,-1.47920758896041,-1.47633380858346,-1.47168614324768,
-1.45076975322874,-1.42986725872078,-1.42513502986856,-1.42245047904512,
-1.41877036451753,-1.41693274391433,-1.41558627954368,-1.41374842139644,
-1.41006710169774,-1.38662246729157,-1.36946824406393,-1.35906816612427,
-1.35518316866157,-1.35244602895658,-1.34997111299487,-1.34601923465861,
-1.33584610277006,-1.3098440644049,-1.29514873571344,-1.29145317741713,
-1.28961248262459,-1.28826585624641,-1.28643085055956,-1.28276429775505,
-1.25903540462543,-1.24205589907407,-1.23171946657212,-1.22784265048085,
-1.22510693153952,-1.22263043708772,-1.21930260098999,-1.2109449171727,
-1.1832097842105,-1.1679168915106,-1.1641548948865,-1.16230119974309,-1.16095395506262,
-1.15913111019459,-1.15563670988857,-1.13027411397566,-1.10745742306897,
-1.10203240215106,-1.09897858837553,-1.09632388415331,-1.0930198071695,
-1.08781314627094,-1.06209783310039,-1.04633310700028,-1.038273538192,-1.03581018759626,
-1.03422838210289,-1.0328268861638,-1.03049017518235,-1.0241072203025,-1.00115569565784,
-0.986285478260796,-0.979802921366489,-0.974558925310408,-0.971542578166978,
-0.968883328041537,-0.96552406304279,-0.95852936884663,-0.929152067421189,
-0.917385045935987,-0.910624556790516,-0.908305906554551,-0.906753810124901,
-0.905123836536867,-0.902438423913228,-0.892879961160621,-0.872328133412494,
-0.853150142875389,-0.847512280971532,-0.844414736372729,-0.841763167617778,
-0.838515332400218,-0.833501665825086,-0.802416151828116,-0.78459835702781,
-0.781598364052852,-0.779900307080142,-0.778380266438147,-0.776242377865235,
-0.770817587207459,-0.766217481918612,-0.746383883285741,-0.724225942957317,
-0.719446862083394,-0.716527783055549,-0.713846873982377,-0.710305397760907,
-0.702257557507502,-0.692976027751027),.UNSPECIFIED.);
#776=B_SPLINE_CURVE_WITH_KNOTS('',3,(#69676,#69677,#69678,#69679,#69680,
#69681,#69682,#69683,#69684,#69685,#69686,#69687,#69688,#69689,#69690,#69691,
#69692,#69693,#69694,#69695,#69696,#69697,#69698,#69699,#69700,#69701,#69702,
#69703,#69704,#69705,#69706,#69707,#69708,#69709,#69710,#69711,#69712,#69713,
#69714,#69715,#69716,#69717,#69718,#69719,#69720,#69721,#69722,#69723,#69724,
#69725,#69726,#69727,#69728,#69729,#69730,#69731,#69732,#69733,#69734,#69735,
#69736,#69737,#69738,#69739,#69740,#69741,#69742,#69743,#69744,#69745,#69746,
#69747,#69748,#69749,#69750,#69751,#69752,#69753,#69754,#69755,#69756,#69757,
#69758,#69759,#69760,#69761,#69762,#69763,#69764,#69765,#69766,#69767,#69768,
#69769,#69770,#69771,#69772,#69773,#69774,#69775,#69776,#69777,#69778,#69779,
#69780,#69781,#69782,#69783,#69784,#69785,#69786,#69787,#69788,#69789,#69790,
#69791,#69792,#69793,#69794,#69795,#69796,#69797,#69798,#69799,#69800,#69801,
#69802,#69803,#69804,#69805,#69806,#69807,#69808,#69809,#69810,#69811,#69812,
#69813,#69814,#69815,#69816,#69817,#69818,#69819,#69820,#69821,#69822,#69823,
#69824,#69825,#69826,#69827,#69828,#69829,#69830,#69831,#69832,#69833,#69834,
#69835,#69836,#69837,#69838,#69839,#69840,#69841,#69842,#69843,#69844,#69845,
#69846,#69847,#69848,#69849,#69850,#69851,#69852,#69853,#69854,#69855,#69856,
#69857,#69858,#69859,#69860,#69861,#69862,#69863,#69864,#69865,#69866,#69867,
#69868,#69869,#69870,#69871,#69872,#69873,#69874,#69875,#69876,#69877,#69878,
#69879,#69880,#69881,#69882,#69883,#69884,#69885,#69886,#69887,#69888,#69889,
#69890,#69891,#69892,#69893,#69894,#69895,#69896,#69897,#69898,#69899,#69900,
#69901),.UNSPECIFIED.,.F.,.F.,(4,2,2,2,2,2,2,2,2,2,2,2,2,2,2,2,2,2,2,2,
2,2,2,2,2,2,2,2,2,2,2,2,2,2,2,2,2,2,2,2,2,2,2,2,2,2,2,2,2,2,2,2,2,2,2,2,
2,2,2,2,2,2,2,2,2,2,2,2,2,2,2,2,2,2,2,2,2,2,2,2,2,2,2,2,2,2,2,2,2,2,2,2,
2,2,2,2,2,2,2,2,2,2,2,2,2,2,2,2,2,2,2,2,4),(-0.912009248555571,-0.910784402950638,
-0.909289046644602,-0.907422346554824,-0.903591713258842,-0.882622942337099,
-0.857892692021188,-0.851255179280141,-0.847962350316943,-0.845308909839391,
-0.842247992512888,-0.836933299051704,-0.802333453471668,-0.787610984940254,
-0.784657787469567,-0.782969996709953,-0.781446841166061,-0.779287586836242,
-0.773716390919297,-0.768935809769165,-0.747617142306819,-0.727253846121918,
-0.722511273796812,-0.719600305866127,-0.716917635026592,-0.71336012745137,
-0.705211181541947,-0.693420146087121,-0.67904876763235,-0.660381678101204,
-0.657367245038164,-0.655666310339294,-0.654147654559383,-0.652017195344845,
-0.646640210832553,-0.642097950440716,-0.62271479616597,-0.599971427264624,
-0.595198129747397,-0.592280650322297,-0.589599979112614,-0.586057015314614,
-0.577997536755071,-0.566392401900445,-0.551812633455501,-0.533043935000858,
-0.53002630190573,-0.52832465831336,-0.526806182118072,-0.524677088241117,
-0.519309368641465,-0.514778380556536,-0.495482268357733,-0.474541513180881,
-0.469279357003971,-0.465959198765666,-0.463303347276791,-0.46026106673824,
-0.454891853230435,-0.448205641016518,-0.432539871035909,-0.407339320875792,
-0.403703025399402,-0.401854091509433,-0.400339962391701,-0.398672142284213,
-0.395812135928608,-0.382046510061183,-0.353888352905454,-0.343586289635233,
-0.339616483537676,-0.337138440253632,-0.334404328575102,-0.330536312694538,
-0.320268342622186,-0.29804531061308,-0.279761385634922,-0.275873065846176,
-0.273995136821017,-0.272499545497755,-0.270625349663056,-0.266756620995827,
-0.261463127026102,-0.246545373619972,-0.21961422785916,-0.214458269126216,
-0.211168935827046,-0.208515285377035,-0.205450776133082,-0.199973740285639,
-0.196244968139523,-0.18508846049105,-0.169931499658724,-0.15240719746132,
-0.148521090343444,-0.146643609415607,-0.145148054534646,-0.145134231998255,
-0.145121479732626,-0.145109713107917,-0.145091632015426,-0.145073850816049,
-0.145056362665238,-0.14503916083859,-0.145022238806452,-0.145005590256122,
-0.144989208963482,-0.144973088953973,-0.143073896434872,-0.13890559370743,
-0.132998811702847,-0.114716118291897,-0.109835420218483),.UNSPECIFIED.);
#777=B_SPLINE_CURVE_WITH_KNOTS('',3,(#69907,#69908,#69909,#69910,#69911,
#69912,#69913,#69914,#69915),.UNSPECIFIED.,.F.,.F.,(4,1,1,1,1,1,4),(59.690260418206,
60.2097426832351,61.2072492651971,62.2047558471591,63.2022624291211,64.1997690110831,
65.1147889235391),.UNSPECIFIED.);
#778=B_SPLINE_CURVE_WITH_KNOTS('',3,(#69916,#69917,#69918,#69919,#69920,
#69921,#69922,#69923,#69924,#69925,#69926,#69927,#69928,#69929,#69930,#69931,
#69932,#69933,#69934,#69935,#69936,#69937,#69938,#69939,#69940,#69941),
 .UNSPECIFIED.,.F.,.F.,(4,2,2,2,2,2,2,2,2,2,2,2,4),(-1.60461039696953,-1.60200406463946,
-1.59780060604424,-1.57558491424115,-1.55491332420186,-1.54748189968155,
-1.54508526809245,-1.54351756503159,-1.54190967647936,-1.53932531048012,
-1.53085774882649,-1.50084484460034,-1.49507327327653),.UNSPECIFIED.);
#779=B_SPLINE_CURVE_WITH_KNOTS('',3,(#69943,#69944,#69945,#69946,#69947,
#69948,#69949,#69950,#69951,#69952,#69953,#69954,#69955,#69956,#69957,#69958,
#69959,#69960,#69961,#69962,#69963,#69964,#69965,#69966,#69967,#69968,#69969,
#69970,#69971,#69972,#69973,#69974,#69975,#69976),.UNSPECIFIED.,.F.,.F.,
(4,2,2,2,2,2,2,2,2,2,2,2,2,2,2,2,4),(-0.109835420218483,-0.0924745669060319,
-0.0872107663617741,-0.0838901580985834,-0.0812343057745877,-0.0781924148245023,
-0.0750033992623017,-0.061516621270222,-0.0474361001445638,-0.0299384713519545,
-0.0225781465623608,-0.0201139955418309,-0.0186887094877936,-0.0172787991718988,
-0.0157260016506987,-0.0135557476351094,-0.000374706389804315),
 .UNSPECIFIED.);
#780=B_SPLINE_CURVE_WITH_KNOTS('',3,(#69977,#69978,#69979,#69980,#69981,
#69982,#69983,#69984,#69985,#69986,#69987,#69988,#69989,#69990,#69991,#69992,
#69993,#69994,#69995,#69996,#69997,#69998,#69999,#70000,#70001,#70002,#70003,
#70004,#70005,#70006,#70007,#70008,#70009,#70010,#70011,#70012,#70013,#70014,
#70015,#70016,#70017,#70018,#70019,#70020,#70021,#70022,#70023,#70024,#70025,
#70026,#70027,#70028,#70029,#70030,#70031,#70032,#70033,#70034,#70035,#70036,
#70037,#70038,#70039,#70040,#70041,#70042,#70043,#70044,#70045,#70046,#70047,
#70048,#70049,#70050,#70051,#70052,#70053,#70054,#70055,#70056,#70057,#70058,
#70059,#70060,#70061,#70062,#70063,#70064,#70065,#70066,#70067,#70068,#70069,
#70070,#70071,#70072,#70073,#70074,#70075,#70076,#70077,#70078,#70079,#70080,
#70081,#70082,#70083,#70084,#70085,#70086,#70087,#70088,#70089,#70090,#70091,
#70092,#70093,#70094,#70095,#70096,#70097,#70098,#70099,#70100,#70101,#70102,
#70103,#70104,#70105,#70106,#70107,#70108,#70109,#70110,#70111,#70112,#70113,
#70114,#70115,#70116,#70117,#70118,#70119,#70120,#70121,#70122,#70123,#70124,
#70125,#70126,#70127,#70128,#70129,#70130,#70131,#70132,#70133,#70134,#70135,
#70136,#70137,#70138,#70139,#70140,#70141,#70142,#70143,#70144),
 .UNSPECIFIED.,.F.,.F.,(4,2,2,2,2,2,2,2,2,2,2,2,2,2,2,2,2,2,2,2,2,2,2,2,
2,2,2,2,2,2,2,2,2,2,2,2,2,2,2,2,2,2,2,2,2,2,2,2,2,2,2,2,2,2,2,2,2,2,2,2,
2,2,2,2,2,2,2,2,2,2,2,2,2,2,2,2,2,2,2,2,2,2,2,4),(-1.60478364820448,-1.57115448853031,
-1.56635300154545,-1.56321387126241,-1.56020659854018,-1.5575477017934,
-1.55417855953096,-1.54874276073197,-1.51825690335156,-1.5062124376139,
-1.50154189002089,-1.49902450528996,-1.4969785366282,-1.49550094237346,
-1.49408266666979,-1.4916529469648,-1.48457165850096,-1.45311605841662,
-1.43925390729897,-1.43499091462708,-1.43218068451344,-1.42948235261338,
-1.42565685690423,-1.41637553110808,-1.38953899675086,-1.37455458675071,
-1.37082748447105,-1.36898112650074,-1.36763485471576,-1.36580697276272,
-1.36217406317925,-1.33785388788463,-1.31342209163813,-1.30840985105733,
-1.30544298884162,-1.30277673980584,-1.29933828806008,-1.29365777363457,
-1.26048375949418,-1.24581753131842,-1.24292066522155,-1.24124532974193,
-1.23971798647798,-1.23753123862588,-1.23215100308795,-1.20835597851232,
-1.1931707862611,-1.18352613860254,-1.17974369018884,-1.17702561955487,
-1.17419654673821,-1.16984309552342,-1.15622264911892,-1.12860700237905,
-1.1180834423465,-1.1154096542646,-1.11378261507004,-1.11224801931406,-1.10993826485808,
-1.10373299486374,-1.08063609601986,-1.06571065011332,-1.05921431399649,
-1.05396209768192,-1.05094464888596,-1.04828655012033,-1.04493161547065,
-1.03954686131757,-1.00898348915641,-0.996918994379538,-0.990051595207271,
-0.987720418930485,-0.986166194615606,-0.984740923599546,-0.982275776062266,
-0.9749031956904,-0.952741745009379,-0.938177046670485,-0.92878641440501,
-0.925039659073643,-0.922327497260759,-0.919825768727951,-0.915718712436704,
-0.912212879656785),.UNSPECIFIED.);
#781=B_SPLINE_CURVE_WITH_KNOTS('',3,(#70150,#70151,#70152,#70153,#70154,
#70155,#70156,#70157,#70158,#70159,#70160,#70161,#70162,#70163,#70164,#70165,
#70166,#70167,#70168,#70169,#70170,#70171,#70172,#70173,#70174,#70175,#70176,
#70177,#70178,#70179,#70180,#70181,#70182,#70183,#70184,#70185,#70186,#70187,
#70188,#70189,#70190,#70191,#70192,#70193,#70194,#70195,#70196,#70197,#70198,
#70199,#70200,#70201,#70202,#70203,#70204,#70205,#70206,#70207,#70208,#70209,
#70210,#70211,#70212,#70213,#70214,#70215,#70216,#70217,#70218,#70219,#70220,
#70221,#70222,#70223,#70224,#70225,#70226,#70227,#70228,#70229,#70230,#70231,
#70232,#70233,#70234,#70235,#70236,#70237,#70238,#70239,#70240,#70241,#70242,
#70243,#70244,#70245,#70246,#70247,#70248,#70249,#70250,#70251,#70252,#70253,
#70254,#70255,#70256,#70257,#70258,#70259,#70260,#70261,#70262,#70263,#70264,
#70265,#70266,#70267,#70268,#70269,#70270,#70271,#70272,#70273,#70274,#70275,
#70276,#70277,#70278,#70279,#70280,#70281,#70282,#70283,#70284,#70285,#70286,
#70287,#70288,#70289,#70290,#70291,#70292,#70293,#70294,#70295,#70296,#70297),
 .UNSPECIFIED.,.F.,.F.,(4,3,3,3,3,3,3,3,3,3,3,3,3,3,3,3,3,3,3,3,3,3,3,3,
3,3,3,3,3,3,3,3,3,3,3,3,3,3,3,3,3,3,3,3,3,3,3,3,3,4),(65.9734457253856,
66.133557022025,66.1947821750071,66.3122857663604,66.4295731536894,66.546741452997,
66.6638406433999,66.7809205913324,66.8981149294539,67.0153723379108,67.1328487102704,
67.1922887569691,67.3097923483223,67.4270797356512,67.5442480349588,67.6613472253615,
67.778427173294,67.8956215114154,68.0128789198722,68.1303552922317,68.189795338931,
68.3072989302843,68.4245863176133,68.5417546169209,68.6588538073237,68.7759337552562,
68.8931280933777,69.0103855018346,69.1278618741942,69.187301920893,69.3048055122463,
69.4220928995753,69.5392611988829,69.6563603892858,69.7734403372183,69.8906346753398,
70.0078920837967,70.1253684561562,70.184808502855,70.3023120942082,70.4195994815371,
70.5367677808447,70.6538669712475,70.77094691918,70.8881412573014,71.0053986657582,
71.1228750381177,71.182315084817,71.2997780450628,71.3990564536364),
 .UNSPECIFIED.);
#782=B_SPLINE_CURVE_WITH_KNOTS('',3,(#70298,#70299,#70300,#70301,#70302),
 .UNSPECIFIED.,.F.,.F.,(4,1,4),(65.1147889235391,65.1972755930451,65.9734445059395),
 .UNSPECIFIED.);
#783=B_SPLINE_CURVE_WITH_KNOTS('',3,(#70303,#70304,#70305,#70306,#70307,
#70308,#70309,#70310,#70311,#70312,#70313,#70314,#70315,#70316,#70317,#70318,
#70319,#70320,#70321,#70322,#70323,#70324,#70325,#70326,#70327,#70328,#70329,
#70330,#70331,#70332,#70333,#70334,#70335,#70336,#70337,#70338,#70339,#70340,
#70341,#70342,#70343,#70344,#70345,#70346,#70347,#70348,#70349,#70350,#70351,
#70352,#70353,#70354,#70355,#70356,#70357,#70358,#70359,#70360,#70361,#70362,
#70363,#70364,#70365,#70366,#70367,#70368,#70369,#70370,#70371,#70372,#70373,
#70374,#70375,#70376,#70377,#70378,#70379,#70380,#70381,#70382,#70383,#70384,
#70385,#70386,#70387,#70388,#70389,#70390,#70391,#70392,#70393,#70394,#70395,
#70396,#70397,#70398,#70399,#70400,#70401,#70402,#70403,#70404,#70405,#70406,
#70407,#70408,#70409,#70410,#70411,#70412,#70413,#70414,#70415,#70416,#70417,
#70418,#70419,#70420,#70421,#70422,#70423,#70424,#70425,#70426,#70427,#70428,
#70429,#70430,#70431,#70432,#70433,#70434,#70435,#70436,#70437,#70438,#70439,
#70440,#70441,#70442,#70443,#70444,#70445,#70446,#70447,#70448,#70449,#70450,
#70451,#70452,#70453,#70454,#70455,#70456,#70457,#70458,#70459,#70460,#70461,
#70462,#70463,#70464,#70465,#70466,#70467,#70468,#70469,#70470,#70471,#70472,
#70473,#70474,#70475,#70476,#70477,#70478,#70479,#70480,#70481,#70482,#70483,
#70484,#70485,#70486,#70487,#70488,#70489,#70490,#70491,#70492,#70493,#70494,
#70495,#70496,#70497,#70498,#70499,#70500,#70501,#70502,#70503,#70504,#70505,
#70506,#70507,#70508,#70509,#70510,#70511,#70512,#70513,#70514,#70515,#70516),
 .UNSPECIFIED.,.F.,.F.,(4,2,2,2,2,2,2,2,2,2,2,2,2,2,2,2,2,2,2,2,2,2,2,2,
2,2,2,2,2,2,2,2,2,2,2,2,2,2,2,2,2,2,2,2,2,2,2,2,2,2,2,2,2,2,2,2,2,2,2,2,
2,2,2,2,2,2,2,2,2,2,2,2,2,2,2,2,2,2,2,2,2,2,2,2,2,2,2,2,2,2,2,2,2,2,2,2,
2,2,2,2,2,2,2,2,2,2,4),(-0.912212879656785,-0.904371023607735,-0.874306003962147,
-0.863460301095778,-0.860763645895146,-0.859131476399047,-0.857599657718553,
-0.855677862819302,-0.850732756831442,-0.81681297279783,-0.802644312257033,
-0.798352856704789,-0.795536211207104,-0.792809628977875,-0.788981056755466,
-0.77900505257007,-0.762980505090563,-0.737558646023001,-0.734067190034405,
-0.732245167146209,-0.73089814192859,-0.729044322108487,-0.725280651839922,
-0.70997001926422,-0.682171892283217,-0.673899944774947,-0.670586203926304,
-0.668113286334403,-0.6653747036933,-0.661480597784054,-0.651009109632286,
-0.633656527188981,-0.610502002417735,-0.606789446568505,-0.60494556068299,
-0.603449632879506,-0.601540053871971,-0.597482183921184,-0.59183827278793,
-0.575073595157904,-0.550799656332624,-0.545560952547799,-0.542247835313155,
-0.539592858237777,-0.536546390060784,-0.531155599761763,-0.524433982851252,
-0.508624802674593,-0.482798063832198,-0.479351863405705,-0.47753936378189,
-0.47605587827031,-0.474116912829285,-0.469898755145193,-0.463951470801384,
-0.445421494855018,-0.423541019803515,-0.418257253800974,-0.414930997133296,
-0.412274861624346,-0.409237239261976,-0.403889774184179,-0.397238729715074,
-0.374475878611681,-0.373538116545626,-0.354661842154876,-0.351675452247035,
-0.34996339990879,-0.348448161193592,-0.346340641175164,-0.341114116742738,
-0.333103969458632,-0.315874414649614,-0.294292184712198,-0.289493868571186,
-0.286571105885082,-0.283892023278006,-0.280360677471308,-0.272371971044671,
-0.260912639243567,-0.246179196378392,-0.227321233872595,-0.224335396498194,
-0.22262343337322,-0.221108102011787,-0.219000219591661,-0.213771625021999,
-0.205757062073263,-0.18861438593341,-0.166965720783982,-0.162159427933233,
-0.159234922758008,-0.156556243405086,-0.156505138420624,-0.156459189880959,
-0.156417850125568,-0.156380634240671,-0.156347112193308,-0.156316902003047,
-0.156289663828868,-0.156265094916364,-0.156201398460163,-0.152846107066361,
-0.144582070318634,-0.132469209821949,-0.118242870080311,-0.110044856416793),
 .UNSPECIFIED.);
#784=B_SPLINE_CURVE_WITH_KNOTS('',3,(#70522,#70523,#70524,#70525,#70526,
#70527,#70528,#70529,#70530,#70531,#70532,#70533,#70534,#70535,#70536,#70537,
#70538,#70539,#70540,#70541,#70542,#70543,#70544,#70545,#70546,#70547,#70548,
#70549,#70550,#70551,#70552,#70553,#70554,#70555,#70556,#70557,#70558,#70559,
#70560,#70561,#70562,#70563,#70564,#70565,#70566,#70567,#70568,#70569,#70570,
#70571,#70572,#70573,#70574,#70575,#70576,#70577,#70578,#70579,#70580,#70581,
#70582,#70583,#70584,#70585,#70586,#70587,#70588,#70589,#70590,#70591,#70592,
#70593,#70594,#70595,#70596,#70597,#70598,#70599,#70600,#70601,#70602,#70603,
#70604,#70605,#70606,#70607,#70608,#70609,#70610,#70611,#70612,#70613,#70614,
#70615,#70616,#70617,#70618,#70619,#70620,#70621,#70622,#70623,#70624,#70625,
#70626,#70627,#70628,#70629,#70630,#70631,#70632,#70633,#70634,#70635,#70636,
#70637,#70638,#70639,#70640,#70641,#70642,#70643,#70644,#70645,#70646,#70647,
#70648,#70649,#70650,#70651,#70652,#70653,#70654,#70655,#70656,#70657,#70658,
#70659,#70660,#70661,#70662,#70663,#70664,#70665,#70666,#70667,#70668,#70669,
#70670,#70671,#70672,#70673,#70674,#70675,#70676,#70677,#70678,#70679,#70680,
#70681,#70682,#70683,#70684,#70685,#70686,#70687,#70688,#70689,#70690,#70691,
#70692,#70693,#70694,#70695,#70696,#70697,#70698,#70699,#70700,#70701,#70702,
#70703,#70704,#70705,#70706,#70707,#70708,#70709,#70710,#70711,#70712,#70713),
 .UNSPECIFIED.,.F.,.F.,(4,2,2,2,2,2,2,2,2,2,2,2,2,2,2,2,2,2,2,2,2,2,2,2,
2,2,2,2,2,2,2,2,2,2,2,2,2,2,2,2,2,2,2,2,2,2,2,2,2,2,2,2,2,2,2,2,2,2,2,2,
2,2,2,2,2,2,2,2,2,2,2,2,2,2,2,2,2,2,2,2,2,2,2,2,2,2,2,2,2,2,2,2,2,2,2,4),
(-0.69301358421698,-0.692651839720984,-0.689997439699259,-0.68694559874889,
-0.681528636664272,-0.674764223940749,-0.658780911705467,-0.633293456051878,
-0.629810067409437,-0.627989707350097,-0.626642519687764,-0.624786662532745,
-0.621012692447938,-0.605607129871799,-0.577522375407419,-0.56953077172595,
-0.566262071179798,-0.563553257195185,-0.560755589122205,-0.55655815072856,
-0.543401469059281,-0.516228515719477,-0.504734770090803,-0.501919654233641,
-0.500261671577866,-0.49872574929122,-0.496492062971919,-0.490390835768222,
-0.480343646828524,-0.445788418525292,-0.440472968659646,-0.437411809619531,
-0.434758236749855,-0.431465325104831,-0.42482799887066,-0.396265834611555,
-0.377728404492275,-0.374717728866283,-0.373017625702815,-0.371498731206136,
-0.369366539035901,-0.363977739667874,-0.359420975068708,-0.339922934576411,
-0.319206360071356,-0.313970189202,-0.310657650025399,-0.308002484140076,
-0.304955068711174,-0.299560535638158,-0.292832920138985,-0.276999533907002,
-0.251226283849575,-0.247774474934284,-0.245960688112422,-0.244477141256913,
-0.242539318569282,-0.23832804645846,-0.232393990958186,-0.21394425479506,
-0.191950651278511,-0.186675840411542,-0.183352016030964,-0.180695844430751,
-0.177656015967709,-0.172298729586701,-0.168678963246298,-0.162811409843366,
-0.14060334161294,-0.123121664605095,-0.120122388135064,-0.118407363266069,
-0.1169410962558,-0.116912876081689,-0.116885059993081,-0.116857609770681,
-0.116830489399522,-0.11680366485246,-0.116777103751712,-0.116750775342384,
-0.116724650321081,-0.116698700532801,-0.116672898932253,-0.116647219376421,
-0.114611867096337,-0.112104789323589,-0.107463970549589,-0.0955484402159176,
-0.0655653205561749,-0.0592040382829809,-0.055922620910389,-0.0532693913354477,
-0.0501987205217863,-0.0446919243745535,-0.0377807281459007,-0.000375412795531045),
 .UNSPECIFIED.);
#785=B_SPLINE_CURVE_WITH_KNOTS('',3,(#70714,#70715,#70716,#70717,#70718,
#70719,#70720,#70721,#70722,#70723,#70724,#70725,#70726,#70727,#70728,#70729,
#70730,#70731,#70732,#70733,#70734,#70735,#70736,#70737,#70738),
 .UNSPECIFIED.,.F.,.F.,(4,3,3,3,3,3,3,3,4),(71.3990564536364,71.5162398299033,
71.6333464109936,71.750426076489,71.8676146843092,71.9848594751022,72.1023289823989,
72.179821666779,72.2566310325652),.UNSPECIFIED.);
#786=B_SPLINE_CURVE_WITH_KNOTS('',3,(#70740,#70741,#70742,#70743,#70744,
#70745,#70746,#70747,#70748,#70749,#70750,#70751,#70752,#70753,#70754,#70755,
#70756,#70757,#70758,#70759,#70760,#70761,#70762,#70763,#70764,#70765,#70766,
#70767,#70768,#70769,#70770,#70771,#70772,#70773),.UNSPECIFIED.,.F.,.F.,
(4,2,2,2,2,2,2,2,2,2,2,2,2,2,2,2,4),(-0.110044856416793,-0.0999516129579047,
-0.0969458658991607,-0.0952467203932099,-0.0937273466900666,-0.0922007675905067,
-0.088597535396166,-0.0812378620567708,-0.060149807966156,-0.0395065387801758,
-0.0347576557653405,-0.0318451886373184,-0.0291626819211827,-0.0265368828350931,
-0.0230751872387385,-0.0156249266252038,-0.000374946432257026),
 .UNSPECIFIED.);
#787=B_SPLINE_CURVE_WITH_KNOTS('',3,(#70774,#70775,#70776,#70777,#70778,
#70779,#70780,#70781,#70782,#70783),.UNSPECIFIED.,.F.,.F.,(4,1,1,1,1,1,
1,4),(72.256633207435,72.5146276293805,73.5121342113425,74.5096407933045,
75.5071473752665,76.5046539572285,77.5021605391904,77.6824992212595),
 .UNSPECIFIED.);
#788=B_SPLINE_CURVE_WITH_KNOTS('',3,(#70788,#70789,#70790,#70791,#70792,
#70793,#70794,#70795,#70796,#70797,#70798,#70799,#70800,#70801,#70802,#70803,
#70804,#70805,#70806,#70807,#70808,#70809,#70810,#70811,#70812,#70813,#70814,
#70815,#70816,#70817,#70818,#70819,#70820,#70821,#70822,#70823,#70824,#70825,
#70826,#70827,#70828,#70829,#70830,#70831,#70832,#70833,#70834,#70835,#70836,
#70837,#70838,#70839,#70840,#70841,#70842,#70843,#70844,#70845,#70846,#70847,
#70848,#70849,#70850,#70851,#70852,#70853,#70854,#70855,#70856,#70857,#70858,
#70859,#70860,#70861,#70862,#70863,#70864,#70865,#70866,#70867,#70868,#70869,
#70870,#70871,#70872,#70873,#70874,#70875,#70876,#70877,#70878,#70879,#70880,
#70881,#70882,#70883,#70884,#70885,#70886,#70887,#70888,#70889,#70890,#70891,
#70892,#70893,#70894,#70895,#70896,#70897,#70898,#70899,#70900,#70901,#70902,
#70903,#70904,#70905,#70906,#70907,#70908,#70909,#70910,#70911,#70912,#70913,
#70914,#70915,#70916,#70917,#70918,#70919,#70920,#70921,#70922,#70923,#70924,
#70925,#70926,#70927,#70928,#70929,#70930,#70931,#70932,#70933,#70934,#70935,
#70936,#70937,#70938,#70939,#70940,#70941,#70942,#70943,#70944,#70945,#70946,
#70947,#70948,#70949,#70950,#70951,#70952,#70953,#70954,#70955,#70956,#70957,
#70958,#70959,#70960,#70961,#70962,#70963,#70964,#70965,#70966,#70967,#70968,
#70969,#70970,#70971,#70972,#70973,#70974,#70975,#70976,#70977,#70978,#70979,
#70980,#70981,#70982,#70983,#70984,#70985,#70986,#70987,#70988,#70989,#70990,
#70991,#70992,#70993,#70994,#70995,#70996,#70997),.UNSPECIFIED.,.F.,.F.,
(4,2,2,2,2,2,2,2,2,2,2,2,2,2,2,2,2,2,2,2,2,2,2,2,2,2,2,2,2,2,2,2,2,2,2,
2,2,2,2,2,2,2,2,2,2,2,2,2,2,2,2,2,2,2,2,2,2,2,2,2,2,2,2,2,2,2,2,2,2,2,2,
2,2,2,2,2,2,2,2,2,2,2,2,2,2,2,2,2,2,2,2,2,2,2,2,2,2,2,2,2,2,2,2,2,4),(-1.49489110793716,
-1.48851040879273,-1.4815898616485,-1.46911976787942,-1.46330136573139,
-1.45975864243683,-1.45653421167254,-1.45643215106401,-1.45631773706341,
-1.45626507241238,-1.4561656573116,-1.45597971139256,-1.45422673620739,
-1.45130121023412,-1.4464882301232,-1.42476291827683,-1.40462053524107,
-1.39998137273359,-1.39452557009446,-1.3923834918489,-1.39086324111583,
-1.38916804628255,-1.38617973320417,-1.36999707459897,-1.3474561383648,
-1.33465279488333,-1.33049113140621,-1.32770080481675,-1.32498678840093,
-1.32107757767587,-1.31121166510398,-1.2849274715219,-1.2701344794187,-1.26642823951693,
-1.26458562220613,-1.26308967815517,-1.26117870018267,-1.25711307255161,
-1.23198765055204,-1.21635515041228,-1.20967825166179,-1.20431433655919,
-1.20127347739827,-1.19861792781786,-1.1952968919721,-1.19003061365599,
-1.16891656839967,-1.14974347581927,-1.14522828139264,-1.13987431459827,
-1.13774747125555,-1.13622952878083,-1.13452714947313,-1.13150539284095,
-1.11261184818741,-1.09780820284829,-1.08645208681706,-1.07851331677216,
-1.07499059162102,-1.07231295798725,-1.06938677477583,-1.06457109503359,
-1.04282597521714,-1.02270129219182,-1.01806423800433,-1.01261008017155,
-1.01046818500423,-1.00894790785714,-1.00725250510562,-1.00426344994474,
-0.988031737189969,-0.965526664071109,-0.952732955666407,-0.948572140588679,
-0.945781892831736,-0.943067587007926,-0.939157306054541,-0.929283382176771,
-0.903004796771474,-0.892066615130021,-0.885616074874488,-0.883336533471173,
-0.881792225656302,-0.880150375395943,-0.877409292505431,-0.867133189761485,
-0.838886489321326,-0.825531915485326,-0.821315606433368,-0.818514221513337,
-0.815808310668869,-0.8119440112042,-0.802457429459729,-0.787203173805783,
-0.763230843010317,-0.758031460640131,-0.756082502699792,-0.754682122929671,
-0.753099385250855,-0.750630871632608,-0.742516188656957,-0.726556737874347,
-0.701170071687919,-0.695957382235664,-0.69301358421698),.UNSPECIFIED.);
#789=B_SPLINE_CURVE_WITH_KNOTS('',3,(#70999,#71000,#71001,#71002,#71003),
 .UNSPECIFIED.,.F.,.F.,(4,1,4),(77.6824992212595,78.4996671211524,78.5398163397448),
 .UNSPECIFIED.);
#790=B_SPLINE_CURVE_WITH_KNOTS('',3,(#71004,#71005,#71006,#71007,#71008,
#71009,#71010,#71011,#71012,#71013,#71014,#71015,#71016,#71017,#71018,#71019,
#71020,#71021,#71022,#71023,#71024,#71025,#71026,#71027,#71028,#71029,#71030,
#71031,#71032,#71033,#71034,#71035,#71036,#71037,#71038,#71039,#71040,#71041,
#71042,#71043,#71044,#71045,#71046,#71047,#71048,#71049,#71050,#71051,#71052,
#71053,#71054,#71055,#71056,#71057,#71058,#71059,#71060,#71061,#71062,#71063,
#71064,#71065,#71066,#71067,#71068,#71069,#71070,#71071,#71072,#71073,#71074,
#71075,#71076,#71077,#71078,#71079,#71080,#71081,#71082,#71083,#71084,#71085,
#71086,#71087,#71088,#71089,#71090,#71091,#71092,#71093,#71094,#71095,#71096,
#71097,#71098,#71099,#71100,#71101,#71102,#71103,#71104,#71105,#71106,#71107,
#71108,#71109,#71110,#71111,#71112,#71113,#71114,#71115,#71116,#71117,#71118,
#71119,#71120,#71121,#71122,#71123,#71124,#71125,#71126,#71127,#71128,#71129,
#71130,#71131,#71132,#71133,#71134,#71135,#71136,#71137,#71138,#71139,#71140,
#71141,#71142,#71143,#71144,#71145,#71146,#71147,#71148,#71149,#71150,#71151,
#71152,#71153,#71154,#71155,#71156,#71157,#71158,#71159,#71160,#71161,#71162,
#71163,#71164,#71165,#71166,#71167,#71168,#71169,#71170,#71171,#71172,#71173,
#71174,#71175,#71176,#71177,#71178,#71179,#71180,#71181,#71182,#71183,#71184,
#71185,#71186,#71187,#71188,#71189,#71190,#71191,#71192,#71193,#71194,#71195,
#71196,#71197,#71198,#71199,#71200,#71201,#71202,#71203,#71204,#71205,#71206,
#71207,#71208,#71209,#71210,#71211,#71212,#71213,#71214,#71215,#71216,#71217,
#71218,#71219,#71220,#71221,#71222,#71223,#71224,#71225,#71226,#71227,#71228,
#71229),.UNSPECIFIED.,.F.,.F.,(4,2,2,2,2,2,2,2,2,2,2,2,2,2,2,2,2,2,2,2,
2,2,2,2,2,2,2,2,2,2,2,2,2,2,2,2,2,2,2,2,2,2,2,2,2,2,2,2,2,2,2,2,2,2,2,2,
2,2,2,2,2,2,2,2,2,2,2,2,2,2,2,2,2,2,2,2,2,2,2,2,2,2,2,2,2,2,2,2,2,2,2,2,
2,2,2,2,2,2,2,2,2,2,2,2,2,2,2,2,2,2,2,2,4),(-1.6048292035244,-1.59977016780302,
-1.58369609630493,-1.56532874704923,-1.55717465345672,-1.55093370317585,
-1.54771677533232,-1.54532523492503,-1.54230190317608,-1.53715853994253,
-1.52985404874484,-1.50360614078768,-1.48882453445654,-1.48618944707944,
-1.48404047097112,-1.48400618512232,-1.48397210208206,-1.48393818271339,
-1.48390438758405,-1.48387067670807,-1.48383700946711,-1.48380334434472,
-1.48376963865202,-1.48373584836451,-1.48370192782456,-1.48366782941582,
-1.48363350321742,-1.48359889658574,-1.4835639537953,-1.48352861554711,
-1.48351226427847,-1.48349456571752,-1.48347534461706,-1.483454392456,-1.48343145888499,
-1.48340624008951,-1.48337836303173,-1.4833473637114,-1.48331265593475,
-1.48327348604044,-1.483228864582,-1.48178632787584,-1.47987800423348,-1.47607785317775,
-1.45861624182952,-1.4435051744279,-1.43232140124349,-1.42858586549684,
-1.42310130926748,-1.42003563270498,-1.41738262651398,-1.4140962314904,
-1.40894915091509,-1.38183228838697,-1.36701262699752,-1.36173867674794,
-1.35788130004178,-1.35600947324365,-1.35451414372993,-1.352634498102,-1.34873605710163,
-1.32868801370663,-1.31767133521675,-1.30560431244284,-1.29732319936252,
-1.29374462308699,-1.29105909868377,-1.28815749128966,-1.28345866517345,
-1.27504977123215,-1.24890771844801,-1.23416232697371,-1.23046119416122,
-1.22861950041388,-1.227272955156,-1.22543929882858,-1.22177914054929,-1.19789922684563,
-1.18100947473718,-1.17070589808303,-1.16683355125372,-1.16409883109408,
-1.16162183084412,-1.15765727761269,-1.14739249045719,-1.11711709508438,
-1.10906575684174,-1.10382104466066,-1.10171070130384,-1.10019507853645,
-1.09848443107537,-1.09550434949171,-1.07682833895893,-1.06241912056978,
-1.05068395189443,-1.04256076877221,-1.03900746110207,-1.03632533882571,
-1.03341243455468,-1.02866090998084,-1.00793103249446,-0.986884379719522,
-0.982134528404293,-0.976588426122863,-0.97443276454899,-0.972910167875554,
-0.971220686528546,-0.968259849336341,-0.953297302979803,-0.929783491563662,
-0.916717145604933,-0.912528510920155,-0.912282028493777),.UNSPECIFIED.);
#791=B_SPLINE_CURVE_WITH_KNOTS('',3,(#71235,#71236,#71237,#71238,#71239,
#71240,#71241,#71242,#71243,#71244,#71245,#71246,#71247,#71248,#71249,#71250,
#71251,#71252,#71253,#71254,#71255,#71256,#71257,#71258,#71259,#71260,#71261,
#71262,#71263,#71264,#71265,#71266,#71267,#71268,#71269,#71270,#71271,#71272,
#71273,#71274,#71275,#71276,#71277,#71278,#71279,#71280,#71281,#71282,#71283,
#71284,#71285,#71286,#71287,#71288,#71289,#71290,#71291,#71292,#71293,#71294,
#71295,#71296,#71297,#71298,#71299,#71300,#71301,#71302,#71303,#71304,#71305,
#71306,#71307,#71308,#71309,#71310,#71311,#71312,#71313,#71314,#71315,#71316,
#71317,#71318,#71319,#71320,#71321,#71322,#71323,#71324,#71325,#71326,#71327,
#71328,#71329,#71330,#71331,#71332,#71333,#71334,#71335,#71336,#71337,#71338,
#71339,#71340,#71341,#71342,#71343,#71344,#71345,#71346,#71347,#71348,#71349,
#71350,#71351,#71352,#71353,#71354,#71355,#71356,#71357,#71358,#71359,#71360,
#71361,#71362,#71363,#71364,#71365,#71366,#71367,#71368,#71369,#71370,#71371,
#71372,#71373,#71374,#71375,#71376,#71377,#71378,#71379,#71380,#71381,#71382,
#71383,#71384,#71385,#71386,#71387,#71388,#71389,#71390,#71391,#71392,#71393,
#71394,#71395,#71396,#71397,#71398,#71399,#71400,#71401,#71402,#71403,#71404,
#71405,#71406,#71407,#71408,#71409,#71410,#71411,#71412),.UNSPECIFIED.,
 .F.,.F.,(4,2,2,2,2,2,2,2,2,2,2,2,2,2,2,2,2,2,2,2,2,2,2,2,2,2,2,2,2,2,2,
2,2,2,2,2,2,2,2,2,2,2,2,2,2,2,2,2,2,2,2,2,2,2,2,2,2,2,2,2,2,2,2,2,2,2,2,
2,2,2,2,2,2,2,2,2,2,2,2,2,2,2,2,2,2,2,2,2,4),(-0.693006869784502,-0.683654895915191,
-0.680632241890465,-0.67892916620703,-0.677410422659474,-0.675282285877349,
-0.669923812895553,-0.665404567543853,-0.646201277630175,-0.625122720119772,
-0.619867266461999,-0.616548442518697,-0.613891862921112,-0.61084677504362,
-0.605467160615383,-0.584062758715741,-0.560645558149656,-0.554787517645369,
-0.552523173264645,-0.550996404234677,-0.5493531378566,-0.546608003167671,
-0.535028882294789,-0.499892492568089,-0.492685423233125,-0.489287528570774,
-0.48662397875073,-0.483630296632608,-0.478497087801861,-0.475078931304347,
-0.465150603687295,-0.448547445733901,-0.430313633403777,-0.426425137698383,
-0.424546883634213,-0.423050892590864,-0.421175971196141,-0.417304964550807,
-0.412007668153858,-0.397072685306411,-0.370166859036,-0.365008821866856,
-0.361718427598524,-0.359064063480933,-0.355998869004036,-0.350520929986073,
-0.346791624930591,-0.335633632963646,-0.320476656624734,-0.301529826584575,
-0.298505458805393,-0.296802076892572,-0.295283547217215,-0.293156376862039,
-0.287803803991192,-0.28329158080209,-0.264140945808024,-0.241107310771599,
-0.236327661557132,-0.233408254661632,-0.230727056925715,-0.227185217835719,
-0.219136639401312,-0.207555124624643,-0.192947515188004,-0.174163353272465,
-0.171144582805802,-0.169442370902138,-0.167923417592538,-0.165793643794449,
-0.160424045492456,-0.155891272854231,-0.136583959723365,-0.11372975454215,
-0.108960302987224,-0.106042996823378,-0.103477221228301,-0.100170748419366,
-0.0930081796813826,-0.0830831313090248,-0.0664776508816948,-0.0482386868303266,
-0.0443500357766238,-0.0424717165716612,-0.0409756787534045,-0.0391007051399124,
-0.037036502167314,-0.0335716462315504,-0.000375349248106819),
 .UNSPECIFIED.);
#792=B_SPLINE_CURVE_WITH_KNOTS('',3,(#71413,#71414,#71415,#71416,#71417,
#71418,#71419,#71420,#71421,#71422,#71423,#71424,#71425,#71426,#71427,#71428,
#71429,#71430,#71431,#71432,#71433,#71434,#71435,#71436,#71437,#71438,#71439,
#71440,#71441,#71442,#71443,#71444),.UNSPECIFIED.,.F.,.F.,(4,2,2,2,2,2,
2,2,2,2,2,2,2,2,2,4),(-1.604518044356,-1.59482654117459,-1.58877374327812,
-1.58575879969892,-1.58325763982483,-1.58060476826667,-1.57731770622977,
-1.57092568823115,-1.54959306788281,-1.52432379448028,-1.52103104075161,
-1.51918967991357,-1.51784327588204,-1.51600961624893,-1.51234881403237,
-1.49489110793716),.UNSPECIFIED.);
#793=B_SPLINE_CURVE_WITH_KNOTS('',3,(#71445,#71446,#71447,#71448,#71449,
#71450,#71451,#71452,#71453,#71454,#71455,#71456,#71457,#71458,#71459,#71460,
#71461,#71462,#71463,#71464,#71465,#71466,#71467,#71468,#71469,#71470,#71471,
#71472,#71473,#71474,#71475,#71476,#71477,#71478,#71479,#71480,#71481,#71482,
#71483,#71484,#71485,#71486,#71487,#71488,#71489,#71490,#71491,#71492,#71493,
#71494,#71495,#71496,#71497,#71498,#71499,#71500,#71501,#71502,#71503,#71504,
#71505,#71506,#71507,#71508,#71509,#71510,#71511,#71512,#71513,#71514,#71515,
#71516,#71517,#71518,#71519,#71520,#71521,#71522,#71523,#71524,#71525,#71526,
#71527,#71528,#71529,#71530,#71531,#71532,#71533,#71534,#71535,#71536,#71537,
#71538,#71539,#71540,#71541,#71542,#71543,#71544,#71545,#71546,#71547,#71548,
#71549,#71550,#71551,#71552,#71553,#71554,#71555,#71556,#71557,#71558,#71559,
#71560,#71561,#71562,#71563,#71564,#71565,#71566,#71567,#71568,#71569,#71570,
#71571,#71572,#71573,#71574,#71575,#71576,#71577,#71578,#71579,#71580,#71581,
#71582,#71583,#71584,#71585,#71586,#71587,#71588,#71589,#71590,#71591,#71592,
#71593,#71594,#71595,#71596,#71597,#71598,#71599,#71600,#71601,#71602,#71603,
#71604,#71605,#71606,#71607,#71608,#71609,#71610,#71611,#71612,#71613,#71614,
#71615,#71616,#71617,#71618,#71619,#71620,#71621,#71622,#71623,#71624,#71625,
#71626,#71627,#71628,#71629,#71630,#71631,#71632,#71633,#71634,#71635,#71636,
#71637,#71638,#71639,#71640,#71641,#71642,#71643,#71644,#71645,#71646,#71647,
#71648),.UNSPECIFIED.,.F.,.F.,(4,2,2,2,2,2,2,2,2,2,2,2,2,2,2,2,2,2,2,2,
2,2,2,2,2,2,2,2,2,2,2,2,2,2,2,2,2,2,2,2,2,2,2,2,2,2,2,2,2,2,2,2,2,2,2,2,
2,2,2,2,2,2,2,2,2,2,2,2,2,2,2,2,2,2,2,2,2,2,2,2,2,2,2,2,2,2,2,2,2,2,2,2,
2,2,2,2,2,2,2,2,2,4),(-0.912282028493777,-0.909732451909759,-0.907022044663811,
-0.903134350440392,-0.893467012592433,-0.866991641093441,-0.855997791384227,
-0.849525498317699,-0.847242989102264,-0.845697990491516,-0.844056883709189,
-0.841319784346746,-0.83110537098309,-0.802787555749626,-0.789604516959915,
-0.785298561161931,-0.78247868405242,-0.779753589220489,-0.775934866291146,
-0.766033762026051,-0.750203385085449,-0.724412086452443,-0.720961308019087,
-0.719147750631595,-0.717664220469517,-0.715726249183874,-0.711514104312759,
-0.705578484861349,-0.687121135556323,-0.665127566259059,-0.659851753887868,
-0.656527652725764,-0.65387149951668,-0.650831970491827,-0.645476031024791,
-0.638811386089502,-0.615989702041514,-0.597688900341373,-0.593800441729262,
-0.591922474985267,-0.590426868758181,-0.5885526732148,-0.584684005300306,
-0.579390640141005,-0.564473646400988,-0.537540844470895,-0.532384909793752,
-0.529095565737712,-0.52644189034469,-0.523377334284261,-0.517900164386236,
-0.514171282351249,-0.50301436850133,-0.48785747772316,-0.468909757636497,
-0.465885849437866,-0.464182828917149,-0.462664721096335,-0.460538330203103,
-0.455188804679728,-0.450679891147248,-0.431552868369006,-0.408518642444654,
-0.403724554954122,-0.40080258671598,-0.39812308615128,-0.394589497767307,
-0.386587864175764,-0.375102234407785,-0.360394480624298,-0.341551944608335,
-0.338531707374926,-0.33682944509048,-0.335311045494618,-0.333182920236384,
-0.32782213331912,-0.323299652381592,-0.304069588409059,-0.283019022764621,
-0.277768698271046,-0.274451856078361,-0.271796115757312,-0.268751194295786,
-0.263369764956323,-0.241183609572746,-0.216304108732404,-0.212379121615335,
-0.210460756325435,-0.208929591944377,-0.20729528686359,-0.204590090842878,
-0.1936227821569,-0.162492732686161,-0.152091753769073,-0.148108231108423,
-0.145627727844826,-0.143533168328323,-0.140825610111392,-0.137411158688223,
-0.131919259359916,-0.12053744697573,-0.110043953422301),.UNSPECIFIED.);
#794=B_SPLINE_CURVE_WITH_KNOTS('',3,(#71653,#71654,#71655,#71656,#71657,
#71658,#71659,#71660,#71661,#71662,#71663,#71664,#71665,#71666,#71667,#71668,
#71669,#71670,#71671,#71672,#71673,#71674,#71675,#71676,#71677,#71678,#71679,
#71680,#71681,#71682,#71683,#71684,#71685,#71686,#71687,#71688,#71689,#71690,
#71691,#71692,#71693,#71694,#71695,#71696,#71697,#71698,#71699,#71700,#71701,
#71702,#71703,#71704,#71705,#71706,#71707,#71708,#71709,#71710,#71711,#71712,
#71713,#71714,#71715,#71716,#71717,#71718,#71719,#71720,#71721,#71722,#71723,
#71724,#71725,#71726,#71727,#71728,#71729,#71730,#71731,#71732,#71733,#71734,
#71735,#71736,#71737,#71738,#71739,#71740,#71741,#71742,#71743,#71744,#71745,
#71746,#71747,#71748,#71749,#71750,#71751,#71752,#71753,#71754,#71755,#71756,
#71757,#71758,#71759,#71760,#71761,#71762,#71763,#71764,#71765,#71766,#71767,
#71768,#71769,#71770,#71771,#71772,#71773,#71774,#71775,#71776,#71777,#71778,
#71779,#71780,#71781,#71782,#71783,#71784,#71785,#71786,#71787,#71788,#71789,
#71790,#71791,#71792,#71793,#71794,#71795,#71796,#71797,#71798,#71799,#71800,
#71801,#71802,#71803,#71804,#71805,#71806,#71807,#71808,#71809,#71810,#71811,
#71812,#71813,#71814,#71815,#71816,#71817,#71818,#71819,#71820,#71821,#71822,
#71823,#71824,#71825,#71826,#71827,#71828,#71829,#71830,#71831,#71832,#71833,
#71834,#71835,#71836,#71837,#71838,#71839,#71840,#71841,#71842,#71843,#71844,
#71845,#71846,#71847,#71848),.UNSPECIFIED.,.F.,.F.,(4,2,2,2,2,2,2,2,2,2,
2,2,2,2,2,2,2,2,2,2,2,2,2,2,2,2,2,2,2,2,2,2,2,2,2,2,2,2,2,2,2,2,2,2,2,2,
2,2,2,2,2,2,2,2,2,2,2,2,2,2,2,2,2,2,2,2,2,2,2,2,2,2,2,2,2,2,2,2,2,2,2,2,
2,2,2,2,2,2,2,2,2,2,2,2,2,2,2,4),(-1.49528681114923,-1.46855272369361,-1.45428468371154,
-1.44912259759338,-1.44532634671494,-1.44346577193218,-1.44211788915904,
-1.44030054743845,-1.43683332844687,-1.41121315842747,-1.38848868021727,
-1.3831234700149,-1.38008157632856,-1.37742495327045,-1.37410235085635,
-1.3688331232657,-1.34789204676443,-1.3285707942032,-1.32403541681642,-1.31866412829265,
-1.31653414524756,-1.31501525121085,-1.3133132825484,-1.31029541555486,
-1.29154122720412,-1.27697453213141,-1.26537970380373,-1.25732375253172,
-1.25378083068097,-1.25109954987935,-1.2481807616687,-1.24340382021235,
-1.22205381702392,-1.20448858781943,-1.19648564712618,-1.19126272168435,
-1.18915538199024,-1.18763985238451,-1.18592688296747,-1.1829377339115,
-1.16400776002152,-1.14886623739257,-1.13771725512934,-1.13398995122727,
-1.12851381892228,-1.1254490228485,-1.12279463976138,-1.11950375375368,
-1.11434392984272,-1.08742109191882,-1.07246850212864,-1.06716714906454,
-1.06329440981626,-1.06141915504791,-1.05992316280081,-1.05804524014052,
-1.0541584817971,-1.03599725474525,-1.00638550074406,-1.00103327809424,
-0.997994085100304,-0.995337174967629,-0.992010721152651,-0.986728122815143,
-0.964753447519439,-0.946256017487257,-0.940312343212254,-0.936096313763103,
-0.934157349015302,-0.932673422108751,-0.930859760031999,-0.927409761503957,
-0.90163963893137,-0.885821903589034,-0.875924423632804,-0.872105609015954,
-0.869379886381196,-0.866558847922251,-0.862250080075497,-0.849049229967423,
-0.820972039672042,-0.810381009023976,-0.80770130321436,-0.806072349638351,
-0.804537392727648,-0.802605348585925,-0.79714509209623,-0.792501934915703,
-0.772327587767281,-0.75065317915987,-0.745842806773145,-0.742916871218985,
-0.740237537532097,-0.736709749514559,-0.728746881905702,-0.717341698123835,
-0.702550424108753,-0.693006869784502),.UNSPECIFIED.);
#795=B_SPLINE_CURVE_WITH_KNOTS('',3,(#71850,#71851,#71852,#71853,#71854,
#71855,#71856,#71857,#71858,#71859,#71860,#71861,#71862,#71863,#71864,#71865,
#71866,#71867,#71868,#71869,#71870,#71871,#71872,#71873,#71874,#71875,#71876,
#71877,#71878,#71879,#71880,#71881),.UNSPECIFIED.,.F.,.F.,(4,2,2,2,2,2,
2,2,2,2,2,2,2,2,2,4),(-0.110043953422301,-0.105723948072265,-0.0868134336401754,
-0.083790770499327,-0.0820879709152286,-0.0805697053593665,-0.0784426078136448,
-0.0735379468835575,-0.0438475112799801,-0.0261388361933189,-0.0214822246042773,
-0.0185891436469133,-0.0160354833484494,-0.013420339260892,-0.00999057246888134,
-0.000374718360681822),.UNSPECIFIED.);
#796=B_SPLINE_CURVE_WITH_KNOTS('',3,(#71882,#71883,#71884,#71885,#71886,
#71887,#71888,#71889,#71890,#71891,#71892,#71893,#71894,#71895,#71896,#71897,
#71898,#71899,#71900,#71901,#71902,#71903,#71904,#71905,#71906,#71907,#71908,
#71909,#71910,#71911,#71912,#71913,#71914,#71915,#71916,#71917,#71918,#71919,
#71920,#71921,#71922,#71923,#71924,#71925,#71926,#71927,#71928,#71929,#71930,
#71931,#71932,#71933,#71934,#71935,#71936,#71937,#71938,#71939,#71940,#71941,
#71942,#71943,#71944,#71945,#71946,#71947,#71948,#71949,#71950,#71951,#71952,
#71953,#71954,#71955,#71956,#71957,#71958,#71959,#71960,#71961,#71962,#71963,
#71964,#71965,#71966,#71967,#71968,#71969,#71970,#71971,#71972,#71973,#71974,
#71975,#71976,#71977,#71978,#71979,#71980,#71981,#71982,#71983,#71984,#71985,
#71986,#71987,#71988,#71989,#71990,#71991,#71992,#71993,#71994,#71995,#71996,
#71997,#71998,#71999,#72000,#72001,#72002,#72003,#72004,#72005,#72006,#72007,
#72008,#72009,#72010,#72011,#72012,#72013,#72014,#72015,#72016,#72017,#72018,
#72019,#72020,#72021,#72022,#72023,#72024,#72025,#72026,#72027,#72028,#72029,
#72030,#72031,#72032,#72033,#72034,#72035,#72036,#72037,#72038,#72039,#72040,
#72041,#72042,#72043,#72044,#72045,#72046,#72047,#72048,#72049,#72050,#72051,
#72052,#72053,#72054,#72055,#72056,#72057,#72058,#72059,#72060,#72061,#72062,
#72063),.UNSPECIFIED.,.F.,.F.,(4,2,2,2,2,2,2,2,2,2,2,2,2,2,2,2,2,2,2,2,
2,2,2,2,2,2,2,2,2,2,2,2,2,2,2,2,2,2,2,2,2,2,2,2,2,2,2,2,2,2,2,2,2,2,2,2,
2,2,2,2,2,2,2,2,2,2,2,2,2,2,2,2,2,2,2,2,2,2,2,2,2,2,2,2,2,2,2,2,2,2,4),
(-2.40676737505766,-2.36885811930424,-2.36539243889984,-2.36332834988335,
-2.36145385669369,-2.35995866505869,-2.35808203778825,-2.35419895511609,
-2.33623601044081,-2.32060916989795,-2.31000876570412,-2.3047626346255,
-2.30040444525601,-2.30027274855213,-2.30014099121797,-2.30000764581859,
-2.29987103087719,-2.29722856429417,-2.29451931915846,-2.2912480939647,
-2.28315200209121,-2.25511701496819,-2.24370005186781,-2.23706883417478,
-2.2347665378962,-2.23321793657518,-2.23158360508162,-2.2288768215928,-2.21906637476102,
-2.1986970470316,-2.1791581740144,-2.17379302171211,-2.17075200161204,-2.16809663777398,
-2.16477628523681,-2.15951208693814,-2.13721650032768,-2.11894980169944,
-2.11304512246817,-2.10884992630379,-2.10691524696749,-2.1054321951931,
-2.10361665105082,-2.10015555029197,-2.07449770850116,-2.05862615101731,
-2.04870888370183,-2.0448884177559,-2.04216330686692,-2.03967691703059,
-2.0363059735757,-2.02763478336961,-2.00020914183136,-1.98502087527762,
-1.98127062914168,-1.97941942847561,-1.97807255577222,-1.9762481484466,
-1.97274535820892,-1.94746155372281,-1.93138704444944,-1.92460025860737,
-1.91916884660418,-1.91611404308323,-1.91345995559178,-1.91015859168998,
-1.90496024985769,-1.8789836033319,-1.86339829114684,-1.8579735724623,-1.85403406252968,
-1.85214660975268,-1.85065117813065,-1.84878684399256,-1.84496872606216,
-1.81643888396224,-1.79713350677552,-1.79176468352873,-1.78872281261131,
-1.7860674015248,-1.78274790590747,-1.77748696564915,-1.75648150480151,
-1.73720627442121,-1.73267741279706,-1.72731205921512,-1.72518348954293,
-1.7236652941129,-1.72196379626685,-1.71894615478858,-1.71427609505927),
 .UNSPECIFIED.);
#797=B_SPLINE_CURVE_WITH_KNOTS('',3,(#72069,#72070,#72071,#72072,#72073,
#72074,#72075,#72076,#72077,#72078,#72079,#72080,#72081,#72082,#72083,#72084,
#72085,#72086,#72087,#72088,#72089,#72090,#72091,#72092,#72093,#72094,#72095,
#72096,#72097,#72098,#72099,#72100,#72101,#72102,#72103,#72104,#72105,#72106,
#72107,#72108,#72109,#72110,#72111,#72112,#72113,#72114,#72115,#72116,#72117,
#72118,#72119,#72120,#72121,#72122,#72123,#72124,#72125,#72126,#72127,#72128,
#72129,#72130,#72131,#72132,#72133,#72134,#72135,#72136,#72137,#72138,#72139,
#72140,#72141,#72142,#72143,#72144,#72145,#72146,#72147,#72148,#72149,#72150,
#72151,#72152,#72153,#72154,#72155,#72156,#72157,#72158,#72159,#72160,#72161,
#72162,#72163,#72164,#72165,#72166,#72167,#72168,#72169,#72170,#72171,#72172,
#72173,#72174,#72175,#72176,#72177,#72178,#72179,#72180,#72181,#72182,#72183,
#72184,#72185,#72186,#72187,#72188,#72189,#72190,#72191,#72192,#72193,#72194,
#72195,#72196,#72197,#72198,#72199,#72200,#72201,#72202,#72203,#72204,#72205,
#72206,#72207,#72208,#72209,#72210,#72211,#72212,#72213,#72214,#72215,#72216,
#72217,#72218,#72219,#72220,#72221,#72222,#72223,#72224,#72225,#72226,#72227,
#72228,#72229,#72230,#72231,#72232,#72233,#72234,#72235,#72236,#72237,#72238,
#72239,#72240,#72241,#72242,#72243,#72244,#72245,#72246),.UNSPECIFIED.,
 .F.,.F.,(4,2,2,2,2,2,2,2,2,2,2,2,2,2,2,2,2,2,2,2,2,2,2,2,2,2,2,2,2,2,2,
2,2,2,2,2,2,2,2,2,2,2,2,2,2,2,2,2,2,2,2,2,2,2,2,2,2,2,2,2,2,2,2,2,2,2,2,
2,2,2,2,2,2,2,2,2,2,2,2,2,2,2,2,2,2,2,2,2,4),(-0.693097973780701,-0.674549641960477,
-0.669769327196677,-0.666850111379091,-0.664169475107421,-0.660628949477002,
-0.652586032237884,-0.641015331240216,-0.626400811058394,-0.607614692510139,
-0.604596273449597,-0.602894319605062,-0.601375640929368,-0.599246312987551,
-0.593878156109545,-0.589346788109495,-0.570047575324775,-0.549117048286052,
-0.543854108710772,-0.540533489627345,-0.537877266572495,-0.534834538807356,
-0.529464413475491,-0.5258331620478,-0.51994071445516,-0.497561490725128,
-0.480235875503355,-0.477238771902252,-0.475541319703888,-0.474021049270523,
-0.471881777337472,-0.466447844962255,-0.461836612463552,-0.4419151443869,
-0.41986999739315,-0.415089819908908,-0.412170485508472,-0.409489609605992,
-0.4059485738069,-0.397903591193224,-0.386329015522499,-0.371716560840827,
-0.352930761147811,-0.349912167527107,-0.348210094899348,-0.346691295159436,
-0.344561776821192,-0.339193032123336,-0.334661104104818,-0.315358786849685,
-0.294429194368609,-0.289165590683144,-0.285844640913248,-0.283188207344413,
-0.280145297173966,-0.274775009919012,-0.268087397708659,-0.252417314302911,
-0.227201442056148,-0.223578551418683,-0.221732704114275,-0.220219043687819,
-0.218548932402678,-0.215679356975658,-0.201704586611215,-0.172437607876477,
-0.163140267015902,-0.159310171578589,-0.156609605734997,-0.154153034911004,
-0.150304655941825,-0.145856576375551,-0.137621381185388,-0.114452245743204,
-0.0981607023113854,-0.0951691819174354,-0.093472860190305,-0.0919520782547177,
-0.0904229041201003,-0.086798293467879,-0.0737300039025831,-0.0479322634489471,
-0.0364539992731121,-0.0323301275026648,-0.029824580290477,-0.02711313506907,
-0.0244320123183317,-0.0208122799601177,-0.000374898576945566),
 .UNSPECIFIED.);
#798=B_SPLINE_CURVE_WITH_KNOTS('',3,(#72247,#72248,#72249,#72250,#72251,
#72252,#72253,#72254,#72255,#72256,#72257,#72258,#72259,#72260,#72261,#72262,
#72263,#72264,#72265,#72266,#72267,#72268,#72269,#72270,#72271,#72272,#72273,
#72274,#72275,#72276,#72277,#72278,#72279,#72280,#72281,#72282,#72283,#72284,
#72285,#72286,#72287,#72288,#72289,#72290,#72291,#72292,#72293,#72294,#72295,
#72296,#72297,#72298,#72299,#72300,#72301,#72302,#72303,#72304),
 .UNSPECIFIED.,.F.,.F.,(4,2,2,2,2,2,2,2,2,2,2,2,2,2,2,2,2,2,2,2,2,2,2,2,
2,2,2,2,4),(-1.60473182869979,-1.57950221225551,-1.57499179546473,-1.57286135670865,
-1.57132330223305,-1.56979822383723,-1.5681137886786,-1.56517774394569,
-1.55095382492133,-1.52912947981169,-1.51420712342516,-1.50981965579016,
-1.50970266867535,-1.50958436993072,-1.50946351888462,-1.50933871895019,
-1.50920833971582,-1.50907040950528,-1.50892246071234,-1.50876129769517,
-1.50858263340586,-1.50838049388529,-1.50814618906318,-1.50791857137058,
-1.5075808029852,-1.50492808808717,-1.5016648820731,-1.49659976078895,-1.49528681114923),
 .UNSPECIFIED.);
#799=B_SPLINE_CURVE_WITH_KNOTS('',3,(#72305,#72306,#72307,#72308,#72309,
#72310,#72311,#72312,#72313,#72314,#72315,#72316,#72317,#72318,#72319,#72320,
#72321,#72322,#72323,#72324,#72325,#72326,#72327,#72328,#72329,#72330,#72331,
#72332,#72333,#72334,#72335,#72336,#72337,#72338,#72339,#72340,#72341,#72342,
#72343,#72344,#72345,#72346,#72347,#72348,#72349,#72350,#72351,#72352,#72353,
#72354,#72355,#72356,#72357,#72358,#72359,#72360,#72361,#72362,#72363,#72364,
#72365,#72366,#72367,#72368,#72369,#72370,#72371,#72372,#72373,#72374,#72375,
#72376,#72377,#72378,#72379,#72380,#72381,#72382,#72383,#72384,#72385,#72386,
#72387,#72388,#72389,#72390,#72391,#72392,#72393,#72394,#72395,#72396,#72397,
#72398,#72399,#72400,#72401,#72402,#72403,#72404,#72405,#72406,#72407,#72408,
#72409,#72410,#72411,#72412,#72413,#72414,#72415,#72416,#72417,#72418,#72419,
#72420,#72421,#72422,#72423,#72424,#72425,#72426,#72427,#72428,#72429,#72430,
#72431,#72432,#72433,#72434,#72435,#72436,#72437,#72438,#72439,#72440,#72441,
#72442,#72443,#72444,#72445,#72446,#72447,#72448,#72449,#72450,#72451,#72452,
#72453,#72454,#72455,#72456,#72457,#72458,#72459,#72460,#72461,#72462,#72463,
#72464,#72465,#72466,#72467,#72468,#72469,#72470,#72471,#72472,#72473,#72474,
#72475,#72476,#72477,#72478,#72479,#72480,#72481,#72482,#72483,#72484,#72485,
#72486,#72487,#72488,#72489,#72490,#72491,#72492,#72493,#72494,#72495,#72496,
#72497,#72498,#72499,#72500),.UNSPECIFIED.,.F.,.F.,(4,2,2,2,2,2,2,2,2,2,
2,2,2,2,2,2,2,2,2,2,2,2,2,2,2,2,2,2,2,2,2,2,2,2,2,2,2,2,2,2,2,2,2,2,2,2,
2,2,2,2,2,2,2,2,2,2,2,2,2,2,2,2,2,2,2,2,2,2,2,2,2,2,2,2,2,2,2,2,2,2,2,2,
2,2,2,2,2,2,2,2,2,2,2,2,2,2,2,4),(-1.71427609505927,-1.70017303108593,-1.68556904885637,
-1.67401337215023,-1.66597714801641,-1.66243832947086,-1.65975850435754,
-1.65683971639778,-1.65205913441651,-1.62999996772187,-1.61006058655689,
-1.60544646022636,-1.60001096042517,-1.59787184069993,-1.59635200523981,
-1.59465539127848,-1.59166066478746,-1.57454439136803,-1.55204064591276,
-1.54392032541994,-1.53769856415861,-1.53448515206266,-1.53209369373478,
-1.52906712745507,-1.52390994022624,-1.49237913026035,-1.48007144990521,
-1.47311729244318,-1.47077555213529,-1.46921909128428,-1.46779583423245,
-1.46534176224731,-1.45806426073014,-1.43582571772125,-1.41394917988829,
-1.40921063025882,-1.40630065135319,-1.40361792659188,-1.40011999009848,
-1.39210156497417,-1.36382223443214,-1.34834535786019,-1.34456347882511,
-1.34270605794405,-1.34121041764444,-1.3393154315555,-1.33533623270764,
-1.31011207241857,-1.29444636538617,-1.28776063683116,-1.28239112492061,
-1.27934893572701,-1.2766932874654,-1.27337354889257,-1.26811233456746,
-1.24710313926716,-1.22782728057926,-1.22329815384168,-1.21793243338644,
-1.21580368829209,-1.21428535744858,-1.21258369603666,-1.20956573923473,
-1.190789692139,-1.17618220113236,-1.164627513391,-1.15659154746579,-1.15305256930436,
-1.15037252280154,-1.14745339606362,-1.142672031759,-1.12065324374132,-1.10382899749774,
-1.09579036606485,-1.09055149765998,-1.08844209345814,-1.0869266444777,
-1.08521561540114,-1.08223368898902,-1.06349601681706,-1.04895993334718,
-1.03733921609711,-1.02927127916442,-1.02572705924817,-1.02304628270159,
-1.02012950208988,-1.01535928236584,-0.994104480282265,-0.976427234666432,
-0.968430370325362,-0.963210584308027,-0.96110412203481,-0.959589099409234,
-0.95787660282681,-0.954888127845239,-0.935959519200394,-0.920819904523672,
-0.912183428409147),.UNSPECIFIED.);
#800=B_SPLINE_CURVE_WITH_KNOTS('',3,(#72505,#72506,#72507,#72508,#72509,
#72510,#72511,#72512,#72513,#72514,#72515,#72516,#72517,#72518,#72519,#72520,
#72521,#72522,#72523,#72524,#72525,#72526,#72527,#72528,#72529,#72530,#72531,
#72532,#72533,#72534,#72535,#72536,#72537,#72538,#72539,#72540,#72541,#72542,
#72543,#72544,#72545,#72546,#72547,#72548,#72549,#72550,#72551,#72552,#72553,
#72554,#72555,#72556,#72557,#72558,#72559,#72560,#72561,#72562,#72563,#72564,
#72565,#72566,#72567,#72568,#72569,#72570,#72571,#72572,#72573,#72574,#72575,
#72576,#72577,#72578,#72579,#72580,#72581,#72582,#72583,#72584,#72585,#72586,
#72587,#72588,#72589,#72590,#72591,#72592,#72593,#72594,#72595,#72596,#72597,
#72598,#72599,#72600,#72601,#72602,#72603,#72604,#72605,#72606,#72607,#72608,
#72609,#72610,#72611,#72612,#72613,#72614,#72615,#72616,#72617,#72618,#72619,
#72620,#72621,#72622,#72623,#72624,#72625,#72626,#72627,#72628,#72629,#72630,
#72631,#72632,#72633,#72634,#72635,#72636,#72637,#72638,#72639,#72640,#72641,
#72642,#72643,#72644,#72645,#72646,#72647,#72648,#72649,#72650,#72651,#72652,
#72653,#72654,#72655,#72656,#72657,#72658,#72659,#72660,#72661,#72662,#72663,
#72664,#72665,#72666,#72667,#72668,#72669,#72670,#72671,#72672,#72673,#72674,
#72675,#72676,#72677,#72678,#72679,#72680,#72681,#72682,#72683,#72684,#72685,
#72686,#72687,#72688,#72689,#72690,#72691,#72692,#72693,#72694,#72695,#72696,
#72697,#72698,#72699,#72700,#72701,#72702,#72703,#72704),.UNSPECIFIED.,
 .F.,.F.,(4,2,2,2,2,2,2,2,2,2,2,2,2,2,2,2,2,2,2,2,2,2,2,2,2,2,2,2,2,2,2,
2,2,2,2,2,2,2,2,2,2,2,2,2,2,2,2,2,2,2,2,2,2,2,2,2,2,2,2,2,2,2,2,2,2,2,2,
2,2,2,2,2,2,2,2,2,2,2,2,2,2,2,2,2,2,2,2,2,2,2,2,2,2,2,2,2,2,2,2,4),(-1.4951650948055,
-1.49447528564397,-1.49306392442721,-1.49114658335287,-1.48704743911027,
-1.46198518424821,-1.44633910347216,-1.43965837595818,-1.43429191177407,
-1.43125022808202,-1.42859430966004,-1.42527327522059,-1.42000795915998,
-1.39904446496783,-1.37974559744137,-1.37521362934586,-1.36984555104675,
-1.36771637310754,-1.36619789203425,-1.36449620136358,-1.36147843240729,
-1.34270960496494,-1.32811110531228,-1.31655189904539,-1.30851379808812,
-1.30497434467855,-1.30229407833229,-1.29937483058712,-1.29459349643746,
-1.27258931935542,-1.2526103525059,-1.24799122551831,-1.24255147102499,
-1.24041151808989,-1.23889136123176,-1.23719465521174,-1.23420027177389,
-1.21722321120531,-1.19461703595385,-1.18647907616479,-1.1802470460008,
-1.17703133033609,-1.17463932956751,-1.17161360477339,-1.16646160399906,
-1.13489545098283,-1.1226079945036,-1.11566084740704,-1.11331972259105,
-1.11176321112413,-1.11033949068955,-1.1078837926122,-1.10059450541295,
-1.07836686979375,-1.05767422533776,-1.05230033791561,-1.04925704616846,
-1.04660119293673,-1.04328217373071,-1.03802406050656,-1.01513600159545,
-0.993369745695994,-0.98788151275423,-0.985734286299891,-0.98421293067608,
-0.982519408292301,-0.979540132601306,-0.963905513812062,-0.940931343280396,
-0.928008123093209,-0.923833616043403,-0.921040227947654,-0.918327367378527,
-0.914427176960801,-0.90462177412823,-0.87826978273584,-0.863451787979356,
-0.859742236505118,-0.857898694544346,-0.856551834473005,-0.854719226595905,
-0.851065418715158,-0.82705142425113,-0.802685988624029,-0.797538249940807,
-0.794513351679398,-0.792121100846208,-0.788903851833482,-0.782664700127272,
-0.774513009440679,-0.751837935199026,-0.734906975750591,-0.731911709645646,
-0.730214732144666,-0.728694462938626,-0.726554609811127,-0.721116098971184,
-0.716499119787935,-0.696530704436245,-0.693097973780701),.UNSPECIFIED.);
#801=B_SPLINE_CURVE_WITH_KNOTS('',3,(#72705,#72706,#72707,#72708,#72709,
#72710,#72711,#72712,#72713,#72714,#72715,#72716,#72717,#72718,#72719,#72720,
#72721,#72722,#72723,#72724,#72725,#72726,#72727,#72728,#72729,#72730,#72731,
#72732,#72733,#72734,#72735,#72736,#72737,#72738,#72739,#72740,#72741,#72742,
#72743,#72744,#72745,#72746,#72747,#72748,#72749,#72750,#72751,#72752,#72753,
#72754,#72755,#72756,#72757,#72758,#72759,#72760,#72761,#72762,#72763,#72764,
#72765,#72766,#72767,#72768,#72769,#72770,#72771,#72772,#72773,#72774,#72775,
#72776,#72777,#72778,#72779,#72780,#72781,#72782,#72783,#72784,#72785,#72786,
#72787,#72788,#72789,#72790,#72791,#72792,#72793,#72794,#72795,#72796,#72797,
#72798,#72799,#72800,#72801,#72802,#72803,#72804,#72805,#72806,#72807,#72808,
#72809,#72810,#72811,#72812,#72813,#72814,#72815,#72816,#72817,#72818,#72819,
#72820,#72821,#72822,#72823,#72824,#72825,#72826,#72827,#72828,#72829,#72830,
#72831,#72832,#72833,#72834,#72835,#72836,#72837,#72838,#72839,#72840,#72841,
#72842,#72843,#72844,#72845,#72846,#72847,#72848,#72849,#72850,#72851,#72852,
#72853,#72854,#72855,#72856,#72857,#72858,#72859,#72860,#72861,#72862,#72863,
#72864,#72865,#72866,#72867,#72868,#72869,#72870,#72871,#72872,#72873,#72874,
#72875,#72876,#72877,#72878,#72879,#72880,#72881,#72882,#72883,#72884,#72885,
#72886,#72887,#72888,#72889,#72890,#72891,#72892,#72893,#72894,#72895,#72896,
#72897,#72898,#72899,#72900,#72901,#72902,#72903,#72904,#72905,#72906,#72907,
#72908,#72909,#72910),.UNSPECIFIED.,.F.,.F.,(4,2,2,2,2,2,2,2,2,2,2,2,2,
2,2,2,2,2,2,2,2,2,2,2,2,2,2,2,2,2,2,2,2,2,2,2,2,2,2,2,2,2,2,2,2,2,2,2,2,
2,2,2,2,2,2,2,2,2,2,2,2,2,2,2,2,2,2,2,2,2,2,2,2,2,2,2,2,2,2,2,2,2,2,2,2,
2,2,2,2,2,2,2,2,2,2,2,2,2,2,2,2,2,4),(-0.912183428409147,-0.909671435824856,
-0.905944473968316,-0.900469105869615,-0.897405062984082,-0.894751533133857,
-0.891461985557897,-0.886304887334374,-0.859350711777633,-0.844420931988362,
-0.839124610941128,-0.835254869517453,-0.833380534110074,-0.831885015905191,
-0.830007410952487,-0.826120492190165,-0.807839026955135,-0.785036967355285,
-0.778375912782796,-0.77302154311998,-0.769982418601881,-0.767326319316143,
-0.764001893366411,-0.758724683002095,-0.736684389957623,-0.71823188451559,
-0.712296011234923,-0.708084289277837,-0.706146412716717,-0.704662927355313,
-0.702849364172057,-0.699398483790527,-0.673641249020921,-0.657817582749607,
-0.651092349110172,-0.645698508893679,-0.642651213017173,-0.639995994759288,
-0.636683208998828,-0.631446267963429,-0.606945776447085,-0.590310389252202,
-0.584688771737222,-0.580643193787097,-0.578735751186671,-0.577239722480526,
-0.575393501099614,-0.571669662655668,-0.54863484980516,-0.523540002267338,
-0.51825073883406,-0.515225132315514,-0.512567408565113,-0.509223062416149,
-0.503876677550803,-0.496252349283697,-0.476421512166381,-0.457052206429446,
-0.453186629666559,-0.451313076497196,-0.449817540386607,-0.447939106896463,
-0.444047895177174,-0.438713157543517,-0.423587361373984,-0.396972971280271,
-0.391801323230041,-0.388507488665556,-0.385853631066752,-0.38279266684416,
-0.377332523307534,-0.370497839597455,-0.35422988640262,-0.329243467800514,
-0.325705504763716,-0.323873526356167,-0.322526754420353,-0.320682921081915,
-0.316971451281173,-0.302135988458375,-0.275726905019111,-0.266013434072886,
-0.262122173922496,-0.259411064736845,-0.256615759259425,-0.252431177050569,
-0.2394087109049,-0.216071193352779,-0.200847480271835,-0.197878256551177,
-0.196186931659452,-0.194664868018181,-0.192513070827879,-0.186993485177083,
-0.182276967053412,-0.16150058880361,-0.140594532836167,-0.135874386843129,
-0.132925957423104,-0.130419423273389,-0.127841855145072,-0.124529608056003,
-0.109984215976658),.UNSPECIFIED.);
#802=B_SPLINE_CURVE_WITH_KNOTS('',3,(#72916,#72917,#72918,#72919,#72920,
#72921,#72922,#72923,#72924,#72925,#72926,#72927,#72928,#72929,#72930,#72931,
#72932,#72933,#72934,#72935,#72936,#72937,#72938,#72939,#72940,#72941,#72942,
#72943,#72944,#72945,#72946,#72947,#72948,#72949,#72950,#72951,#72952,#72953,
#72954,#72955,#72956,#72957,#72958,#72959,#72960,#72961,#72962,#72963,#72964,
#72965,#72966,#72967,#72968,#72969,#72970,#72971,#72972,#72973,#72974,#72975,
#72976,#72977,#72978,#72979,#72980,#72981,#72982,#72983,#72984,#72985,#72986,
#72987,#72988,#72989,#72990,#72991,#72992,#72993,#72994,#72995,#72996,#72997,
#72998,#72999,#73000,#73001,#73002,#73003,#73004,#73005,#73006,#73007,#73008,
#73009,#73010,#73011,#73012,#73013,#73014,#73015,#73016,#73017,#73018,#73019,
#73020,#73021,#73022,#73023,#73024,#73025,#73026,#73027,#73028,#73029,#73030,
#73031,#73032,#73033,#73034,#73035,#73036,#73037,#73038,#73039,#73040,#73041,
#73042,#73043,#73044,#73045,#73046,#73047,#73048,#73049,#73050,#73051,#73052,
#73053,#73054,#73055,#73056,#73057,#73058,#73059,#73060,#73061,#73062,#73063,
#73064,#73065,#73066,#73067,#73068,#73069,#73070,#73071,#73072,#73073,#73074,
#73075,#73076,#73077,#73078,#73079,#73080,#73081,#73082,#73083,#73084,#73085,
#73086,#73087,#73088,#73089,#73090,#73091,#73092,#73093),.UNSPECIFIED.,
 .F.,.F.,(4,2,2,2,2,2,2,2,2,2,2,2,2,2,2,2,2,2,2,2,2,2,2,2,2,2,2,2,2,2,2,
2,2,2,2,2,2,2,2,2,2,2,2,2,2,2,2,2,2,2,2,2,2,2,2,2,2,2,2,2,2,2,2,2,2,2,2,
2,2,2,2,2,2,2,2,2,2,2,2,2,2,2,2,2,2,2,2,2,4),(-0.692866832200926,-0.692429841896259,
-0.677564642022375,-0.65860681414682,-0.65561734955069,-0.653904485899281,
-0.652389220739771,-0.650282554339005,-0.645062507749672,-0.637066663952617,
-0.619534767965853,-0.598195365700189,-0.593418847644417,-0.590500442820064,
-0.587819576856678,-0.584277303563173,-0.576223648773558,-0.564630744430341,
-0.550040282648017,-0.531267419531168,-0.528249450010645,-0.526547598542327,
-0.525028900155804,-0.522899391304837,-0.517529975729226,-0.512997069945273,
-0.493685947566791,-0.472774422140611,-0.46750966263123,-0.464188529998434,
-0.461532284157875,-0.458489952235369,-0.45312167465568,-0.431151421593968,
-0.406740703957918,-0.402028112199817,-0.400143080609763,-0.398620233435407,
-0.39697042339584,-0.394194188743825,-0.382084872669531,-0.365235832692922,
-0.343572521515228,-0.338763872908473,-0.335838590220417,-0.333159600641532,
-0.329631892310251,-0.321667481345501,-0.310258397245341,-0.295475021956934,
-0.276586065095174,-0.273564000444231,-0.271861210906231,-0.270342688413377,
-0.268214814823387,-0.262856762593005,-0.25833772914005,-0.239133741195724,
-0.218059994578015,-0.212806940996901,-0.20948908364662,-0.206832941453479,
-0.203787988550606,-0.198407612120565,-0.176555692585955,-0.152330650292729,
-0.147418826773976,-0.145501521755874,-0.14397049987697,-0.142368283753846,
-0.139771155769888,-0.136568396477909,-0.129885128383817,-0.106156268801215,
-0.0885737715830057,-0.0839176749963868,-0.0810243844670173,-0.0783345105395892,
-0.0747317980163937,-0.0664631824218435,-0.0433552328482521,-0.0266755417178896,
-0.0204804644227642,-0.0181713332211261,-0.0166363156174901,-0.0152426914363794,
-0.0136145686663947,-0.0112495068105053,-0.000374704675043261),
 .UNSPECIFIED.);
#803=B_SPLINE_CURVE_WITH_KNOTS('',3,(#73094,#73095,#73096,#73097,#73098,
#73099,#73100,#73101,#73102,#73103,#73104,#73105,#73106,#73107,#73108,#73109,
#73110,#73111,#73112,#73113,#73114,#73115,#73116,#73117,#73118,#73119,#73120,
#73121),.UNSPECIFIED.,.F.,.F.,(4,2,2,2,2,2,2,2,2,2,2,2,2,4),(-1.60482636128448,
-1.57369633890873,-1.56700004022034,-1.56311826205165,-1.55959258294555,
-1.55691425521273,-1.5539888304229,-1.54917796400828,-1.52747173937229,
-1.51170533182018,-1.5028548534436,-1.49900355783005,-1.49609325357449,
-1.4951650948055),.UNSPECIFIED.);
#804=B_SPLINE_CURVE_WITH_KNOTS('',3,(#73123,#73124,#73125,#73126,#73127,
#73128,#73129,#73130,#73131,#73132,#73133,#73134,#73135,#73136,#73137,#73138,
#73139,#73140,#73141,#73142,#73143,#73144,#73145,#73146,#73147,#73148,#73149,
#73150,#73151,#73152,#73153,#73154,#73155,#73156),.UNSPECIFIED.,.F.,.F.,
(4,2,2,2,2,2,2,2,2,2,2,2,2,2,2,2,4),(-0.109984215976658,-0.108466704677333,
-0.0929800570091766,-0.0750124521263942,-0.0711272018396201,-0.0692498278984506,
-0.0677541996645172,-0.0658793571402882,-0.0620073879157499,-0.0511499299104798,
-0.0284204838189786,-0.0198058823455182,-0.0109766423492752,-0.0072974848453584,
-0.0046289889386618,-0.00236675908727173,-0.000393535835646313),
 .UNSPECIFIED.);
#805=B_SPLINE_CURVE_WITH_KNOTS('',3,(#73157,#73158,#73159,#73160,#73161,
#73162,#73163,#73164,#73165),.UNSPECIFIED.,.F.,.F.,(4,1,1,1,1,1,4),(109.955745458758,
110.419877743936,111.417384325898,112.41489090786,113.412397489822,114.409904071784,
115.380591207589),.UNSPECIFIED.);
#806=B_SPLINE_CURVE_WITH_KNOTS('',3,(#73170,#73171,#73172,#73173,#73174,
#73175,#73176,#73177,#73178,#73179,#73180,#73181,#73182,#73183,#73184,#73185,
#73186,#73187,#73188,#73189,#73190,#73191,#73192,#73193,#73194,#73195,#73196,
#73197,#73198,#73199,#73200,#73201,#73202,#73203,#73204,#73205,#73206,#73207,
#73208,#73209,#73210,#73211,#73212,#73213,#73214,#73215,#73216,#73217,#73218,
#73219,#73220,#73221,#73222,#73223,#73224,#73225,#73226,#73227,#73228,#73229,
#73230,#73231,#73232,#73233,#73234,#73235,#73236,#73237,#73238,#73239,#73240,
#73241,#73242,#73243,#73244,#73245,#73246,#73247,#73248,#73249,#73250,#73251,
#73252,#73253,#73254,#73255,#73256,#73257,#73258,#73259,#73260,#73261,#73262,
#73263,#73264,#73265,#73266,#73267,#73268,#73269,#73270,#73271,#73272,#73273,
#73274,#73275,#73276,#73277,#73278,#73279,#73280,#73281,#73282,#73283,#73284,
#73285,#73286,#73287,#73288,#73289,#73290,#73291,#73292,#73293,#73294,#73295,
#73296,#73297,#73298,#73299,#73300,#73301,#73302,#73303,#73304,#73305,#73306,
#73307,#73308,#73309,#73310,#73311,#73312,#73313,#73314,#73315,#73316,#73317,
#73318,#73319,#73320,#73321,#73322,#73323,#73324,#73325,#73326,#73327,#73328,
#73329,#73330,#73331,#73332,#73333,#73334,#73335,#73336,#73337,#73338,#73339,
#73340,#73341,#73342,#73343,#73344,#73345,#73346,#73347,#73348,#73349,#73350,
#73351,#73352,#73353,#73354,#73355,#73356,#73357,#73358,#73359,#73360,#73361,
#73362,#73363,#73364,#73365,#73366,#73367,#73368,#73369,#73370,#73371,#73372,
#73373,#73374,#73375,#73376,#73377,#73378,#73379),.UNSPECIFIED.,.F.,.F.,
(4,2,2,2,2,2,2,2,2,2,2,2,2,2,2,2,2,2,2,2,2,2,2,2,2,2,2,2,2,2,2,2,2,2,2,
2,2,2,2,2,2,2,2,2,2,2,2,2,2,2,2,2,2,2,2,2,2,2,2,2,2,2,2,2,2,2,2,2,2,2,2,
2,2,2,2,2,2,2,2,2,2,2,2,2,2,2,2,2,2,2,2,2,2,2,2,2,2,2,2,2,2,2,2,2,4),(-1.49484735329919,
-1.49484548901206,-1.48674394087996,-1.4839536958272,-1.48351580354143,
-1.48306057098407,-1.48293853263072,-1.4803502913914,-1.47746324147295,
-1.47275409837007,-1.45158379469974,-1.43390306301323,-1.42590944699101,
-1.4206916357885,-1.4185858469295,-1.41707121592934,-1.41535893770416,-1.41237061585787,
-1.39343189219521,-1.37828272968426,-1.36715911855713,-1.36343853441178,
-1.35797040008061,-1.35490814343165,-1.35225488253909,-1.34896398869188,
-1.34380129057227,-1.31699938277325,-1.30198523054024,-1.29667275036799,
-1.29279439127633,-1.29091857199719,-1.28942327352004,-1.28754764365696,
-1.28367002008495,-1.26601815451493,-1.25073985275118,-1.23976218660559,
-1.2360777320863,-1.23064916854066,-1.22759503359207,-1.22494098479056,
-1.22163894194219,-1.21643798574239,-1.19057483620645,-1.17491973908619,
-1.1694819540276,-1.1655354693624,-1.16364676100844,-1.16215137738946,-1.16028835999769,
-1.15647676786762,-1.13494336649669,-1.10767686376367,-1.10283125577838,
-1.09989869333012,-1.09722271970327,-1.09377241829604,-1.08634130077601,
-1.05475867166893,-1.04499675958336,-1.03901212495264,-1.03679422347914,
-1.0352611145489,-1.03359713622626,-1.03075458245268,-1.0188465865962,-0.992079180076298,
-0.979005382801924,-0.974816139563256,-0.972019986638176,-0.969309702161997,
-0.966035601471855,-0.958012128188596,-0.929930811708622,-0.914521581428813,
-0.910747012175014,-0.908890930492542,-0.907395147213971,-0.905498384784684,
-0.901510071644215,-0.876299941408438,-0.86064015035326,-0.850805503732773,
-0.846995895977954,-0.844272312627503,-0.841783114440567,-0.838401865113623,
-0.829634538140932,-0.802297646701117,-0.785878197715148,-0.782885869073012,
-0.781189565407821,-0.779669157251544,-0.777528087703224,-0.772081042854728,
-0.76745354877006,-0.747400586835847,-0.725614204714521,-0.72078946134825,
-0.717860973303176,-0.715183259198693,-0.711663411498443,-0.703745144296636,
-0.692866832200926),.UNSPECIFIED.);
#807=B_SPLINE_CURVE_WITH_KNOTS('',3,(#73381,#73382,#73383,#73384,#73385),
 .UNSPECIFIED.,.F.,.F.,(4,1,4),(115.380591207589,115.407410653746,116.238922074783),
 .UNSPECIFIED.);
#808=B_SPLINE_CURVE_WITH_KNOTS('',3,(#73386,#73387,#73388,#73389,#73390,
#73391,#73392,#73393,#73394,#73395,#73396,#73397,#73398,#73399,#73400,#73401,
#73402,#73403,#73404,#73405,#73406,#73407,#73408,#73409,#73410,#73411,#73412,
#73413,#73414,#73415,#73416,#73417,#73418,#73419,#73420,#73421,#73422,#73423,
#73424,#73425,#73426,#73427,#73428,#73429,#73430,#73431,#73432,#73433,#73434,
#73435,#73436,#73437,#73438,#73439,#73440,#73441,#73442,#73443,#73444,#73445,
#73446,#73447,#73448,#73449,#73450,#73451,#73452,#73453,#73454,#73455,#73456,
#73457,#73458,#73459,#73460,#73461,#73462,#73463,#73464,#73465,#73466,#73467,
#73468,#73469,#73470,#73471,#73472,#73473,#73474,#73475,#73476,#73477,#73478,
#73479,#73480,#73481,#73482,#73483,#73484,#73485,#73486,#73487,#73488,#73489,
#73490,#73491,#73492,#73493,#73494,#73495,#73496,#73497,#73498,#73499,#73500,
#73501,#73502,#73503,#73504,#73505,#73506,#73507,#73508,#73509,#73510,#73511,
#73512,#73513,#73514,#73515,#73516,#73517,#73518,#73519,#73520,#73521,#73522,
#73523,#73524,#73525,#73526,#73527,#73528,#73529,#73530,#73531,#73532,#73533),
 .UNSPECIFIED.,.F.,.F.,(4,3,3,3,3,3,3,3,3,3,3,3,3,3,3,3,3,3,3,3,3,3,3,3,
3,3,3,3,3,3,3,3,3,3,3,3,3,3,3,3,3,3,3,3,3,3,3,3,3,4),(116.238928182822,
116.404917235708,116.522420828224,116.639708216653,116.756876517021,116.873975708443,
116.991055657352,117.108249996379,117.225507405703,117.342983778858,117.40242381767,
117.519927421395,117.637214821166,117.754383132948,117.871482335835,117.988562296238,
118.105756646709,118.223014067466,118.340490451903,118.399930399632,118.51743395948,
118.634721315403,118.751889583392,118.868988742619,118.986068659578,119.10326296727,
119.220520345564,119.337996688525,119.397436981594,119.514940591803,119.632227997493,
119.74939631484,119.866495522933,119.983575488175,120.100769842902,120.218027267589,
120.335503655412,120.394943563556,120.512447240091,120.629734713282,120.7469030988,
120.864002375596,120.981082409943,121.098276833821,121.215534327787,121.333010784262,
121.392450145518,121.509946639959,121.627240956719,121.664501811606),
 .UNSPECIFIED.);
#809=B_SPLINE_CURVE_WITH_KNOTS('',3,(#73539,#73540,#73541,#73542,#73543,
#73544,#73545,#73546,#73547,#73548,#73549,#73550,#73551,#73552,#73553,#73554,
#73555,#73556,#73557,#73558,#73559,#73560,#73561,#73562,#73563,#73564,#73565,
#73566,#73567,#73568,#73569,#73570,#73571,#73572,#73573,#73574,#73575,#73576,
#73577,#73578,#73579,#73580,#73581,#73582,#73583,#73584,#73585,#73586,#73587,
#73588,#73589,#73590,#73591,#73592,#73593,#73594,#73595,#73596,#73597,#73598,
#73599,#73600,#73601,#73602,#73603,#73604,#73605,#73606,#73607,#73608,#73609,
#73610,#73611,#73612,#73613,#73614,#73615,#73616,#73617,#73618,#73619,#73620,
#73621,#73622,#73623,#73624,#73625,#73626,#73627,#73628,#73629,#73630,#73631,
#73632,#73633,#73634,#73635,#73636,#73637,#73638,#73639,#73640,#73641,#73642,
#73643,#73644,#73645,#73646,#73647,#73648,#73649,#73650,#73651,#73652,#73653,
#73654,#73655,#73656,#73657,#73658,#73659,#73660,#73661,#73662,#73663,#73664,
#73665,#73666,#73667,#73668,#73669,#73670,#73671,#73672,#73673,#73674,#73675,
#73676,#73677,#73678,#73679,#73680,#73681,#73682,#73683,#73684,#73685,#73686,
#73687,#73688,#73689,#73690,#73691,#73692,#73693,#73694,#73695,#73696,#73697,
#73698,#73699,#73700,#73701,#73702,#73703,#73704,#73705,#73706,#73707,#73708,
#73709,#73710,#73711,#73712,#73713,#73714,#73715,#73716),.UNSPECIFIED.,
 .F.,.F.,(4,2,2,2,2,2,2,2,2,2,2,2,2,2,2,2,2,2,2,2,2,2,2,2,2,2,2,2,2,2,2,
2,2,2,2,2,2,2,2,2,2,2,2,2,2,2,2,2,2,2,2,2,2,2,2,2,2,2,2,2,2,2,2,2,2,2,2,
2,2,2,2,2,2,2,2,2,2,2,2,2,2,2,2,2,2,2,2,2,4),(-0.693046076597336,-0.67984367033363,
-0.657314152795425,-0.650710899261982,-0.645398194889328,-0.64237851699963,
-0.639737645699231,-0.636430661683604,-0.631180142899999,-0.607317004738094,
-0.583659683272591,-0.579984035916418,-0.5781545758962,-0.576812305898406,
-0.574979657766784,-0.571326877153677,-0.568669832407123,-0.564004018590832,
-0.543649580028403,-0.522133931197164,-0.517337810503212,-0.514411653907558,
-0.511726202112982,-0.508181299774085,-0.500134417949507,-0.488553912624194,
-0.47402647844802,-0.455327241911143,-0.452308382772382,-0.450603032831665,
-0.449080856939599,-0.446943006495797,-0.441527973681299,-0.436941316139848,
-0.417217420032999,-0.394939896062259,-0.39016139982296,-0.38724141816417,
-0.384558816089793,-0.381013781139237,-0.372951530440752,-0.361344608985499,
-0.34675015436894,-0.327966938021777,-0.324947921403686,-0.323245627857243,
-0.321727506028327,-0.319599527645496,-0.314236176964177,-0.309709986991027,
-0.290449445942093,-0.269445252832055,-0.264191031941215,-0.260873983802779,
-0.258219522360854,-0.255177697464234,-0.249806411144251,-0.243116288392084,
-0.227434139712926,-0.202197602112536,-0.198582957905506,-0.196739843945332,
-0.195212367729667,-0.193536227487522,-0.190639190152574,-0.17599882191069,
-0.142967169524369,-0.136696940021199,-0.133468587600331,-0.130864095882273,
-0.127909473341464,-0.124774710473348,-0.112133632282807,-0.090175540155627,
-0.0731777383191034,-0.0701813756983897,-0.068483582301325,-0.0669627322876045,
-0.0648218228567381,-0.0593784514073219,-0.0575108321596313,-0.0516968829590682,
-0.0292266003357285,-0.0203116323057249,-0.010850371782216,-0.00707572352057534,
-0.0043886250177014,-0.00223372215546031,-0.000389518114393014),
 .UNSPECIFIED.);
#810=B_SPLINE_CURVE_WITH_KNOTS('',3,(#73717,#73718,#73719,#73720,#73721,
#73722,#73723,#73724,#73725,#73726,#73727,#73728,#73729,#73730,#73731,#73732,
#73733,#73734,#73735,#73736,#73737,#73738,#73739,#73740,#73741,#73742),
 .UNSPECIFIED.,.F.,.F.,(4,2,2,2,2,2,2,2,2,2,2,2,4),(-1.60432934360076,-1.6017175531892,
-1.59737603752716,-1.57573503141855,-1.55340729196558,-1.54803406782767,
-1.54590447709287,-1.54438628912393,-1.54268566933008,-1.53967125642436,
-1.52098345817347,-1.50653753337139,-1.49484735329919),.UNSPECIFIED.);
#811=B_SPLINE_CURVE_WITH_KNOTS('',3,(#73744,#73745,#73746,#73747,#73748,
#73749,#73750,#73751,#73752,#73753,#73754,#73755,#73756,#73757,#73758,#73759,
#73760,#73761,#73762,#73763,#73764,#73765,#73766,#73767,#73768),
 .UNSPECIFIED.,.F.,.F.,(4,3,3,3,3,3,3,3,4),(121.664501811606,121.781642468112,
121.898729879809,122.021536591726,122.138748597292,122.256040087996,122.373537832758,
122.38995672748,122.522113490002),.UNSPECIFIED.);
#812=B_SPLINE_CURVE_WITH_KNOTS('',3,(#73769,#73770,#73771,#73772,#73773,
#73774,#73775,#73776,#73777,#73778,#73779,#73780,#73781,#73782,#73783,#73784,
#73785,#73786,#73787,#73788,#73789,#73790,#73791,#73792,#73793,#73794,#73795,
#73796,#73797,#73798,#73799,#73800,#73801,#73802,#73803,#73804,#73805,#73806,
#73807,#73808,#73809,#73810,#73811,#73812,#73813,#73814,#73815,#73816,#73817,
#73818,#73819,#73820,#73821,#73822,#73823,#73824,#73825,#73826,#73827,#73828,
#73829,#73830,#73831,#73832,#73833,#73834,#73835,#73836,#73837,#73838,#73839,
#73840,#73841,#73842,#73843,#73844,#73845,#73846,#73847,#73848,#73849,#73850,
#73851,#73852,#73853,#73854,#73855,#73856,#73857,#73858,#73859,#73860,#73861,
#73862,#73863,#73864,#73865,#73866,#73867,#73868,#73869,#73870,#73871,#73872,
#73873,#73874,#73875,#73876,#73877,#73878,#73879,#73880,#73881,#73882,#73883,
#73884,#73885,#73886,#73887,#73888,#73889,#73890,#73891,#73892,#73893,#73894,
#73895,#73896,#73897,#73898,#73899,#73900,#73901,#73902,#73903,#73904,#73905,
#73906,#73907,#73908,#73909,#73910,#73911,#73912,#73913,#73914,#73915,#73916,
#73917,#73918,#73919,#73920,#73921,#73922,#73923,#73924,#73925,#73926,#73927,
#73928,#73929,#73930,#73931,#73932,#73933,#73934,#73935,#73936,#73937,#73938,
#73939,#73940,#73941,#73942,#73943,#73944),.UNSPECIFIED.,.F.,.F.,(4,2,2,
2,2,2,2,2,2,2,2,2,2,2,2,2,2,2,2,2,2,2,2,2,2,2,2,2,2,2,2,2,2,2,2,2,2,2,2,
2,2,2,2,2,2,2,2,2,2,2,2,2,2,2,2,2,2,2,2,2,2,2,2,2,2,2,2,2,2,2,2,2,2,2,2,
2,2,2,2,2,2,2,2,2,2,2,2,4),(0.693071669236789,0.698139480370448,0.701159145804299,
0.703549748828527,0.706767878550367,0.713019731837982,0.721193300910815,
0.744007185647916,0.760744345774809,0.763736737013293,0.765432136789302,
0.766951918442264,0.76909125399323,0.774526537050775,0.779140034139169,
0.799071535765026,0.82115054123654,0.825932508069584,0.828852336482292,
0.831533270601716,0.835073826443107,0.843115720755329,0.854682594518121,
0.86926813760988,0.88802725884411,0.89101038689015,0.892722152931211,0.894238006802906,
0.896348044187626,0.901589764195582,0.909634290722259,0.940249205308818,
0.94861430045093,0.953326133262378,0.956230627265531,0.958915444628075,
0.962487990685922,0.97073041562263,0.982715138785732,0.99327613972987,1.01404218243176,
1.01786618427992,1.01973164475163,1.0212270070191,1.02311312686503,1.02704593738579,
1.03245836805485,1.04798026679867,1.07405043982704,1.07924558177018,1.08254590067681,
1.08519974830861,1.08825492680061,1.09368877397592,1.10047962213288,1.11657082973311,
1.1418275443702,1.14533339886679,1.14715837449832,1.14850518700561,1.15035567698938,
1.15410208217629,1.16925486562512,1.19657645759496,1.20536281344284,1.20874555568777,
1.21123487604378,1.21395764252497,1.21776428684172,1.2275796837714,1.24319127644046,
1.26815672914931,1.2719479951072,1.27383431523484,1.27535716237261,1.27698857654572,
1.2794642809716,1.28262848955899,1.28919300781133,1.31196240089643,1.33064817936872,
1.33535100676426,1.33825327154474,1.34093821051274,1.34451420554197,1.3484685323124,
1.35535731767862,1.38572530886986),.UNSPECIFIED.);
#813=B_SPLINE_CURVE_WITH_KNOTS('',3,(#73948,#73949,#73950,#73951,#73952,
#73953,#73954,#73955,#73956,#73957,#73958,#73959,#73960,#73961,#73962,#73963,
#73964,#73965,#73966,#73967,#73968,#73969,#73970,#73971,#73972,#73973,#73974,
#73975,#73976,#73977,#73978,#73979,#73980,#73981,#73982,#73983,#73984,#73985,
#73986,#73987,#73988,#73989,#73990,#73991,#73992,#73993,#73994,#73995,#73996,
#73997,#73998,#73999,#74000,#74001,#74002,#74003,#74004,#74005,#74006,#74007,
#74008),.UNSPECIFIED.,.F.,.F.,(4,3,3,3,3,3,3,3,3,3,3,3,3,3,3,3,3,3,3,3,
4),(-4.04123713824992,-3.99002632784797,-3.88065880480044,-3.76964142243613,
-3.66057630191354,-3.55157904186602,-3.44260994457981,-3.33008739490635,
-3.22098672178644,-3.10675323383621,-2.99251974588598,-2.88328166339718,
-2.77224810096303,-2.66330470611944,-2.5544259875385,-2.4455720800857,-2.33293235104527,
-2.22393731289834,-2.10947523841116,-1.99501316392398,-1.98502202421803),
 .UNSPECIFIED.);
#814=B_SPLINE_CURVE_WITH_KNOTS('',3,(#74012,#74013,#74014,#74015,#74016),
 .UNSPECIFIED.,.F.,.F.,(4,1,4),(0.,0.997506581961993,1.08537753955764),
 .UNSPECIFIED.);
#815=B_SPLINE_CURVE_WITH_KNOTS('',3,(#74018,#74019,#74020,#74021,#74022,
#74023,#74024,#74025,#74026,#74027,#74028,#74029,#74030,#74031,#74032,#74033,
#74034,#74035,#74036,#74037,#74038,#74039,#74040,#74041,#74042,#74043,#74044,
#74045,#74046,#74047,#74048,#74049,#74050,#74051,#74052,#74053,#74054,#74055,
#74056,#74057,#74058,#74059,#74060,#74061,#74062,#74063,#74064,#74065,#74066,
#74067,#74068,#74069,#74070,#74071,#74072,#74073,#74074,#74075,#74076,#74077,
#74078,#74079,#74080,#74081,#74082,#74083,#74084,#74085,#74086,#74087,#74088,
#74089,#74090,#74091,#74092,#74093,#74094,#74095,#74096,#74097,#74098,#74099,
#74100,#74101,#74102,#74103,#74104,#74105,#74106,#74107,#74108,#74109,#74110,
#74111,#74112,#74113,#74114,#74115,#74116,#74117,#74118,#74119,#74120,#74121,
#74122,#74123,#74124,#74125,#74126,#74127,#74128,#74129,#74130,#74131,#74132,
#74133,#74134,#74135,#74136,#74137,#74138,#74139,#74140,#74141,#74142,#74143,
#74144,#74145,#74146,#74147,#74148,#74149,#74150,#74151,#74152,#74153,#74154,
#74155,#74156,#74157,#74158,#74159,#74160,#74161,#74162,#74163,#74164,#74165,
#74166,#74167,#74168,#74169,#74170,#74171,#74172,#74173,#74174,#74175,#74176,
#74177,#74178,#74179,#74180,#74181,#74182,#74183,#74184,#74185,#74186,#74187,
#74188,#74189,#74190,#74191,#74192,#74193,#74194,#74195),.UNSPECIFIED.,
 .F.,.F.,(4,3,3,3,3,3,3,3,3,3,3,3,3,3,3,3,3,3,3,3,3,3,3,3,3,3,3,3,3,3,3,
3,3,3,3,3,3,3,3,3,3,3,3,3,3,3,3,3,3,3,3,3,3,3,3,3,3,3,3,4),(1.08537753955764,
1.19237208039302,1.29918413117133,1.40589593993818,1.51255020384418,1.61918951761686,
1.72592914702087,1.83272395932984,1.93970883738257,1.99501316392399,2.10426582070635,
2.21529756135381,2.32424717166913,2.43312898501853,2.54198287098267,2.65461708970849,
2.76360437795769,2.87806206192184,2.99251974588598,3.10186876550467,3.21288846079758,
3.32194593157733,3.43093959586529,3.53990914493888,3.65243844066615,3.76154958654277,
3.87578795719537,3.99002632784798,4.09908565806964,4.21014156453718,4.31889683448837,
4.42758448166435,4.5362447001632,4.64906675257489,4.75786389897493,4.86673806894133,
4.97579377032075,4.98753290980997,5.09672274281777,5.20776233643704,5.31665180314716,
5.42547465207295,5.53427085876912,5.64696301701983,5.7558965477232,5.87046801974758,
5.98503949177196,6.09423082675942,6.20527023263123,6.31416227081442,6.4229880838998,
6.5317876437074,6.64447725121404,6.75341507275383,6.86798057324389,6.98254607373395,
7.10492809094954,7.2268464510175,7.34802169307296,7.36856284629668),
 .UNSPECIFIED.);
#816=B_SPLINE_CURVE_WITH_KNOTS('',3,(#74197,#74198,#74199,#74200,#74201,
#74202,#74203,#74204,#74205,#74206,#74207,#74208,#74209,#74210,#74211,#74212,
#74213,#74214,#74215,#74216,#74217,#74218,#74219,#74220,#74221,#74222,#74223,
#74224,#74225,#74226,#74227,#74228,#74229,#74230,#74231,#74232,#74233,#74234,
#74235,#74236,#74237,#74238,#74239,#74240,#74241,#74242,#74243,#74244,#74245,
#74246,#74247,#74248,#74249,#74250,#74251,#74252,#74253,#74254,#74255,#74256,
#74257,#74258,#74259,#74260,#74261,#74262,#74263,#74264,#74265,#74266,#74267,
#74268,#74269,#74270,#74271,#74272,#74273,#74274,#74275,#74276,#74277,#74278,
#74279,#74280,#74281,#74282,#74283,#74284,#74285,#74286,#74287,#74288,#74289,
#74290,#74291,#74292,#74293,#74294,#74295,#74296,#74297,#74298,#74299,#74300,
#74301,#74302,#74303,#74304,#74305,#74306,#74307,#74308,#74309,#74310,#74311,
#74312,#74313,#74314,#74315,#74316,#74317,#74318,#74319,#74320,#74321,#74322,
#74323,#74324,#74325,#74326,#74327,#74328,#74329,#74330,#74331,#74332,#74333,
#74334,#74335,#74336,#74337,#74338,#74339,#74340,#74341,#74342,#74343,#74344,
#74345,#74346,#74347,#74348,#74349,#74350,#74351,#74352,#74353,#74354,#74355,
#74356,#74357,#74358,#74359,#74360,#74361,#74362,#74363,#74364,#74365,#74366,
#74367,#74368,#74369,#74370,#74371),.UNSPECIFIED.,.F.,.F.,(4,3,3,3,3,3,
3,3,3,3,3,3,3,3,3,3,3,3,3,3,3,3,3,3,3,3,3,3,3,3,3,3,3,3,3,3,3,3,3,3,3,3,
3,3,3,3,3,3,3,3,3,3,3,3,3,3,3,3,4),(7.36856284673721,7.47844486294954,7.58835513743192,
7.69841751039424,7.8085631522594,7.91893214887187,7.98005265569595,8.08922828502025,
8.20026965409996,8.3091450252022,8.4179538590293,8.52673615478103,8.63944192550026,
8.74836197033257,8.86296060399525,8.97755923765794,9.08673359194986,9.19777512040862,
9.30664929434707,9.41545696352864,9.52423812919371,9.63694505180026,9.74586406663919,
9.86046494312956,9.97506581961993,10.0842364222147,10.1952784196356,10.3041486612738,
10.4129523417652,10.5217294688119,10.6344402020044,10.7433551001326,10.8579637508572,
10.9725724015819,11.0817453572512,11.1927870605378,11.3016597337144,11.4104658681936,
11.519245467665,11.6319538466347,11.7408712345231,11.8554751090335,11.9700789835439,
12.0792516006844,12.1902933462871,12.299165683508,12.4079714839463,12.5167507518537,
12.6294594552667,12.7383765217031,12.8529810436045,12.9675855655059,13.0763258634871,
13.1849044295828,13.2933621425984,13.4017517461816,13.5101030392779,13.6184871728317,
13.6517481539168),.UNSPECIFIED.);
#817=B_SPLINE_CURVE_WITH_KNOTS('',3,(#74373,#74374,#74375,#74376,#74377,
#74378,#74379,#74380,#74381,#74382,#74383,#74384,#74385,#74386,#74387,#74388,
#74389,#74390,#74391,#74392,#74393,#74394,#74395,#74396,#74397,#74398,#74399,
#74400,#74401,#74402,#74403,#74404,#74405,#74406,#74407,#74408,#74409,#74410,
#74411,#74412,#74413,#74414,#74415,#74416,#74417,#74418,#74419,#74420,#74421,
#74422,#74423,#74424,#74425,#74426,#74427,#74428,#74429,#74430,#74431,#74432,
#74433,#74434,#74435,#74436,#74437,#74438,#74439,#74440,#74441,#74442,#74443,
#74444,#74445,#74446,#74447,#74448,#74449,#74450,#74451,#74452,#74453,#74454,
#74455,#74456,#74457,#74458,#74459,#74460,#74461,#74462,#74463,#74464,#74465,
#74466,#74467,#74468,#74469,#74470,#74471,#74472,#74473,#74474,#74475,#74476,
#74477,#74478,#74479,#74480,#74481,#74482,#74483,#74484,#74485,#74486,#74487,
#74488,#74489,#74490,#74491,#74492,#74493,#74494,#74495,#74496,#74497,#74498,
#74499,#74500,#74501,#74502,#74503,#74504,#74505,#74506,#74507,#74508,#74509,
#74510,#74511,#74512,#74513,#74514,#74515,#74516,#74517,#74518,#74519,#74520,
#74521,#74522,#74523,#74524,#74525,#74526,#74527,#74528,#74529,#74530,#74531,
#74532,#74533,#74534,#74535,#74536,#74537,#74538,#74539,#74540,#74541,#74542,
#74543,#74544),.UNSPECIFIED.,.F.,.F.,(4,3,3,3,3,3,3,3,3,3,3,3,3,3,3,3,3,
3,3,3,3,3,3,3,3,3,3,3,3,3,3,3,3,3,3,3,3,3,3,3,3,3,3,3,3,3,3,3,3,3,3,3,3,
3,3,3,3,4),(13.6517481542948,13.7807998321804,13.9114792371605,13.9650921474679,
14.0742646640749,14.1853064222443,14.2941786486733,14.4029843347975,14.5117634850477,
14.6244722961433,14.7333892379024,14.8479939836662,14.9625987294299,15.0717711822896,
15.1828129484274,15.2916851105296,15.4004907322928,15.5092698182548,15.621978691539,
15.7308955699467,15.8455004406693,15.9601053113919,16.0692777228638,16.1803194941751,
16.2891916125174,16.3979971897579,16.5067762305057,16.6194851462177,16.7284019782044,
16.8430069357792,16.9576118933539,17.066784343201,17.1778261097154,17.2866982678641,
17.3955038853332,17.5042829666664,17.6169918438287,17.7259087168211,17.8405135960685,
17.9551184753159,18.0642909146953,18.1753326825181,18.2842048300158,18.3930104367955,
18.5017895074187,18.6144983948835,18.7234152572394,18.8380201572587,18.9526250572779,
19.0615109035367,19.1706887231708,19.2792768455527,19.3877990279444,19.4962957334554,
19.605955165244,19.7145896233196,19.8247615419647,19.9349334606099),
 .UNSPECIFIED.);
#818=B_SPLINE_CURVE_WITH_KNOTS('',3,(#74546,#74547,#74548,#74549,#74550,
#74551,#74552,#74553,#74554,#74555,#74556,#74557,#74558,#74559,#74560,#74561,
#74562,#74563,#74564,#74565,#74566,#74567,#74568,#74569,#74570,#74571,#74572,
#74573,#74574,#74575,#74576,#74577,#74578,#74579,#74580,#74581,#74582,#74583,
#74584,#74585,#74586,#74587,#74588,#74589,#74590,#74591,#74592,#74593,#74594,
#74595,#74596,#74597,#74598,#74599,#74600,#74601,#74602,#74603,#74604,#74605,
#74606,#74607,#74608,#74609,#74610,#74611,#74612,#74613,#74614,#74615,#74616,
#74617,#74618,#74619,#74620,#74621,#74622,#74623,#74624,#74625,#74626,#74627,
#74628,#74629,#74630,#74631,#74632,#74633,#74634,#74635,#74636,#74637,#74638,
#74639,#74640,#74641,#74642,#74643,#74644,#74645,#74646,#74647,#74648,#74649,
#74650,#74651,#74652,#74653,#74654,#74655,#74656,#74657,#74658,#74659,#74660,
#74661,#74662,#74663,#74664,#74665,#74666,#74667,#74668,#74669,#74670,#74671,
#74672,#74673,#74674,#74675,#74676,#74677,#74678,#74679,#74680,#74681,#74682,
#74683,#74684,#74685,#74686,#74687,#74688,#74689,#74690,#74691,#74692,#74693,
#74694,#74695,#74696,#74697,#74698,#74699,#74700,#74701,#74702,#74703,#74704,
#74705,#74706,#74707,#74708,#74709,#74710,#74711,#74712,#74713,#74714,#74715,
#74716,#74717,#74718,#74719,#74720),.UNSPECIFIED.,.F.,.F.,(4,3,3,3,3,3,
3,3,3,3,3,3,3,3,3,3,3,3,3,3,3,3,3,3,3,3,3,3,3,3,3,3,3,3,3,3,3,3,3,3,3,3,
3,3,3,3,3,3,3,3,3,3,3,3,3,3,3,3,4),(19.9349334610964,19.9501316392399,20.059304079444,
20.1703458471637,20.2792179954136,20.3880236029164,20.496802674232,20.6095115609745,
20.7184284239382,20.83303332257,20.9476382212018,21.0568106598144,21.167852427733,
21.2767245743552,21.3855301802213,21.494309249894,21.6070181382114,21.7159349995358,
21.8305399013498,21.9451448031638,22.0543172414554,22.1653590094142,22.2742311556886,
22.3830367611979,22.4918158305054,22.6045247191605,22.7134415801027,22.8280464826142,
22.9426513851258,23.0518238239892,23.1628655918765,23.2717377387463,23.3805433448581,
23.4893224147742,23.6020313028526,23.7109481644118,23.8255530657498,23.9401579670878,
24.0493304057212,24.1603721736373,24.269244320271,24.3780499261452,24.4868289958225,
24.5995378841293,24.7084547454493,24.8230596472496,24.9376645490498,25.0468369876651,
25.1578787555834,25.2667509021965,25.375556508049,25.4843355777038,25.5970444660308,
25.7059613273264,25.8205662291691,25.9351711310118,26.0766449493812,26.2101144995944,
26.2181187677507),.UNSPECIFIED.);
#819=B_SPLINE_CURVE_WITH_KNOTS('',3,(#74722,#74723,#74724,#74725,#74726,
#74727,#74728,#74729,#74730,#74731,#74732,#74733,#74734,#74735,#74736,#74737,
#74738,#74739,#74740,#74741,#74742,#74743,#74744,#74745,#74746,#74747,#74748,
#74749,#74750,#74751,#74752,#74753,#74754,#74755,#74756,#74757,#74758,#74759,
#74760,#74761,#74762,#74763,#74764,#74765,#74766,#74767,#74768,#74769,#74770,
#74771,#74772,#74773,#74774,#74775,#74776,#74777,#74778,#74779,#74780,#74781,
#74782,#74783,#74784,#74785,#74786,#74787,#74788,#74789,#74790,#74791,#74792,
#74793,#74794,#74795,#74796,#74797,#74798,#74799,#74800,#74801,#74802,#74803,
#74804,#74805,#74806,#74807,#74808,#74809,#74810,#74811,#74812,#74813,#74814,
#74815,#74816,#74817,#74818,#74819,#74820,#74821,#74822,#74823,#74824,#74825,
#74826,#74827,#74828,#74829,#74830,#74831,#74832,#74833,#74834,#74835,#74836,
#74837,#74838,#74839,#74840,#74841,#74842,#74843,#74844,#74845,#74846,#74847,
#74848,#74849,#74850,#74851,#74852,#74853,#74854,#74855,#74856,#74857,#74858,
#74859,#74860,#74861,#74862,#74863,#74864,#74865,#74866,#74867,#74868,#74869,
#74870,#74871,#74872,#74873,#74874,#74875,#74876,#74877,#74878,#74879,#74880,
#74881,#74882,#74883,#74884,#74885,#74886,#74887,#74888,#74889,#74890,#74891,
#74892,#74893,#74894,#74895,#74896),.UNSPECIFIED.,.F.,.F.,(4,3,3,3,3,3,
3,3,3,3,3,3,3,3,3,3,3,3,3,3,3,3,3,3,3,3,3,3,3,3,3,3,3,3,3,3,3,3,3,3,3,3,
3,3,3,3,3,3,3,3,3,3,3,3,3,3,3,3,4),(26.218118768276,26.3260897132672,26.4340090703127,
26.5419180814198,26.6499336004416,26.7580059949489,26.8662760152752,26.9326777129738,
27.0418501516244,27.1528919195383,27.2617640661886,27.3705696720791,27.4793487417723,
27.5920576300632,27.7009744913982,27.815579393167,27.9301842949358,28.0393567335869,
28.1503985015008,28.2592706481514,28.3680762540422,28.4768553237355,28.5895642120261,
28.6984810733612,28.8130859751295,28.9276908768978,29.0368633155567,29.1479050834696,
29.2567772301283,29.3655828360272,29.4743619057289,29.5870707940116,29.6959876553551,
29.8105925571075,29.9251974588598,30.0343698975143,30.1454116654277,30.2542838120819,
30.3630894179761,30.4718684876732,30.5845773759603,30.693494237299,30.8080991390604,
30.9227040408218,31.0318764794768,31.1429182473902,31.2517903940449,31.3605959999397,
31.4693750696373,31.5820839579239,31.6910008192631,31.8056057210235,31.9202106227838,
32.0315396882388,32.1426749812362,32.2536208585234,32.3644559905224,32.4752076844519,
32.5013040754555),.UNSPECIFIED.);
#820=B_SPLINE_CURVE_WITH_KNOTS('',3,(#74898,#74899,#74900,#74901,#74902,
#74903,#74904,#74905,#74906,#74907,#74908,#74909,#74910,#74911,#74912,#74913,
#74914,#74915,#74916,#74917,#74918,#74919,#74920,#74921,#74922,#74923,#74924,
#74925,#74926,#74927,#74928,#74929,#74930,#74931,#74932,#74933,#74934,#74935,
#74936,#74937,#74938,#74939,#74940,#74941,#74942,#74943,#74944,#74945,#74946,
#74947,#74948,#74949,#74950,#74951,#74952,#74953,#74954,#74955,#74956,#74957,
#74958,#74959,#74960,#74961,#74962,#74963,#74964,#74965,#74966,#74967,#74968,
#74969,#74970,#74971,#74972,#74973,#74974,#74975,#74976,#74977,#74978,#74979,
#74980,#74981,#74982,#74983,#74984,#74985,#74986,#74987,#74988,#74989,#74990,
#74991,#74992,#74993,#74994,#74995,#74996,#74997,#74998,#74999,#75000,#75001,
#75002,#75003,#75004,#75005,#75006,#75007,#75008,#75009,#75010,#75011,#75012,
#75013,#75014,#75015,#75016,#75017,#75018,#75019,#75020,#75021,#75022,#75023,
#75024,#75025,#75026,#75027,#75028,#75029,#75030,#75031,#75032,#75033,#75034,
#75035,#75036,#75037,#75038,#75039,#75040,#75041,#75042,#75043,#75044,#75045,
#75046,#75047,#75048,#75049,#75050,#75051,#75052,#75053,#75054,#75055,#75056,
#75057,#75058,#75059,#75060,#75061,#75062,#75063,#75064,#75065,#75066,#75067,
#75068,#75069,#75070,#75071,#75072),.UNSPECIFIED.,.F.,.F.,(4,3,3,3,3,3,
3,3,3,3,3,3,3,3,3,3,3,3,3,3,3,3,3,3,3,3,3,3,3,3,3,3,3,3,3,3,3,3,3,3,3,3,
3,3,3,3,3,3,3,3,3,3,3,3,3,3,3,3,4),(32.501304075825,32.6202820172976,32.7396425606215,
32.8595408410294,32.9177172047458,33.026889643401,33.1379314113144,33.2468035579693,
33.3556091638644,33.4643882335622,33.5770971218486,33.6860139831881,33.800618884948,
33.9152237867078,34.0243962253632,34.1354379932765,34.2443101399316,34.3531157458268,
34.4618948155248,34.574603703811,34.6835205651507,34.7981254669102,34.9127303686697,
35.0219028073251,35.1329445752384,35.2418167218935,35.3506223277888,35.4594013974868,
35.5721102857731,35.6810271471128,35.7956320488722,35.9102369506317,36.019409389287,
36.1304511572004,36.2393233038555,36.3481289097506,36.4569079794486,36.5696168677349,
36.6785337290746,36.7931386308341,36.9077435325937,37.0169159712491,37.1279577391624,
37.2368298858175,37.3456354917128,37.4544145614108,37.567123449697,37.6760403110367,
37.7906452127962,37.9052501145557,38.0151550230095,38.1226501109105,38.2300416406864,
38.3373717088353,38.449151127173,38.5565434348571,38.6639882702517,38.7715852654564,
38.7844893821862),.UNSPECIFIED.);
#821=B_SPLINE_CURVE_WITH_KNOTS('',3,(#75074,#75075,#75076,#75077,#75078,
#75079,#75080,#75081,#75082,#75083,#75084,#75085,#75086,#75087,#75088,#75089,
#75090,#75091,#75092,#75093,#75094,#75095,#75096,#75097,#75098,#75099,#75100,
#75101,#75102,#75103,#75104,#75105,#75106,#75107,#75108,#75109,#75110,#75111,
#75112,#75113,#75114,#75115,#75116,#75117,#75118,#75119,#75120,#75121,#75122,
#75123,#75124,#75125,#75126,#75127,#75128,#75129,#75130,#75131,#75132,#75133,
#75134,#75135,#75136,#75137,#75138,#75139,#75140,#75141,#75142,#75143,#75144,
#75145,#75146,#75147,#75148,#75149,#75150,#75151,#75152,#75153,#75154,#75155,
#75156,#75157,#75158,#75159,#75160,#75161,#75162,#75163,#75164,#75165,#75166,
#75167,#75168,#75169,#75170,#75171,#75172,#75173,#75174,#75175,#75176,#75177,
#75178,#75179,#75180,#75181,#75182,#75183,#75184,#75185,#75186,#75187,#75188,
#75189,#75190,#75191,#75192,#75193,#75194,#75195,#75196,#75197,#75198,#75199,
#75200,#75201,#75202,#75203,#75204,#75205,#75206,#75207,#75208,#75209,#75210,
#75211,#75212,#75213,#75214,#75215,#75216,#75217,#75218,#75219,#75220,#75221,
#75222,#75223,#75224,#75225,#75226,#75227,#75228,#75229,#75230,#75231,#75232,
#75233,#75234,#75235,#75236,#75237,#75238,#75239,#75240,#75241,#75242,#75243,
#75244,#75245),.UNSPECIFIED.,.F.,.F.,(4,3,3,3,3,3,3,3,3,3,3,3,3,3,3,3,3,
3,3,3,3,3,3,3,3,3,3,3,3,3,3,3,3,3,3,3,3,3,3,3,3,3,3,3,3,3,3,3,3,3,3,3,3,
3,3,3,3,4),(38.7844893826352,38.9027566965177,39.0119291351729,39.1229709030862,
39.2318430497411,39.3406486556361,39.4494277253338,39.5621366136203,39.6710534749597,
39.7856583767197,39.9002632784797,40.0094357171351,40.1204774850484,40.2293496317034,
40.3381552375986,40.4469343072967,40.5596431955829,40.6685600569226,40.7831649586822,
40.8977698604417,41.0069422990971,41.1179840670104,41.2268562136655,41.3356618195608,
41.4444408892588,41.557149777545,41.6660666388848,41.7806715406442,41.8952764424037,
42.0044488810591,42.1154906489724,42.2243627956275,42.3331684015227,42.4419474712208,
42.554656359507,42.6635732208467,42.7781781226062,42.8927830243657,43.001955463021,
43.1129972309344,43.2218693775894,43.3306749834846,43.4394540531826,43.5521629414689,
43.6610798028085,43.7756847045681,43.8902896063277,43.9994620449831,44.1105038128964,
44.2193759595516,44.3281815654469,44.4369606351449,44.5496695234311,44.6585863847709,
44.7731912865303,44.8877961882897,45.0529483136957,45.0676746898147),
 .UNSPECIFIED.);
#822=B_SPLINE_CURVE_WITH_KNOTS('',3,(#75247,#75248,#75249,#75250,#75251,
#75252,#75253,#75254,#75255,#75256,#75257,#75258,#75259,#75260,#75261,#75262,
#75263,#75264,#75265,#75266,#75267,#75268,#75269,#75270,#75271,#75272,#75273,
#75274,#75275,#75276,#75277,#75278,#75279,#75280,#75281,#75282,#75283,#75284,
#75285,#75286,#75287,#75288,#75289,#75290,#75291,#75292,#75293,#75294,#75295,
#75296,#75297,#75298,#75299,#75300,#75301,#75302,#75303,#75304,#75305,#75306,
#75307,#75308,#75309,#75310,#75311,#75312,#75313,#75314,#75315,#75316,#75317,
#75318,#75319,#75320,#75321,#75322,#75323,#75324,#75325,#75326,#75327,#75328,
#75329,#75330,#75331,#75332,#75333,#75334,#75335,#75336,#75337,#75338,#75339,
#75340,#75341,#75342,#75343,#75344,#75345,#75346,#75347,#75348,#75349,#75350,
#75351,#75352,#75353,#75354,#75355,#75356,#75357,#75358,#75359,#75360,#75361,
#75362,#75363,#75364,#75365,#75366,#75367,#75368,#75369,#75370,#75371,#75372,
#75373,#75374,#75375,#75376,#75377,#75378,#75379,#75380,#75381,#75382,#75383,
#75384,#75385,#75386,#75387,#75388,#75389,#75390,#75391,#75392,#75393,#75394,
#75395,#75396,#75397,#75398,#75399,#75400,#75401,#75402,#75403,#75404,#75405,
#75406,#75407,#75408,#75409,#75410,#75411,#75412,#75413,#75414,#75415,#75416,
#75417,#75418,#75419,#75420,#75421),.UNSPECIFIED.,.F.,.F.,(4,3,3,3,3,3,
3,3,3,3,3,3,3,3,3,3,3,3,3,3,3,3,3,3,3,3,3,3,3,3,3,3,3,3,3,3,3,3,3,3,3,3,
3,3,3,3,3,3,3,3,3,3,3,3,3,3,3,3,4),(45.0676746903426,45.1750415219094,45.2823049101596,
45.3895070927842,45.4966902086682,45.6039694274682,45.711299424467,45.8188205351401,
45.8853027702517,45.994475208907,46.1055169768203,46.2143891234754,46.3231947293705,
46.4319737990685,46.5446826873548,46.6535995486945,46.7682044504541,46.8828093522137,
46.9919817908691,47.1030235587824,47.2118957054375,47.3207013113326,47.4294803810306,
47.5421892693169,47.6511061306565,47.765711032416,47.8803159341756,47.989488372831,
48.1005301407443,48.2094022873994,48.3182078932946,48.4269869629926,48.5396958512789,
48.6486127126186,48.7632176143781,48.8778225161376,48.9869949547929,49.0980367227062,
49.2069088693613,49.3157144752566,49.4244935449546,49.5372024332409,49.6461192945806,
49.7607241963401,49.8753290980996,49.9845015367549,50.0955433046682,50.2044154513233,
50.3132210572187,50.4220001269168,50.534709015203,50.6436258765428,50.7582307783022,
50.8728356800616,50.9923417591862,51.1078495281233,51.2231187442687,51.3380919842859,
51.35085999656),.UNSPECIFIED.);
#823=B_SPLINE_CURVE_WITH_KNOTS('',3,(#75423,#75424,#75425,#75426,#75427,
#75428,#75429,#75430,#75431,#75432,#75433,#75434,#75435,#75436,#75437,#75438,
#75439,#75440,#75441,#75442,#75443,#75444,#75445,#75446,#75447,#75448,#75449,
#75450,#75451,#75452,#75453,#75454,#75455,#75456,#75457,#75458,#75459,#75460,
#75461,#75462,#75463,#75464,#75465,#75466,#75467,#75468,#75469,#75470,#75471,
#75472,#75473,#75474,#75475,#75476,#75477,#75478,#75479,#75480,#75481,#75482,
#75483,#75484,#75485,#75486,#75487,#75488,#75489,#75490,#75491,#75492,#75493,
#75494,#75495,#75496,#75497,#75498,#75499,#75500,#75501,#75502,#75503,#75504,
#75505,#75506,#75507,#75508,#75509,#75510,#75511,#75512,#75513,#75514,#75515,
#75516,#75517,#75518,#75519,#75520,#75521,#75522,#75523,#75524,#75525,#75526,
#75527,#75528,#75529,#75530,#75531,#75532,#75533,#75534,#75535,#75536,#75537,
#75538,#75539,#75540,#75541,#75542,#75543,#75544,#75545,#75546,#75547,#75548,
#75549,#75550,#75551,#75552,#75553,#75554,#75555,#75556,#75557,#75558,#75559,
#75560,#75561,#75562,#75563,#75564,#75565,#75566,#75567,#75568,#75569,#75570,
#75571,#75572,#75573,#75574,#75575,#75576,#75577,#75578,#75579,#75580,#75581,
#75582,#75583,#75584,#75585,#75586,#75587,#75588,#75589,#75590,#75591,#75592,
#75593,#75594,#75595,#75596,#75597),.UNSPECIFIED.,.F.,.F.,(4,3,3,3,3,3,
3,3,3,3,3,3,3,3,3,3,3,3,3,3,3,3,3,3,3,3,3,3,3,3,3,3,3,3,3,3,3,3,3,3,3,3,
3,3,3,3,3,3,3,3,3,3,3,3,3,3,3,3,4),(51.3508599969944,51.4638640035928,51.5771436363338,
51.6905694161473,51.8042913248099,51.8703422620236,51.9795147006789,52.0905564685923,
52.1994286152473,52.3082342211425,52.4170132908405,52.5297221791268,52.6386390404664,
52.753243942226,52.8678488439856,52.977021282641,53.0880630505543,53.1969351972094,
53.3057408031046,53.4145198728028,53.527228761089,53.6361456224286,53.7507505241881,
53.8653554259476,53.9745278646031,54.0855696325164,54.1944417791714,54.3032473850665,
54.4120264547646,54.5247353430508,54.6336522043904,54.74825710615,54.8628620079096,
54.9720344465651,55.0830762144784,55.1919483611336,55.3007539670289,55.4095330367269,
55.5222419250131,55.6311587863528,55.7457636881122,55.8603685898716,55.969541028527,
56.0805827964403,56.1894549430954,56.2982605489907,56.4070396186886,56.5197485069748,
56.6286653683146,56.7432702700741,56.8578751718336,56.9655412073146,57.0730567352133,
57.1804640188214,57.2878051514156,57.3951602707806,57.5025261982831,57.6099931887045,
57.6340453036562),.UNSPECIFIED.);
#824=B_SPLINE_CURVE_WITH_KNOTS('',3,(#75599,#75600,#75601,#75602,#75603,
#75604,#75605,#75606,#75607,#75608,#75609,#75610,#75611,#75612,#75613,#75614,
#75615,#75616,#75617,#75618,#75619,#75620,#75621,#75622,#75623,#75624,#75625,
#75626,#75627,#75628,#75629,#75630,#75631,#75632,#75633,#75634,#75635,#75636,
#75637,#75638,#75639,#75640,#75641,#75642,#75643,#75644,#75645,#75646,#75647,
#75648,#75649,#75650,#75651,#75652,#75653,#75654,#75655,#75656,#75657,#75658,
#75659,#75660,#75661,#75662,#75663,#75664,#75665,#75666,#75667,#75668,#75669,
#75670,#75671,#75672,#75673,#75674,#75675,#75676,#75677,#75678,#75679,#75680,
#75681,#75682,#75683,#75684,#75685,#75686,#75687,#75688,#75689,#75690,#75691,
#75692,#75693,#75694,#75695,#75696,#75697,#75698,#75699,#75700,#75701,#75702,
#75703,#75704,#75705,#75706,#75707,#75708,#75709,#75710,#75711,#75712,#75713,
#75714,#75715,#75716,#75717,#75718,#75719,#75720,#75721,#75722,#75723,#75724,
#75725,#75726,#75727,#75728,#75729,#75730,#75731,#75732,#75733,#75734,#75735,
#75736,#75737,#75738,#75739,#75740,#75741,#75742,#75743,#75744,#75745,#75746,
#75747,#75748,#75749,#75750,#75751,#75752,#75753,#75754,#75755,#75756,#75757,
#75758,#75759,#75760,#75761,#75762,#75763,#75764,#75765,#75766,#75767,#75768,
#75769,#75770),.UNSPECIFIED.,.F.,.F.,(4,3,3,3,3,3,3,3,3,3,3,3,3,3,3,3,3,
3,3,3,3,3,3,3,3,3,3,3,3,3,3,3,3,3,3,3,3,3,3,3,3,3,3,3,3,3,3,3,3,3,3,3,3,
3,3,3,3,4),(57.6340453041739,57.7828045081191,57.8553817537956,57.9645541924508,
58.0755959603642,58.1844681070192,58.2932737129144,58.4020527826123,58.5147616708987,
58.6236785322383,58.7382834339979,58.8528883357576,58.9620607744129,59.0731025423262,
59.1819746889812,59.2907802948764,59.3995593645744,59.5122682528606,59.6211851142003,
59.7357900159599,59.8503949177195,59.9595673563749,60.0706091242882,60.1794812709433,
60.2882868768386,60.3970659465366,60.5097748348228,60.6186916961625,60.733296597922,
60.8479014996815,60.9570739383369,61.0681157062502,61.1769878529053,61.2857934588005,
61.3945725284986,61.5072814167848,61.6161982781245,61.730803179884,61.8454080816435,
61.9545805202989,62.0656222882122,62.1744944348673,62.2833000407625,62.3920791104606,
62.5047879987468,62.6137048600865,62.728309761846,62.8429146636055,62.9520871022609,
63.0631288701742,63.1720010168293,63.2808066227245,63.3895856924226,63.5022945807089,
63.6112114420486,63.725816343808,63.8404212455675,63.9172306113535),
 .UNSPECIFIED.);
#825=B_SPLINE_CURVE_WITH_KNOTS('',3,(#75772,#75773,#75774,#75775,#75776,
#75777,#75778,#75779,#75780,#75781,#75782,#75783,#75784,#75785,#75786,#75787,
#75788,#75789,#75790,#75791,#75792,#75793,#75794,#75795,#75796,#75797,#75798,
#75799,#75800,#75801,#75802,#75803,#75804,#75805,#75806,#75807,#75808,#75809,
#75810,#75811,#75812,#75813,#75814,#75815,#75816,#75817,#75818,#75819,#75820,
#75821,#75822,#75823,#75824,#75825,#75826,#75827,#75828,#75829,#75830,#75831,
#75832,#75833,#75834,#75835,#75836,#75837,#75838,#75839,#75840,#75841,#75842,
#75843,#75844,#75845,#75846,#75847,#75848,#75849,#75850,#75851,#75852,#75853,
#75854,#75855,#75856,#75857,#75858,#75859,#75860,#75861,#75862,#75863,#75864,
#75865,#75866,#75867,#75868,#75869,#75870,#75871,#75872,#75873,#75874,#75875,
#75876,#75877,#75878,#75879,#75880,#75881,#75882,#75883,#75884,#75885,#75886,
#75887,#75888,#75889,#75890,#75891,#75892,#75893,#75894,#75895,#75896,#75897,
#75898,#75899,#75900,#75901,#75902,#75903,#75904,#75905,#75906,#75907,#75908,
#75909,#75910,#75911,#75912,#75913,#75914,#75915,#75916,#75917,#75918,#75919,
#75920,#75921,#75922,#75923,#75924,#75925,#75926,#75927,#75928,#75929,#75930,
#75931,#75932,#75933,#75934,#75935,#75936,#75937,#75938,#75939,#75940,#75941,
#75942,#75943),.UNSPECIFIED.,.F.,.F.,(4,3,3,3,3,3,3,3,3,3,3,3,3,3,3,3,3,
3,3,3,3,3,3,3,3,3,3,3,3,3,3,3,3,3,3,3,3,3,3,3,3,3,3,3,3,3,3,3,3,3,3,3,3,
3,3,3,3,4),(63.9172306117697,64.0252086767897,64.133012703545,64.2407214388638,
64.3483765813558,64.456019747366,64.5637655410965,64.6715675260603,64.7795605025846,
64.8379278275295,64.9471002661847,65.0581420340981,65.1670141807532,65.2758197866484,
65.3845988563465,65.4973077446327,65.6062246059724,65.720829507732,65.8354344094915,
65.9446068481468,66.0556486160601,66.1645207627152,66.2733263686105,66.3821054383085,
66.4948143265948,66.6037311879345,66.718336089694,66.8329409914535,66.9421134301088,
67.0531551980222,67.1620273446773,67.2708329505726,67.3796120202706,67.4923209085568,
67.6012377698965,67.715842671656,67.8304475734155,67.9396200120708,68.0506617799842,
68.1595339266392,68.2683395325344,68.3771186022324,68.4898274905187,68.5987443518583,
68.7133492536179,68.8279541553775,68.9371265940329,69.0481683619462,69.1570405086014,
69.2658461144964,69.3746251841943,69.4873340724806,69.5962509338203,69.7108558355799,
69.8254607373395,69.9489215589145,70.0746687384978,70.2004159180811),
 .UNSPECIFIED.);
#826=B_SPLINE_CURVE_WITH_KNOTS('',3,(#75945,#75946,#75947,#75948,#75949,
#75950,#75951,#75952,#75953,#75954,#75955,#75956,#75957,#75958,#75959,#75960,
#75961,#75962,#75963,#75964,#75965,#75966,#75967,#75968,#75969,#75970,#75971,
#75972,#75973,#75974,#75975,#75976,#75977,#75978,#75979,#75980,#75981,#75982,
#75983,#75984,#75985,#75986,#75987,#75988,#75989,#75990,#75991,#75992,#75993,
#75994,#75995,#75996,#75997,#75998,#75999,#76000,#76001,#76002,#76003,#76004,
#76005,#76006,#76007,#76008,#76009,#76010,#76011,#76012,#76013,#76014,#76015,
#76016,#76017,#76018,#76019,#76020,#76021,#76022,#76023,#76024,#76025,#76026,
#76027,#76028,#76029,#76030,#76031,#76032,#76033,#76034,#76035,#76036,#76037,
#76038,#76039,#76040,#76041,#76042,#76043,#76044,#76045,#76046,#76047,#76048,
#76049,#76050,#76051,#76052,#76053,#76054,#76055,#76056,#76057,#76058,#76059,
#76060,#76061,#76062,#76063,#76064,#76065,#76066,#76067,#76068,#76069,#76070,
#76071,#76072,#76073,#76074,#76075,#76076,#76077,#76078,#76079,#76080,#76081,
#76082,#76083,#76084,#76085,#76086,#76087,#76088,#76089,#76090,#76091,#76092,
#76093,#76094,#76095,#76096,#76097,#76098,#76099,#76100,#76101,#76102,#76103,
#76104,#76105,#76106,#76107,#76108,#76109,#76110,#76111,#76112,#76113,#76114,
#76115,#76116,#76117,#76118,#76119),.UNSPECIFIED.,.F.,.F.,(4,3,3,3,3,3,
3,3,3,3,3,3,3,3,3,3,3,3,3,3,3,3,3,3,3,3,3,3,3,3,3,3,3,3,3,3,3,3,3,3,3,3,
3,3,3,3,3,3,3,3,3,3,3,3,3,3,3,3,4),(70.2004159185332,70.3100324153458,70.4196665537124,
70.5294427104895,70.6392940861559,70.7493686748722,70.8229673193015,70.9321397579569,
71.0431815258702,71.1520536725254,71.2608592784206,71.3696383481187,71.4823472364049,
71.5912640977445,71.705868999504,71.8204739012635,71.9296463399186,72.040688107832,
72.149560254487,72.2583658603823,72.3671449300802,72.4798538183665,72.5887706797061,
72.7033755814658,72.8179804832255,72.9271529218808,73.0381946897941,73.1470668364492,
73.2558724423444,73.3646515120424,73.4773604003287,73.5862772616684,73.7008821634279,
73.8154870651875,73.924659503843,74.0357012717563,74.1445734184114,74.2533790243066,
74.3621580940044,74.4748669822907,74.5837838436304,74.6983887453899,74.8129936471494,
74.9221660858047,75.0332078537181,75.1420800003732,75.2508856062684,75.3596646759663,
75.4723735642526,75.5812904255922,75.6958953273518,75.8105002291114,75.9194429915219,
76.0282218606248,76.1420667018968,76.250645200874,76.3591846308122,76.4677479638505,
76.4836012257127),.UNSPECIFIED.);
#827=B_SPLINE_CURVE_WITH_KNOTS('',3,(#76121,#76122,#76123,#76124,#76125,
#76126,#76127,#76128,#76129,#76130,#76131,#76132,#76133,#76134,#76135,#76136,
#76137,#76138,#76139,#76140,#76141,#76142,#76143,#76144,#76145,#76146,#76147,
#76148,#76149,#76150,#76151,#76152,#76153,#76154,#76155,#76156,#76157,#76158,
#76159,#76160,#76161,#76162,#76163,#76164,#76165,#76166,#76167,#76168,#76169,
#76170,#76171,#76172,#76173,#76174,#76175,#76176,#76177,#76178,#76179,#76180,
#76181,#76182,#76183,#76184,#76185,#76186,#76187,#76188,#76189,#76190,#76191,
#76192,#76193,#76194,#76195,#76196,#76197,#76198,#76199,#76200,#76201,#76202,
#76203,#76204,#76205,#76206,#76207,#76208,#76209,#76210,#76211,#76212,#76213,
#76214,#76215,#76216,#76217,#76218,#76219,#76220,#76221,#76222,#76223,#76224,
#76225,#76226,#76227,#76228,#76229,#76230,#76231,#76232,#76233,#76234,#76235,
#76236,#76237,#76238,#76239,#76240,#76241,#76242,#76243,#76244,#76245,#76246,
#76247,#76248,#76249,#76250,#76251,#76252,#76253,#76254,#76255,#76256,#76257,
#76258,#76259,#76260,#76261,#76262,#76263,#76264,#76265,#76266,#76267,#76268,
#76269,#76270,#76271,#76272,#76273,#76274,#76275,#76276,#76277,#76278,#76279,
#76280,#76281,#76282,#76283,#76284,#76285,#76286,#76287,#76288,#76289,#76290,
#76291,#76292),.UNSPECIFIED.,.F.,.F.,(4,3,3,3,3,3,3,3,3,3,3,3,3,3,3,3,3,
3,3,3,3,3,3,3,3,3,3,3,3,3,3,3,3,3,3,3,3,3,3,3,3,3,3,3,3,3,3,3,3,3,3,3,3,
3,3,3,3,4),(76.4836012261201,76.6112555507849,76.740372532373,76.8080068110734,
76.9171792497287,77.028221017642,77.1370931642971,77.2458987701923,77.3546778398902,
77.4673867281765,77.5763035895162,77.6909084912758,77.8055133930354,77.9146858316908,
78.0257275996041,78.1345997462592,78.2434053521544,78.3521844218525,78.4648933101387,
78.5738101714784,78.6884150732379,78.8030199749974,78.9121924136527,79.0232341815661,
79.1321063282212,79.2409119341164,79.3496910038144,79.4623998921006,79.5713167534403,
79.6859216551999,79.8005265569594,79.9096989956147,80.0207407635281,80.1296129101831,
80.2384185160783,80.3471975857763,80.4599064740625,80.5688233354022,80.6834282371618,
80.7980331389214,80.9072055775768,81.0182473454901,81.1271194921453,81.2359250980405,
81.3447041677386,81.4574130560248,81.5663299173645,81.680934819124,81.7955397208834,
81.9042355427827,82.0127410724368,82.1211403939236,82.2294743442541,82.3377836693491,
82.4461876480963,82.5546348576525,82.6632882530645,82.7667865324968),
 .UNSPECIFIED.);
#828=B_SPLINE_CURVE_WITH_KNOTS('',3,(#76294,#76295,#76296,#76297,#76298,
#76299,#76300,#76301,#76302,#76303,#76304,#76305,#76306,#76307,#76308,#76309,
#76310,#76311,#76312,#76313,#76314,#76315,#76316,#76317,#76318,#76319,#76320,
#76321,#76322,#76323,#76324,#76325,#76326,#76327,#76328,#76329,#76330,#76331,
#76332,#76333,#76334,#76335,#76336,#76337,#76338,#76339,#76340,#76341,#76342,
#76343,#76344,#76345,#76346,#76347,#76348,#76349,#76350,#76351,#76352,#76353,
#76354,#76355,#76356,#76357,#76358,#76359,#76360,#76361,#76362,#76363,#76364,
#76365,#76366,#76367,#76368,#76369,#76370,#76371,#76372,#76373,#76374,#76375,
#76376,#76377,#76378,#76379,#76380,#76381,#76382,#76383,#76384,#76385,#76386,
#76387,#76388,#76389,#76390,#76391,#76392,#76393,#76394,#76395,#76396,#76397,
#76398,#76399,#76400,#76401,#76402,#76403,#76404,#76405,#76406,#76407,#76408,
#76409,#76410,#76411,#76412,#76413,#76414,#76415,#76416,#76417,#76418,#76419,
#76420,#76421,#76422,#76423,#76424,#76425,#76426,#76427,#76428,#76429,#76430,
#76431,#76432,#76433,#76434,#76435,#76436,#76437,#76438,#76439,#76440,#76441,
#76442,#76443,#76444,#76445,#76446,#76447,#76448,#76449,#76450,#76451,#76452,
#76453,#76454,#76455,#76456,#76457,#76458,#76459,#76460,#76461,#76462,#76463,
#76464,#76465),.UNSPECIFIED.,.F.,.F.,(4,3,3,3,3,3,3,3,3,3,3,3,3,3,3,3,3,
3,3,3,3,3,3,3,3,3,3,3,3,3,3,3,3,3,3,3,3,3,3,3,3,3,3,3,3,3,3,3,3,3,3,3,3,
3,3,3,3,4),(82.7667865328923,82.7930463028454,82.9022187415008,83.0132605094141,
83.1221326560692,83.2309382619644,83.3397173316625,83.4524262199487,83.5613430812884,
83.6759479830479,83.7905528848074,83.8997253234628,84.0107670913761,84.1196392380312,
84.2284448439264,84.3372239136245,84.4499328019107,84.5588496632504,84.6734545650099,
84.7880594667694,84.8972319054247,85.0082736733381,85.1171458199932,85.2259514258884,
85.3347304955864,85.4474393838727,85.5563562452124,85.6709611469719,85.7855660487314,
85.8947384873868,86.0057802553001,86.1146524019552,86.2234580078504,86.3322370775484,
86.4449459658347,86.5538628271744,86.6684677289339,86.7830726306934,86.8922450693488,
87.0032868372621,87.1121589839172,87.2209645898124,87.3297436595103,87.4424525477966,
87.5513694091363,87.6659743108958,87.7805792126554,87.8897516513109,88.0007934192242,
88.1096655658794,88.2184711717746,88.3272502414726,88.4399591297588,88.5488759910986,
88.663480892858,88.7780857946174,88.9147451508073,89.0499718396522),
 .UNSPECIFIED.);
#829=B_SPLINE_CURVE_WITH_KNOTS('',3,(#76467,#76468,#76469,#76470,#76471,
#76472,#76473,#76474,#76475,#76476,#76477,#76478,#76479,#76480,#76481,#76482,
#76483,#76484,#76485,#76486,#76487,#76488,#76489,#76490,#76491,#76492,#76493,
#76494,#76495,#76496,#76497,#76498,#76499,#76500,#76501,#76502,#76503,#76504,
#76505,#76506,#76507,#76508,#76509,#76510,#76511,#76512,#76513,#76514,#76515,
#76516,#76517,#76518,#76519,#76520,#76521,#76522,#76523,#76524,#76525,#76526,
#76527,#76528,#76529,#76530,#76531,#76532,#76533,#76534,#76535,#76536,#76537,
#76538,#76539,#76540,#76541,#76542,#76543,#76544,#76545,#76546,#76547,#76548,
#76549,#76550,#76551,#76552,#76553,#76554,#76555,#76556,#76557,#76558,#76559,
#76560,#76561,#76562,#76563,#76564,#76565,#76566,#76567,#76568,#76569,#76570,
#76571,#76572,#76573,#76574,#76575,#76576,#76577,#76578,#76579,#76580,#76581,
#76582,#76583,#76584,#76585,#76586,#76587,#76588,#76589,#76590,#76591,#76592,
#76593,#76594,#76595,#76596,#76597,#76598,#76599,#76600,#76601,#76602,#76603,
#76604,#76605,#76606,#76607,#76608,#76609,#76610,#76611,#76612,#76613,#76614,
#76615,#76616,#76617,#76618,#76619,#76620,#76621,#76622,#76623,#76624,#76625,
#76626,#76627,#76628,#76629,#76630,#76631,#76632,#76633,#76634,#76635,#76636,
#76637,#76638),.UNSPECIFIED.,.F.,.F.,(4,3,3,3,3,3,3,3,3,3,3,3,3,3,3,3,3,
3,3,3,3,3,3,3,3,3,3,3,3,3,3,3,3,3,3,3,3,3,3,3,3,3,3,3,3,3,3,3,3,3,3,3,3,
3,3,3,3,4),(89.0499718400719,89.1578186100854,89.2656072096612,89.3733790748927,
89.4812520864616,89.5891766087315,89.6973011055592,89.7755923765794,89.8847648152346,
89.9958065831479,90.1046787298029,90.213484335698,90.3222634053958,90.4349722936822,
90.5438891550218,90.6584940567815,90.7730989585413,90.8822713971971,90.9933131651104,
91.1021853117659,91.2109909176616,91.3197699873602,91.432478875646,91.5413957369861,
91.6560006387447,91.7706055405033,91.8797779791581,91.9908197470715,92.0996918937262,
92.2084974996209,92.3172765693185,92.4299854576052,92.5389023189444,92.6535072207049,
92.7681121224653,92.8772845611197,92.9883263290332,93.0971984756875,93.2060040815818,
93.314783151279,93.4274920395661,93.5364089009049,93.6510138026661,93.7656187044273,
93.8747911430863,93.9858329109992,94.094705057658,94.2035106635569,94.3122897332586,
94.4249986215413,94.5339154828846,94.6485203846369,94.7631252863893,94.8748360662789,
94.989416336522,95.1007236987982,95.2169404230248,95.3331571472515),
 .UNSPECIFIED.);
#830=B_SPLINE_CURVE_WITH_KNOTS('',3,(#76640,#76641,#76642,#76643,#76644,
#76645,#76646,#76647,#76648,#76649,#76650,#76651,#76652,#76653,#76654,#76655,
#76656,#76657,#76658,#76659,#76660,#76661,#76662,#76663,#76664,#76665,#76666,
#76667,#76668,#76669,#76670,#76671,#76672,#76673,#76674,#76675,#76676,#76677,
#76678,#76679,#76680,#76681,#76682,#76683,#76684,#76685,#76686,#76687,#76688,
#76689,#76690,#76691,#76692,#76693,#76694,#76695,#76696,#76697,#76698,#76699,
#76700,#76701,#76702,#76703,#76704,#76705,#76706,#76707,#76708,#76709,#76710,
#76711,#76712,#76713,#76714,#76715,#76716,#76717,#76718,#76719,#76720,#76721,
#76722,#76723,#76724,#76725,#76726,#76727,#76728,#76729,#76730,#76731,#76732,
#76733,#76734,#76735,#76736,#76737,#76738,#76739,#76740,#76741,#76742,#76743,
#76744,#76745,#76746,#76747,#76748,#76749,#76750,#76751,#76752,#76753,#76754,
#76755,#76756,#76757,#76758,#76759,#76760,#76761,#76762,#76763,#76764,#76765,
#76766,#76767,#76768,#76769,#76770,#76771,#76772,#76773,#76774,#76775,#76776,
#76777,#76778,#76779,#76780,#76781,#76782,#76783,#76784,#76785,#76786,#76787,
#76788,#76789,#76790,#76791,#76792,#76793,#76794,#76795,#76796,#76797,#76798,
#76799,#76800,#76801,#76802,#76803,#76804,#76805,#76806,#76807,#76808,#76809,
#76810,#76811),.UNSPECIFIED.,.F.,.F.,(4,3,3,3,3,3,3,3,3,3,3,3,3,3,3,3,3,
3,3,3,3,3,3,3,3,3,3,3,3,3,3,3,3,3,3,3,3,3,3,3,3,3,3,3,3,3,3,3,3,3,3,3,3,
3,3,3,3,4),(95.3331571475866,95.4513555745942,95.5698952158399,95.6889447197994,
95.7606318683513,95.8698043070021,95.980846074916,96.0897182215664,96.1985238274569,
96.3073028971503,96.420011785441,96.5289286467759,96.6435335485446,96.7581384503133,
96.8673108889975,96.9783526569072,97.0872248035911,97.1960304095152,97.3048094792419,
97.4175183675002,97.526435228868,97.6410401305717,97.7556450322753,97.8648174708862,
97.9758592388051,98.0847313854162,98.1935369912679,98.3023160609226,98.4150249492513,
98.5239418105492,98.6385467123932,98.7531516142373,98.8623240528741,98.9733658207898,
99.082237967425,99.1910435732999,99.2998226429772,99.4125315312828,99.521448392601,
99.6360532944001,99.7506581961993,99.8598306350725,99.9708724029585,100.079744549832,
100.188550155946,100.297329225862,100.410038113937,100.51895497549,100.633559876826,
100.748164778161,100.856686987641,100.964128213411,101.071465293244,101.178740384828,
101.28814090212,101.39547392521,101.505908189604,101.616342453998),
 .UNSPECIFIED.);
#831=B_SPLINE_CURVE_WITH_KNOTS('',3,(#76813,#76814,#76815,#76816,#76817,
#76818,#76819,#76820,#76821,#76822,#76823,#76824,#76825,#76826,#76827,#76828,
#76829,#76830,#76831,#76832,#76833,#76834,#76835,#76836,#76837,#76838,#76839,
#76840,#76841,#76842,#76843,#76844,#76845,#76846,#76847,#76848,#76849,#76850,
#76851,#76852,#76853,#76854,#76855,#76856,#76857,#76858,#76859,#76860,#76861,
#76862,#76863,#76864,#76865,#76866,#76867,#76868,#76869,#76870,#76871,#76872,
#76873,#76874,#76875,#76876,#76877,#76878,#76879,#76880,#76881,#76882,#76883,
#76884,#76885,#76886,#76887,#76888,#76889,#76890,#76891,#76892,#76893,#76894,
#76895,#76896,#76897,#76898,#76899,#76900,#76901,#76902,#76903,#76904,#76905,
#76906,#76907,#76908,#76909,#76910,#76911,#76912,#76913,#76914,#76915,#76916,
#76917,#76918,#76919,#76920,#76921,#76922,#76923,#76924,#76925,#76926,#76927,
#76928,#76929,#76930,#76931,#76932,#76933,#76934,#76935,#76936,#76937,#76938,
#76939,#76940,#76941,#76942,#76943,#76944,#76945,#76946,#76947,#76948,#76949,
#76950,#76951,#76952,#76953,#76954,#76955,#76956,#76957,#76958,#76959,#76960,
#76961,#76962,#76963,#76964,#76965,#76966,#76967,#76968,#76969,#76970,#76971,
#76972,#76973,#76974,#76975,#76976,#76977,#76978,#76979,#76980,#76981),
 .UNSPECIFIED.,.F.,.F.,(4,3,3,3,3,3,3,3,3,3,3,3,3,3,3,3,3,3,3,3,3,3,3,3,
3,3,3,3,3,3,3,3,3,3,3,3,3,3,3,3,3,3,3,3,3,3,3,3,3,3,3,3,3,3,3,3,4),(101.616342454431,
101.745671360123,101.854843798772,101.965885566686,102.074757713323,102.183563319196,
102.292342388868,102.405051277172,102.513968138477,102.628573040281,102.743177942085,
102.852350382351,102.963392150063,103.072264298338,103.181069905853,103.289848977168,
103.402557863888,103.511474726817,103.626079625432,103.740684524047,103.849856959235,
103.960898727582,104.069770870792,104.178576473261,104.287355539555,104.400064431169,
104.508981289201,104.623586197605,104.738191106009,104.847363545745,104.958405313523,
105.067277461168,105.176083068018,105.284862138634,105.397571025968,105.506487888124,
105.621092788048,105.735697687971,105.844870138156,105.955911904628,106.064784062917,
106.173589680453,106.282368761779,106.395077638818,106.50399451162,106.618599390777,
106.733204269933,106.842376679246,106.953418450827,107.062290568273,107.171096145088,
107.279875185881,107.392584102385,107.501500935583,107.616105893739,107.730710851895,
107.899527761611),.UNSPECIFIED.);
#832=B_SPLINE_CURVE_WITH_KNOTS('',3,(#76983,#76984,#76985,#76986,#76987,
#76988,#76989,#76990,#76991,#76992,#76993,#76994,#76995,#76996,#76997,#76998,
#76999,#77000,#77001,#77002,#77003,#77004,#77005,#77006,#77007,#77008,#77009,
#77010,#77011,#77012,#77013,#77014,#77015,#77016,#77017,#77018,#77019,#77020,
#77021,#77022,#77023,#77024,#77025,#77026,#77027,#77028,#77029,#77030,#77031,
#77032,#77033,#77034,#77035,#77036,#77037,#77038,#77039,#77040,#77041,#77042,
#77043,#77044,#77045,#77046,#77047,#77048,#77049,#77050,#77051,#77052,#77053,
#77054,#77055,#77056,#77057,#77058,#77059,#77060,#77061,#77062,#77063,#77064,
#77065,#77066,#77067,#77068,#77069,#77070,#77071,#77072,#77073,#77074,#77075,
#77076,#77077,#77078,#77079,#77080,#77081,#77082,#77083,#77084,#77085,#77086,
#77087,#77088,#77089,#77090,#77091,#77092,#77093,#77094,#77095,#77096,#77097,
#77098,#77099,#77100,#77101,#77102,#77103,#77104,#77105,#77106,#77107,#77108,
#77109,#77110,#77111,#77112,#77113,#77114,#77115,#77116,#77117,#77118,#77119,
#77120,#77121,#77122,#77123,#77124,#77125,#77126,#77127,#77128,#77129,#77130,
#77131,#77132,#77133,#77134,#77135,#77136,#77137,#77138,#77139,#77140,#77141,
#77142,#77143,#77144,#77145,#77146,#77147,#77148,#77149,#77150,#77151,#77152,
#77153,#77154),.UNSPECIFIED.,.F.,.F.,(4,3,3,3,3,3,3,3,3,3,3,3,3,3,3,3,3,
3,3,3,3,3,3,3,3,3,3,3,3,3,3,3,3,3,3,3,3,3,3,3,3,3,3,3,3,3,3,3,3,3,3,3,3,
3,3,3,3,4),(107.899527761921,108.006900864593,108.114166062461,108.221365614772,
108.328541675354,108.435810646325,108.543126437004,108.650636673681,108.728217433857,
108.837389951873,108.948431709866,109.05730393688,109.166109623282,109.274888773503,
109.387597584082,109.49651452505,109.611119270435,109.725724015819,109.834896212092,
109.945938010303,110.054809915234,110.16361528031,110.272394110473,110.3851032323,
110.494019860034,110.608625228907,110.723230597781,110.83240324485,110.943444986712,
111.052317336357,111.161123142689,111.269902409969,111.382611102413,111.491528152047,
111.606132665895,111.720737179743,111.82991013605,111.940951839257,112.049824512698,
112.158630647303,112.267410246761,112.380118625497,112.489036013027,112.603639887366,
112.718243761705,112.827414243178,112.938456255739,113.047326447098,113.156130103738,
113.264907233319,113.377618010906,113.486532977032,113.60114166035,113.715750343667,
113.832491024865,113.948637158773,114.065675113617,114.182713068461),
 .UNSPECIFIED.);
#833=B_SPLINE_CURVE_WITH_KNOTS('',3,(#77156,#77157,#77158,#77159,#77160,
#77161,#77162,#77163,#77164,#77165,#77166,#77167,#77168,#77169,#77170,#77171,
#77172,#77173,#77174,#77175,#77176,#77177,#77178,#77179,#77180,#77181,#77182,
#77183,#77184,#77185,#77186,#77187,#77188,#77189,#77190,#77191,#77192,#77193,
#77194,#77195,#77196,#77197,#77198,#77199,#77200,#77201,#77202,#77203,#77204,
#77205,#77206,#77207,#77208,#77209,#77210,#77211,#77212,#77213,#77214,#77215,
#77216,#77217,#77218,#77219,#77220,#77221,#77222,#77223,#77224,#77225,#77226,
#77227,#77228,#77229,#77230,#77231,#77232,#77233,#77234,#77235,#77236,#77237,
#77238,#77239,#77240,#77241,#77242,#77243,#77244,#77245,#77246,#77247,#77248,
#77249,#77250,#77251,#77252,#77253,#77254,#77255,#77256,#77257,#77258,#77259,
#77260,#77261,#77262,#77263,#77264,#77265,#77266,#77267,#77268,#77269,#77270,
#77271,#77272,#77273,#77274,#77275,#77276,#77277,#77278,#77279,#77280,#77281,
#77282,#77283,#77284,#77285,#77286,#77287,#77288,#77289,#77290,#77291,#77292,
#77293,#77294,#77295,#77296,#77297,#77298,#77299,#77300,#77301,#77302,#77303,
#77304,#77305,#77306,#77307,#77308,#77309,#77310,#77311,#77312,#77313,#77314,
#77315,#77316,#77317,#77318,#77319,#77320,#77321,#77322,#77323,#77324,#77325,
#77326,#77327,#77328,#77329,#77330),.UNSPECIFIED.,.F.,.F.,(4,3,3,3,3,3,
3,3,3,3,3,3,3,3,3,3,3,3,3,3,3,3,3,3,3,3,3,3,3,3,3,3,3,3,3,3,3,3,3,3,3,3,
3,3,3,3,3,3,3,3,3,3,3,3,3,3,3,3,4),(114.18271306879,114.295259121202,114.40805768734,
114.520987722838,114.634207955653,114.713256925629,114.822432474766,114.933473853869,
115.042349191685,115.151158009723,115.259940307156,115.372646107264,115.481566197116,
115.596164852353,115.710763507591,115.819920495038,115.930964194352,116.039820877543,
116.148611057667,116.257374763845,116.370098595272,116.479000423707,116.59363525663,
116.708270089553,116.817463632358,116.928502762252,117.037395716857,117.14622196453,
117.255021477854,117.367710276269,117.476646858088,117.591211764801,117.705776671515,
117.814965193221,117.926004950753,118.03489387316,118.143716463952,118.252512698232,
118.365205337043,118.47413960404,118.588711428758,118.703283253477,118.8123366592,
118.92339330623,119.032146115717,119.140832593708,119.249492932242,119.362317158041,
119.471117626952,119.579996228259,119.689057881339,119.700789835439,119.808769052271,
119.916596187234,120.024313170425,120.134709471811,120.242364817779,120.354131596875,
120.46589837597),.UNSPECIFIED.);
#834=B_SPLINE_CURVE_WITH_KNOTS('',3,(#77332,#77333,#77334,#77335,#77336,
#77337,#77338,#77339,#77340,#77341,#77342,#77343,#77344,#77345,#77346,#77347,
#77348,#77349,#77350,#77351,#77352,#77353,#77354,#77355,#77356,#77357,#77358,
#77359,#77360,#77361,#77362,#77363,#77364,#77365,#77366,#77367,#77368),
 .UNSPECIFIED.,.F.,.F.,(4,3,3,3,3,3,3,3,3,3,3,3,4),(120.465898376338,120.611331523754,
120.698296417401,120.80753478414,120.918568311043,121.027511991089,121.136390994414,
121.245245185674,121.357884639096,121.466879955347,121.581341477355,121.695802999363,
121.705794139069),.UNSPECIFIED.);
#835=B_SPLINE_CURVE_WITH_KNOTS('',3,(#77372,#77373,#77374,#77375,#77376,
#77377,#77378),.UNSPECIFIED.,.F.,.F.,(4,3,4),(-123.690816163287,-123.552129947919,
-123.421758301599),.UNSPECIFIED.);
#836=B_SPLINE_CURVE_WITH_KNOTS('',3,(#77380,#77381,#77382,#77383,#77384,
#77385,#77386,#77387,#77388,#77389),.UNSPECIFIED.,.F.,.F.,(4,1,1,1,1,1,
1,4),(-123.421757974662,-122.693309581325,-121.695802999363,-120.698296417401,
-119.700789835439,-118.703283253477,-117.705776671515,-117.138572667483),
 .UNSPECIFIED.);
#837=B_SPLINE_CURVE_WITH_KNOTS('',3,(#77391,#77392,#77393,#77394,#77395,
#77396,#77397,#77398,#77399,#77400,#77401,#77402,#77403,#77404,#77405,#77406,
#77407,#77408,#77409,#77410,#77411,#77412,#77413,#77414,#77415,#77416,#77417,
#77418,#77419,#77420,#77421,#77422,#77423,#77424,#77425,#77426,#77427,#77428,
#77429,#77430,#77431,#77432,#77433,#77434,#77435,#77436,#77437,#77438,#77439,
#77440,#77441,#77442,#77443,#77444,#77445,#77446,#77447,#77448,#77449,#77450,
#77451,#77452,#77453,#77454,#77455,#77456,#77457,#77458,#77459,#77460,#77461,
#77462,#77463,#77464,#77465,#77466,#77467,#77468,#77469,#77470,#77471,#77472,
#77473,#77474,#77475,#77476,#77477,#77478,#77479,#77480,#77481,#77482,#77483,
#77484,#77485,#77486,#77487,#77488,#77489,#77490,#77491,#77492,#77493,#77494,
#77495,#77496,#77497,#77498,#77499,#77500,#77501,#77502,#77503,#77504,#77505,
#77506,#77507,#77508,#77509,#77510,#77511,#77512,#77513,#77514,#77515,#77516,
#77517,#77518,#77519,#77520,#77521,#77522,#77523,#77524,#77525,#77526,#77527,
#77528,#77529,#77530,#77531,#77532,#77533,#77534,#77535,#77536,#77537,#77538,
#77539,#77540,#77541,#77542,#77543,#77544,#77545,#77546,#77547,#77548,#77549,
#77550,#77551,#77552,#77553,#77554,#77555,#77556,#77557,#77558,#77559,#77560,
#77561,#77562),.UNSPECIFIED.,.F.,.F.,(4,3,3,3,3,3,3,3,3,3,3,3,3,3,3,3,3,
3,3,3,3,3,3,3,3,3,3,3,3,3,3,3,3,3,3,3,3,3,3,3,3,3,3,3,3,3,3,3,3,3,3,3,3,
3,3,3,3,4),(-117.138572329772,-117.020515175888,-116.902124778381,-116.783229707864,
-116.708270089553,-116.599112217178,-116.488068628479,-116.379211566519,
-116.270421196485,-116.161657488991,-116.048933993641,-115.940032632066,
-115.825398069829,-115.710763507591,-115.601587885419,-115.490546515445,
-115.381671151657,-115.272862325182,-115.164080036811,-115.051374259016,
-114.942454221547,-114.827855573588,-114.713256925629,-114.604082572887,
-114.493041044235,-114.384166871964,-114.27535920449,-114.166578040568,
-114.053871116343,-113.944952103319,-113.830351223493,-113.715750343667,
-113.606579738047,-113.495537741004,-113.386667496225,-113.277863812558,
-113.169086682307,-113.056375952157,-112.947461050788,-112.832852406246,
-112.718243761705,-112.609070807295,-112.498029103851,-112.389156431964,
-112.280350298782,-112.171570700614,-112.058862320396,-111.94994493381,
-111.835341056776,-111.720737179743,-111.612568452366,-111.505138681501,
-111.397813214992,-111.290549882046,-111.181759251717,-111.074439119888,
-110.964913240309,-110.85538736073),.UNSPECIFIED.);
#838=B_SPLINE_CURVE_WITH_KNOTS('',3,(#77564,#77565,#77566,#77567,#77568,
#77569,#77570,#77571,#77572,#77573,#77574,#77575,#77576,#77577,#77578,#77579,
#77580,#77581,#77582,#77583,#77584,#77585,#77586,#77587,#77588,#77589,#77590,
#77591,#77592,#77593,#77594,#77595,#77596,#77597,#77598,#77599,#77600,#77601,
#77602,#77603,#77604,#77605,#77606,#77607,#77608,#77609,#77610,#77611,#77612,
#77613,#77614,#77615,#77616,#77617,#77618,#77619,#77620,#77621,#77622,#77623,
#77624,#77625,#77626,#77627,#77628,#77629,#77630,#77631,#77632,#77633,#77634,
#77635,#77636,#77637,#77638,#77639,#77640,#77641,#77642,#77643,#77644,#77645,
#77646,#77647,#77648,#77649,#77650,#77651,#77652,#77653,#77654,#77655,#77656,
#77657,#77658,#77659,#77660,#77661,#77662,#77663,#77664,#77665,#77666,#77667,
#77668,#77669,#77670,#77671,#77672,#77673,#77674,#77675,#77676,#77677,#77678,
#77679,#77680,#77681,#77682,#77683,#77684,#77685,#77686,#77687,#77688,#77689,
#77690,#77691,#77692,#77693,#77694,#77695,#77696,#77697,#77698,#77699,#77700,
#77701,#77702,#77703,#77704,#77705,#77706,#77707,#77708,#77709,#77710,#77711,
#77712,#77713,#77714,#77715,#77716,#77717,#77718,#77719,#77720,#77721,#77722,
#77723,#77724,#77725,#77726,#77727,#77728,#77729,#77730,#77731,#77732),
 .UNSPECIFIED.,.F.,.F.,(4,3,3,3,3,3,3,3,3,3,3,3,3,3,3,3,3,3,3,3,3,3,3,3,
3,3,3,3,3,3,3,3,3,3,3,3,3,3,3,3,3,3,3,3,3,3,3,3,3,3,3,3,3,3,3,3,4),(-110.855387360303,
-110.723230597781,-110.614058384659,-110.503016588554,-110.394144676341,
-110.285339307555,-110.176560477246,-110.06385136189,-109.954934742862,
-109.84032937934,-109.725724015819,-109.616551499424,-109.505509741228,
-109.396637515017,-109.287831829112,-109.179052679082,-109.066343867775,
-108.957426926237,-108.842822180047,-108.728217433857,-108.619044981008,
-108.508003214869,-108.399131052779,-108.29032543103,-108.181546345082,
-108.068837471785,-107.959920593393,-107.845315722644,-107.730710851895,
-107.621538440357,-107.510496669054,-107.401624550643,-107.292818973334,
-107.184039932516,-107.07133101687,-106.962414184812,-106.847809227373,
-106.733204269933,-106.62403182012,-106.512990053601,-106.404117895488,
-106.295312278054,-106.186533196756,-106.07382431956,-105.964907446603,
-105.850302567287,-105.735697687971,-105.626525248591,-105.515483480768,
-105.40661133327,-105.297805726489,-105.189026655866,-105.076317768402,
-104.967400906045,-104.852796006027,-104.738191106009,-104.572202053123),
 .UNSPECIFIED.);
#839=B_SPLINE_CURVE_WITH_KNOTS('',3,(#77734,#77735,#77736,#77737,#77738,
#77739,#77740,#77741,#77742,#77743,#77744,#77745,#77746,#77747,#77748,#77749,
#77750,#77751,#77752,#77753,#77754,#77755,#77756,#77757,#77758,#77759,#77760,
#77761,#77762,#77763,#77764,#77765,#77766,#77767,#77768,#77769,#77770,#77771,
#77772,#77773,#77774,#77775,#77776,#77777,#77778,#77779,#77780,#77781,#77782,
#77783,#77784,#77785,#77786,#77787,#77788,#77789,#77790,#77791,#77792,#77793,
#77794,#77795,#77796,#77797,#77798,#77799,#77800,#77801,#77802,#77803,#77804,
#77805,#77806,#77807,#77808,#77809,#77810,#77811,#77812,#77813,#77814,#77815,
#77816,#77817,#77818,#77819,#77820,#77821,#77822,#77823,#77824,#77825,#77826,
#77827,#77828,#77829,#77830,#77831,#77832,#77833,#77834,#77835,#77836,#77837,
#77838,#77839,#77840,#77841,#77842,#77843,#77844,#77845,#77846,#77847,#77848,
#77849,#77850,#77851,#77852,#77853,#77854,#77855,#77856,#77857,#77858,#77859,
#77860,#77861,#77862,#77863,#77864,#77865,#77866,#77867,#77868,#77869,#77870,
#77871,#77872,#77873,#77874,#77875,#77876,#77877,#77878,#77879,#77880,#77881,
#77882,#77883,#77884,#77885,#77886,#77887,#77888,#77889,#77890,#77891,#77892,
#77893,#77894,#77895,#77896,#77897,#77898,#77899,#77900,#77901,#77902,#77903,
#77904,#77905),.UNSPECIFIED.,.F.,.F.,(4,3,3,3,3,3,3,3,3,3,3,3,3,3,3,3,3,
3,3,3,3,3,3,3,3,3,3,3,3,3,3,3,3,3,3,3,3,3,3,3,3,3,3,3,3,3,3,3,3,3,3,3,3,
3,3,3,3,4),(-104.572202052802,-104.464825203815,-104.357557368283,-104.250356283725,
-104.143179794702,-104.035911189414,-103.928596755901,-103.821086998969,
-103.740684524047,-103.631512083848,-103.520470316128,-103.411598167883,
-103.302792560386,-103.194013489076,-103.081304602328,-102.97238773937,
-102.857782840727,-102.743177942085,-102.634005503472,-102.522963735553,
-102.41409158893,-102.305285983064,-102.19650691339,-102.083798025074,-101.974881163749,
-101.860276261936,-101.745671360123,-101.63649892183,-101.525457153872,
-101.416585007596,-101.307779402086,-101.199000332777,-101.086291444123,
-100.97737458318,-100.86276968067,-100.748164778161,-100.638992339298,-100.527950571411,
-100.419078424542,-100.310272818431,-100.201493748516,-100.088784860437,
-99.9798679988786,-99.865263097539,-99.7506581961993,-99.6414857575659,
-99.5304439896498,-99.4215718430159,-99.3127662371415,-99.2039871674642,
-99.0912782791575,-98.9823614178373,-98.8677565160373,-98.7531516142373,
-98.6365755860952,-98.52026925052,-98.4043629935902,-98.2890167463),
 .UNSPECIFIED.);
#840=B_SPLINE_CURVE_WITH_KNOTS('',3,(#77907,#77908,#77909,#77910,#77911,
#77912,#77913,#77914,#77915,#77916,#77917,#77918,#77919,#77920,#77921,#77922,
#77923,#77924,#77925,#77926,#77927,#77928,#77929,#77930,#77931,#77932,#77933,
#77934,#77935,#77936,#77937,#77938,#77939,#77940,#77941,#77942,#77943,#77944,
#77945,#77946,#77947,#77948,#77949,#77950,#77951,#77952,#77953,#77954,#77955,
#77956,#77957,#77958,#77959,#77960,#77961,#77962,#77963,#77964,#77965,#77966,
#77967,#77968,#77969,#77970,#77971,#77972,#77973,#77974,#77975,#77976,#77977,
#77978,#77979,#77980,#77981,#77982,#77983,#77984,#77985,#77986,#77987,#77988,
#77989,#77990,#77991,#77992,#77993,#77994,#77995,#77996,#77997,#77998,#77999,
#78000,#78001,#78002,#78003,#78004,#78005,#78006,#78007,#78008,#78009,#78010,
#78011,#78012,#78013,#78014,#78015,#78016,#78017,#78018,#78019,#78020,#78021,
#78022,#78023,#78024,#78025,#78026,#78027,#78028,#78029,#78030,#78031,#78032,
#78033,#78034,#78035,#78036,#78037,#78038,#78039,#78040,#78041,#78042,#78043,
#78044,#78045,#78046,#78047,#78048,#78049,#78050,#78051,#78052,#78053,#78054,
#78055,#78056,#78057,#78058,#78059,#78060,#78061,#78062,#78063,#78064,#78065,
#78066,#78067,#78068,#78069,#78070,#78071,#78072,#78073,#78074,#78075,#78076,
#78077,#78078),.UNSPECIFIED.,.F.,.F.,(4,3,3,3,3,3,3,3,3,3,3,3,3,3,3,3,3,
3,3,3,3,3,3,3,3,3,3,3,3,3,3,3,3,3,3,3,3,3,3,3,3,3,3,3,3,3,3,3,3,3,3,3,3,
3,3,3,3,4),(-98.2890167459438,-98.1765832750562,-98.0639026838957,-97.9510940965738,
-97.8379965452098,-97.7556450322753,-97.6464725935929,-97.535430825683,
-97.4265586789999,-97.3177530730765,-97.20897400335,-97.0962651150908,-96.9873482537224,
-96.8727433520178,-96.7581384503133,-96.6489660116626,-96.5379242437487,
-96.4290520970982,-96.3202464912076,-96.2114674215143,-96.0987585332235,
-95.9898416718884,-95.8752367701198,-95.7606318683513,-95.6514594297002,
-95.5404176617863,-95.4315455151358,-95.3227399092451,-95.2139608395516,
-95.101251951261,-94.9923350899261,-94.8777301881577,-94.7631252863893,
-94.6539528477305,-94.5429110798176,-94.434038933159,-94.3252333272602,
-94.2164542575586,-94.1037453692758,-93.9948285079324,-93.8802236061799,
-93.7656187044273,-93.6564462657728,-93.5454044978594,-93.4365323512051,
-93.3277267453107,-93.2189476756135,-93.1062387873264,-92.9973219259875,
-92.8827170242264,-92.7681121224653,-92.660350082923,-92.5527396333652,
-92.4452386139182,-92.3353868201298,-92.2279447729249,-92.1168881058446,
-92.0058314387643),.UNSPECIFIED.);
#841=B_SPLINE_CURVE_WITH_KNOTS('',3,(#78080,#78081,#78082,#78083,#78084,
#78085,#78086,#78087,#78088,#78089,#78090,#78091,#78092,#78093,#78094,#78095,
#78096,#78097,#78098,#78099,#78100,#78101,#78102,#78103,#78104,#78105,#78106,
#78107,#78108,#78109,#78110,#78111,#78112,#78113,#78114,#78115,#78116,#78117,
#78118,#78119,#78120,#78121,#78122,#78123,#78124,#78125,#78126,#78127,#78128,
#78129,#78130,#78131,#78132,#78133,#78134,#78135,#78136,#78137,#78138,#78139,
#78140,#78141,#78142,#78143,#78144,#78145,#78146,#78147,#78148,#78149,#78150,
#78151,#78152,#78153,#78154,#78155,#78156,#78157,#78158,#78159,#78160,#78161,
#78162,#78163,#78164,#78165,#78166,#78167,#78168,#78169,#78170,#78171,#78172,
#78173,#78174,#78175,#78176,#78177,#78178,#78179,#78180,#78181,#78182,#78183,
#78184,#78185,#78186,#78187,#78188,#78189,#78190,#78191,#78192,#78193,#78194,
#78195,#78196,#78197,#78198,#78199,#78200,#78201,#78202,#78203,#78204,#78205,
#78206,#78207,#78208,#78209,#78210,#78211,#78212,#78213,#78214,#78215,#78216,
#78217,#78218,#78219,#78220,#78221,#78222,#78223,#78224,#78225,#78226,#78227,
#78228,#78229,#78230,#78231,#78232,#78233,#78234,#78235,#78236,#78237,#78238,
#78239,#78240,#78241,#78242,#78243,#78244,#78245,#78246,#78247,#78248,#78249,
#78250,#78251),.UNSPECIFIED.,.F.,.F.,(4,3,3,3,3,3,3,3,3,3,3,3,3,3,3,3,3,
3,3,3,3,3,3,3,3,3,3,3,3,3,3,3,3,3,3,3,3,3,3,3,3,3,3,3,3,3,3,3,3,3,3,3,3,
3,3,3,3,4),(-92.0058314383864,-91.8610046365001,-91.7706055405034,-91.6614331018477,
-91.5503913339344,-91.441519187279,-91.3327135813835,-91.2239345116852,
-91.1112256233992,-91.0023087620593,-90.8877038603003,-90.7730989585413,
-90.6639265198859,-90.5528847519726,-90.4440126053175,-90.3352069994222,
-90.2264279297242,-90.1137190414379,-90.0048021800982,-89.8901972783387,
-89.7755923765793,-89.666419937924,-89.5553781700107,-89.4465060233557,
-89.3377004174606,-89.2289213477627,-89.1162124594764,-89.0072955981368,
-88.8926906963771,-88.7780857946174,-88.668913355962,-88.5578715880487,
-88.4489994413936,-88.3401938354983,-88.2314147658003,-88.1187058775141,
-88.0097890161743,-87.8951841144149,-87.7805792126554,-87.671406774,-87.5603650060866,
-87.4514928594315,-87.3426872535362,-87.2339081838382,-87.121199295552,
-87.0122824342123,-86.8976775324528,-86.7830726306934,-86.673900192038,
-86.5628584241247,-86.4539862774696,-86.3451806715744,-86.2364016018764,
-86.1236927135901,-86.0147758522505,-85.9001709504909,-85.7855660487314,
-85.7226461315846),.UNSPECIFIED.);
#842=B_SPLINE_CURVE_WITH_KNOTS('',3,(#78253,#78254,#78255,#78256,#78257,
#78258,#78259,#78260,#78261,#78262,#78263,#78264,#78265,#78266,#78267,#78268,
#78269,#78270,#78271,#78272,#78273,#78274,#78275,#78276,#78277,#78278,#78279,
#78280,#78281,#78282,#78283,#78284,#78285,#78286,#78287,#78288,#78289,#78290,
#78291,#78292,#78293,#78294,#78295,#78296,#78297,#78298,#78299,#78300,#78301,
#78302,#78303,#78304,#78305,#78306,#78307,#78308,#78309,#78310,#78311,#78312,
#78313,#78314,#78315,#78316,#78317,#78318,#78319,#78320,#78321,#78322,#78323,
#78324,#78325,#78326,#78327,#78328,#78329,#78330,#78331,#78332,#78333,#78334,
#78335,#78336,#78337,#78338,#78339,#78340,#78341,#78342,#78343,#78344,#78345,
#78346,#78347,#78348,#78349,#78350,#78351,#78352,#78353,#78354,#78355,#78356,
#78357,#78358,#78359,#78360,#78361,#78362,#78363,#78364,#78365,#78366,#78367,
#78368,#78369,#78370,#78371,#78372,#78373,#78374,#78375,#78376,#78377,#78378,
#78379,#78380,#78381,#78382,#78383,#78384,#78385,#78386,#78387,#78388,#78389,
#78390,#78391,#78392,#78393,#78394,#78395,#78396,#78397,#78398,#78399,#78400,
#78401,#78402,#78403,#78404,#78405,#78406,#78407,#78408,#78409,#78410,#78411,
#78412,#78413,#78414,#78415,#78416,#78417,#78418,#78419,#78420,#78421,#78422,
#78423,#78424),.UNSPECIFIED.,.F.,.F.,(4,3,3,3,3,3,3,3,3,3,3,3,3,3,3,3,3,
3,3,3,3,3,3,3,3,3,3,3,3,3,3,3,3,3,3,3,3,3,3,3,3,3,3,3,3,3,3,3,3,3,3,3,3,
3,3,3,3,4),(-85.72264613121,-85.6145003567967,-85.5065334315114,-85.3986650150454,
-85.2908535890857,-85.1830577204263,-85.0751612384323,-84.9672121288341,
-84.8590675344965,-84.7880594667694,-84.6788870281141,-84.5678452602007,
-84.4589731135457,-84.3501675076505,-84.2413884379525,-84.1286795496662,
-84.0197626883265,-83.9051577865669,-83.7905528848074,-83.681380446152,
-83.5703386782387,-83.4614665315836,-83.3526609256883,-83.2438818559903,
-83.1311729677041,-83.0222561063644,-82.9076512046049,-82.7930463028454,
-82.6838738641901,-82.5728320962768,-82.4639599496218,-82.3551543437266,
-82.2463752740285,-82.1336663857422,-82.0247495244026,-81.910144622643,
-81.7955397208834,-81.686367282228,-81.5753255143147,-81.4664533676596,
-81.3576477617644,-81.2488686920663,-81.1361598037801,-81.0272429424404,
-80.9126380406809,-80.7980331389214,-80.6888607002659,-80.5778189323526,
-80.4689467856975,-80.3601411798021,-80.2513621101042,-80.138653221818,
-80.0297363604782,-79.9151314587188,-79.8005265569594,-79.6756486279101,
-79.5517871056718,-79.4394608248622),.UNSPECIFIED.);
#843=B_SPLINE_CURVE_WITH_KNOTS('',3,(#78426,#78427,#78428,#78429,#78430,
#78431,#78432,#78433,#78434,#78435,#78436,#78437,#78438,#78439,#78440,#78441,
#78442,#78443,#78444,#78445,#78446,#78447,#78448,#78449,#78450,#78451,#78452,
#78453,#78454,#78455,#78456,#78457,#78458,#78459,#78460,#78461,#78462,#78463,
#78464,#78465,#78466,#78467,#78468,#78469,#78470,#78471,#78472,#78473,#78474,
#78475,#78476,#78477,#78478,#78479,#78480,#78481,#78482,#78483,#78484,#78485,
#78486,#78487,#78488,#78489,#78490,#78491,#78492,#78493,#78494,#78495,#78496,
#78497,#78498,#78499,#78500,#78501,#78502,#78503,#78504,#78505,#78506,#78507,
#78508,#78509,#78510,#78511,#78512,#78513,#78514,#78515,#78516,#78517,#78518,
#78519,#78520,#78521,#78522,#78523,#78524,#78525,#78526,#78527,#78528,#78529,
#78530,#78531,#78532,#78533,#78534,#78535,#78536,#78537,#78538,#78539,#78540,
#78541,#78542,#78543,#78544,#78545,#78546,#78547,#78548,#78549,#78550,#78551,
#78552,#78553,#78554,#78555,#78556,#78557,#78558,#78559,#78560,#78561,#78562,
#78563,#78564,#78565,#78566,#78567,#78568,#78569,#78570,#78571,#78572,#78573,
#78574,#78575,#78576,#78577,#78578,#78579,#78580,#78581,#78582,#78583,#78584,
#78585,#78586,#78587,#78588,#78589,#78590,#78591,#78592,#78593,#78594,#78595,
#78596,#78597),.UNSPECIFIED.,.F.,.F.,(4,3,3,3,3,3,3,3,3,3,3,3,3,3,3,3,3,
3,3,3,3,3,3,3,3,3,3,3,3,3,3,3,3,3,3,3,3,3,3,3,3,3,3,3,3,3,3,3,3,3,3,3,3,
3,3,3,3,4),(-79.4394608244051,-79.3301673042638,-79.2208686887329,-79.1114399455883,
-79.0019456137403,-78.8922276554658,-78.8030199749974,-78.6938475363419,
-78.5828057684286,-78.4739336217734,-78.3651280158782,-78.2563489461802,
-78.143640057894,-78.0347231965542,-77.9201182947948,-77.8055133930354,
-77.6963409543801,-77.5852991864668,-77.4764270398118,-77.3676214339166,
-77.2588423642185,-77.1461334759323,-77.0372166145927,-76.9226117128331,
-76.8080068110735,-76.6988343724183,-76.5877926045049,-76.4789204578498,
-76.3701148519545,-76.2613357822566,-76.1486268939703,-76.0397100326307,
-75.9251051308711,-75.8105002291115,-75.7013277904561,-75.5902860225428,
-75.4814138758876,-75.3726082699924,-75.2638292002946,-75.1511203120083,
-75.0422034506686,-74.9275985489091,-74.8129936471495,-74.7038212084941,
-74.5927794405808,-74.4839072939257,-74.3751016880306,-74.2663226183327,
-74.1536137300464,-74.0446968687067,-73.9300919669471,-73.8154870651875,
-73.7062663965449,-73.5972126760366,-73.4869783863338,-73.3781347024253,
-73.2672051098253,-73.1562755172254),.UNSPECIFIED.);
#844=B_SPLINE_CURVE_WITH_KNOTS('',3,(#78599,#78600,#78601,#78602,#78603,
#78604,#78605,#78606,#78607,#78608,#78609,#78610,#78611,#78612,#78613,#78614,
#78615,#78616,#78617,#78618,#78619,#78620,#78621,#78622,#78623,#78624,#78625,
#78626,#78627,#78628,#78629,#78630,#78631,#78632,#78633,#78634,#78635,#78636,
#78637,#78638,#78639,#78640,#78641,#78642,#78643,#78644,#78645,#78646,#78647,
#78648,#78649,#78650,#78651,#78652,#78653,#78654,#78655,#78656,#78657,#78658,
#78659,#78660,#78661,#78662,#78663,#78664,#78665,#78666,#78667,#78668,#78669,
#78670,#78671,#78672,#78673,#78674,#78675,#78676,#78677,#78678,#78679,#78680,
#78681,#78682,#78683,#78684,#78685,#78686,#78687,#78688,#78689,#78690,#78691,
#78692,#78693,#78694,#78695,#78696,#78697,#78698,#78699,#78700,#78701,#78702,
#78703,#78704,#78705,#78706,#78707,#78708,#78709,#78710,#78711,#78712,#78713,
#78714,#78715,#78716,#78717,#78718,#78719,#78720,#78721,#78722,#78723,#78724,
#78725,#78726,#78727,#78728,#78729,#78730,#78731,#78732,#78733,#78734,#78735,
#78736,#78737,#78738,#78739,#78740,#78741,#78742,#78743,#78744,#78745,#78746,
#78747,#78748,#78749,#78750,#78751,#78752,#78753,#78754,#78755,#78756,#78757,
#78758,#78759,#78760,#78761,#78762,#78763,#78764,#78765,#78766,#78767,#78768,
#78769,#78770),.UNSPECIFIED.,.F.,.F.,(4,3,3,3,3,3,3,3,3,3,3,3,3,3,3,3,3,
3,3,3,3,3,3,3,3,3,3,3,3,3,3,3,3,3,3,3,3,3,3,3,3,3,3,3,3,3,3,3,3,3,3,3,3,
3,3,3,3,4),(-73.1562755167914,-73.0302440560829,-72.9029247194667,-72.8179804832255,
-72.70880804457,-72.5977662766567,-72.4888941300014,-72.380088524106,-72.2713094544078,
-72.1586005661217,-72.0496837047819,-71.9350788030227,-71.8204739012635,
-71.7113014626082,-71.6002596946948,-71.4913875480398,-71.3825819421446,
-71.2738028724466,-71.1610939841603,-71.0521771228207,-70.9375722210611,
-70.8229673193015,-70.7137948806462,-70.6027531127328,-70.4938809660778,
-70.3850753601826,-70.2762962904846,-70.1635874021983,-70.0546705408586,
-69.9400656390991,-69.8254607373395,-69.7162882986841,-69.6052465307708,
-69.4963743841157,-69.3875687782204,-69.2787897085223,-69.1660808202361,
-69.0571639588964,-68.9425590571369,-68.8279541553775,-68.7187817167221,
-68.6077399488088,-68.4988678021537,-68.3900621962585,-68.2812831265604,
-68.1685742382742,-68.0596573769345,-67.945052475175,-67.8304475734155,
-67.7219687232105,-67.6136797702115,-67.5054965122317,-67.3973778082143,
-67.2892826089374,-67.1810938588446,-67.0728602415266,-66.9644273644967,
-66.8730902106081),.UNSPECIFIED.);
#845=B_SPLINE_CURVE_WITH_KNOTS('',3,(#78772,#78773,#78774,#78775,#78776,
#78777,#78778,#78779,#78780,#78781,#78782,#78783,#78784,#78785,#78786,#78787,
#78788,#78789,#78790,#78791,#78792,#78793,#78794,#78795,#78796,#78797,#78798,
#78799,#78800,#78801,#78802,#78803,#78804,#78805,#78806,#78807,#78808,#78809,
#78810,#78811,#78812,#78813,#78814,#78815,#78816,#78817,#78818,#78819,#78820,
#78821,#78822,#78823,#78824,#78825,#78826,#78827,#78828,#78829,#78830,#78831,
#78832,#78833,#78834,#78835,#78836,#78837,#78838,#78839,#78840,#78841,#78842,
#78843,#78844,#78845,#78846,#78847,#78848,#78849,#78850,#78851,#78852,#78853,
#78854,#78855,#78856,#78857,#78858,#78859,#78860,#78861,#78862,#78863,#78864,
#78865,#78866,#78867,#78868,#78869,#78870,#78871,#78872,#78873,#78874,#78875,
#78876,#78877,#78878,#78879,#78880,#78881,#78882,#78883,#78884,#78885,#78886,
#78887,#78888,#78889,#78890,#78891,#78892,#78893,#78894,#78895,#78896,#78897,
#78898,#78899,#78900,#78901,#78902,#78903,#78904,#78905,#78906,#78907,#78908,
#78909,#78910,#78911,#78912,#78913,#78914,#78915,#78916,#78917,#78918,#78919,
#78920,#78921,#78922,#78923,#78924,#78925,#78926,#78927,#78928,#78929,#78930,
#78931,#78932,#78933,#78934,#78935,#78936,#78937,#78938,#78939,#78940,#78941,
#78942,#78943),.UNSPECIFIED.,.F.,.F.,(4,3,3,3,3,3,3,3,3,3,3,3,3,3,3,3,3,
3,3,3,3,3,3,3,3,3,3,3,3,3,3,3,3,3,3,3,3,3,3,3,3,3,3,3,3,3,3,3,3,3,3,3,3,
3,3,3,3,4),(-66.8730902100459,-66.8329409914535,-66.7237685527981,-66.6127267848848,
-66.5038546382296,-66.3950490323343,-66.2862699626363,-66.1735610743501,
-66.0646442130104,-65.9500393112509,-65.8354344094915,-65.7262619708361,
-65.6152202029228,-65.5063480562677,-65.3975424503725,-65.2887633806745,
-65.1760544923882,-65.0671376310485,-64.952532729289,-64.8379278275295,
-64.7287553888741,-64.6177136209608,-64.5088414743057,-64.4000358684105,
-64.2912567987124,-64.1785479104262,-64.0696310490865,-63.955026147327,
-63.8404212455675,-63.7312488069121,-63.6202070389988,-63.5113348923437,
-63.4025292864485,-63.2937502167505,-63.1810413284643,-63.0721244671246,
-62.957519565365,-62.8429146636055,-62.7337422249501,-62.6227004570368,
-62.5138283103817,-62.4050227044865,-62.2962436347884,-62.1835347465022,
-62.0746178851625,-61.960012983403,-61.8454080816435,-61.7362356429881,
-61.6251938750748,-61.5163217284197,-61.4075161225244,-61.2987370528264,
-61.1860281645402,-61.0771113032005,-60.962506401441,-60.8479014996816,
-60.708459556948,-60.5899049034139),.UNSPECIFIED.);
#846=B_SPLINE_CURVE_WITH_KNOTS('',3,(#78945,#78946,#78947,#78948,#78949,
#78950,#78951,#78952,#78953,#78954,#78955,#78956,#78957,#78958,#78959,#78960,
#78961,#78962,#78963,#78964,#78965,#78966,#78967,#78968,#78969,#78970,#78971,
#78972,#78973,#78974,#78975,#78976,#78977,#78978,#78979,#78980,#78981,#78982,
#78983,#78984,#78985,#78986,#78987,#78988,#78989,#78990,#78991,#78992,#78993,
#78994,#78995,#78996,#78997,#78998,#78999,#79000,#79001,#79002,#79003,#79004,
#79005,#79006,#79007,#79008,#79009,#79010,#79011,#79012,#79013,#79014,#79015,
#79016,#79017,#79018,#79019,#79020,#79021,#79022,#79023,#79024,#79025,#79026,
#79027,#79028,#79029,#79030,#79031,#79032,#79033,#79034,#79035,#79036,#79037,
#79038,#79039,#79040,#79041,#79042,#79043,#79044,#79045,#79046,#79047,#79048,
#79049,#79050,#79051,#79052,#79053,#79054,#79055,#79056,#79057,#79058,#79059,
#79060,#79061,#79062,#79063,#79064,#79065,#79066,#79067,#79068,#79069,#79070,
#79071,#79072,#79073,#79074,#79075,#79076,#79077,#79078,#79079,#79080,#79081,
#79082,#79083,#79084,#79085,#79086,#79087,#79088,#79089,#79090,#79091,#79092,
#79093,#79094,#79095,#79096,#79097,#79098,#79099,#79100,#79101,#79102,#79103,
#79104,#79105,#79106,#79107,#79108,#79109,#79110,#79111,#79112,#79113,#79114,
#79115,#79116),.UNSPECIFIED.,.F.,.F.,(4,3,3,3,3,3,3,3,3,3,3,3,3,3,3,3,3,
3,3,3,3,3,3,3,3,3,3,3,3,3,3,3,3,3,3,3,3,3,3,3,3,3,3,3,3,3,3,3,3,3,3,3,3,
3,3,3,3,4),(-60.5899049028662,-60.4821931879117,-60.3745475152884,-60.2669262422658,
-60.1592102498021,-60.0514492410922,-59.9434849929317,-59.8503949177196,
-59.7412224790642,-59.6301807111508,-59.5213085644957,-59.4125029586005,
-59.3037238889025,-59.1910150006163,-59.0820981392765,-58.9674932375171,
-58.8528883357576,-58.7437158971022,-58.6326741291889,-58.5238019825338,
-58.4149963766385,-58.3062173069406,-58.1935084186543,-58.0845915573146,
-57.9699866555551,-57.8553817537956,-57.7462093151402,-57.6351675472269,
-57.5262954005718,-57.4174897946765,-57.3087107249786,-57.1960018366923,
-57.0870849753527,-56.9724800735931,-56.8578751718336,-56.7487027331782,
-56.6376609652649,-56.5287888186098,-56.4199832127146,-56.3112041430166,
-56.1984952547304,-56.0895783933908,-55.9749734916312,-55.8603685898716,
-55.7511961512163,-55.640154383303,-55.5312822366479,-55.4224766307527,
-55.3136975610548,-55.2009886727685,-55.0920718114288,-54.9774669096692,
-54.8628620079096,-54.75063905054,-54.6386821891945,-54.5268818601967,-54.4152297097849,
-54.3067195956867),.UNSPECIFIED.);
#847=B_SPLINE_CURVE_WITH_KNOTS('',3,(#79118,#79119,#79120,#79121,#79122,
#79123,#79124,#79125,#79126,#79127,#79128,#79129,#79130,#79131,#79132,#79133,
#79134,#79135,#79136,#79137,#79138,#79139,#79140,#79141,#79142,#79143,#79144,
#79145,#79146,#79147,#79148,#79149,#79150,#79151,#79152,#79153,#79154,#79155,
#79156,#79157,#79158,#79159,#79160,#79161,#79162,#79163,#79164,#79165,#79166,
#79167,#79168,#79169,#79170,#79171,#79172,#79173,#79174,#79175,#79176,#79177,
#79178,#79179,#79180,#79181,#79182,#79183,#79184,#79185,#79186,#79187,#79188,
#79189,#79190,#79191,#79192,#79193,#79194,#79195,#79196,#79197,#79198,#79199,
#79200,#79201,#79202,#79203,#79204,#79205,#79206,#79207,#79208,#79209,#79210,
#79211,#79212,#79213,#79214,#79215,#79216,#79217,#79218,#79219,#79220,#79221,
#79222,#79223,#79224,#79225,#79226,#79227,#79228,#79229,#79230,#79231,#79232,
#79233,#79234,#79235,#79236,#79237,#79238,#79239,#79240,#79241,#79242,#79243,
#79244,#79245,#79246,#79247,#79248,#79249,#79250,#79251,#79252,#79253,#79254,
#79255,#79256,#79257,#79258,#79259,#79260,#79261,#79262,#79263,#79264,#79265,
#79266,#79267,#79268,#79269,#79270,#79271,#79272,#79273,#79274,#79275,#79276,
#79277,#79278,#79279,#79280,#79281,#79282,#79283,#79284,#79285,#79286,#79287,
#79288,#79289),.UNSPECIFIED.,.F.,.F.,(4,3,3,3,3,3,3,3,3,3,3,3,3,3,3,3,3,
3,3,3,3,3,3,3,3,3,3,3,3,3,3,3,3,3,3,3,3,3,3,3,3,3,3,3,3,3,3,3,3,3,3,3,3,
3,3,3,3,4),(-54.3067195951254,-54.189439388817,-54.0718637479082,-53.9538094079238,
-53.8653554259476,-53.7561829872923,-53.645141219379,-53.536269072724,-53.4274634668289,
-53.318684397131,-53.2059755088446,-53.0970586475051,-52.9824537457453,
-52.8678488439856,-52.7586764053301,-52.6476346374168,-52.5387624907616,
-52.4299568848663,-52.3211778151681,-52.208468926882,-52.0995520655422,
-51.9849471637829,-51.8703422620236,-51.7611698233683,-51.6501280554549,
-51.5412559087998,-51.4324503029046,-51.3236712332067,-51.2109623449204,
-51.1020454835807,-50.9874405818212,-50.8728356800616,-50.7636632414063,
-50.6526214734929,-50.5437493268379,-50.4349437209427,-50.3261646512448,
-50.2134557629585,-50.1045389016188,-49.9899339998592,-49.8753290980996,
-49.7661566594441,-49.6551148915308,-49.5462427448756,-49.4374371389804,
-49.3286580692823,-49.2159491809961,-49.1070323196563,-48.992427417897,
-48.8778225161376,-48.770283184556,-48.6628909290572,-48.5556033712,-48.4483782985246,
-48.3411132279635,-48.2338352157278,-48.1263962591731,-48.0235342889076),
 .UNSPECIFIED.);
#848=B_SPLINE_CURVE_WITH_KNOTS('',3,(#79291,#79292,#79293,#79294,#79295,
#79296,#79297,#79298,#79299,#79300,#79301,#79302,#79303,#79304,#79305,#79306,
#79307,#79308,#79309,#79310,#79311,#79312,#79313,#79314,#79315,#79316,#79317,
#79318,#79319,#79320,#79321,#79322,#79323,#79324,#79325,#79326,#79327,#79328,
#79329,#79330,#79331,#79332,#79333,#79334,#79335,#79336,#79337,#79338,#79339,
#79340,#79341,#79342,#79343,#79344,#79345,#79346,#79347,#79348,#79349,#79350,
#79351,#79352,#79353,#79354,#79355,#79356,#79357,#79358,#79359,#79360,#79361,
#79362,#79363,#79364,#79365,#79366,#79367,#79368,#79369,#79370,#79371,#79372,
#79373,#79374,#79375,#79376,#79377,#79378,#79379,#79380,#79381,#79382,#79383,
#79384,#79385,#79386,#79387,#79388,#79389,#79390,#79391,#79392,#79393,#79394,
#79395,#79396,#79397,#79398,#79399,#79400,#79401,#79402,#79403,#79404,#79405,
#79406,#79407,#79408,#79409,#79410,#79411,#79412,#79413,#79414,#79415,#79416,
#79417,#79418,#79419,#79420,#79421,#79422,#79423,#79424,#79425,#79426,#79427,
#79428,#79429,#79430,#79431,#79432,#79433,#79434,#79435,#79436,#79437,#79438,
#79439,#79440,#79441,#79442,#79443,#79444,#79445,#79446,#79447,#79448,#79449,
#79450,#79451,#79452,#79453,#79454,#79455,#79456,#79457,#79458,#79459),
 .UNSPECIFIED.,.F.,.F.,(4,3,3,3,3,3,3,3,3,3,3,3,3,3,3,3,3,3,3,3,3,3,3,3,
3,3,3,3,3,3,3,3,3,3,3,3,3,3,3,3,3,3,3,3,3,3,3,3,3,3,3,3,3,3,3,3,4),(-48.0235342885071,
-47.8803159341757,-47.77114349552,-47.6601017276067,-47.5512295809513,-47.4424239750557,
-47.3336449053574,-47.2209360170715,-47.1120191557314,-46.9974142539726,
-46.8828093522137,-46.7736369135582,-46.6625951456449,-46.5537229989897,
-46.4449173930943,-46.3361383233961,-46.22342943511,-46.1145125737702,-45.9999076720109,
-45.8853027702517,-45.7761303315965,-45.6650885636831,-45.5562164170282,
-45.4474108111331,-45.3386317414353,-45.2259228531489,-45.1170059918093,
-45.0024010900495,-44.8877961882897,-44.7786237496343,-44.667581981721,
-44.5587098350659,-44.4499042291706,-44.3411251594726,-44.2284162711863,
-44.1194994098466,-44.0048945080872,-43.8902896063277,-43.7811171676722,
-43.6700753997589,-43.5612032531037,-43.4523976472084,-43.3436185775103,
-43.2309096892242,-43.1219928278844,-43.0073879261251,-42.8927830243657,
-42.7836105857104,-42.6725688177971,-42.563696671142,-42.4548910652469,
-42.346111995549,-42.2334031072627,-42.1244862459231,-42.0098813441634,
-41.8952764424037,-41.7403489813275),.UNSPECIFIED.);
#849=B_SPLINE_CURVE_WITH_KNOTS('',3,(#79461,#79462,#79463,#79464,#79465,
#79466,#79467,#79468,#79469,#79470,#79471,#79472,#79473,#79474,#79475,#79476,
#79477,#79478,#79479,#79480,#79481,#79482,#79483,#79484,#79485,#79486,#79487,
#79488,#79489,#79490,#79491,#79492,#79493,#79494,#79495,#79496,#79497,#79498,
#79499,#79500,#79501,#79502,#79503,#79504,#79505,#79506,#79507,#79508,#79509,
#79510,#79511,#79512,#79513,#79514,#79515,#79516,#79517,#79518,#79519,#79520,
#79521,#79522,#79523,#79524,#79525,#79526,#79527,#79528,#79529,#79530,#79531,
#79532,#79533,#79534,#79535,#79536,#79537,#79538,#79539,#79540,#79541,#79542,
#79543,#79544,#79545,#79546,#79547,#79548,#79549,#79550,#79551,#79552,#79553,
#79554,#79555,#79556,#79557,#79558,#79559,#79560,#79561,#79562,#79563,#79564,
#79565,#79566,#79567,#79568,#79569,#79570,#79571,#79572,#79573,#79574,#79575,
#79576,#79577,#79578,#79579,#79580,#79581,#79582,#79583,#79584,#79585,#79586,
#79587,#79588,#79589,#79590,#79591,#79592,#79593,#79594,#79595,#79596,#79597,
#79598,#79599,#79600,#79601,#79602,#79603,#79604,#79605,#79606,#79607,#79608,
#79609,#79610,#79611,#79612,#79613,#79614,#79615,#79616,#79617,#79618,#79619,
#79620,#79621,#79622,#79623,#79624,#79625,#79626,#79627,#79628,#79629,#79630,
#79631,#79632),.UNSPECIFIED.,.F.,.F.,(4,3,3,3,3,3,3,3,3,3,3,3,3,3,3,3,3,
3,3,3,3,3,3,3,3,3,3,3,3,3,3,3,3,3,3,3,3,3,3,3,3,3,3,3,3,3,3,3,3,3,3,3,3,
3,3,3,3,4),(-41.7403489809666,-41.6329490692741,-41.5256623867346,-41.4184466672188,
-41.3112597576395,-41.2039837574797,-41.096665730506,-40.9891488560991,
-40.8977698604417,-40.7885974217861,-40.6775556538728,-40.5686835072176,
-40.4598779013223,-40.3510988316241,-40.238389943338,-40.1294730819981,
-40.0148681802389,-39.9002632784797,-39.7910908398243,-39.680049071911,
-39.571176925256,-39.4623713193608,-39.3535922496629,-39.2408833613766,
-39.131966500037,-39.0173615982773,-38.9027566965177,-38.7935842578622,
-38.6825424899489,-38.5736703432938,-38.4648647373985,-38.3560856677007,
-38.2433767794144,-38.1344599180748,-38.0198550163152,-37.9052501145557,
-37.7960776759003,-37.6850359079869,-37.5761637613317,-37.4673581554365,
-37.3585790857385,-37.2458701974523,-37.1369533361124,-37.0223484343531,
-36.9077435325937,-36.7985710939385,-36.6875293260252,-36.5786571793702,
-36.469851573475,-36.3610725037773,-36.2483636154909,-36.1394467541514,
-36.0248418523915,-35.9102369506317,-35.792973733972,-35.6759975257706,
-35.5594572831808,-35.4571636746066),.UNSPECIFIED.);
#850=B_SPLINE_CURVE_WITH_KNOTS('',3,(#79634,#79635,#79636,#79637,#79638,
#79639,#79640,#79641,#79642,#79643,#79644,#79645,#79646,#79647,#79648,#79649,
#79650,#79651,#79652,#79653,#79654,#79655,#79656,#79657,#79658,#79659,#79660,
#79661,#79662,#79663,#79664,#79665,#79666,#79667,#79668,#79669,#79670,#79671,
#79672,#79673,#79674,#79675,#79676,#79677,#79678,#79679,#79680,#79681,#79682,
#79683,#79684,#79685,#79686,#79687,#79688,#79689,#79690,#79691,#79692,#79693,
#79694,#79695,#79696,#79697,#79698,#79699,#79700,#79701,#79702,#79703,#79704,
#79705,#79706,#79707,#79708,#79709,#79710,#79711,#79712,#79713,#79714,#79715,
#79716,#79717,#79718,#79719,#79720,#79721,#79722,#79723,#79724,#79725,#79726,
#79727,#79728,#79729,#79730,#79731,#79732,#79733,#79734,#79735,#79736,#79737,
#79738,#79739,#79740,#79741,#79742,#79743,#79744,#79745,#79746,#79747,#79748,
#79749,#79750,#79751,#79752,#79753,#79754,#79755,#79756,#79757,#79758,#79759,
#79760,#79761,#79762,#79763,#79764,#79765,#79766,#79767,#79768,#79769,#79770,
#79771,#79772,#79773,#79774,#79775,#79776,#79777,#79778,#79779,#79780,#79781,
#79782,#79783,#79784,#79785,#79786,#79787,#79788,#79789,#79790,#79791,#79792,
#79793,#79794,#79795,#79796,#79797,#79798,#79799,#79800,#79801,#79802,#79803,
#79804,#79805),.UNSPECIFIED.,.F.,.F.,(4,3,3,3,3,3,3,3,3,3,3,3,3,3,3,3,3,
3,3,3,3,3,3,3,3,3,3,3,3,3,3,3,3,3,3,3,3,3,3,3,3,3,3,3,3,3,3,3,3,3,3,3,3,
3,3,3,3,4),(-35.4571636741479,-35.3451567223982,-35.2329232796229,-35.1205751861138,
-35.0079430284769,-34.9127303686697,-34.8035579300143,-34.692516162101,
-34.583644015446,-34.4748384095508,-34.3660593398529,-34.2533504515666,
-34.144433590227,-34.0298286884674,-33.9152237867078,-33.8060513480526,
-33.6950095801392,-33.5861374334843,-33.4773318275893,-33.3685527578914,
-33.255843869605,-33.1469270082655,-33.0323221065056,-32.9177172047458,
-32.8085447660899,-32.6975029981766,-32.588630851521,-32.4798252456253,
-32.371046175927,-32.2583372876412,-32.149420426301,-32.0348155245424,-31.9202106227838,
-31.8110381841289,-31.6999964162155,-31.5911242695608,-31.482318663666,
-31.3735395939685,-31.2608307056818,-31.1519138443426,-31.0373089425822,
-30.9227040408218,-30.8135316021673,-30.7024898342538,-30.5936176875995,
-30.4848120817052,-30.3760330120079,-30.2633241237209,-30.1544072623821,
-30.039802360621,-29.9251974588598,-29.8173426398448,-29.7096404023268,
-29.602048690314,-29.4944927141703,-29.3869653894048,-29.2793456073155,
-29.1739783669683),.UNSPECIFIED.);
#851=B_SPLINE_CURVE_WITH_KNOTS('',3,(#79807,#79808,#79809,#79810,#79811,
#79812,#79813,#79814,#79815,#79816,#79817,#79818,#79819,#79820,#79821,#79822,
#79823,#79824,#79825,#79826,#79827,#79828,#79829,#79830,#79831,#79832,#79833,
#79834,#79835,#79836,#79837,#79838,#79839,#79840,#79841,#79842,#79843,#79844,
#79845,#79846,#79847,#79848,#79849,#79850,#79851,#79852,#79853,#79854,#79855,
#79856,#79857,#79858,#79859,#79860,#79861,#79862,#79863,#79864,#79865,#79866,
#79867,#79868,#79869,#79870,#79871,#79872,#79873,#79874,#79875,#79876,#79877,
#79878,#79879,#79880,#79881,#79882,#79883,#79884,#79885,#79886,#79887,#79888,
#79889,#79890,#79891,#79892,#79893,#79894,#79895,#79896,#79897,#79898,#79899,
#79900,#79901,#79902,#79903,#79904,#79905,#79906,#79907,#79908,#79909,#79910,
#79911,#79912,#79913,#79914,#79915,#79916,#79917,#79918,#79919,#79920,#79921,
#79922,#79923,#79924,#79925,#79926,#79927,#79928,#79929,#79930,#79931,#79932,
#79933,#79934,#79935,#79936,#79937,#79938,#79939,#79940,#79941,#79942,#79943,
#79944,#79945,#79946,#79947,#79948,#79949,#79950,#79951,#79952,#79953,#79954,
#79955,#79956,#79957,#79958,#79959,#79960,#79961,#79962,#79963,#79964,#79965,
#79966,#79967,#79968,#79969,#79970,#79971,#79972,#79973,#79974,#79975,#79976,
#79977,#79978),.UNSPECIFIED.,.F.,.F.,(4,3,3,3,3,3,3,3,3,3,3,3,3,3,3,3,3,
3,3,3,3,3,3,3,3,3,3,3,3,3,3,3,3,3,3,3,3,3,3,3,3,3,3,3,3,3,3,3,3,3,3,3,3,
3,3,3,3,4),(-29.1739783663998,-29.0319114532481,-28.9276908768978,-28.818518438247,
-28.7074766703331,-28.5986045236825,-28.4897989177918,-28.3810198480982,
-28.2683109598076,-28.1593940984721,-28.044789196704,-27.9301842949358,
-27.8210118562849,-27.709970088371,-27.6010979417206,-27.4922923358301,
-27.3835132661369,-27.2708043778461,-27.1618875165112,-27.0472826147425,
-26.9326777129738,-26.8235052742899,-26.7124635063801,-26.6035913596964,
-26.4947857537726,-26.3860066840462,-26.2732977957876,-26.16438093442,-26.0497760327159,
-25.9351711310118,-25.8259986924006,-25.7149569244818,-25.6060847778703,
-25.4972791720185,-25.3885001023634,-25.275791214035,-25.1668743527369,
-25.0522694508933,-24.9376645490498,-24.8284921104129,-24.7174503424973,
-24.608578195862,-24.499772589987,-24.3909935203097,-24.2782846320042,-24.169367770686,
-24.0547628688869,-23.9401579670878,-23.8309855282153,-23.7199437603291,
-23.611071613456,-23.5022660073431,-23.393486937428,-23.2807780493524,-23.1718611877997,
-23.0572562864627,-22.9426513851258,-22.8907930597887),.UNSPECIFIED.);
#852=B_SPLINE_CURVE_WITH_KNOTS('',3,(#79980,#79981,#79982,#79983,#79984,
#79985,#79986,#79987,#79988,#79989,#79990,#79991,#79992,#79993,#79994,#79995,
#79996,#79997,#79998,#79999,#80000,#80001,#80002,#80003,#80004,#80005,#80006,
#80007,#80008,#80009,#80010,#80011,#80012,#80013,#80014,#80015,#80016,#80017,
#80018,#80019,#80020,#80021,#80022,#80023,#80024,#80025,#80026,#80027,#80028,
#80029,#80030,#80031,#80032,#80033,#80034,#80035,#80036,#80037,#80038,#80039,
#80040,#80041,#80042,#80043,#80044,#80045,#80046,#80047,#80048,#80049,#80050,
#80051,#80052,#80053,#80054,#80055,#80056,#80057,#80058,#80059,#80060,#80061,
#80062,#80063,#80064,#80065,#80066,#80067,#80068,#80069,#80070,#80071,#80072,
#80073,#80074,#80075,#80076,#80077,#80078,#80079,#80080,#80081,#80082,#80083,
#80084,#80085,#80086,#80087,#80088,#80089,#80090,#80091,#80092,#80093,#80094,
#80095,#80096,#80097,#80098,#80099,#80100,#80101,#80102,#80103,#80104,#80105,
#80106,#80107,#80108,#80109,#80110,#80111,#80112,#80113,#80114,#80115,#80116,
#80117,#80118,#80119,#80120,#80121,#80122,#80123,#80124,#80125,#80126,#80127,
#80128,#80129,#80130,#80131,#80132,#80133,#80134,#80135,#80136,#80137,#80138,
#80139,#80140,#80141,#80142,#80143,#80144,#80145,#80146,#80147,#80148,#80149,
#80150,#80151),.UNSPECIFIED.,.F.,.F.,(4,3,3,3,3,3,3,3,3,3,3,3,3,3,3,3,3,
3,3,3,3,3,3,3,3,3,3,3,3,3,3,3,3,3,3,3,3,3,3,3,3,3,3,3,3,3,3,3,3,3,3,3,3,
3,3,3,3,4),(-22.8907930594592,-22.7824986164422,-22.6743864007115,-22.5663749719121,
-22.4584229836816,-22.3504891765429,-22.2424561812702,-22.1343732431433,
-22.0260911452468,-21.9451448031638,-21.835972364515,-21.7249305966008,
-21.6160584499633,-21.5072528440898,-21.3984737744173,-21.2857648861134,
-21.1768480248088,-21.0622431230053,-20.9476382212018,-20.8384657809417,
-20.727424013229,-20.618551864959,-20.5097462574496,-20.4009671861407,-20.2882582994155,
-20.1793414364916,-20.0647365378658,-19.9501316392399,-19.840959204042,
-19.7299174356965,-19.6210452924763,-19.5122396899983,-19.4034606236942,
-19.2907517320901,-19.1818348740486,-19.0672299656633,-18.9526250572779,
-18.8434526175422,-18.7324108497639,-18.623538702118,-18.5147330952675,
-18.4059540246515,-18.2932451373176,-18.1843282751608,-18.0697233752383,
-17.9551184753159,-17.845946025166,-17.7349042586895,-17.6260321004361,
-17.517226482936,-17.4084474016456,-17.2957385245727,-17.1868216518051,
-17.0722167725795,-16.9576118933539,-16.8315168208368,-16.7065414420316,
-16.6076077530562),.UNSPECIFIED.);
#853=B_SPLINE_CURVE_WITH_KNOTS('',3,(#80153,#80154,#80155,#80156,#80157,
#80158,#80159,#80160,#80161,#80162,#80163,#80164,#80165,#80166,#80167,#80168,
#80169,#80170,#80171,#80172,#80173,#80174,#80175,#80176,#80177,#80178,#80179,
#80180,#80181,#80182,#80183,#80184,#80185,#80186,#80187,#80188,#80189,#80190,
#80191,#80192,#80193,#80194,#80195,#80196,#80197,#80198,#80199,#80200,#80201,
#80202,#80203,#80204,#80205,#80206,#80207,#80208,#80209,#80210,#80211,#80212,
#80213,#80214,#80215,#80216,#80217,#80218,#80219,#80220,#80221,#80222,#80223,
#80224,#80225,#80226,#80227,#80228,#80229,#80230,#80231,#80232,#80233,#80234,
#80235,#80236,#80237,#80238,#80239,#80240,#80241,#80242,#80243,#80244,#80245,
#80246,#80247,#80248,#80249,#80250,#80251,#80252,#80253,#80254,#80255,#80256,
#80257,#80258,#80259,#80260,#80261,#80262,#80263,#80264,#80265,#80266,#80267,
#80268,#80269,#80270,#80271,#80272,#80273,#80274,#80275,#80276,#80277,#80278,
#80279,#80280,#80281,#80282,#80283,#80284,#80285,#80286,#80287,#80288,#80289,
#80290,#80291,#80292,#80293,#80294,#80295,#80296,#80297,#80298,#80299,#80300,
#80301,#80302,#80303,#80304,#80305,#80306,#80307,#80308,#80309,#80310,#80311,
#80312,#80313,#80314,#80315,#80316,#80317,#80318,#80319,#80320,#80321,#80322,
#80323,#80324),.UNSPECIFIED.,.F.,.F.,(4,3,3,3,3,3,3,3,3,3,3,3,3,3,3,3,3,
3,3,3,3,3,3,3,3,3,3,3,3,3,3,3,3,3,3,3,3,3,3,3,3,3,3,3,3,3,3,3,3,3,3,3,3,
3,3,3,3,4),(-16.6076077526091,-16.4985515258746,-16.3894995583923,-16.2803263451299,
-16.1710948393509,-16.061638988216,-15.9601053113919,-15.8509328552173,
-15.7398910894939,-15.6310189260239,-15.5222133036192,-15.4134342177412,
-15.3007253456633,-15.1918084691386,-15.0772035992843,-14.9625987294299,
-14.8534262116324,-14.7423844536118,-14.6335122268185,-14.5247065406372,
-14.4159273906366,-14.3032185798444,-14.1943016390933,-14.0796968932806,
-13.9650921474679,-13.8559199507005,-13.7448781525512,-13.636006247127,
-13.5272008815609,-13.4184220509095,-13.3057129295586,-13.1967963013489,
-13.0821909334274,-12.9675855655059,-12.8584129186525,-12.7473711767639,
-12.6384988273246,-12.529693021194,-12.42091375411,-12.3082050614685,-12.1992880120175,
-12.0846834977807,-11.9700789835439,-11.8609060285232,-11.7498643251556,
-11.6409916530149,-11.532185519713,-11.4234059215571,-11.3106975415633,
-11.2017801553197,-11.0871762784508,-10.9725724015819,-10.8631125115013,
-10.7538223022557,-10.6446684475115,-10.5355975774757,-10.4265343818605,
-10.3244224454296),.UNSPECIFIED.);
#854=B_SPLINE_CURVE_WITH_KNOTS('',3,(#80325,#80326,#80327,#80328,#80329,
#80330,#80331,#80332,#80333,#80334,#80335,#80336,#80337,#80338,#80339,#80340,
#80341,#80342,#80343,#80344,#80345,#80346,#80347,#80348,#80349,#80350,#80351,
#80352,#80353,#80354,#80355,#80356,#80357,#80358,#80359,#80360,#80361,#80362,
#80363,#80364,#80365,#80366,#80367,#80368,#80369,#80370,#80371,#80372,#80373,
#80374,#80375,#80376,#80377,#80378,#80379,#80380,#80381,#80382,#80383,#80384,
#80385,#80386,#80387,#80388,#80389,#80390,#80391,#80392,#80393,#80394,#80395,
#80396,#80397,#80398,#80399,#80400,#80401,#80402,#80403,#80404,#80405,#80406,
#80407,#80408,#80409,#80410,#80411,#80412,#80413,#80414,#80415,#80416,#80417,
#80418,#80419,#80420,#80421,#80422,#80423,#80424,#80425,#80426,#80427,#80428,
#80429,#80430,#80431,#80432,#80433,#80434,#80435,#80436,#80437,#80438,#80439,
#80440,#80441,#80442,#80443,#80444,#80445,#80446,#80447,#80448,#80449,#80450,
#80451,#80452,#80453,#80454,#80455,#80456,#80457,#80458,#80459,#80460,#80461,
#80462,#80463,#80464,#80465,#80466,#80467,#80468,#80469,#80470,#80471,#80472,
#80473,#80474,#80475,#80476,#80477,#80478,#80479,#80480,#80481,#80482,#80483,
#80484,#80485,#80486,#80487,#80488,#80489,#80490,#80491,#80492,#80493,#80494,
#80495,#80496),.UNSPECIFIED.,.F.,.F.,(4,3,3,3,3,3,3,3,3,3,3,3,3,3,3,3,3,
3,3,3,3,3,3,3,3,3,3,3,3,3,3,3,3,3,3,3,3,3,3,3,3,3,3,3,3,3,3,3,3,3,3,3,3,
3,3,3,3,4),(-10.3244224449829,-10.1995927077105,-10.073593116902,-9.97506581961992,
-9.86589120680441,-9.7548497106611,-9.64597543043115,-9.53716771174615,
-9.4283865532732,-9.31567972436938,-9.20676085735733,-9.09216004750763,
-8.97755923765793,-8.86838369578316,-8.75734231577226,-8.64846698531538,
-8.53965817465189,-8.43087588459778,-8.31817007737232,-8.20924999482244,
-8.09465132525919,-7.98005265569594,-7.87089564873598,-7.75985195186073,
-7.6509952491671,-7.54220504959516,-7.43344132405663,-7.32071751147596,
-7.2118156641143,-7.09718086892413,-6.98254607373395,-6.87335254294226,
-6.76231341154597,-6.65342046864044,-6.54459423251996,-6.43579473058479,
-6.32310592088158,-6.21416934992145,-6.0996044208467,-5.98503949177195,
-5.87585101044478,-5.76481124786543,-5.65592236636929,-5.54709981657177,
-5.43830362330433,-5.32561094493074,-5.21667671851355,-5.10210481416175,
-4.98753290980996,-4.87932161623076,-4.77130015508177,-4.66338411673174,
-4.55553201849392,-4.44770247128745,-4.33977959528017,-4.231810353224,-4.1236459576977,
-4.04123713858906),.UNSPECIFIED.);
#855=B_SPLINE_CURVE_WITH_KNOTS('',3,(#80499,#80500,#80501,#80502,#80503,
#80504,#80505,#80506,#80507,#80508,#80509,#80510,#80511,#80512,#80513,#80514,
#80515,#80516,#80517,#80518,#80519,#80520,#80521,#80522,#80523,#80524,#80525,
#80526,#80527,#80528,#80529,#80530,#80531,#80532,#80533,#80534,#80535,#80536,
#80537,#80538,#80539,#80540,#80541,#80542,#80543,#80544,#80545,#80546,#80547,
#80548,#80549,#80550,#80551,#80552,#80553,#80554,#80555,#80556,#80557,#80558,
#80559,#80560,#80561,#80562,#80563,#80564,#80565,#80566,#80567,#80568,#80569,
#80570,#80571,#80572,#80573,#80574,#80575,#80576,#80577,#80578,#80579,#80580,
#80581,#80582,#80583,#80584,#80585,#80586,#80587,#80588,#80589,#80590,#80591,
#80592,#80593,#80594,#80595,#80596,#80597,#80598,#80599,#80600,#80601,#80602,
#80603,#80604,#80605,#80606,#80607,#80608,#80609,#80610,#80611,#80612,#80613,
#80614,#80615,#80616,#80617,#80618,#80619,#80620,#80621,#80622,#80623,#80624,
#80625,#80626,#80627,#80628,#80629,#80630,#80631,#80632,#80633,#80634,#80635,
#80636,#80637,#80638,#80639,#80640,#80641,#80642,#80643,#80644,#80645,#80646,
#80647,#80648,#80649,#80650,#80651,#80652,#80653,#80654,#80655,#80656,#80657,
#80658,#80659,#80660,#80661,#80662,#80663,#80664,#80665,#80666,#80667,#80668,
#80669,#80670,#80671,#80672,#80673,#80674,#80675,#80676,#80677,#80678,#80679,
#80680,#80681,#80682),.UNSPECIFIED.,.F.,.F.,(4,2,2,2,2,2,2,2,2,2,2,2,2,
2,2,2,2,2,2,2,2,2,2,2,2,2,2,2,2,2,2,2,2,2,2,2,2,2,2,2,2,2,2,2,2,2,2,2,2,
2,2,2,2,2,2,2,2,2,2,2,2,2,2,2,2,2,2,2,2,2,2,2,2,2,2,2,2,2,2,2,2,2,2,2,2,
2,2,2,2,2,2,4),(0.00170434132766192,0.00222412714886743,0.00373601697648723,
0.0059415231071054,0.0117360227398377,0.017247955900676,0.017345838820968,
0.0174552527306371,0.0175774491000871,0.0374495435397178,0.0564270685292465,
0.0621405782386566,0.0652770672322874,0.0679619515167662,0.0712524927571661,
0.0763431234435016,0.102928841043105,0.123180376523087,0.126539422500572,
0.128307276186441,0.129676046129487,0.131560486136817,0.135367328950562,
0.152782962332486,0.167564078927962,0.178903712896266,0.182678939142569,
0.18821226293721,0.191298880215098,0.193967152687614,0.197269305304302,
0.202435535612447,0.22966587140207,0.244485620429274,0.249765905044866,
0.253630236470186,0.255506916157342,0.257001517832908,0.258873224420235,
0.262755254770772,0.281475463725533,0.303371544332112,0.313561671749094,
0.317406143038283,0.320124030405426,0.32258720604536,0.325900736712319,
0.334235710145613,0.362108165961765,0.377483591113132,0.381245848717689,
0.38309199948349,0.384434512856435,0.386250802041238,0.389713645455654,
0.415420966420263,0.431318841396034,0.438066890234673,0.443476504489122,
0.446530575575806,0.449190669476744,0.452508468110459,0.457752142300946,
0.478430974805413,0.497830187895307,0.502372988413577,0.507752871488063,
0.509887545386098,0.511409903047414,0.513114681621342,0.516141724622532,
0.535119214841241,0.550306121472088,0.561411665912576,0.565127868494102,
0.570591548050806,0.573654184871182,0.576309378965146,0.579604763978552,
0.586248897086325,0.616023804690947,0.627890307045252,0.634688156072327,
0.637011355795411,0.638564255999007,0.639990803976973,0.642464443964867,
0.649913308050295,0.672047429990563,0.686608283213725,0.693008730419268,
0.693071669236789),.UNSPECIFIED.);
#856=B_SPLINE_CURVE_WITH_KNOTS('',3,(#80685,#80686,#80687,#80688,#80689,
#80690,#80691,#80692,#80693,#80694,#80695,#80696,#80697,#80698,#80699,#80700,
#80701,#80702,#80703,#80704,#80705,#80706,#80707,#80708,#80709,#80710,#80711,
#80712,#80713,#80714,#80715,#80716,#80717,#80718,#80719,#80720,#80721,#80722,
#80723,#80724,#80725,#80726,#80727,#80728,#80729,#80730,#80731,#80732,#80733,
#80734,#80735,#80736,#80737,#80738,#80739,#80740,#80741,#80742,#80743,#80744,
#80745,#80746,#80747,#80748,#80749,#80750,#80751,#80752,#80753,#80754,#80755,
#80756,#80757,#80758,#80759,#80760,#80761,#80762,#80763,#80764,#80765,#80766,
#80767,#80768,#80769,#80770,#80771,#80772,#80773,#80774,#80775,#80776,#80777,
#80778,#80779,#80780,#80781,#80782,#80783,#80784,#80785,#80786,#80787,#80788,
#80789,#80790,#80791,#80792,#80793,#80794,#80795,#80796,#80797,#80798,#80799,
#80800,#80801,#80802,#80803,#80804,#80805,#80806,#80807,#80808,#80809,#80810,
#80811,#80812,#80813,#80814,#80815,#80816,#80817,#80818),.UNSPECIFIED.,
 .F.,.F.,(4,2,2,2,2,2,2,2,2,2,2,2,2,2,2,2,2,2,2,2,2,2,2,2,2,2,2,2,2,2,2,
2,2,2,2,2,2,2,2,2,2,2,2,2,2,2,2,2,2,2,2,2,2,2,2,2,2,2,2,2,2,2,2,2,2,2,4),
(-1.21432109392595,-1.21309489238909,-1.21161499497023,-1.20825651986386,
-1.19086412431765,-1.17341047878535,-1.16320924961495,-1.16000169195814,
-1.15685872449779,-1.15385408419519,-1.15026350757091,-1.14160636751801,
-1.11192084073898,-1.09879692054717,-1.09381828270841,-1.09021572424298,
-1.0886892369214,-1.08716890249636,-1.08551775590911,-1.08257570974892,
-1.06466749901094,-1.04288623040399,-1.03112489252229,-1.02718586039154,
-1.02452873706152,-1.02193600082763,-1.01819402636549,-1.00884615489993,
-0.978163101527409,-0.968318526508513,-0.962341623811722,-0.960198655696911,
-0.958712428561933,-0.957078828496771,-0.954369277831652,-0.944505008315516,
-0.92406809812312,-0.904827116101953,-0.89914520706868,-0.896014892835797,
-0.893329234251391,-0.890030050485331,-0.884910586675138,-0.858803055882306,
-0.844148749484679,-0.838902933278007,-0.835050012219561,-0.833154148950896,
-0.831632301850252,-0.82970469115684,-0.825608588436889,-0.796933686108921,
-0.778625224269768,-0.773093220731051,-0.770006727556216,-0.767338178168486,
-0.764035169042359,-0.758866437518332,-0.731636077449794,-0.716792357624474,
-0.711506749238995,-0.707639951393525,-0.705762701889296,-0.704267960777809,
-0.702396420488034,-0.698515765632526,-0.693046076597336),.UNSPECIFIED.);
#857=B_SPLINE_CURVE_WITH_KNOTS('',3,(#80823,#80824,#80825,#80826,#80827,
#80828,#80829,#80830,#80831,#80832,#80833,#80834,#80835,#80836,#80837,#80838,
#80839,#80840,#80841,#80842,#80843,#80844,#80845,#80846,#80847,#80848,#80849,
#80850,#80851,#80852,#80853,#80854,#80855,#80856,#80857,#80858,#80859,#80860,
#80861,#80862,#80863,#80864,#80865,#80866,#80867,#80868,#80869,#80870,#80871,
#80872,#80873,#80874,#80875,#80876,#80877,#80878,#80879,#80880,#80881,#80882,
#80883,#80884,#80885,#80886,#80887,#80888,#80889,#80890,#80891,#80892,#80893,
#80894,#80895,#80896,#80897,#80898),.UNSPECIFIED.,.F.,.F.,(4,3,3,3,3,3,
3,3,3,3,3,3,3,3,3,3,3,3,3,3,3,3,3,3,3,4),(-0.295806004217947,-0.276346276763905,
-0.259134503548442,-0.254903097588525,-0.235929794728117,-0.223290645753993,
-0.218631610496081,-0.200430896336404,-0.182506041781569,-0.171709967209082,
-0.162747187230736,-0.158780673832424,-0.1416815104781,-0.139485560058239,
-0.121912858869917,-0.106673751511178,-0.103639837841612,-0.0867995465133564,
-0.0700962905132021,-0.0537853027443874,-0.0504514462069721,-0.0476210400737898,
-0.0318234390049184,-0.0159117195024592,-0.000873246935291439,0.),
 .UNSPECIFIED.);
#858=B_SPLINE_CURVE_WITH_KNOTS('',3,(#80900,#80901,#80902,#80903),
 .UNSPECIFIED.,.F.,.F.,(4,4),(0.,0.0104675605378427),.UNSPECIFIED.);
#859=B_SPLINE_CURVE_WITH_KNOTS('',3,(#80904,#80905,#80906,#80907,#80908,
#80909,#80910,#80911,#80912,#80913,#80914,#80915,#80916,#80917,#80918,#80919,
#80920,#80921,#80922,#80923,#80924,#80925,#80926,#80927,#80928,#80929,#80930,
#80931,#80932,#80933,#80934,#80935,#80936,#80937,#80938,#80939,#80940,#80941,
#80942,#80943,#80944,#80945,#80946,#80947,#80948,#80949,#80950,#80951,#80952,
#80953,#80954,#80955,#80956,#80957,#80958,#80959,#80960,#80961,#80962,#80963,
#80964,#80965,#80966,#80967,#80968,#80969,#80970,#80971,#80972,#80973,#80974,
#80975,#80976,#80977,#80978,#80979,#80980,#80981,#80982),.UNSPECIFIED.,
 .F.,.F.,(4,3,3,3,3,3,3,3,3,3,3,3,3,3,3,3,3,3,3,3,3,3,3,3,3,3,4),(-0.300067541140031,
-0.284903583137558,-0.273513846777917,-0.269501705381138,-0.253425057571093,
-0.24192514309105,-0.238272923892424,-0.221674243793147,-0.204570474865403,
-0.187512420545603,-0.184305757918836,-0.181394803662524,-0.163580075937423,
-0.161367923522646,-0.144185213822354,-0.13484192266634,-0.12798949631024,
-0.123541197591128,-0.10530462789074,-0.0870680581903524,-0.0684458915674173,
-0.0648760934804545,-0.0612715484369567,-0.0420158017011555,-0.0227263924376532,
-0.00360798048806816,0.),.UNSPECIFIED.);
#860=B_SPLINE_CURVE_WITH_KNOTS('',3,(#81492,#81493,#81494,#81495),
 .UNSPECIFIED.,.F.,.F.,(4,4),(-0.0234817857221697,0.),.UNSPECIFIED.);
#861=B_SPLINE_CURVE_WITH_KNOTS('',3,(#81497,#81498,#81499,#81500,#81501,
#81502,#81503,#81504,#81505,#81506,#81507,#81508,#81509,#81510,#81511,#81512,
#81513,#81514,#81515,#81516,#81517,#81518,#81519,#81520,#81521,#81522,#81523,
#81524,#81525,#81526,#81527,#81528,#81529,#81530,#81531,#81532,#81533,#81534,
#81535,#81536,#81537,#81538,#81539,#81540,#81541,#81542,#81543,#81544,#81545,
#81546,#81547,#81548,#81549,#81550,#81551,#81552,#81553,#81554,#81555,#81556,
#81557,#81558,#81559,#81560,#81561,#81562,#81563,#81564,#81565,#81566,#81567,
#81568,#81569,#81570,#81571,#81572,#81573,#81574,#81575),.UNSPECIFIED.,
 .F.,.F.,(4,3,3,3,3,3,3,3,3,3,3,3,3,3,3,3,3,3,3,3,3,3,3,3,3,3,4),(-0.300067541140086,
-0.28490359311403,-0.273513832743188,-0.26950170426489,-0.253425062718846,
-0.241925147594606,-0.238272927914922,-0.221674254034694,-0.20457048503947,
-0.193769844660272,-0.184305769912281,-0.181394826747799,-0.163580099041372,
-0.161367923522675,-0.144185214827314,-0.134841924365739,-0.127989499740197,
-0.123541196970117,-0.105507157043589,-0.0870680627985426,-0.0684461374457819,
-0.06487607603814,-0.0612715444558154,-0.0420000585199136,-0.0227107712124592,
-0.00360796795722674,-1.56163160422294E-14),.UNSPECIFIED.);
#862=B_SPLINE_CURVE_WITH_KNOTS('',3,(#81576,#81577,#81578,#81579),
 .UNSPECIFIED.,.F.,.F.,(4,4),(-0.0104673718805252,0.),.UNSPECIFIED.);
#863=B_SPLINE_CURVE_WITH_KNOTS('',3,(#81584,#81585,#81586,#81587,#81588,
#81589,#81590,#81591,#81592,#81593,#81594,#81595,#81596,#81597,#81598,#81599,
#81600,#81601,#81602,#81603,#81604,#81605,#81606,#81607,#81608,#81609,#81610,
#81611,#81612,#81613,#81614,#81615,#81616,#81617,#81618,#81619,#81620,#81621,
#81622,#81623,#81624,#81625,#81626,#81627,#81628,#81629,#81630,#81631,#81632,
#81633,#81634,#81635,#81636,#81637,#81638,#81639,#81640,#81641,#81642,#81643,
#81644,#81645,#81646,#81647,#81648,#81649,#81650,#81651,#81652,#81653,#81654,
#81655,#81656,#81657,#81658,#81659),.UNSPECIFIED.,.F.,.F.,(4,3,3,3,3,3,
3,3,3,3,3,3,3,3,3,3,3,3,3,3,3,3,3,3,3,4),(-0.295805969970282,-0.276346242507802,
-0.259134493682388,-0.254903093723924,-0.235948130553021,-0.223290631511216,
-0.218631609492188,-0.200430890716852,-0.182506029139112,-0.171709957912945,
-0.162747174009377,-0.158780670974258,-0.141681498829962,-0.139485560058265,
-0.121907132417156,-0.106673752808531,-0.10363984067179,-0.0867987766194497,
-0.0702234074835109,-0.0537853237239207,-0.0504510919926865,-0.047620967918163,
-0.0318233773104902,-0.0159116886552451,-0.000873229362510297,0.),
 .UNSPECIFIED.);
#864=B_SPLINE_CURVE_WITH_KNOTS('',3,(#82169,#82170,#82171,#82172),
 .UNSPECIFIED.,.F.,.F.,(4,4),(-0.0234821165293861,0.),.UNSPECIFIED.);
#865=B_SPLINE_SURFACE_WITH_KNOTS('',5,1,((#37149,#37150),(#37151,#37152),
(#37153,#37154),(#37155,#37156),(#37157,#37158),(#37159,#37160),(#37161,
#37162),(#37163,#37164),(#37165,#37166),(#37167,#37168),(#37169,#37170),
(#37171,#37172),(#37173,#37174),(#37175,#37176),(#37177,#37178),(#37179,
#37180),(#37181,#37182),(#37183,#37184),(#37185,#37186),(#37187,#37188),
(#37189,#37190),(#37191,#37192),(#37193,#37194),(#37195,#37196),(#37197,
#37198),(#37199,#37200),(#37201,#37202),(#37203,#37204),(#37205,#37206),
(#37207,#37208),(#37209,#37210),(#37211,#37212),(#37213,#37214),(#37215,
#37216),(#37217,#37218)),.UNSPECIFIED.,.F.,.F.,.F.,(6,1,1,1,1,1,1,1,1,1,
1,1,1,1,1,1,1,1,1,1,1,1,1,1,1,1,1,1,1,1,6),(2,2),(0.,0.0333333333333333,
0.0666666666666667,0.1,0.133333333333333,0.166666666666667,0.2,0.233333333333333,
0.266666666666667,0.3,0.333333333333333,0.366666666666667,0.4,0.433333333333333,
0.466666666666667,0.5,0.533333333333333,0.566666666666667,0.6,0.633333333333333,
0.666666666666667,0.7,0.733333333333333,0.766666666666667,0.8,0.833333333333333,
0.866666666666667,0.9,0.933333333333333,0.966666666666667,1.),(0.,0.762),
 .UNSPECIFIED.);
#866=B_SPLINE_SURFACE_WITH_KNOTS('',5,1,((#37298,#37299),(#37300,#37301),
(#37302,#37303),(#37304,#37305),(#37306,#37307),(#37308,#37309),(#37310,
#37311),(#37312,#37313),(#37314,#37315),(#37316,#37317),(#37318,#37319),
(#37320,#37321),(#37322,#37323),(#37324,#37325),(#37326,#37327),(#37328,
#37329),(#37330,#37331),(#37332,#37333),(#37334,#37335),(#37336,#37337),
(#37338,#37339),(#37340,#37341),(#37342,#37343),(#37344,#37345),(#37346,
#37347),(#37348,#37349),(#37350,#37351),(#37352,#37353),(#37354,#37355),
(#37356,#37357),(#37358,#37359),(#37360,#37361),(#37362,#37363),(#37364,
#37365),(#37366,#37367)),.UNSPECIFIED.,.F.,.F.,.F.,(6,1,1,1,1,1,1,1,1,1,
1,1,1,1,1,1,1,1,1,1,1,1,1,1,1,1,1,1,1,1,6),(2,2),(-1.,-0.966666666666667,
-0.933333333333333,-0.9,-0.866666666666667,-0.833333333333333,-0.8,-0.766666666666667,
-0.733333333333333,-0.7,-0.666666666666667,-0.633333333333333,-0.6,-0.566666666666667,
-0.533333333333333,-0.5,-0.466666666666667,-0.433333333333333,-0.4,-0.366666666666667,
-0.333333333333333,-0.3,-0.266666666666667,-0.233333333333333,-0.2,-0.166666666666667,
-0.133333333333333,-0.1,-0.0666666666666667,-0.0333333333333333,0.),(0.,
0.762),.UNSPECIFIED.);
#867=B_SPLINE_SURFACE_WITH_KNOTS('',5,1,((#38656,#38657),(#38658,#38659),
(#38660,#38661),(#38662,#38663),(#38664,#38665),(#38666,#38667),(#38668,
#38669),(#38670,#38671),(#38672,#38673),(#38674,#38675),(#38676,#38677),
(#38678,#38679),(#38680,#38681),(#38682,#38683),(#38684,#38685),(#38686,
#38687),(#38688,#38689),(#38690,#38691),(#38692,#38693),(#38694,#38695),
(#38696,#38697),(#38698,#38699),(#38700,#38701),(#38702,#38703),(#38704,
#38705),(#38706,#38707),(#38708,#38709),(#38710,#38711),(#38712,#38713),
(#38714,#38715),(#38716,#38717),(#38718,#38719),(#38720,#38721),(#38722,
#38723),(#38724,#38725)),.UNSPECIFIED.,.F.,.F.,.F.,(6,1,1,1,1,1,1,1,1,1,
1,1,1,1,1,1,1,1,1,1,1,1,1,1,1,1,1,1,1,1,6),(2,2),(0.,0.0333333333333333,
0.0666666666666667,0.1,0.133333333333333,0.166666666666667,0.2,0.233333333333333,
0.266666666666667,0.3,0.333333333333333,0.366666666666667,0.4,0.433333333333333,
0.466666666666667,0.5,0.533333333333333,0.566666666666667,0.6,0.633333333333333,
0.666666666666667,0.7,0.733333333333333,0.766666666666667,0.8,0.833333333333333,
0.866666666666667,0.9,0.933333333333333,0.966666666666667,1.),(0.,0.762),
 .UNSPECIFIED.);
#868=B_SPLINE_SURFACE_WITH_KNOTS('',5,1,((#38767,#38768),(#38769,#38770),
(#38771,#38772),(#38773,#38774),(#38775,#38776),(#38777,#38778),(#38779,
#38780),(#38781,#38782),(#38783,#38784),(#38785,#38786),(#38787,#38788),
(#38789,#38790),(#38791,#38792),(#38793,#38794),(#38795,#38796),(#38797,
#38798),(#38799,#38800),(#38801,#38802),(#38803,#38804),(#38805,#38806),
(#38807,#38808),(#38809,#38810),(#38811,#38812),(#38813,#38814),(#38815,
#38816),(#38817,#38818),(#38819,#38820),(#38821,#38822),(#38823,#38824),
(#38825,#38826),(#38827,#38828),(#38829,#38830),(#38831,#38832),(#38833,
#38834),(#38835,#38836)),.UNSPECIFIED.,.F.,.F.,.F.,(6,1,1,1,1,1,1,1,1,1,
1,1,1,1,1,1,1,1,1,1,1,1,1,1,1,1,1,1,1,1,6),(2,2),(-1.,-0.966666666666667,
-0.933333333333333,-0.9,-0.866666666666667,-0.833333333333333,-0.8,-0.766666666666667,
-0.733333333333333,-0.7,-0.666666666666667,-0.633333333333333,-0.6,-0.566666666666667,
-0.533333333333333,-0.5,-0.466666666666667,-0.433333333333333,-0.4,-0.366666666666667,
-0.333333333333333,-0.3,-0.266666666666667,-0.233333333333333,-0.2,-0.166666666666667,
-0.133333333333333,-0.1,-0.0666666666666667,-0.0333333333333333,0.),(0.,
0.762),.UNSPECIFIED.);
#869=B_SPLINE_SURFACE_WITH_KNOTS('',5,1,((#38886,#38887),(#38888,#38889),
(#38890,#38891),(#38892,#38893),(#38894,#38895),(#38896,#38897),(#38898,
#38899),(#38900,#38901),(#38902,#38903),(#38904,#38905),(#38906,#38907),
(#38908,#38909),(#38910,#38911),(#38912,#38913),(#38914,#38915),(#38916,
#38917),(#38918,#38919),(#38920,#38921),(#38922,#38923),(#38924,#38925),
(#38926,#38927),(#38928,#38929),(#38930,#38931),(#38932,#38933),(#38934,
#38935),(#38936,#38937),(#38938,#38939),(#38940,#38941),(#38942,#38943),
(#38944,#38945),(#38946,#38947),(#38948,#38949),(#38950,#38951),(#38952,
#38953),(#38954,#38955)),.UNSPECIFIED.,.F.,.F.,.F.,(6,1,1,1,1,1,1,1,1,1,
1,1,1,1,1,1,1,1,1,1,1,1,1,1,1,1,1,1,1,1,6),(2,2),(0.,0.0333333333333333,
0.0666666666666667,0.1,0.133333333333333,0.166666666666667,0.2,0.233333333333333,
0.266666666666667,0.3,0.333333333333333,0.366666666666667,0.4,0.433333333333333,
0.466666666666667,0.5,0.533333333333333,0.566666666666667,0.6,0.633333333333333,
0.666666666666667,0.7,0.733333333333333,0.766666666666667,0.8,0.833333333333333,
0.866666666666667,0.9,0.933333333333333,0.966666666666667,1.),(0.,0.762),
 .UNSPECIFIED.);
#870=B_SPLINE_SURFACE_WITH_KNOTS('',5,1,((#38997,#38998),(#38999,#39000),
(#39001,#39002),(#39003,#39004),(#39005,#39006),(#39007,#39008),(#39009,
#39010),(#39011,#39012),(#39013,#39014),(#39015,#39016),(#39017,#39018),
(#39019,#39020),(#39021,#39022),(#39023,#39024),(#39025,#39026),(#39027,
#39028),(#39029,#39030),(#39031,#39032),(#39033,#39034),(#39035,#39036),
(#39037,#39038),(#39039,#39040),(#39041,#39042),(#39043,#39044),(#39045,
#39046),(#39047,#39048),(#39049,#39050),(#39051,#39052),(#39053,#39054),
(#39055,#39056),(#39057,#39058),(#39059,#39060),(#39061,#39062),(#39063,
#39064),(#39065,#39066)),.UNSPECIFIED.,.F.,.F.,.F.,(6,1,1,1,1,1,1,1,1,1,
1,1,1,1,1,1,1,1,1,1,1,1,1,1,1,1,1,1,1,1,6),(2,2),(-1.,-0.966666666666667,
-0.933333333333333,-0.9,-0.866666666666667,-0.833333333333333,-0.8,-0.766666666666667,
-0.733333333333333,-0.7,-0.666666666666667,-0.633333333333333,-0.6,-0.566666666666667,
-0.533333333333333,-0.5,-0.466666666666667,-0.433333333333333,-0.4,-0.366666666666667,
-0.333333333333333,-0.3,-0.266666666666667,-0.233333333333333,-0.2,-0.166666666666667,
-0.133333333333333,-0.1,-0.0666666666666667,-0.0333333333333333,0.),(0.,
0.762),.UNSPECIFIED.);
#871=B_SPLINE_SURFACE_WITH_KNOTS('',5,1,((#39116,#39117),(#39118,#39119),
(#39120,#39121),(#39122,#39123),(#39124,#39125),(#39126,#39127),(#39128,
#39129),(#39130,#39131),(#39132,#39133),(#39134,#39135),(#39136,#39137),
(#39138,#39139),(#39140,#39141),(#39142,#39143),(#39144,#39145),(#39146,
#39147),(#39148,#39149),(#39150,#39151),(#39152,#39153),(#39154,#39155),
(#39156,#39157),(#39158,#39159),(#39160,#39161),(#39162,#39163),(#39164,
#39165),(#39166,#39167),(#39168,#39169),(#39170,#39171),(#39172,#39173),
(#39174,#39175),(#39176,#39177),(#39178,#39179),(#39180,#39181),(#39182,
#39183),(#39184,#39185)),.UNSPECIFIED.,.F.,.F.,.F.,(6,1,1,1,1,1,1,1,1,1,
1,1,1,1,1,1,1,1,1,1,1,1,1,1,1,1,1,1,1,1,6),(2,2),(0.,0.0333333333333333,
0.0666666666666667,0.1,0.133333333333333,0.166666666666667,0.2,0.233333333333333,
0.266666666666667,0.3,0.333333333333333,0.366666666666667,0.4,0.433333333333333,
0.466666666666667,0.5,0.533333333333333,0.566666666666667,0.6,0.633333333333333,
0.666666666666667,0.7,0.733333333333333,0.766666666666667,0.8,0.833333333333333,
0.866666666666667,0.9,0.933333333333333,0.966666666666667,1.),(0.,0.762),
 .UNSPECIFIED.);
#872=B_SPLINE_SURFACE_WITH_KNOTS('',5,1,((#39227,#39228),(#39229,#39230),
(#39231,#39232),(#39233,#39234),(#39235,#39236),(#39237,#39238),(#39239,
#39240),(#39241,#39242),(#39243,#39244),(#39245,#39246),(#39247,#39248),
(#39249,#39250),(#39251,#39252),(#39253,#39254),(#39255,#39256),(#39257,
#39258),(#39259,#39260),(#39261,#39262),(#39263,#39264),(#39265,#39266),
(#39267,#39268),(#39269,#39270),(#39271,#39272),(#39273,#39274),(#39275,
#39276),(#39277,#39278),(#39279,#39280),(#39281,#39282),(#39283,#39284),
(#39285,#39286),(#39287,#39288),(#39289,#39290),(#39291,#39292),(#39293,
#39294),(#39295,#39296)),.UNSPECIFIED.,.F.,.F.,.F.,(6,1,1,1,1,1,1,1,1,1,
1,1,1,1,1,1,1,1,1,1,1,1,1,1,1,1,1,1,1,1,6),(2,2),(-1.,-0.966666666666667,
-0.933333333333333,-0.9,-0.866666666666667,-0.833333333333333,-0.8,-0.766666666666667,
-0.733333333333333,-0.7,-0.666666666666667,-0.633333333333333,-0.6,-0.566666666666667,
-0.533333333333333,-0.5,-0.466666666666667,-0.433333333333333,-0.4,-0.366666666666667,
-0.333333333333333,-0.3,-0.266666666666667,-0.233333333333333,-0.2,-0.166666666666667,
-0.133333333333333,-0.1,-0.0666666666666667,-0.0333333333333333,0.),(0.,
0.762),.UNSPECIFIED.);
#873=B_SPLINE_SURFACE_WITH_KNOTS('',5,1,((#39346,#39347),(#39348,#39349),
(#39350,#39351),(#39352,#39353),(#39354,#39355),(#39356,#39357),(#39358,
#39359),(#39360,#39361),(#39362,#39363),(#39364,#39365),(#39366,#39367),
(#39368,#39369),(#39370,#39371),(#39372,#39373),(#39374,#39375),(#39376,
#39377),(#39378,#39379),(#39380,#39381),(#39382,#39383),(#39384,#39385),
(#39386,#39387),(#39388,#39389),(#39390,#39391),(#39392,#39393),(#39394,
#39395),(#39396,#39397),(#39398,#39399),(#39400,#39401),(#39402,#39403),
(#39404,#39405),(#39406,#39407),(#39408,#39409),(#39410,#39411),(#39412,
#39413),(#39414,#39415)),.UNSPECIFIED.,.F.,.F.,.F.,(6,1,1,1,1,1,1,1,1,1,
1,1,1,1,1,1,1,1,1,1,1,1,1,1,1,1,1,1,1,1,6),(2,2),(0.,0.0333333333333333,
0.0666666666666667,0.1,0.133333333333333,0.166666666666667,0.2,0.233333333333333,
0.266666666666667,0.3,0.333333333333333,0.366666666666667,0.4,0.433333333333333,
0.466666666666667,0.5,0.533333333333333,0.566666666666667,0.6,0.633333333333333,
0.666666666666667,0.7,0.733333333333333,0.766666666666667,0.8,0.833333333333333,
0.866666666666667,0.9,0.933333333333333,0.966666666666667,1.),(0.,0.762),
 .UNSPECIFIED.);
#874=B_SPLINE_SURFACE_WITH_KNOTS('',5,1,((#39457,#39458),(#39459,#39460),
(#39461,#39462),(#39463,#39464),(#39465,#39466),(#39467,#39468),(#39469,
#39470),(#39471,#39472),(#39473,#39474),(#39475,#39476),(#39477,#39478),
(#39479,#39480),(#39481,#39482),(#39483,#39484),(#39485,#39486),(#39487,
#39488),(#39489,#39490),(#39491,#39492),(#39493,#39494),(#39495,#39496),
(#39497,#39498),(#39499,#39500),(#39501,#39502),(#39503,#39504),(#39505,
#39506),(#39507,#39508),(#39509,#39510),(#39511,#39512),(#39513,#39514),
(#39515,#39516),(#39517,#39518),(#39519,#39520),(#39521,#39522),(#39523,
#39524),(#39525,#39526)),.UNSPECIFIED.,.F.,.F.,.F.,(6,1,1,1,1,1,1,1,1,1,
1,1,1,1,1,1,1,1,1,1,1,1,1,1,1,1,1,1,1,1,6),(2,2),(-1.,-0.966666666666667,
-0.933333333333333,-0.9,-0.866666666666667,-0.833333333333333,-0.8,-0.766666666666667,
-0.733333333333333,-0.7,-0.666666666666667,-0.633333333333333,-0.6,-0.566666666666667,
-0.533333333333333,-0.5,-0.466666666666667,-0.433333333333333,-0.4,-0.366666666666667,
-0.333333333333333,-0.3,-0.266666666666667,-0.233333333333333,-0.2,-0.166666666666667,
-0.133333333333333,-0.1,-0.0666666666666667,-0.0333333333333333,0.),(0.,
0.762),.UNSPECIFIED.);
#875=B_SPLINE_SURFACE_WITH_KNOTS('',5,1,((#39576,#39577),(#39578,#39579),
(#39580,#39581),(#39582,#39583),(#39584,#39585),(#39586,#39587),(#39588,
#39589),(#39590,#39591),(#39592,#39593),(#39594,#39595),(#39596,#39597),
(#39598,#39599),(#39600,#39601),(#39602,#39603),(#39604,#39605),(#39606,
#39607),(#39608,#39609),(#39610,#39611),(#39612,#39613),(#39614,#39615),
(#39616,#39617),(#39618,#39619),(#39620,#39621),(#39622,#39623),(#39624,
#39625),(#39626,#39627),(#39628,#39629),(#39630,#39631),(#39632,#39633),
(#39634,#39635),(#39636,#39637),(#39638,#39639),(#39640,#39641),(#39642,
#39643),(#39644,#39645)),.UNSPECIFIED.,.F.,.F.,.F.,(6,1,1,1,1,1,1,1,1,1,
1,1,1,1,1,1,1,1,1,1,1,1,1,1,1,1,1,1,1,1,6),(2,2),(0.,0.0333333333333333,
0.0666666666666667,0.1,0.133333333333333,0.166666666666667,0.2,0.233333333333333,
0.266666666666667,0.3,0.333333333333333,0.366666666666667,0.4,0.433333333333333,
0.466666666666667,0.5,0.533333333333333,0.566666666666667,0.6,0.633333333333333,
0.666666666666667,0.7,0.733333333333333,0.766666666666667,0.8,0.833333333333333,
0.866666666666667,0.9,0.933333333333333,0.966666666666667,1.),(0.,0.762),
 .UNSPECIFIED.);
#876=B_SPLINE_SURFACE_WITH_KNOTS('',5,1,((#39687,#39688),(#39689,#39690),
(#39691,#39692),(#39693,#39694),(#39695,#39696),(#39697,#39698),(#39699,
#39700),(#39701,#39702),(#39703,#39704),(#39705,#39706),(#39707,#39708),
(#39709,#39710),(#39711,#39712),(#39713,#39714),(#39715,#39716),(#39717,
#39718),(#39719,#39720),(#39721,#39722),(#39723,#39724),(#39725,#39726),
(#39727,#39728),(#39729,#39730),(#39731,#39732),(#39733,#39734),(#39735,
#39736),(#39737,#39738),(#39739,#39740),(#39741,#39742),(#39743,#39744),
(#39745,#39746),(#39747,#39748),(#39749,#39750),(#39751,#39752),(#39753,
#39754),(#39755,#39756)),.UNSPECIFIED.,.F.,.F.,.F.,(6,1,1,1,1,1,1,1,1,1,
1,1,1,1,1,1,1,1,1,1,1,1,1,1,1,1,1,1,1,1,6),(2,2),(-1.,-0.966666666666667,
-0.933333333333333,-0.9,-0.866666666666667,-0.833333333333333,-0.8,-0.766666666666667,
-0.733333333333333,-0.7,-0.666666666666667,-0.633333333333333,-0.6,-0.566666666666667,
-0.533333333333333,-0.5,-0.466666666666667,-0.433333333333333,-0.4,-0.366666666666667,
-0.333333333333333,-0.3,-0.266666666666667,-0.233333333333333,-0.2,-0.166666666666667,
-0.133333333333333,-0.1,-0.0666666666666667,-0.0333333333333333,0.),(0.,
0.762),.UNSPECIFIED.);
#877=B_SPLINE_SURFACE_WITH_KNOTS('',5,1,((#39806,#39807),(#39808,#39809),
(#39810,#39811),(#39812,#39813),(#39814,#39815),(#39816,#39817),(#39818,
#39819),(#39820,#39821),(#39822,#39823),(#39824,#39825),(#39826,#39827),
(#39828,#39829),(#39830,#39831),(#39832,#39833),(#39834,#39835),(#39836,
#39837),(#39838,#39839),(#39840,#39841),(#39842,#39843),(#39844,#39845),
(#39846,#39847),(#39848,#39849),(#39850,#39851),(#39852,#39853),(#39854,
#39855),(#39856,#39857),(#39858,#39859),(#39860,#39861),(#39862,#39863),
(#39864,#39865),(#39866,#39867),(#39868,#39869),(#39870,#39871),(#39872,
#39873),(#39874,#39875)),.UNSPECIFIED.,.F.,.F.,.F.,(6,1,1,1,1,1,1,1,1,1,
1,1,1,1,1,1,1,1,1,1,1,1,1,1,1,1,1,1,1,1,6),(2,2),(0.,0.0333333333333333,
0.0666666666666667,0.1,0.133333333333333,0.166666666666667,0.2,0.233333333333333,
0.266666666666667,0.3,0.333333333333333,0.366666666666667,0.4,0.433333333333333,
0.466666666666667,0.5,0.533333333333333,0.566666666666667,0.6,0.633333333333333,
0.666666666666667,0.7,0.733333333333333,0.766666666666667,0.8,0.833333333333333,
0.866666666666667,0.9,0.933333333333333,0.966666666666667,1.),(0.,0.762),
 .UNSPECIFIED.);
#878=B_SPLINE_SURFACE_WITH_KNOTS('',5,1,((#39917,#39918),(#39919,#39920),
(#39921,#39922),(#39923,#39924),(#39925,#39926),(#39927,#39928),(#39929,
#39930),(#39931,#39932),(#39933,#39934),(#39935,#39936),(#39937,#39938),
(#39939,#39940),(#39941,#39942),(#39943,#39944),(#39945,#39946),(#39947,
#39948),(#39949,#39950),(#39951,#39952),(#39953,#39954),(#39955,#39956),
(#39957,#39958),(#39959,#39960),(#39961,#39962),(#39963,#39964),(#39965,
#39966),(#39967,#39968),(#39969,#39970),(#39971,#39972),(#39973,#39974),
(#39975,#39976),(#39977,#39978),(#39979,#39980),(#39981,#39982),(#39983,
#39984),(#39985,#39986)),.UNSPECIFIED.,.F.,.F.,.F.,(6,1,1,1,1,1,1,1,1,1,
1,1,1,1,1,1,1,1,1,1,1,1,1,1,1,1,1,1,1,1,6),(2,2),(-1.,-0.966666666666667,
-0.933333333333333,-0.9,-0.866666666666667,-0.833333333333333,-0.8,-0.766666666666667,
-0.733333333333333,-0.7,-0.666666666666667,-0.633333333333333,-0.6,-0.566666666666667,
-0.533333333333333,-0.5,-0.466666666666667,-0.433333333333333,-0.4,-0.366666666666667,
-0.333333333333333,-0.3,-0.266666666666667,-0.233333333333333,-0.2,-0.166666666666667,
-0.133333333333333,-0.1,-0.0666666666666667,-0.0333333333333333,0.),(0.,
0.762),.UNSPECIFIED.);
#879=B_SPLINE_SURFACE_WITH_KNOTS('',5,1,((#40036,#40037),(#40038,#40039),
(#40040,#40041),(#40042,#40043),(#40044,#40045),(#40046,#40047),(#40048,
#40049),(#40050,#40051),(#40052,#40053),(#40054,#40055),(#40056,#40057),
(#40058,#40059),(#40060,#40061),(#40062,#40063),(#40064,#40065),(#40066,
#40067),(#40068,#40069),(#40070,#40071),(#40072,#40073),(#40074,#40075),
(#40076,#40077),(#40078,#40079),(#40080,#40081),(#40082,#40083),(#40084,
#40085),(#40086,#40087),(#40088,#40089),(#40090,#40091),(#40092,#40093),
(#40094,#40095),(#40096,#40097),(#40098,#40099),(#40100,#40101),(#40102,
#40103),(#40104,#40105)),.UNSPECIFIED.,.F.,.F.,.F.,(6,1,1,1,1,1,1,1,1,1,
1,1,1,1,1,1,1,1,1,1,1,1,1,1,1,1,1,1,1,1,6),(2,2),(0.,0.0333333333333333,
0.0666666666666667,0.1,0.133333333333333,0.166666666666667,0.2,0.233333333333333,
0.266666666666667,0.3,0.333333333333333,0.366666666666667,0.4,0.433333333333333,
0.466666666666667,0.5,0.533333333333333,0.566666666666667,0.6,0.633333333333333,
0.666666666666667,0.7,0.733333333333333,0.766666666666667,0.8,0.833333333333333,
0.866666666666667,0.9,0.933333333333333,0.966666666666667,1.),(0.,0.762),
 .UNSPECIFIED.);
#880=B_SPLINE_SURFACE_WITH_KNOTS('',5,1,((#40147,#40148),(#40149,#40150),
(#40151,#40152),(#40153,#40154),(#40155,#40156),(#40157,#40158),(#40159,
#40160),(#40161,#40162),(#40163,#40164),(#40165,#40166),(#40167,#40168),
(#40169,#40170),(#40171,#40172),(#40173,#40174),(#40175,#40176),(#40177,
#40178),(#40179,#40180),(#40181,#40182),(#40183,#40184),(#40185,#40186),
(#40187,#40188),(#40189,#40190),(#40191,#40192),(#40193,#40194),(#40195,
#40196),(#40197,#40198),(#40199,#40200),(#40201,#40202),(#40203,#40204),
(#40205,#40206),(#40207,#40208),(#40209,#40210),(#40211,#40212),(#40213,
#40214),(#40215,#40216)),.UNSPECIFIED.,.F.,.F.,.F.,(6,1,1,1,1,1,1,1,1,1,
1,1,1,1,1,1,1,1,1,1,1,1,1,1,1,1,1,1,1,1,6),(2,2),(-1.,-0.966666666666667,
-0.933333333333333,-0.9,-0.866666666666667,-0.833333333333333,-0.8,-0.766666666666667,
-0.733333333333333,-0.7,-0.666666666666667,-0.633333333333333,-0.6,-0.566666666666667,
-0.533333333333333,-0.5,-0.466666666666667,-0.433333333333333,-0.4,-0.366666666666667,
-0.333333333333333,-0.3,-0.266666666666667,-0.233333333333333,-0.2,-0.166666666666667,
-0.133333333333333,-0.1,-0.0666666666666667,-0.0333333333333333,0.),(0.,
0.762),.UNSPECIFIED.);
#881=B_SPLINE_SURFACE_WITH_KNOTS('',5,1,((#40266,#40267),(#40268,#40269),
(#40270,#40271),(#40272,#40273),(#40274,#40275),(#40276,#40277),(#40278,
#40279),(#40280,#40281),(#40282,#40283),(#40284,#40285),(#40286,#40287),
(#40288,#40289),(#40290,#40291),(#40292,#40293),(#40294,#40295),(#40296,
#40297),(#40298,#40299),(#40300,#40301),(#40302,#40303),(#40304,#40305),
(#40306,#40307),(#40308,#40309),(#40310,#40311),(#40312,#40313),(#40314,
#40315),(#40316,#40317),(#40318,#40319),(#40320,#40321),(#40322,#40323),
(#40324,#40325),(#40326,#40327),(#40328,#40329),(#40330,#40331),(#40332,
#40333),(#40334,#40335)),.UNSPECIFIED.,.F.,.F.,.F.,(6,1,1,1,1,1,1,1,1,1,
1,1,1,1,1,1,1,1,1,1,1,1,1,1,1,1,1,1,1,1,6),(2,2),(0.,0.0333333333333333,
0.0666666666666667,0.1,0.133333333333333,0.166666666666667,0.2,0.233333333333333,
0.266666666666667,0.3,0.333333333333333,0.366666666666667,0.4,0.433333333333333,
0.466666666666667,0.5,0.533333333333333,0.566666666666667,0.6,0.633333333333333,
0.666666666666667,0.7,0.733333333333333,0.766666666666667,0.8,0.833333333333333,
0.866666666666667,0.9,0.933333333333333,0.966666666666667,1.),(0.,0.762),
 .UNSPECIFIED.);
#882=B_SPLINE_SURFACE_WITH_KNOTS('',5,1,((#40377,#40378),(#40379,#40380),
(#40381,#40382),(#40383,#40384),(#40385,#40386),(#40387,#40388),(#40389,
#40390),(#40391,#40392),(#40393,#40394),(#40395,#40396),(#40397,#40398),
(#40399,#40400),(#40401,#40402),(#40403,#40404),(#40405,#40406),(#40407,
#40408),(#40409,#40410),(#40411,#40412),(#40413,#40414),(#40415,#40416),
(#40417,#40418),(#40419,#40420),(#40421,#40422),(#40423,#40424),(#40425,
#40426),(#40427,#40428),(#40429,#40430),(#40431,#40432),(#40433,#40434),
(#40435,#40436),(#40437,#40438),(#40439,#40440),(#40441,#40442),(#40443,
#40444),(#40445,#40446)),.UNSPECIFIED.,.F.,.F.,.F.,(6,1,1,1,1,1,1,1,1,1,
1,1,1,1,1,1,1,1,1,1,1,1,1,1,1,1,1,1,1,1,6),(2,2),(-1.,-0.966666666666667,
-0.933333333333333,-0.9,-0.866666666666667,-0.833333333333333,-0.8,-0.766666666666667,
-0.733333333333333,-0.7,-0.666666666666667,-0.633333333333333,-0.6,-0.566666666666667,
-0.533333333333333,-0.5,-0.466666666666667,-0.433333333333333,-0.4,-0.366666666666667,
-0.333333333333333,-0.3,-0.266666666666667,-0.233333333333333,-0.2,-0.166666666666667,
-0.133333333333333,-0.1,-0.0666666666666667,-0.0333333333333333,0.),(0.,
0.762),.UNSPECIFIED.);
#883=B_SPLINE_SURFACE_WITH_KNOTS('',5,1,((#40496,#40497),(#40498,#40499),
(#40500,#40501),(#40502,#40503),(#40504,#40505),(#40506,#40507),(#40508,
#40509),(#40510,#40511),(#40512,#40513),(#40514,#40515),(#40516,#40517),
(#40518,#40519),(#40520,#40521),(#40522,#40523),(#40524,#40525),(#40526,
#40527),(#40528,#40529),(#40530,#40531),(#40532,#40533),(#40534,#40535),
(#40536,#40537),(#40538,#40539),(#40540,#40541),(#40542,#40543),(#40544,
#40545),(#40546,#40547),(#40548,#40549),(#40550,#40551),(#40552,#40553),
(#40554,#40555),(#40556,#40557),(#40558,#40559),(#40560,#40561),(#40562,
#40563),(#40564,#40565)),.UNSPECIFIED.,.F.,.F.,.F.,(6,1,1,1,1,1,1,1,1,1,
1,1,1,1,1,1,1,1,1,1,1,1,1,1,1,1,1,1,1,1,6),(2,2),(0.,0.0333333333333333,
0.0666666666666667,0.1,0.133333333333333,0.166666666666667,0.2,0.233333333333333,
0.266666666666667,0.3,0.333333333333333,0.366666666666667,0.4,0.433333333333333,
0.466666666666667,0.5,0.533333333333333,0.566666666666667,0.6,0.633333333333333,
0.666666666666667,0.7,0.733333333333333,0.766666666666667,0.8,0.833333333333333,
0.866666666666667,0.9,0.933333333333333,0.966666666666667,1.),(0.,0.762),
 .UNSPECIFIED.);
#884=B_SPLINE_SURFACE_WITH_KNOTS('',5,1,((#40607,#40608),(#40609,#40610),
(#40611,#40612),(#40613,#40614),(#40615,#40616),(#40617,#40618),(#40619,
#40620),(#40621,#40622),(#40623,#40624),(#40625,#40626),(#40627,#40628),
(#40629,#40630),(#40631,#40632),(#40633,#40634),(#40635,#40636),(#40637,
#40638),(#40639,#40640),(#40641,#40642),(#40643,#40644),(#40645,#40646),
(#40647,#40648),(#40649,#40650),(#40651,#40652),(#40653,#40654),(#40655,
#40656),(#40657,#40658),(#40659,#40660),(#40661,#40662),(#40663,#40664),
(#40665,#40666),(#40667,#40668),(#40669,#40670),(#40671,#40672),(#40673,
#40674),(#40675,#40676)),.UNSPECIFIED.,.F.,.F.,.F.,(6,1,1,1,1,1,1,1,1,1,
1,1,1,1,1,1,1,1,1,1,1,1,1,1,1,1,1,1,1,1,6),(2,2),(-1.,-0.966666666666667,
-0.933333333333333,-0.9,-0.866666666666667,-0.833333333333333,-0.8,-0.766666666666667,
-0.733333333333333,-0.7,-0.666666666666667,-0.633333333333333,-0.6,-0.566666666666667,
-0.533333333333333,-0.5,-0.466666666666667,-0.433333333333333,-0.4,-0.366666666666667,
-0.333333333333333,-0.3,-0.266666666666667,-0.233333333333333,-0.2,-0.166666666666667,
-0.133333333333333,-0.1,-0.0666666666666667,-0.0333333333333333,0.),(0.,
0.762),.UNSPECIFIED.);
#885=B_SPLINE_SURFACE_WITH_KNOTS('',5,1,((#40726,#40727),(#40728,#40729),
(#40730,#40731),(#40732,#40733),(#40734,#40735),(#40736,#40737),(#40738,
#40739),(#40740,#40741),(#40742,#40743),(#40744,#40745),(#40746,#40747),
(#40748,#40749),(#40750,#40751),(#40752,#40753),(#40754,#40755),(#40756,
#40757),(#40758,#40759),(#40760,#40761),(#40762,#40763),(#40764,#40765),
(#40766,#40767),(#40768,#40769),(#40770,#40771),(#40772,#40773),(#40774,
#40775),(#40776,#40777),(#40778,#40779),(#40780,#40781),(#40782,#40783),
(#40784,#40785),(#40786,#40787),(#40788,#40789),(#40790,#40791),(#40792,
#40793),(#40794,#40795)),.UNSPECIFIED.,.F.,.F.,.F.,(6,1,1,1,1,1,1,1,1,1,
1,1,1,1,1,1,1,1,1,1,1,1,1,1,1,1,1,1,1,1,6),(2,2),(0.,0.0333333333333333,
0.0666666666666667,0.1,0.133333333333333,0.166666666666667,0.2,0.233333333333333,
0.266666666666667,0.3,0.333333333333333,0.366666666666667,0.4,0.433333333333333,
0.466666666666667,0.5,0.533333333333333,0.566666666666667,0.6,0.633333333333333,
0.666666666666667,0.7,0.733333333333333,0.766666666666667,0.8,0.833333333333333,
0.866666666666667,0.9,0.933333333333333,0.966666666666667,1.),(0.,0.762),
 .UNSPECIFIED.);
#886=B_SPLINE_SURFACE_WITH_KNOTS('',5,1,((#40837,#40838),(#40839,#40840),
(#40841,#40842),(#40843,#40844),(#40845,#40846),(#40847,#40848),(#40849,
#40850),(#40851,#40852),(#40853,#40854),(#40855,#40856),(#40857,#40858),
(#40859,#40860),(#40861,#40862),(#40863,#40864),(#40865,#40866),(#40867,
#40868),(#40869,#40870),(#40871,#40872),(#40873,#40874),(#40875,#40876),
(#40877,#40878),(#40879,#40880),(#40881,#40882),(#40883,#40884),(#40885,
#40886),(#40887,#40888),(#40889,#40890),(#40891,#40892),(#40893,#40894),
(#40895,#40896),(#40897,#40898),(#40899,#40900),(#40901,#40902),(#40903,
#40904),(#40905,#40906)),.UNSPECIFIED.,.F.,.F.,.F.,(6,1,1,1,1,1,1,1,1,1,
1,1,1,1,1,1,1,1,1,1,1,1,1,1,1,1,1,1,1,1,6),(2,2),(-1.,-0.966666666666667,
-0.933333333333333,-0.9,-0.866666666666667,-0.833333333333333,-0.8,-0.766666666666667,
-0.733333333333333,-0.7,-0.666666666666667,-0.633333333333333,-0.6,-0.566666666666667,
-0.533333333333333,-0.5,-0.466666666666667,-0.433333333333333,-0.4,-0.366666666666667,
-0.333333333333333,-0.3,-0.266666666666667,-0.233333333333333,-0.2,-0.166666666666667,
-0.133333333333333,-0.1,-0.0666666666666667,-0.0333333333333333,0.),(0.,
0.762),.UNSPECIFIED.);
#887=B_SPLINE_SURFACE_WITH_KNOTS('',5,1,((#40956,#40957),(#40958,#40959),
(#40960,#40961),(#40962,#40963),(#40964,#40965),(#40966,#40967),(#40968,
#40969),(#40970,#40971),(#40972,#40973),(#40974,#40975),(#40976,#40977),
(#40978,#40979),(#40980,#40981),(#40982,#40983),(#40984,#40985),(#40986,
#40987),(#40988,#40989),(#40990,#40991),(#40992,#40993),(#40994,#40995),
(#40996,#40997),(#40998,#40999),(#41000,#41001),(#41002,#41003),(#41004,
#41005),(#41006,#41007),(#41008,#41009),(#41010,#41011),(#41012,#41013),
(#41014,#41015),(#41016,#41017),(#41018,#41019),(#41020,#41021),(#41022,
#41023),(#41024,#41025)),.UNSPECIFIED.,.F.,.F.,.F.,(6,1,1,1,1,1,1,1,1,1,
1,1,1,1,1,1,1,1,1,1,1,1,1,1,1,1,1,1,1,1,6),(2,2),(0.,0.0333333333333333,
0.0666666666666667,0.1,0.133333333333333,0.166666666666667,0.2,0.233333333333333,
0.266666666666667,0.3,0.333333333333333,0.366666666666667,0.4,0.433333333333333,
0.466666666666667,0.5,0.533333333333333,0.566666666666667,0.6,0.633333333333333,
0.666666666666667,0.7,0.733333333333333,0.766666666666667,0.8,0.833333333333333,
0.866666666666667,0.9,0.933333333333333,0.966666666666667,1.),(0.,0.762),
 .UNSPECIFIED.);
#888=B_SPLINE_SURFACE_WITH_KNOTS('',5,1,((#41067,#41068),(#41069,#41070),
(#41071,#41072),(#41073,#41074),(#41075,#41076),(#41077,#41078),(#41079,
#41080),(#41081,#41082),(#41083,#41084),(#41085,#41086),(#41087,#41088),
(#41089,#41090),(#41091,#41092),(#41093,#41094),(#41095,#41096),(#41097,
#41098),(#41099,#41100),(#41101,#41102),(#41103,#41104),(#41105,#41106),
(#41107,#41108),(#41109,#41110),(#41111,#41112),(#41113,#41114),(#41115,
#41116),(#41117,#41118),(#41119,#41120),(#41121,#41122),(#41123,#41124),
(#41125,#41126),(#41127,#41128),(#41129,#41130),(#41131,#41132),(#41133,
#41134),(#41135,#41136)),.UNSPECIFIED.,.F.,.F.,.F.,(6,1,1,1,1,1,1,1,1,1,
1,1,1,1,1,1,1,1,1,1,1,1,1,1,1,1,1,1,1,1,6),(2,2),(-1.,-0.966666666666667,
-0.933333333333333,-0.9,-0.866666666666667,-0.833333333333333,-0.8,-0.766666666666667,
-0.733333333333333,-0.7,-0.666666666666667,-0.633333333333333,-0.6,-0.566666666666667,
-0.533333333333333,-0.5,-0.466666666666667,-0.433333333333333,-0.4,-0.366666666666667,
-0.333333333333333,-0.3,-0.266666666666667,-0.233333333333333,-0.2,-0.166666666666667,
-0.133333333333333,-0.1,-0.0666666666666667,-0.0333333333333333,0.),(0.,
0.762),.UNSPECIFIED.);
#889=B_SPLINE_SURFACE_WITH_KNOTS('',5,1,((#41186,#41187),(#41188,#41189),
(#41190,#41191),(#41192,#41193),(#41194,#41195),(#41196,#41197),(#41198,
#41199),(#41200,#41201),(#41202,#41203),(#41204,#41205),(#41206,#41207),
(#41208,#41209),(#41210,#41211),(#41212,#41213),(#41214,#41215),(#41216,
#41217),(#41218,#41219),(#41220,#41221),(#41222,#41223),(#41224,#41225),
(#41226,#41227),(#41228,#41229),(#41230,#41231),(#41232,#41233),(#41234,
#41235),(#41236,#41237),(#41238,#41239),(#41240,#41241),(#41242,#41243),
(#41244,#41245),(#41246,#41247),(#41248,#41249),(#41250,#41251),(#41252,
#41253),(#41254,#41255)),.UNSPECIFIED.,.F.,.F.,.F.,(6,1,1,1,1,1,1,1,1,1,
1,1,1,1,1,1,1,1,1,1,1,1,1,1,1,1,1,1,1,1,6),(2,2),(0.,0.0333333333333333,
0.0666666666666667,0.1,0.133333333333333,0.166666666666667,0.2,0.233333333333333,
0.266666666666667,0.3,0.333333333333333,0.366666666666667,0.4,0.433333333333333,
0.466666666666667,0.5,0.533333333333333,0.566666666666667,0.6,0.633333333333333,
0.666666666666667,0.7,0.733333333333333,0.766666666666667,0.8,0.833333333333333,
0.866666666666667,0.9,0.933333333333333,0.966666666666667,1.),(0.,0.762),
 .UNSPECIFIED.);
#890=B_SPLINE_SURFACE_WITH_KNOTS('',5,1,((#41297,#41298),(#41299,#41300),
(#41301,#41302),(#41303,#41304),(#41305,#41306),(#41307,#41308),(#41309,
#41310),(#41311,#41312),(#41313,#41314),(#41315,#41316),(#41317,#41318),
(#41319,#41320),(#41321,#41322),(#41323,#41324),(#41325,#41326),(#41327,
#41328),(#41329,#41330),(#41331,#41332),(#41333,#41334),(#41335,#41336),
(#41337,#41338),(#41339,#41340),(#41341,#41342),(#41343,#41344),(#41345,
#41346),(#41347,#41348),(#41349,#41350),(#41351,#41352),(#41353,#41354),
(#41355,#41356),(#41357,#41358),(#41359,#41360),(#41361,#41362),(#41363,
#41364),(#41365,#41366)),.UNSPECIFIED.,.F.,.F.,.F.,(6,1,1,1,1,1,1,1,1,1,
1,1,1,1,1,1,1,1,1,1,1,1,1,1,1,1,1,1,1,1,6),(2,2),(-1.,-0.966666666666667,
-0.933333333333333,-0.9,-0.866666666666667,-0.833333333333333,-0.8,-0.766666666666667,
-0.733333333333333,-0.7,-0.666666666666667,-0.633333333333333,-0.6,-0.566666666666667,
-0.533333333333333,-0.5,-0.466666666666667,-0.433333333333333,-0.4,-0.366666666666667,
-0.333333333333333,-0.3,-0.266666666666667,-0.233333333333333,-0.2,-0.166666666666667,
-0.133333333333333,-0.1,-0.0666666666666667,-0.0333333333333333,0.),(0.,
0.762),.UNSPECIFIED.);
#891=B_SPLINE_SURFACE_WITH_KNOTS('',5,1,((#41416,#41417),(#41418,#41419),
(#41420,#41421),(#41422,#41423),(#41424,#41425),(#41426,#41427),(#41428,
#41429),(#41430,#41431),(#41432,#41433),(#41434,#41435),(#41436,#41437),
(#41438,#41439),(#41440,#41441),(#41442,#41443),(#41444,#41445),(#41446,
#41447),(#41448,#41449),(#41450,#41451),(#41452,#41453),(#41454,#41455),
(#41456,#41457),(#41458,#41459),(#41460,#41461),(#41462,#41463),(#41464,
#41465),(#41466,#41467),(#41468,#41469),(#41470,#41471),(#41472,#41473),
(#41474,#41475),(#41476,#41477),(#41478,#41479),(#41480,#41481),(#41482,
#41483),(#41484,#41485)),.UNSPECIFIED.,.F.,.F.,.F.,(6,1,1,1,1,1,1,1,1,1,
1,1,1,1,1,1,1,1,1,1,1,1,1,1,1,1,1,1,1,1,6),(2,2),(0.,0.0333333333333333,
0.0666666666666667,0.1,0.133333333333333,0.166666666666667,0.2,0.233333333333333,
0.266666666666667,0.3,0.333333333333333,0.366666666666667,0.4,0.433333333333333,
0.466666666666667,0.5,0.533333333333333,0.566666666666667,0.6,0.633333333333333,
0.666666666666667,0.7,0.733333333333333,0.766666666666667,0.8,0.833333333333333,
0.866666666666667,0.9,0.933333333333333,0.966666666666667,1.),(0.,0.762),
 .UNSPECIFIED.);
#892=B_SPLINE_SURFACE_WITH_KNOTS('',5,1,((#41527,#41528),(#41529,#41530),
(#41531,#41532),(#41533,#41534),(#41535,#41536),(#41537,#41538),(#41539,
#41540),(#41541,#41542),(#41543,#41544),(#41545,#41546),(#41547,#41548),
(#41549,#41550),(#41551,#41552),(#41553,#41554),(#41555,#41556),(#41557,
#41558),(#41559,#41560),(#41561,#41562),(#41563,#41564),(#41565,#41566),
(#41567,#41568),(#41569,#41570),(#41571,#41572),(#41573,#41574),(#41575,
#41576),(#41577,#41578),(#41579,#41580),(#41581,#41582),(#41583,#41584),
(#41585,#41586),(#41587,#41588),(#41589,#41590),(#41591,#41592),(#41593,
#41594),(#41595,#41596)),.UNSPECIFIED.,.F.,.F.,.F.,(6,1,1,1,1,1,1,1,1,1,
1,1,1,1,1,1,1,1,1,1,1,1,1,1,1,1,1,1,1,1,6),(2,2),(-1.,-0.966666666666667,
-0.933333333333333,-0.9,-0.866666666666667,-0.833333333333333,-0.8,-0.766666666666667,
-0.733333333333333,-0.7,-0.666666666666667,-0.633333333333333,-0.6,-0.566666666666667,
-0.533333333333333,-0.5,-0.466666666666667,-0.433333333333333,-0.4,-0.366666666666667,
-0.333333333333333,-0.3,-0.266666666666667,-0.233333333333333,-0.2,-0.166666666666667,
-0.133333333333333,-0.1,-0.0666666666666667,-0.0333333333333333,0.),(0.,
0.762),.UNSPECIFIED.);
#893=B_SPLINE_SURFACE_WITH_KNOTS('',5,1,((#41652,#41653),(#41654,#41655),
(#41656,#41657),(#41658,#41659),(#41660,#41661),(#41662,#41663),(#41664,
#41665),(#41666,#41667),(#41668,#41669),(#41670,#41671),(#41672,#41673),
(#41674,#41675),(#41676,#41677),(#41678,#41679),(#41680,#41681),(#41682,
#41683),(#41684,#41685),(#41686,#41687),(#41688,#41689),(#41690,#41691),
(#41692,#41693),(#41694,#41695),(#41696,#41697),(#41698,#41699),(#41700,
#41701),(#41702,#41703),(#41704,#41705),(#41706,#41707),(#41708,#41709),
(#41710,#41711),(#41712,#41713),(#41714,#41715),(#41716,#41717),(#41718,
#41719),(#41720,#41721)),.UNSPECIFIED.,.F.,.F.,.F.,(6,1,1,1,1,1,1,1,1,1,
1,1,1,1,1,1,1,1,1,1,1,1,1,1,1,1,1,1,1,1,6),(2,2),(0.,0.0333333333333333,
0.0666666666666667,0.1,0.133333333333333,0.166666666666667,0.2,0.233333333333333,
0.266666666666667,0.3,0.333333333333333,0.366666666666667,0.4,0.433333333333333,
0.466666666666667,0.5,0.533333333333333,0.566666666666667,0.6,0.633333333333333,
0.666666666666667,0.7,0.733333333333333,0.766666666666667,0.8,0.833333333333333,
0.866666666666667,0.9,0.933333333333333,0.966666666666667,1.),(0.,0.762),
 .UNSPECIFIED.);
#894=B_SPLINE_SURFACE_WITH_KNOTS('',5,1,((#41757,#41758),(#41759,#41760),
(#41761,#41762),(#41763,#41764),(#41765,#41766),(#41767,#41768),(#41769,
#41770),(#41771,#41772),(#41773,#41774),(#41775,#41776),(#41777,#41778),
(#41779,#41780),(#41781,#41782),(#41783,#41784),(#41785,#41786),(#41787,
#41788),(#41789,#41790),(#41791,#41792),(#41793,#41794),(#41795,#41796),
(#41797,#41798),(#41799,#41800),(#41801,#41802),(#41803,#41804),(#41805,
#41806),(#41807,#41808),(#41809,#41810),(#41811,#41812),(#41813,#41814),
(#41815,#41816),(#41817,#41818),(#41819,#41820),(#41821,#41822),(#41823,
#41824),(#41825,#41826)),.UNSPECIFIED.,.F.,.F.,.F.,(6,1,1,1,1,1,1,1,1,1,
1,1,1,1,1,1,1,1,1,1,1,1,1,1,1,1,1,1,1,1,6),(2,2),(-1.,-0.966666666666667,
-0.933333333333333,-0.9,-0.866666666666667,-0.833333333333333,-0.8,-0.766666666666667,
-0.733333333333333,-0.7,-0.666666666666667,-0.633333333333333,-0.6,-0.566666666666667,
-0.533333333333333,-0.5,-0.466666666666667,-0.433333333333333,-0.4,-0.366666666666667,
-0.333333333333333,-0.3,-0.266666666666667,-0.233333333333333,-0.2,-0.166666666666667,
-0.133333333333333,-0.1,-0.0666666666666667,-0.0333333333333333,0.),(0.,
0.762),.UNSPECIFIED.);
#895=B_SPLINE_SURFACE_WITH_KNOTS('',5,1,((#41953,#41954),(#41955,#41956),
(#41957,#41958),(#41959,#41960),(#41961,#41962),(#41963,#41964),(#41965,
#41966),(#41967,#41968),(#41969,#41970),(#41971,#41972),(#41973,#41974),
(#41975,#41976),(#41977,#41978),(#41979,#41980),(#41981,#41982),(#41983,
#41984),(#41985,#41986),(#41987,#41988),(#41989,#41990),(#41991,#41992),
(#41993,#41994),(#41995,#41996),(#41997,#41998),(#41999,#42000),(#42001,
#42002),(#42003,#42004),(#42005,#42006),(#42007,#42008),(#42009,#42010),
(#42011,#42012),(#42013,#42014),(#42015,#42016),(#42017,#42018),(#42019,
#42020),(#42021,#42022)),.UNSPECIFIED.,.F.,.F.,.F.,(6,1,1,1,1,1,1,1,1,1,
1,1,1,1,1,1,1,1,1,1,1,1,1,1,1,1,1,1,1,1,6),(2,2),(0.,0.0333333333333333,
0.0666666666666667,0.1,0.133333333333333,0.166666666666667,0.2,0.233333333333333,
0.266666666666667,0.3,0.333333333333333,0.366666666666667,0.4,0.433333333333333,
0.466666666666667,0.5,0.533333333333333,0.566666666666667,0.6,0.633333333333333,
0.666666666666667,0.7,0.733333333333333,0.766666666666667,0.8,0.833333333333333,
0.866666666666667,0.9,0.933333333333333,0.966666666666667,1.),(0.,0.762),
 .UNSPECIFIED.);
#896=B_SPLINE_SURFACE_WITH_KNOTS('',5,1,((#42026,#42027),(#42028,#42029),
(#42030,#42031),(#42032,#42033),(#42034,#42035),(#42036,#42037),(#42038,
#42039),(#42040,#42041),(#42042,#42043),(#42044,#42045),(#42046,#42047),
(#42048,#42049),(#42050,#42051),(#42052,#42053),(#42054,#42055),(#42056,
#42057),(#42058,#42059),(#42060,#42061),(#42062,#42063),(#42064,#42065),
(#42066,#42067),(#42068,#42069),(#42070,#42071),(#42072,#42073),(#42074,
#42075),(#42076,#42077),(#42078,#42079),(#42080,#42081),(#42082,#42083),
(#42084,#42085),(#42086,#42087),(#42088,#42089),(#42090,#42091),(#42092,
#42093),(#42094,#42095)),.UNSPECIFIED.,.F.,.F.,.F.,(6,1,1,1,1,1,1,1,1,1,
1,1,1,1,1,1,1,1,1,1,1,1,1,1,1,1,1,1,1,1,6),(2,2),(-1.,-0.966666666666667,
-0.933333333333333,-0.9,-0.866666666666667,-0.833333333333333,-0.8,-0.766666666666667,
-0.733333333333333,-0.7,-0.666666666666667,-0.633333333333333,-0.6,-0.566666666666667,
-0.533333333333333,-0.5,-0.466666666666667,-0.433333333333333,-0.4,-0.366666666666667,
-0.333333333333333,-0.3,-0.266666666666667,-0.233333333333333,-0.2,-0.166666666666667,
-0.133333333333333,-0.1,-0.0666666666666667,-0.0333333333333333,0.),(0.,
0.762),.UNSPECIFIED.);
#897=B_SPLINE_SURFACE_WITH_KNOTS('',3,3,((#48924,#48925,#48926,#48927,#48928,
#48929,#48930,#48931,#48932,#48933,#48934,#48935,#48936,#48937,#48938,#48939,
#48940,#48941,#48942,#48943,#48944,#48945,#48946,#48947,#48948,#48949,#48950,
#48951,#48952,#48953,#48954,#48955,#48956,#48957,#48958,#48959,#48960,#48961,
#48962,#48963,#48964,#48965,#48966,#48967,#48968,#48969,#48970,#48971,#48972,
#48973,#48974,#48975,#48976,#48977,#48978,#48979,#48980,#48981,#48982,#48983,
#48984,#48985,#48986,#48987,#48988,#48989,#48990,#48991,#48992,#48993,#48994,
#48995,#48996,#48997,#48998),(#48999,#49000,#49001,#49002,#49003,#49004,
#49005,#49006,#49007,#49008,#49009,#49010,#49011,#49012,#49013,#49014,#49015,
#49016,#49017,#49018,#49019,#49020,#49021,#49022,#49023,#49024,#49025,#49026,
#49027,#49028,#49029,#49030,#49031,#49032,#49033,#49034,#49035,#49036,#49037,
#49038,#49039,#49040,#49041,#49042,#49043,#49044,#49045,#49046,#49047,#49048,
#49049,#49050,#49051,#49052,#49053,#49054,#49055,#49056,#49057,#49058,#49059,
#49060,#49061,#49062,#49063,#49064,#49065,#49066,#49067,#49068,#49069,#49070,
#49071,#49072,#49073),(#49074,#49075,#49076,#49077,#49078,#49079,#49080,
#49081,#49082,#49083,#49084,#49085,#49086,#49087,#49088,#49089,#49090,#49091,
#49092,#49093,#49094,#49095,#49096,#49097,#49098,#49099,#49100,#49101,#49102,
#49103,#49104,#49105,#49106,#49107,#49108,#49109,#49110,#49111,#49112,#49113,
#49114,#49115,#49116,#49117,#49118,#49119,#49120,#49121,#49122,#49123,#49124,
#49125,#49126,#49127,#49128,#49129,#49130,#49131,#49132,#49133,#49134,#49135,
#49136,#49137,#49138,#49139,#49140,#49141,#49142,#49143,#49144,#49145,#49146,
#49147,#49148),(#49149,#49150,#49151,#49152,#49153,#49154,#49155,#49156,
#49157,#49158,#49159,#49160,#49161,#49162,#49163,#49164,#49165,#49166,#49167,
#49168,#49169,#49170,#49171,#49172,#49173,#49174,#49175,#49176,#49177,#49178,
#49179,#49180,#49181,#49182,#49183,#49184,#49185,#49186,#49187,#49188,#49189,
#49190,#49191,#49192,#49193,#49194,#49195,#49196,#49197,#49198,#49199,#49200,
#49201,#49202,#49203,#49204,#49205,#49206,#49207,#49208,#49209,#49210,#49211,
#49212,#49213,#49214,#49215,#49216,#49217,#49218,#49219,#49220,#49221,#49222,
#49223)),.UNSPECIFIED.,.F.,.F.,.F.,(4,4),(4,1,1,1,1,1,1,1,1,1,1,1,1,1,1,
1,1,1,1,1,1,1,1,1,1,1,1,1,1,1,1,1,1,1,1,1,1,1,1,1,1,1,1,1,1,1,1,1,1,1,1,
1,1,1,1,1,1,1,1,1,1,1,1,1,1,1,1,1,1,1,1,1,4),(-0.000245115248125111,0.0332154979215098),
(8.30203615430821,9.29948795407228,10.2969397538364,11.2943915536004,12.2918433533645,
13.2892951531286,14.2867469528926,15.2841987526567,16.2816505524208,17.2791023521849,
18.2765541519489,19.274005951713,20.2714577514771,21.2689095512411,22.2663613510052,
23.2638131507693,24.2612649505334,25.2587167502974,26.2561685500615,27.2536203498256,
28.2510721495896,29.2485239493537,30.2459757491178,31.2434275488818,32.2408793486459,
33.23833114841,34.2357829481741,35.2332347479381,36.2306865477022,37.2281383474663,
38.2255901472303,39.2230419469944,40.2204937467585,41.2179455465226,42.2153973462866,
43.2128491460507,44.2103009458148,45.2077527455788,46.2052045453429,47.202656345107,
48.2001081448711,49.1975599446351,50.1950117443992,51.1924635441633,52.1899153439273,
53.1873671436914,54.1848189434555,55.1822707432196,56.1797225429836,57.1771743427477,
58.1746261425118,59.1720779422758,60.1695297420399,61.166981541804,62.1644333415681,
63.1618851413321,64.1593369410962,65.1567887408603,66.1542405406243,67.1516923403884,
68.1491441401525,69.1465959399166,70.1440477396806,71.1414995394447,72.1389513392088,
73.1364031389728,74.1338549387369,75.131306738501,76.128758538265,77.1262103380291,
78.1236621377932,79.1211139375573,80.1188108525694),.UNSPECIFIED.);
#898=B_SPLINE_SURFACE_WITH_KNOTS('',3,3,((#49397,#49398,#49399,#49400,#49401,
#49402,#49403,#49404,#49405,#49406,#49407,#49408,#49409,#49410,#49411,#49412,
#49413,#49414,#49415,#49416,#49417,#49418,#49419,#49420,#49421,#49422,#49423,
#49424,#49425,#49426,#49427,#49428,#49429,#49430,#49431,#49432,#49433,#49434,
#49435,#49436,#49437,#49438,#49439,#49440,#49441,#49442,#49443,#49444,#49445,
#49446,#49447,#49448,#49449,#49450,#49451,#49452,#49453,#49454,#49455,#49456,
#49457,#49458,#49459,#49460,#49461,#49462,#49463,#49464,#49465,#49466,#49467,
#49468,#49469,#49470,#49471),(#49472,#49473,#49474,#49475,#49476,#49477,
#49478,#49479,#49480,#49481,#49482,#49483,#49484,#49485,#49486,#49487,#49488,
#49489,#49490,#49491,#49492,#49493,#49494,#49495,#49496,#49497,#49498,#49499,
#49500,#49501,#49502,#49503,#49504,#49505,#49506,#49507,#49508,#49509,#49510,
#49511,#49512,#49513,#49514,#49515,#49516,#49517,#49518,#49519,#49520,#49521,
#49522,#49523,#49524,#49525,#49526,#49527,#49528,#49529,#49530,#49531,#49532,
#49533,#49534,#49535,#49536,#49537,#49538,#49539,#49540,#49541,#49542,#49543,
#49544,#49545,#49546),(#49547,#49548,#49549,#49550,#49551,#49552,#49553,
#49554,#49555,#49556,#49557,#49558,#49559,#49560,#49561,#49562,#49563,#49564,
#49565,#49566,#49567,#49568,#49569,#49570,#49571,#49572,#49573,#49574,#49575,
#49576,#49577,#49578,#49579,#49580,#49581,#49582,#49583,#49584,#49585,#49586,
#49587,#49588,#49589,#49590,#49591,#49592,#49593,#49594,#49595,#49596,#49597,
#49598,#49599,#49600,#49601,#49602,#49603,#49604,#49605,#49606,#49607,#49608,
#49609,#49610,#49611,#49612,#49613,#49614,#49615,#49616,#49617,#49618,#49619,
#49620,#49621),(#49622,#49623,#49624,#49625,#49626,#49627,#49628,#49629,
#49630,#49631,#49632,#49633,#49634,#49635,#49636,#49637,#49638,#49639,#49640,
#49641,#49642,#49643,#49644,#49645,#49646,#49647,#49648,#49649,#49650,#49651,
#49652,#49653,#49654,#49655,#49656,#49657,#49658,#49659,#49660,#49661,#49662,
#49663,#49664,#49665,#49666,#49667,#49668,#49669,#49670,#49671,#49672,#49673,
#49674,#49675,#49676,#49677,#49678,#49679,#49680,#49681,#49682,#49683,#49684,
#49685,#49686,#49687,#49688,#49689,#49690,#49691,#49692,#49693,#49694,#49695,
#49696)),.UNSPECIFIED.,.F.,.F.,.F.,(4,4),(4,1,1,1,1,1,1,1,1,1,1,1,1,1,1,
1,1,1,1,1,1,1,1,1,1,1,1,1,1,1,1,1,1,1,1,1,1,1,1,1,1,1,1,1,1,1,1,1,1,1,1,
1,1,1,1,1,1,1,1,1,1,1,1,1,1,1,1,1,1,1,1,1,4),(-0.000210453224954951,0.0332406947647496),
(11.6156946206196,12.6133915472643,13.6108433470284,14.6082951467925,15.6057469465565,
16.6031987463206,17.6006505460847,18.5981023458487,19.5955541456128,20.5930059453769,
21.590457745141,22.587909544905,23.5853613446691,24.5828131444332,25.5802649441972,
26.5777167439613,27.5751685437254,28.5726203434894,29.5700721432535,30.5675239430176,
31.5649757427817,32.5624275425457,33.5598793423098,34.5573311420739,35.5547829418379,
36.552234741602,37.5496865413661,38.5471383411302,39.5445901408942,40.5420419406583,
41.5394937404224,42.5369455401864,43.5343973399505,44.5318491397146,45.5293009394787,
46.5267527392427,47.5242045390068,48.5216563387709,49.5191081385349,50.516559938299,
51.5140117380631,52.5114635378272,53.5089153375912,54.5063671373553,55.5038189371194,
56.5012707368834,57.4987225366475,58.4961743364116,59.4936261361756,60.4910779359397,
61.4885297357038,62.4859815354679,63.4834333352319,64.480885134996,65.4783369347601,
66.4757887345241,67.4732405342882,68.4706923340523,69.4681441338164,70.4655959335804,
71.4630477333445,72.4604995331086,73.4579513328726,74.4554031326367,75.4528549324008,
76.4503067321649,77.4477585319289,78.445210331693,79.4426621314571,80.4401139312211,
81.4375657309852,82.4350175307493,83.4324693305134),.UNSPECIFIED.);
#899=B_SPLINE_SURFACE_WITH_KNOTS('',3,3,((#57921,#57922,#57923,#57924,#57925,
#57926,#57927,#57928,#57929,#57930,#57931,#57932,#57933,#57934,#57935,#57936,
#57937,#57938,#57939,#57940,#57941,#57942,#57943,#57944,#57945,#57946,#57947,
#57948,#57949,#57950,#57951,#57952,#57953,#57954,#57955,#57956,#57957,#57958,
#57959,#57960,#57961,#57962,#57963,#57964,#57965,#57966,#57967,#57968,#57969,
#57970,#57971,#57972),(#57973,#57974,#57975,#57976,#57977,#57978,#57979,
#57980,#57981,#57982,#57983,#57984,#57985,#57986,#57987,#57988,#57989,#57990,
#57991,#57992,#57993,#57994,#57995,#57996,#57997,#57998,#57999,#58000,#58001,
#58002,#58003,#58004,#58005,#58006,#58007,#58008,#58009,#58010,#58011,#58012,
#58013,#58014,#58015,#58016,#58017,#58018,#58019,#58020,#58021,#58022,#58023,
#58024),(#58025,#58026,#58027,#58028,#58029,#58030,#58031,#58032,#58033,
#58034,#58035,#58036,#58037,#58038,#58039,#58040,#58041,#58042,#58043,#58044,
#58045,#58046,#58047,#58048,#58049,#58050,#58051,#58052,#58053,#58054,#58055,
#58056,#58057,#58058,#58059,#58060,#58061,#58062,#58063,#58064,#58065,#58066,
#58067,#58068,#58069,#58070,#58071,#58072,#58073,#58074,#58075,#58076),
(#58077,#58078,#58079,#58080,#58081,#58082,#58083,#58084,#58085,#58086,
#58087,#58088,#58089,#58090,#58091,#58092,#58093,#58094,#58095,#58096,#58097,
#58098,#58099,#58100,#58101,#58102,#58103,#58104,#58105,#58106,#58107,#58108,
#58109,#58110,#58111,#58112,#58113,#58114,#58115,#58116,#58117,#58118,#58119,
#58120,#58121,#58122,#58123,#58124,#58125,#58126,#58127,#58128)),
 .UNSPECIFIED.,.F.,.F.,.F.,(4,4),(4,1,1,1,1,1,1,1,1,1,1,1,1,1,1,1,1,1,1,
1,1,1,1,1,1,1,1,1,1,1,1,1,1,1,1,1,1,1,1,1,1,1,1,1,1,1,1,1,1,4),(-0.000256380190589609,
0.0503983527946267),(8.33940042121162,9.32496353298982,10.310526644768,
11.2960897565462,12.2816528683244,13.2672159801026,14.2527790918808,15.2383422036591,
16.2239053154373,17.2094684272155,18.1950315389937,19.1805946507719,20.1661577625501,
21.1517208743283,22.1372839861065,23.1228470978847,24.1084102096629,25.0939733214411,
26.0795364332193,27.0650995449975,28.0506626567757,29.0362257685539,30.0217888803321,
31.0073519921103,31.9929151038885,32.9784782156668,33.964041327445,34.9496044392232,
35.9351675510014,36.9207306627796,37.9062937745578,38.891856886336,39.8774199981142,
40.8629831098924,41.8485462216706,42.8341093334488,43.819672445227,44.8052355570052,
45.7907986687834,46.7763617805616,47.7619248923398,48.747488004118,49.7330511158962,
50.7186142276745,51.7041773394527,52.6897404512309,53.6753035630091,54.6608666747873,
55.6464297865655,56.6322492785343),.UNSPECIFIED.);
#900=B_SPLINE_SURFACE_WITH_KNOTS('',3,3,((#58307,#58308,#58309,#58310,#58311,
#58312,#58313,#58314,#58315,#58316,#58317,#58318,#58319,#58320,#58321,#58322,
#58323,#58324,#58325,#58326,#58327,#58328,#58329,#58330,#58331,#58332,#58333,
#58334,#58335,#58336,#58337,#58338,#58339,#58340,#58341,#58342,#58343,#58344,
#58345,#58346,#58347,#58348,#58349,#58350,#58351,#58352,#58353,#58354,#58355,
#58356,#58357,#58358),(#58359,#58360,#58361,#58362,#58363,#58364,#58365,
#58366,#58367,#58368,#58369,#58370,#58371,#58372,#58373,#58374,#58375,#58376,
#58377,#58378,#58379,#58380,#58381,#58382,#58383,#58384,#58385,#58386,#58387,
#58388,#58389,#58390,#58391,#58392,#58393,#58394,#58395,#58396,#58397,#58398,
#58399,#58400,#58401,#58402,#58403,#58404,#58405,#58406,#58407,#58408,#58409,
#58410),(#58411,#58412,#58413,#58414,#58415,#58416,#58417,#58418,#58419,
#58420,#58421,#58422,#58423,#58424,#58425,#58426,#58427,#58428,#58429,#58430,
#58431,#58432,#58433,#58434,#58435,#58436,#58437,#58438,#58439,#58440,#58441,
#58442,#58443,#58444,#58445,#58446,#58447,#58448,#58449,#58450,#58451,#58452,
#58453,#58454,#58455,#58456,#58457,#58458,#58459,#58460,#58461,#58462),
(#58463,#58464,#58465,#58466,#58467,#58468,#58469,#58470,#58471,#58472,
#58473,#58474,#58475,#58476,#58477,#58478,#58479,#58480,#58481,#58482,#58483,
#58484,#58485,#58486,#58487,#58488,#58489,#58490,#58491,#58492,#58493,#58494,
#58495,#58496,#58497,#58498,#58499,#58500,#58501,#58502,#58503,#58504,#58505,
#58506,#58507,#58508,#58509,#58510,#58511,#58512,#58513,#58514)),
 .UNSPECIFIED.,.F.,.F.,.F.,(4,4),(4,1,1,1,1,1,1,1,1,1,1,1,1,1,1,1,1,1,1,
1,1,1,1,1,1,1,1,1,1,1,1,1,1,1,1,1,1,1,1,1,1,1,1,1,1,1,1,1,1,4),(-0.000235021283989965,
0.05040963628664),(11.6664697565963,12.6522892414772,13.6378523532554,14.6234154650336,
15.6089785768118,16.59454168859,17.5801048003682,18.5656679121464,19.5512310239246,
20.5367941357028,21.522357247481,22.5079203592592,23.4934834710374,24.4790465828156,
25.4646096945938,26.450172806372,27.4357359181503,28.4212990299285,29.4068621417067,
30.3924252534849,31.3779883652631,32.3635514770413,33.3491145888195,34.3346777005977,
35.3202408123759,36.3058039241541,37.2913670359323,38.2769301477105,39.2624932594887,
40.2480563712669,41.2336194830451,42.2191825948233,43.2047457066015,44.1903088183797,
45.175871930158,46.1614350419362,47.1469981537144,48.1325612654926,49.1181243772708,
50.103687489049,51.0892506008272,52.0748137126054,53.0603768243836,54.0459399361618,
55.03150304794,56.0170661597182,57.0026292714964,57.9881923832746,58.9737554950528,
59.959318606831),.UNSPECIFIED.);
#901=B_SPLINE_SURFACE_WITH_KNOTS('',3,3,((#65292,#65293,#65294,#65295,#65296,
#65297,#65298,#65299,#65300,#65301,#65302,#65303,#65304,#65305,#65306,#65307,
#65308,#65309,#65310,#65311,#65312,#65313,#65314,#65315,#65316,#65317,#65318,
#65319,#65320,#65321,#65322,#65323,#65324,#65325,#65326,#65327,#65328,#65329,
#65330,#65331,#65332,#65333,#65334,#65335,#65336,#65337,#65338,#65339,#65340,
#65341,#65342,#65343,#65344,#65345,#65346,#65347,#65348,#65349,#65350,#65351,
#65352,#65353,#65354,#65355),(#65356,#65357,#65358,#65359,#65360,#65361,
#65362,#65363,#65364,#65365,#65366,#65367,#65368,#65369,#65370,#65371,#65372,
#65373,#65374,#65375,#65376,#65377,#65378,#65379,#65380,#65381,#65382,#65383,
#65384,#65385,#65386,#65387,#65388,#65389,#65390,#65391,#65392,#65393,#65394,
#65395,#65396,#65397,#65398,#65399,#65400,#65401,#65402,#65403,#65404,#65405,
#65406,#65407,#65408,#65409,#65410,#65411,#65412,#65413,#65414,#65415,#65416,
#65417,#65418,#65419),(#65420,#65421,#65422,#65423,#65424,#65425,#65426,
#65427,#65428,#65429,#65430,#65431,#65432,#65433,#65434,#65435,#65436,#65437,
#65438,#65439,#65440,#65441,#65442,#65443,#65444,#65445,#65446,#65447,#65448,
#65449,#65450,#65451,#65452,#65453,#65454,#65455,#65456,#65457,#65458,#65459,
#65460,#65461,#65462,#65463,#65464,#65465,#65466,#65467,#65468,#65469,#65470,
#65471,#65472,#65473,#65474,#65475,#65476,#65477,#65478,#65479,#65480,#65481,
#65482,#65483),(#65484,#65485,#65486,#65487,#65488,#65489,#65490,#65491,
#65492,#65493,#65494,#65495,#65496,#65497,#65498,#65499,#65500,#65501,#65502,
#65503,#65504,#65505,#65506,#65507,#65508,#65509,#65510,#65511,#65512,#65513,
#65514,#65515,#65516,#65517,#65518,#65519,#65520,#65521,#65522,#65523,#65524,
#65525,#65526,#65527,#65528,#65529,#65530,#65531,#65532,#65533,#65534,#65535,
#65536,#65537,#65538,#65539,#65540,#65541,#65542,#65543,#65544,#65545,#65546,
#65547)),.UNSPECIFIED.,.F.,.F.,.F.,(4,4),(4,1,1,1,1,1,1,1,1,1,1,1,1,1,1,
1,1,1,1,1,1,1,1,1,1,1,1,1,1,1,1,1,1,1,1,1,1,1,1,1,1,1,1,1,1,1,1,1,1,1,1,
1,1,1,1,1,1,1,1,1,1,4),(-0.000266152038421994,0.0504103259038983),(8.3394004212115,
9.33708834074415,10.3347762602768,11.3324641798094,12.3301520993421,13.3278400188747,
14.3255279384074,15.32321585794,16.3209037774727,17.3185916970053,18.3162796165379,
19.3139675360706,20.3116554556032,21.3093433751359,22.3070312946685,23.3047192142012,
24.3024071337338,25.3000950532664,26.2977829727991,27.2954708923317,28.2931588118644,
29.290846731397,30.2885346509297,31.2862225704623,32.283910489995,33.2815984095276,
34.2792863290602,35.2769742485929,36.2746621681255,37.2723500876582,38.2700380071908,
39.2677259267235,40.2654138462561,41.2631017657887,42.2607896853214,43.258477604854,
44.2561655243867,45.2538534439193,46.251541363452,47.2492292829846,48.2469172025173,
49.2446051220499,50.2422930415825,51.2399809611152,52.2376688806478,53.2353568001805,
54.2330447197131,55.2307326392458,56.2284205587784,57.226108478311,58.2237963978437,
59.2214843173763,60.219172236909,61.2168601564416,62.2145480759743,63.2122359955069,
64.2099239150396,65.2076118345722,66.2052997541048,67.2029876736375,68.2006755931701,
69.1986296647412),.UNSPECIFIED.);
#902=B_SPLINE_SURFACE_WITH_KNOTS('',3,3,((#65712,#65713,#65714,#65715,#65716,
#65717,#65718,#65719,#65720,#65721,#65722,#65723,#65724,#65725,#65726,#65727,
#65728,#65729,#65730,#65731,#65732,#65733,#65734,#65735,#65736,#65737,#65738,
#65739,#65740,#65741,#65742,#65743,#65744,#65745,#65746,#65747,#65748,#65749,
#65750,#65751,#65752,#65753,#65754,#65755,#65756,#65757,#65758,#65759,#65760,
#65761,#65762,#65763,#65764,#65765,#65766,#65767,#65768,#65769,#65770,#65771,
#65772,#65773,#65774,#65775),(#65776,#65777,#65778,#65779,#65780,#65781,
#65782,#65783,#65784,#65785,#65786,#65787,#65788,#65789,#65790,#65791,#65792,
#65793,#65794,#65795,#65796,#65797,#65798,#65799,#65800,#65801,#65802,#65803,
#65804,#65805,#65806,#65807,#65808,#65809,#65810,#65811,#65812,#65813,#65814,
#65815,#65816,#65817,#65818,#65819,#65820,#65821,#65822,#65823,#65824,#65825,
#65826,#65827,#65828,#65829,#65830,#65831,#65832,#65833,#65834,#65835,#65836,
#65837,#65838,#65839),(#65840,#65841,#65842,#65843,#65844,#65845,#65846,
#65847,#65848,#65849,#65850,#65851,#65852,#65853,#65854,#65855,#65856,#65857,
#65858,#65859,#65860,#65861,#65862,#65863,#65864,#65865,#65866,#65867,#65868,
#65869,#65870,#65871,#65872,#65873,#65874,#65875,#65876,#65877,#65878,#65879,
#65880,#65881,#65882,#65883,#65884,#65885,#65886,#65887,#65888,#65889,#65890,
#65891,#65892,#65893,#65894,#65895,#65896,#65897,#65898,#65899,#65900,#65901,
#65902,#65903),(#65904,#65905,#65906,#65907,#65908,#65909,#65910,#65911,
#65912,#65913,#65914,#65915,#65916,#65917,#65918,#65919,#65920,#65921,#65922,
#65923,#65924,#65925,#65926,#65927,#65928,#65929,#65930,#65931,#65932,#65933,
#65934,#65935,#65936,#65937,#65938,#65939,#65940,#65941,#65942,#65943,#65944,
#65945,#65946,#65947,#65948,#65949,#65950,#65951,#65952,#65953,#65954,#65955,
#65956,#65957,#65958,#65959,#65960,#65961,#65962,#65963,#65964,#65965,#65966,
#65967)),.UNSPECIFIED.,.F.,.F.,.F.,(4,4),(4,1,1,1,1,1,1,1,1,1,1,1,1,1,1,
1,1,1,1,1,1,1,1,1,1,1,1,1,1,1,1,1,1,1,1,1,1,1,1,1,1,1,1,1,1,1,1,1,1,1,1,
1,1,1,1,1,1,1,1,1,1,4),(-0.000246149933917203,0.0504194085446373),(11.6664599843382,
12.6644140492316,13.6621019687642,14.6597898882969,15.6574778078295,16.6551657273622,
17.6528536468948,18.6505415664274,19.6482294859601,20.6459174054927,21.6436053250254,
22.641293244558,23.6389811640907,24.6366690836233,25.634357003156,26.6320449226886,
27.6297328422212,28.6274207617539,29.6251086812865,30.6227966008192,31.6204845203518,
32.6181724398845,33.6158603594171,34.6135482789498,35.6112361984824,36.608924118015,
37.6066120375477,38.6042999570803,39.601987876613,40.5996757961456,41.5973637156783,
42.5950516352109,43.5927395547435,44.5904274742762,45.5881153938088,46.5858033133415,
47.5834912328741,48.5811791524068,49.5788670719394,50.5765549914721,51.5742429110047,
52.5719308305373,53.56961875007,54.5673066696026,55.5649945891353,56.5626825086679,
57.5603704282006,58.5580583477332,59.5557462672658,60.5534341867985,61.5511221063311,
62.5488100258638,63.5464979453964,64.5441858649291,65.5418737844617,66.5395617039943,
67.537249623527,68.5349375430596,69.5326254625923,70.5303133821249,71.5280013016576,
72.5256892211902),.UNSPECIFIED.);
#903=B_SPLINE_SURFACE_WITH_KNOTS('',3,3,((#80984,#80985,#80986,#80987,#80988,
#80989,#80990,#80991,#80992,#80993,#80994,#80995,#80996,#80997,#80998,#80999,
#81000,#81001,#81002,#81003,#81004,#81005,#81006,#81007,#81008,#81009,#81010,
#81011,#81012,#81013,#81014,#81015,#81016,#81017,#81018,#81019,#81020,#81021,
#81022,#81023,#81024,#81025,#81026,#81027,#81028,#81029,#81030,#81031,#81032,
#81033,#81034,#81035,#81036,#81037,#81038,#81039,#81040,#81041,#81042,#81043,
#81044,#81045,#81046,#81047,#81048,#81049,#81050,#81051,#81052,#81053,#81054,
#81055,#81056,#81057,#81058,#81059,#81060,#81061,#81062,#81063,#81064,#81065,
#81066,#81067,#81068,#81069,#81070,#81071,#81072,#81073,#81074,#81075,#81076,
#81077,#81078,#81079,#81080,#81081,#81082,#81083,#81084,#81085,#81086,#81087,
#81088,#81089,#81090,#81091,#81092,#81093,#81094,#81095,#81096,#81097,#81098,
#81099,#81100,#81101,#81102,#81103,#81104,#81105,#81106,#81107,#81108,#81109,
#81110),(#81111,#81112,#81113,#81114,#81115,#81116,#81117,#81118,#81119,
#81120,#81121,#81122,#81123,#81124,#81125,#81126,#81127,#81128,#81129,#81130,
#81131,#81132,#81133,#81134,#81135,#81136,#81137,#81138,#81139,#81140,#81141,
#81142,#81143,#81144,#81145,#81146,#81147,#81148,#81149,#81150,#81151,#81152,
#81153,#81154,#81155,#81156,#81157,#81158,#81159,#81160,#81161,#81162,#81163,
#81164,#81165,#81166,#81167,#81168,#81169,#81170,#81171,#81172,#81173,#81174,
#81175,#81176,#81177,#81178,#81179,#81180,#81181,#81182,#81183,#81184,#81185,
#81186,#81187,#81188,#81189,#81190,#81191,#81192,#81193,#81194,#81195,#81196,
#81197,#81198,#81199,#81200,#81201,#81202,#81203,#81204,#81205,#81206,#81207,
#81208,#81209,#81210,#81211,#81212,#81213,#81214,#81215,#81216,#81217,#81218,
#81219,#81220,#81221,#81222,#81223,#81224,#81225,#81226,#81227,#81228,#81229,
#81230,#81231,#81232,#81233,#81234,#81235,#81236,#81237),(#81238,#81239,
#81240,#81241,#81242,#81243,#81244,#81245,#81246,#81247,#81248,#81249,#81250,
#81251,#81252,#81253,#81254,#81255,#81256,#81257,#81258,#81259,#81260,#81261,
#81262,#81263,#81264,#81265,#81266,#81267,#81268,#81269,#81270,#81271,#81272,
#81273,#81274,#81275,#81276,#81277,#81278,#81279,#81280,#81281,#81282,#81283,
#81284,#81285,#81286,#81287,#81288,#81289,#81290,#81291,#81292,#81293,#81294,
#81295,#81296,#81297,#81298,#81299,#81300,#81301,#81302,#81303,#81304,#81305,
#81306,#81307,#81308,#81309,#81310,#81311,#81312,#81313,#81314,#81315,#81316,
#81317,#81318,#81319,#81320,#81321,#81322,#81323,#81324,#81325,#81326,#81327,
#81328,#81329,#81330,#81331,#81332,#81333,#81334,#81335,#81336,#81337,#81338,
#81339,#81340,#81341,#81342,#81343,#81344,#81345,#81346,#81347,#81348,#81349,
#81350,#81351,#81352,#81353,#81354,#81355,#81356,#81357,#81358,#81359,#81360,
#81361,#81362,#81363,#81364),(#81365,#81366,#81367,#81368,#81369,#81370,
#81371,#81372,#81373,#81374,#81375,#81376,#81377,#81378,#81379,#81380,#81381,
#81382,#81383,#81384,#81385,#81386,#81387,#81388,#81389,#81390,#81391,#81392,
#81393,#81394,#81395,#81396,#81397,#81398,#81399,#81400,#81401,#81402,#81403,
#81404,#81405,#81406,#81407,#81408,#81409,#81410,#81411,#81412,#81413,#81414,
#81415,#81416,#81417,#81418,#81419,#81420,#81421,#81422,#81423,#81424,#81425,
#81426,#81427,#81428,#81429,#81430,#81431,#81432,#81433,#81434,#81435,#81436,
#81437,#81438,#81439,#81440,#81441,#81442,#81443,#81444,#81445,#81446,#81447,
#81448,#81449,#81450,#81451,#81452,#81453,#81454,#81455,#81456,#81457,#81458,
#81459,#81460,#81461,#81462,#81463,#81464,#81465,#81466,#81467,#81468,#81469,
#81470,#81471,#81472,#81473,#81474,#81475,#81476,#81477,#81478,#81479,#81480,
#81481,#81482,#81483,#81484,#81485,#81486,#81487,#81488,#81489,#81490,#81491)),
 .UNSPECIFIED.,.F.,.F.,.F.,(4,4),(4,1,1,1,1,1,1,1,1,1,1,1,1,1,1,1,1,1,1,
1,1,1,1,1,1,1,1,1,1,1,1,1,1,1,1,1,1,1,1,1,1,1,1,1,1,1,1,1,1,1,1,1,1,1,1,
1,1,1,1,1,1,1,1,1,1,1,1,1,1,1,1,1,1,1,1,1,1,1,1,1,1,1,1,1,1,1,1,1,1,1,1,
1,1,1,1,1,1,1,1,1,1,1,1,1,1,1,1,1,1,1,1,1,1,1,1,1,1,1,1,1,1,1,1,1,4),(-0.000266755740803004,
0.0504104417085662),(8.3394004212115,9.33690700317349,10.3344135851355,
11.3319201670975,12.3294267490595,13.3269333310215,14.3244399129835,15.3219464949454,
16.3194530769074,17.3169596588694,18.3144662408314,19.3119728227934,20.3094794047554,
21.3069859867174,22.3044925686794,23.3019991506414,24.2995057326034,25.2970123145654,
26.2945188965274,27.2920254784894,28.2895320604514,29.2870386424133,30.2845452243753,
31.2820518063373,32.2795583882993,33.2770649702613,34.2745715522233,35.2720781341853,
36.2695847161473,37.2670912981093,38.2645978800713,39.2621044620333,40.2596110439953,
41.2571176259573,42.2546242079192,43.2521307898812,44.2496373718432,45.2471439538052,
46.2446505357672,47.2421571177292,48.2396636996912,49.2371702816532,50.2346768636152,
51.2321834455772,52.2296900275392,53.2271966095012,54.2247031914632,55.2222097734252,
56.2197163553871,57.2172229373491,58.2147295193111,59.2122361012731,60.2097426832351,
61.2072492651971,62.2047558471591,63.2022624291211,64.1997690110831,65.1972755930451,
66.1947821750071,67.1922887569691,68.189795338931,69.187301920893,70.184808502855,
71.182315084817,72.179821666779,73.177328248741,74.174834830703,75.172341412665,
76.169847994627,77.167354576589,78.164861158551,79.162367740513,80.159874322475,
81.157380904437,82.154887486399,83.1523940683609,84.1499006503229,85.1474072322849,
86.1449138142469,87.1424203962089,88.1399269781709,89.1374335601329,90.1349401420949,
91.1324467240569,92.1299533060189,93.1274598879809,94.1249664699429,95.1224730519048,
96.1199796338668,97.1174862158288,98.1149927977908,99.1124993797528,100.110005961715,
101.107512543677,102.105019125639,103.102525707601,104.100032289563,105.097538871525,
106.095045453487,107.092552035449,108.090058617411,109.087565199373,110.085071781335,
111.082578363297,112.080084945259,113.077591527221,114.075098109183,115.072604691145,
116.070111273107,117.067617855069,118.065124437031,119.062631018993,120.060137600955,
121.057644182917,122.055150764879,123.052657346841,124.050163928803,125.047670510765,
126.045177092727,127.042683674689,128.040190256651,129.037696838613,130.035203420575,
131.032710002537,132.03048334024),.UNSPECIFIED.);
#904=B_SPLINE_SURFACE_WITH_KNOTS('',3,3,((#81661,#81662,#81663,#81664,#81665,
#81666,#81667,#81668,#81669,#81670,#81671,#81672,#81673,#81674,#81675,#81676,
#81677,#81678,#81679,#81680,#81681,#81682,#81683,#81684,#81685,#81686,#81687,
#81688,#81689,#81690,#81691,#81692,#81693,#81694,#81695,#81696,#81697,#81698,
#81699,#81700,#81701,#81702,#81703,#81704,#81705,#81706,#81707,#81708,#81709,
#81710,#81711,#81712,#81713,#81714,#81715,#81716,#81717,#81718,#81719,#81720,
#81721,#81722,#81723,#81724,#81725,#81726,#81727,#81728,#81729,#81730,#81731,
#81732,#81733,#81734,#81735,#81736,#81737,#81738,#81739,#81740,#81741,#81742,
#81743,#81744,#81745,#81746,#81747,#81748,#81749,#81750,#81751,#81752,#81753,
#81754,#81755,#81756,#81757,#81758,#81759,#81760,#81761,#81762,#81763,#81764,
#81765,#81766,#81767,#81768,#81769,#81770,#81771,#81772,#81773,#81774,#81775,
#81776,#81777,#81778,#81779,#81780,#81781,#81782,#81783,#81784,#81785,#81786,
#81787),(#81788,#81789,#81790,#81791,#81792,#81793,#81794,#81795,#81796,
#81797,#81798,#81799,#81800,#81801,#81802,#81803,#81804,#81805,#81806,#81807,
#81808,#81809,#81810,#81811,#81812,#81813,#81814,#81815,#81816,#81817,#81818,
#81819,#81820,#81821,#81822,#81823,#81824,#81825,#81826,#81827,#81828,#81829,
#81830,#81831,#81832,#81833,#81834,#81835,#81836,#81837,#81838,#81839,#81840,
#81841,#81842,#81843,#81844,#81845,#81846,#81847,#81848,#81849,#81850,#81851,
#81852,#81853,#81854,#81855,#81856,#81857,#81858,#81859,#81860,#81861,#81862,
#81863,#81864,#81865,#81866,#81867,#81868,#81869,#81870,#81871,#81872,#81873,
#81874,#81875,#81876,#81877,#81878,#81879,#81880,#81881,#81882,#81883,#81884,
#81885,#81886,#81887,#81888,#81889,#81890,#81891,#81892,#81893,#81894,#81895,
#81896,#81897,#81898,#81899,#81900,#81901,#81902,#81903,#81904,#81905,#81906,
#81907,#81908,#81909,#81910,#81911,#81912,#81913,#81914),(#81915,#81916,
#81917,#81918,#81919,#81920,#81921,#81922,#81923,#81924,#81925,#81926,#81927,
#81928,#81929,#81930,#81931,#81932,#81933,#81934,#81935,#81936,#81937,#81938,
#81939,#81940,#81941,#81942,#81943,#81944,#81945,#81946,#81947,#81948,#81949,
#81950,#81951,#81952,#81953,#81954,#81955,#81956,#81957,#81958,#81959,#81960,
#81961,#81962,#81963,#81964,#81965,#81966,#81967,#81968,#81969,#81970,#81971,
#81972,#81973,#81974,#81975,#81976,#81977,#81978,#81979,#81980,#81981,#81982,
#81983,#81984,#81985,#81986,#81987,#81988,#81989,#81990,#81991,#81992,#81993,
#81994,#81995,#81996,#81997,#81998,#81999,#82000,#82001,#82002,#82003,#82004,
#82005,#82006,#82007,#82008,#82009,#82010,#82011,#82012,#82013,#82014,#82015,
#82016,#82017,#82018,#82019,#82020,#82021,#82022,#82023,#82024,#82025,#82026,
#82027,#82028,#82029,#82030,#82031,#82032,#82033,#82034,#82035,#82036,#82037,
#82038,#82039,#82040,#82041),(#82042,#82043,#82044,#82045,#82046,#82047,
#82048,#82049,#82050,#82051,#82052,#82053,#82054,#82055,#82056,#82057,#82058,
#82059,#82060,#82061,#82062,#82063,#82064,#82065,#82066,#82067,#82068,#82069,
#82070,#82071,#82072,#82073,#82074,#82075,#82076,#82077,#82078,#82079,#82080,
#82081,#82082,#82083,#82084,#82085,#82086,#82087,#82088,#82089,#82090,#82091,
#82092,#82093,#82094,#82095,#82096,#82097,#82098,#82099,#82100,#82101,#82102,
#82103,#82104,#82105,#82106,#82107,#82108,#82109,#82110,#82111,#82112,#82113,
#82114,#82115,#82116,#82117,#82118,#82119,#82120,#82121,#82122,#82123,#82124,
#82125,#82126,#82127,#82128,#82129,#82130,#82131,#82132,#82133,#82134,#82135,
#82136,#82137,#82138,#82139,#82140,#82141,#82142,#82143,#82144,#82145,#82146,
#82147,#82148,#82149,#82150,#82151,#82152,#82153,#82154,#82155,#82156,#82157,
#82158,#82159,#82160,#82161,#82162,#82163,#82164,#82165,#82166,#82167,#82168)),
 .UNSPECIFIED.,.F.,.F.,.F.,(4,4),(4,1,1,1,1,1,1,1,1,1,1,1,1,1,1,1,1,1,1,
1,1,1,1,1,1,1,1,1,1,1,1,1,1,1,1,1,1,1,1,1,1,1,1,1,1,1,1,1,1,1,1,1,1,1,1,
1,1,1,1,1,1,1,1,1,1,1,1,1,1,1,1,1,1,1,1,1,1,1,1,1,1,1,1,1,1,1,1,1,1,1,1,
1,1,1,1,1,1,1,1,1,1,1,1,1,1,1,1,1,1,1,1,1,1,1,1,1,1,1,1,1,1,1,1,1,4),(-0.000246377393080283,
0.0504200384722922),(11.6664593544106,12.6642327116609,13.6617392936229,
14.6592458755849,15.6567524575469,16.6542590395089,17.6517656214709,18.6492722034329,
19.6467787853949,20.6442853673569,21.6417919493189,22.6392985312808,23.6368051132428,
24.6343116952048,25.6318182771668,26.6293248591288,27.6268314410908,28.6243380230528,
29.6218446050148,30.6193511869768,31.6168577689388,32.6143643509008,33.6118709328628,
34.6093775148248,35.6068840967868,36.6043906787487,37.6018972607107,38.5994038426727,
39.5969104246347,40.5944170065967,41.5919235885587,42.5894301705207,43.5869367524827,
44.5844433344447,45.5819499164067,46.5794564983687,47.5769630803307,48.5744696622927,
49.5719762442546,50.5694828262166,51.5669894081786,52.5644959901406,53.5620025721026,
54.5595091540646,55.5570157360266,56.5545223179886,57.5520288999506,58.5495354819126,
59.5470420638746,60.5445486458366,61.5420552277986,62.5395618097606,63.5370683917225,
64.5345749736845,65.5320815556465,66.5295881376085,67.5270947195705,68.5246013015325,
69.5221078834945,70.5196144654565,71.5171210474185,72.5146276293805,73.5121342113425,
74.5096407933045,75.5071473752665,76.5046539572285,77.5021605391904,78.4996671211524,
79.4971737031144,80.4946802850764,81.4921868670384,82.4896934490004,83.4872000309624,
84.4847066129244,85.4822131948864,86.4797197768484,87.4772263588104,88.4747329407724,
89.4722395227344,90.4697461046964,91.4672526866584,92.4647592686204,93.4622658505823,
94.4597724325443,95.4572790145063,96.4547855964683,97.4522921784303,98.4497987603923,
99.4473053423543,100.444811924316,101.442318506278,102.43982508824,103.437331670202,
104.434838252164,105.432344834126,106.429851416088,107.42735799805,108.424864580012,
109.422371161974,110.419877743936,111.417384325898,112.41489090786,113.412397489822,
114.409904071784,115.407410653746,116.404917235708,117.40242381767,118.399930399632,
119.397436981594,120.394943563556,121.392450145518,122.38995672748,123.387463309442,
124.384969891404,125.382476473366,126.379983055328,127.37748963729,128.374996219252,
129.372502801214,130.370009383176,131.367515965138,132.3650225471,133.362529129062,
134.360035711024,135.357542292986),.UNSPECIFIED.);
#905=SHAPE_REPRESENTATION_RELATIONSHIP('SRR','None',#83300,#919);
#906=SHAPE_REPRESENTATION_RELATIONSHIP('SRR','None',#83301,#920);
#907=SHAPE_REPRESENTATION_RELATIONSHIP('SRR','None',#83302,#921);
#908=SHAPE_REPRESENTATION_RELATIONSHIP('SRR','None',#83303,#922);
#909=SHAPE_REPRESENTATION_RELATIONSHIP('SRR','None',#83304,#923);
#910=SHAPE_REPRESENTATION_RELATIONSHIP('SRR','None',#83305,#924);
#911=SHAPE_REPRESENTATION_RELATIONSHIP('SRR','None',#83306,#925);
#912=SHAPE_REPRESENTATION_RELATIONSHIP('SRR','None',#83307,#926);
#913=SHAPE_REPRESENTATION_RELATIONSHIP('SRR','None',#83308,#927);
#914=SHAPE_REPRESENTATION_RELATIONSHIP('SRR','None',#83309,#928);
#915=SHAPE_REPRESENTATION_RELATIONSHIP('SRR','None',#83310,#929);
#916=SHAPE_REPRESENTATION_RELATIONSHIP('SRR','None',#83311,#930);
#917=SHAPE_REPRESENTATION_RELATIONSHIP('SRR','None',#83312,#931);
#918=SHAPE_REPRESENTATION_RELATIONSHIP('SRR','None',#83313,#932);
#919=ADVANCED_BREP_SHAPE_REPRESENTATION('',(#947),#83205);
#920=ADVANCED_BREP_SHAPE_REPRESENTATION('',(#948),#83206);
#921=ADVANCED_BREP_SHAPE_REPRESENTATION('',(#949),#83207);
#922=ADVANCED_BREP_SHAPE_REPRESENTATION('',(#950),#83208);
#923=ADVANCED_BREP_SHAPE_REPRESENTATION('',(#951),#83209);
#924=ADVANCED_BREP_SHAPE_REPRESENTATION('',(#952),#83210);
#925=ADVANCED_BREP_SHAPE_REPRESENTATION('',(#953),#83211);
#926=ADVANCED_BREP_SHAPE_REPRESENTATION('',(#954),#83212);
#927=ADVANCED_BREP_SHAPE_REPRESENTATION('',(#955),#83213);
#928=ADVANCED_BREP_SHAPE_REPRESENTATION('',(#956),#83214);
#929=ADVANCED_BREP_SHAPE_REPRESENTATION('',(#957),#83215);
#930=ADVANCED_BREP_SHAPE_REPRESENTATION('',(#958),#83216);
#931=ADVANCED_BREP_SHAPE_REPRESENTATION('',(#959),#83217);
#932=ADVANCED_BREP_SHAPE_REPRESENTATION('',(#960),#83218);
#933=STYLED_ITEM('',(#83379),#947);
#934=STYLED_ITEM('',(#83380),#948);
#935=STYLED_ITEM('',(#83381),#949);
#936=STYLED_ITEM('',(#83382),#950);
#937=STYLED_ITEM('',(#83383),#951);
#938=STYLED_ITEM('',(#83384),#952);
#939=STYLED_ITEM('',(#83385),#953);
#940=STYLED_ITEM('',(#83386),#954);
#941=STYLED_ITEM('',(#83387),#955);
#942=STYLED_ITEM('',(#83388),#956);
#943=STYLED_ITEM('',(#83389),#957);
#944=STYLED_ITEM('',(#83390),#958);
#945=STYLED_ITEM('',(#83391),#959);
#946=STYLED_ITEM('',(#83392),#960);
#947=MANIFOLD_SOLID_BREP('Body1',#26929);
#948=MANIFOLD_SOLID_BREP('Body1',#26930);
#949=MANIFOLD_SOLID_BREP('Body1',#26931);
#950=MANIFOLD_SOLID_BREP('Body1',#26932);
#951=MANIFOLD_SOLID_BREP('Body1',#26933);
#952=MANIFOLD_SOLID_BREP('Body1',#26934);
#953=MANIFOLD_SOLID_BREP('Body1',#26935);
#954=MANIFOLD_SOLID_BREP('Body1',#26936);
#955=MANIFOLD_SOLID_BREP('Body1',#26937);
#956=MANIFOLD_SOLID_BREP('Body1',#26938);
#957=MANIFOLD_SOLID_BREP('Body1',#26939);
#958=MANIFOLD_SOLID_BREP('Body1',#26940);
#959=MANIFOLD_SOLID_BREP('Body1',#26941);
#960=MANIFOLD_SOLID_BREP('Body1',#26942);
#961=FACE_BOUND('',#3739,.T.);
#962=FACE_BOUND('',#3743,.T.);
#963=FACE_BOUND('',#3749,.T.);
#964=FACE_BOUND('',#3753,.T.);
#965=FACE_BOUND('',#3762,.T.);
#966=FACE_BOUND('',#3763,.T.);
#967=FACE_BOUND('',#3764,.T.);
#968=FACE_BOUND('',#3765,.T.);
#969=FACE_BOUND('',#3766,.T.);
#970=FACE_BOUND('',#3767,.T.);
#971=FACE_BOUND('',#3768,.T.);
#972=FACE_BOUND('',#3769,.T.);
#973=FACE_BOUND('',#3770,.T.);
#974=FACE_BOUND('',#3814,.T.);
#975=FACE_BOUND('',#3815,.T.);
#976=FACE_BOUND('',#3816,.T.);
#977=FACE_BOUND('',#3817,.T.);
#978=FACE_BOUND('',#3818,.T.);
#979=FACE_BOUND('',#3819,.T.);
#980=FACE_BOUND('',#3820,.T.);
#981=FACE_BOUND('',#3821,.T.);
#982=FACE_BOUND('',#3822,.T.);
#983=FACE_BOUND('',#3828,.T.);
#984=FACE_BOUND('',#3829,.T.);
#985=FACE_BOUND('',#3830,.T.);
#986=FACE_BOUND('',#3831,.T.);
#987=FACE_BOUND('',#3832,.T.);
#988=FACE_BOUND('',#3833,.T.);
#989=FACE_BOUND('',#3834,.T.);
#990=FACE_BOUND('',#3835,.T.);
#991=FACE_BOUND('',#3836,.T.);
#992=FACE_BOUND('',#3846,.T.);
#993=FACE_BOUND('',#3847,.T.);
#994=FACE_BOUND('',#3848,.T.);
#995=FACE_BOUND('',#3849,.T.);
#996=FACE_BOUND('',#3850,.T.);
#997=FACE_BOUND('',#3851,.T.);
#998=FACE_BOUND('',#3852,.T.);
#999=FACE_BOUND('',#3853,.T.);
#1000=FACE_BOUND('',#3854,.T.);
#1001=FACE_BOUND('',#3951,.T.);
#1002=FACE_BOUND('',#3957,.T.);
#1003=FACE_BOUND('',#3966,.T.);
#1004=FACE_BOUND('',#3968,.T.);
#1005=FACE_BOUND('',#3969,.T.);
#1006=FACE_BOUND('',#3971,.T.);
#1007=FACE_BOUND('',#3972,.T.);
#1008=FACE_BOUND('',#3974,.T.);
#1009=FACE_BOUND('',#3975,.T.);
#1010=FACE_BOUND('',#3985,.T.);
#1011=FACE_BOUND('',#3986,.T.);
#1012=FACE_BOUND('',#3993,.T.);
#1013=FACE_BOUND('',#4005,.T.);
#1014=FACE_BOUND('',#4091,.T.);
#1015=FACE_BOUND('',#4100,.T.);
#1016=FACE_BOUND('',#4103,.T.);
#1017=FACE_BOUND('',#4136,.T.);
#1018=FACE_BOUND('',#4251,.T.);
#1019=FACE_BOUND('',#4280,.T.);
#1020=FACE_BOUND('',#4281,.T.);
#1021=FACE_BOUND('',#4282,.T.);
#1022=FACE_BOUND('',#4283,.T.);
#1023=FACE_BOUND('',#4284,.T.);
#1024=FACE_BOUND('',#4285,.T.);
#1025=FACE_BOUND('',#4286,.T.);
#1026=FACE_BOUND('',#4287,.T.);
#1027=FACE_BOUND('',#4288,.T.);
#1028=FACE_BOUND('',#4289,.T.);
#1029=FACE_BOUND('',#4290,.T.);
#1030=FACE_BOUND('',#4291,.T.);
#1031=FACE_BOUND('',#4292,.T.);
#1032=FACE_BOUND('',#4293,.T.);
#1033=FACE_BOUND('',#4294,.T.);
#1034=FACE_BOUND('',#4295,.T.);
#1035=FACE_BOUND('',#4296,.T.);
#1036=FACE_BOUND('',#4297,.T.);
#1037=FACE_BOUND('',#4298,.T.);
#1038=FACE_BOUND('',#4299,.T.);
#1039=FACE_BOUND('',#4300,.T.);
#1040=FACE_BOUND('',#4354,.T.);
#1041=FACE_BOUND('',#4355,.T.);
#1042=FACE_BOUND('',#4356,.T.);
#1043=FACE_BOUND('',#4357,.T.);
#1044=FACE_BOUND('',#4358,.T.);
#1045=FACE_BOUND('',#4359,.T.);
#1046=FACE_BOUND('',#4360,.T.);
#1047=FACE_BOUND('',#4361,.T.);
#1048=FACE_BOUND('',#4362,.T.);
#1049=FACE_BOUND('',#4363,.T.);
#1050=FACE_BOUND('',#4364,.T.);
#1051=FACE_BOUND('',#4365,.T.);
#1052=FACE_BOUND('',#4366,.T.);
#1053=FACE_BOUND('',#4367,.T.);
#1054=FACE_BOUND('',#4368,.T.);
#1055=FACE_BOUND('',#4369,.T.);
#1056=FACE_BOUND('',#4370,.T.);
#1057=FACE_BOUND('',#4371,.T.);
#1058=FACE_BOUND('',#4372,.T.);
#1059=FACE_BOUND('',#4373,.T.);
#1060=FACE_BOUND('',#4374,.T.);
#1061=FACE_BOUND('',#4681,.T.);
#1062=FACE_BOUND('',#4682,.T.);
#1063=FACE_BOUND('',#4683,.T.);
#1064=FACE_BOUND('',#4684,.T.);
#1065=FACE_BOUND('',#4685,.T.);
#1066=FACE_BOUND('',#4686,.T.);
#1067=FACE_BOUND('',#4687,.T.);
#1068=FACE_BOUND('',#4688,.T.);
#1069=FACE_BOUND('',#4689,.T.);
#1070=FACE_BOUND('',#4690,.T.);
#1071=FACE_BOUND('',#4692,.T.);
#1072=FACE_BOUND('',#4693,.T.);
#1073=FACE_BOUND('',#4694,.T.);
#1074=FACE_BOUND('',#4695,.T.);
#1075=FACE_BOUND('',#4696,.T.);
#1076=FACE_BOUND('',#4697,.T.);
#1077=FACE_BOUND('',#4698,.T.);
#1078=FACE_BOUND('',#4699,.T.);
#1079=FACE_BOUND('',#4700,.T.);
#1080=FACE_BOUND('',#4701,.T.);
#1081=FACE_BOUND('',#4704,.T.);
#1082=FACE_BOUND('',#4705,.T.);
#1083=FACE_BOUND('',#4706,.T.);
#1084=FACE_BOUND('',#4707,.T.);
#1085=FACE_BOUND('',#4708,.T.);
#1086=FACE_BOUND('',#4709,.T.);
#1087=FACE_BOUND('',#4710,.T.);
#1088=FACE_BOUND('',#4711,.T.);
#1089=FACE_BOUND('',#4712,.T.);
#1090=FACE_BOUND('',#4713,.T.);
#1091=FACE_BOUND('',#4758,.T.);
#1092=FACE_BOUND('',#4759,.T.);
#1093=FACE_BOUND('',#4760,.T.);
#1094=FACE_BOUND('',#4761,.T.);
#1095=FACE_BOUND('',#4762,.T.);
#1096=FACE_BOUND('',#4763,.T.);
#1097=FACE_BOUND('',#4764,.T.);
#1098=FACE_BOUND('',#4765,.T.);
#1099=FACE_BOUND('',#4766,.T.);
#1100=FACE_BOUND('',#4767,.T.);
#1101=FACE_BOUND('',#4773,.T.);
#1102=FACE_BOUND('',#4777,.T.);
#1103=FACE_BOUND('',#4781,.T.);
#1104=FACE_BOUND('',#4785,.T.);
#1105=FACE_BOUND('',#4788,.T.);
#1106=FACE_BOUND('',#4792,.T.);
#1107=FACE_BOUND('',#4801,.T.);
#1108=FACE_BOUND('',#4802,.T.);
#1109=FACE_BOUND('',#4804,.T.);
#1110=FACE_BOUND('',#4805,.T.);
#1111=FACE_BOUND('',#4821,.T.);
#1112=FACE_BOUND('',#4935,.T.);
#1113=FACE_BOUND('',#4966,.T.);
#1114=FACE_BOUND('',#5080,.T.);
#1115=FACE_BOUND('',#5121,.T.);
#1116=FACE_BOUND('',#5235,.T.);
#1117=FACE_BOUND('',#5251,.T.);
#1118=FACE_BOUND('',#5255,.T.);
#1119=FACE_BOUND('',#5260,.T.);
#1120=FACE_BOUND('',#5264,.T.);
#1121=FACE_BOUND('',#5267,.T.);
#1122=FACE_BOUND('',#5276,.T.);
#1123=PLANE('',#27106);
#1124=PLANE('',#27113);
#1125=PLANE('',#27122);
#1126=PLANE('',#27129);
#1127=PLANE('',#27147);
#1128=PLANE('',#27170);
#1129=PLANE('',#27171);
#1130=PLANE('',#27172);
#1131=PLANE('',#27173);
#1132=PLANE('',#27174);
#1133=PLANE('',#27175);
#1134=PLANE('',#27176);
#1135=PLANE('',#27177);
#1136=PLANE('',#27178);
#1137=PLANE('',#27179);
#1138=PLANE('',#27180);
#1139=PLANE('',#27181);
#1140=PLANE('',#27182);
#1141=PLANE('',#27183);
#1142=PLANE('',#27184);
#1143=PLANE('',#27185);
#1144=PLANE('',#27186);
#1145=PLANE('',#27187);
#1146=PLANE('',#27188);
#1147=PLANE('',#27189);
#1148=PLANE('',#27190);
#1149=PLANE('',#27191);
#1150=PLANE('',#27192);
#1151=PLANE('',#27193);
#1152=PLANE('',#27194);
#1153=PLANE('',#27195);
#1154=PLANE('',#27196);
#1155=PLANE('',#27197);
#1156=PLANE('',#27198);
#1157=PLANE('',#27199);
#1158=PLANE('',#27200);
#1159=PLANE('',#27201);
#1160=PLANE('',#27202);
#1161=PLANE('',#27203);
#1162=PLANE('',#27204);
#1163=PLANE('',#27205);
#1164=PLANE('',#27206);
#1165=PLANE('',#27211);
#1166=PLANE('',#27246);
#1167=PLANE('',#27270);
#1168=PLANE('',#27271);
#1169=PLANE('',#27272);
#1170=PLANE('',#27273);
#1171=PLANE('',#27274);
#1172=PLANE('',#27275);
#1173=PLANE('',#27276);
#1174=PLANE('',#27277);
#1175=PLANE('',#27278);
#1176=PLANE('',#27279);
#1177=PLANE('',#27280);
#1178=PLANE('',#27281);
#1179=PLANE('',#27282);
#1180=PLANE('',#27285);
#1181=PLANE('',#27288);
#1182=PLANE('',#27291);
#1183=PLANE('',#27294);
#1184=PLANE('',#27295);
#1185=PLANE('',#27296);
#1186=PLANE('',#27297);
#1187=PLANE('',#27298);
#1188=PLANE('',#27299);
#1189=PLANE('',#27300);
#1190=PLANE('',#27301);
#1191=PLANE('',#27302);
#1192=PLANE('',#27303);
#1193=PLANE('',#27304);
#1194=PLANE('',#27305);
#1195=PLANE('',#27307);
#1196=PLANE('',#27309);
#1197=PLANE('',#27310);
#1198=PLANE('',#27311);
#1199=PLANE('',#27312);
#1200=PLANE('',#27315);
#1201=PLANE('',#27316);
#1202=PLANE('',#27319);
#1203=PLANE('',#27322);
#1204=PLANE('',#27325);
#1205=PLANE('',#27328);
#1206=PLANE('',#27331);
#1207=PLANE('',#27332);
#1208=PLANE('',#27334);
#1209=PLANE('',#27335);
#1210=PLANE('',#27337);
#1211=PLANE('',#27339);
#1212=PLANE('',#27340);
#1213=PLANE('',#27341);
#1214=PLANE('',#27343);
#1215=PLANE('',#27344);
#1216=PLANE('',#27346);
#1217=PLANE('',#27348);
#1218=PLANE('',#27349);
#1219=PLANE('',#27350);
#1220=PLANE('',#27351);
#1221=PLANE('',#27352);
#1222=PLANE('',#27353);
#1223=PLANE('',#27354);
#1224=PLANE('',#27355);
#1225=PLANE('',#27357);
#1226=PLANE('',#27359);
#1227=PLANE('',#27364);
#1228=PLANE('',#27382);
#1229=PLANE('',#27392);
#1230=PLANE('',#27395);
#1231=PLANE('',#27402);
#1232=PLANE('',#27409);
#1233=PLANE('',#27410);
#1234=PLANE('',#27413);
#1235=PLANE('',#27416);
#1236=PLANE('',#27421);
#1237=PLANE('',#27423);
#1238=PLANE('',#27426);
#1239=PLANE('',#27429);
#1240=PLANE('',#27431);
#1241=PLANE('',#27434);
#1242=PLANE('',#27437);
#1243=PLANE('',#27441);
#1244=PLANE('',#27445);
#1245=PLANE('',#27448);
#1246=PLANE('',#27451);
#1247=PLANE('',#27452);
#1248=PLANE('',#27454);
#1249=PLANE('',#27458);
#1250=PLANE('',#27459);
#1251=PLANE('',#27494);
#1252=PLANE('',#27497);
#1253=PLANE('',#27500);
#1254=PLANE('',#27503);
#1255=PLANE('',#27506);
#1256=PLANE('',#27509);
#1257=PLANE('',#27512);
#1258=PLANE('',#27515);
#1259=PLANE('',#27518);
#1260=PLANE('',#27521);
#1261=PLANE('',#27524);
#1262=PLANE('',#27527);
#1263=PLANE('',#27530);
#1264=PLANE('',#27533);
#1265=PLANE('',#27536);
#1266=PLANE('',#27539);
#1267=PLANE('',#27542);
#1268=PLANE('',#27545);
#1269=PLANE('',#27548);
#1270=PLANE('',#27551);
#1271=PLANE('',#27554);
#1272=PLANE('',#27557);
#1273=PLANE('',#27560);
#1274=PLANE('',#27563);
#1275=PLANE('',#27566);
#1276=PLANE('',#27569);
#1277=PLANE('',#27572);
#1278=PLANE('',#27573);
#1279=PLANE('',#27576);
#1280=PLANE('',#27582);
#1281=PLANE('',#27584);
#1282=PLANE('',#27586);
#1283=PLANE('',#27591);
#1284=PLANE('',#27624);
#1285=PLANE('',#27627);
#1286=PLANE('',#27633);
#1287=PLANE('',#27637);
#1288=PLANE('',#27638);
#1289=PLANE('',#27639);
#1290=PLANE('',#27641);
#1291=PLANE('',#27717);
#1292=PLANE('',#27718);
#1293=PLANE('',#27719);
#1294=PLANE('',#27720);
#1295=PLANE('',#27721);
#1296=PLANE('',#27722);
#1297=PLANE('',#27723);
#1298=PLANE('',#27724);
#1299=PLANE('',#27725);
#1300=PLANE('',#27726);
#1301=PLANE('',#27727);
#1302=PLANE('',#27728);
#1303=PLANE('',#27729);
#1304=PLANE('',#27730);
#1305=PLANE('',#27731);
#1306=PLANE('',#27732);
#1307=PLANE('',#27733);
#1308=PLANE('',#27734);
#1309=PLANE('',#27735);
#1310=PLANE('',#27736);
#1311=PLANE('',#27737);
#1312=PLANE('',#27738);
#1313=PLANE('',#27739);
#1314=PLANE('',#27740);
#1315=PLANE('',#27741);
#1316=PLANE('',#27742);
#1317=PLANE('',#27743);
#1318=PLANE('',#27744);
#1319=PLANE('',#27745);
#1320=PLANE('',#27746);
#1321=PLANE('',#27747);
#1322=PLANE('',#27748);
#1323=PLANE('',#27749);
#1324=PLANE('',#27750);
#1325=PLANE('',#27751);
#1326=PLANE('',#27752);
#1327=PLANE('',#27753);
#1328=PLANE('',#27754);
#1329=PLANE('',#27755);
#1330=PLANE('',#27756);
#1331=PLANE('',#27757);
#1332=PLANE('',#27758);
#1333=PLANE('',#27759);
#1334=PLANE('',#27760);
#1335=PLANE('',#27761);
#1336=PLANE('',#27762);
#1337=PLANE('',#27763);
#1338=PLANE('',#27764);
#1339=PLANE('',#27765);
#1340=PLANE('',#27766);
#1341=PLANE('',#27767);
#1342=PLANE('',#27768);
#1343=PLANE('',#27769);
#1344=PLANE('',#27770);
#1345=PLANE('',#27771);
#1346=PLANE('',#27772);
#1347=PLANE('',#27773);
#1348=PLANE('',#27774);
#1349=PLANE('',#27775);
#1350=PLANE('',#27776);
#1351=PLANE('',#27777);
#1352=PLANE('',#27778);
#1353=PLANE('',#27779);
#1354=PLANE('',#27780);
#1355=PLANE('',#27781);
#1356=PLANE('',#27782);
#1357=PLANE('',#27783);
#1358=PLANE('',#27784);
#1359=PLANE('',#27785);
#1360=PLANE('',#27786);
#1361=PLANE('',#27787);
#1362=PLANE('',#27788);
#1363=PLANE('',#27789);
#1364=PLANE('',#27790);
#1365=PLANE('',#27791);
#1366=PLANE('',#27792);
#1367=PLANE('',#27793);
#1368=PLANE('',#27794);
#1369=PLANE('',#27795);
#1370=PLANE('',#27796);
#1371=PLANE('',#27797);
#1372=PLANE('',#27798);
#1373=PLANE('',#27799);
#1374=PLANE('',#27800);
#1375=PLANE('',#27801);
#1376=PLANE('',#27802);
#1377=PLANE('',#27803);
#1378=PLANE('',#27804);
#1379=PLANE('',#27805);
#1380=PLANE('',#27806);
#1381=PLANE('',#27807);
#1382=PLANE('',#27808);
#1383=PLANE('',#27809);
#1384=PLANE('',#27810);
#1385=PLANE('',#27811);
#1386=PLANE('',#27812);
#1387=PLANE('',#27813);
#1388=PLANE('',#27814);
#1389=PLANE('',#27815);
#1390=PLANE('',#27816);
#1391=PLANE('',#27817);
#1392=PLANE('',#27818);
#1393=PLANE('',#27819);
#1394=PLANE('',#27820);
#1395=PLANE('',#27821);
#1396=PLANE('',#27826);
#1397=PLANE('',#27847);
#1398=PLANE('',#27848);
#1399=PLANE('',#27849);
#1400=PLANE('',#27850);
#1401=PLANE('',#27851);
#1402=PLANE('',#27852);
#1403=PLANE('',#27853);
#1404=PLANE('',#27854);
#1405=PLANE('',#27855);
#1406=PLANE('',#27856);
#1407=PLANE('',#27858);
#1408=PLANE('',#27860);
#1409=PLANE('',#27862);
#1410=PLANE('',#27864);
#1411=PLANE('',#27866);
#1412=PLANE('',#27869);
#1413=PLANE('',#27870);
#1414=PLANE('',#27871);
#1415=PLANE('',#27876);
#1416=PLANE('',#27981);
#1417=PLANE('',#27984);
#1418=PLANE('',#27989);
#1419=PLANE('',#27990);
#1420=PLANE('',#27994);
#1421=PLANE('',#27998);
#1422=PLANE('',#27999);
#1423=PLANE('',#28001);
#1424=PLANE('',#28005);
#1425=PLANE('',#28009);
#1426=PLANE('',#28010);
#1427=PLANE('',#28013);
#1428=PLANE('',#28016);
#1429=PLANE('',#28017);
#1430=PLANE('',#28020);
#1431=PLANE('',#28023);
#1432=PLANE('',#28054);
#1433=PLANE('',#28055);
#1434=PLANE('',#28056);
#1435=PLANE('',#28057);
#1436=PLANE('',#28058);
#1437=PLANE('',#28059);
#1438=PLANE('',#28060);
#1439=PLANE('',#28061);
#1440=PLANE('',#28062);
#1441=PLANE('',#28063);
#1442=PLANE('',#28064);
#1443=PLANE('',#28065);
#1444=PLANE('',#28066);
#1445=PLANE('',#28067);
#1446=PLANE('',#28068);
#1447=PLANE('',#28069);
#1448=PLANE('',#28070);
#1449=PLANE('',#28071);
#1450=PLANE('',#28072);
#1451=PLANE('',#28073);
#1452=PLANE('',#28074);
#1453=PLANE('',#28075);
#1454=PLANE('',#28076);
#1455=PLANE('',#28077);
#1456=PLANE('',#28078);
#1457=PLANE('',#28079);
#1458=PLANE('',#28080);
#1459=PLANE('',#28081);
#1460=PLANE('',#28082);
#1461=PLANE('',#28083);
#1462=PLANE('',#28084);
#1463=PLANE('',#28085);
#1464=PLANE('',#28086);
#1465=PLANE('',#28087);
#1466=PLANE('',#28088);
#1467=PLANE('',#28089);
#1468=PLANE('',#28090);
#1469=PLANE('',#28091);
#1470=PLANE('',#28092);
#1471=PLANE('',#28093);
#1472=PLANE('',#28094);
#1473=PLANE('',#28095);
#1474=PLANE('',#28096);
#1475=PLANE('',#28097);
#1476=PLANE('',#28098);
#1477=PLANE('',#28099);
#1478=PLANE('',#28100);
#1479=PLANE('',#28101);
#1480=PLANE('',#28102);
#1481=PLANE('',#28103);
#1482=PLANE('',#28104);
#1483=PLANE('',#28105);
#1484=PLANE('',#28106);
#1485=PLANE('',#28107);
#1486=PLANE('',#28108);
#1487=PLANE('',#28109);
#1488=PLANE('',#28110);
#1489=PLANE('',#28111);
#1490=PLANE('',#28112);
#1491=PLANE('',#28113);
#1492=PLANE('',#28114);
#1493=PLANE('',#28115);
#1494=PLANE('',#28116);
#1495=PLANE('',#28117);
#1496=PLANE('',#28118);
#1497=PLANE('',#28119);
#1498=PLANE('',#28120);
#1499=PLANE('',#28121);
#1500=PLANE('',#28122);
#1501=PLANE('',#28123);
#1502=PLANE('',#28124);
#1503=PLANE('',#28125);
#1504=PLANE('',#28126);
#1505=PLANE('',#28127);
#1506=PLANE('',#28128);
#1507=PLANE('',#28129);
#1508=PLANE('',#28130);
#1509=PLANE('',#28131);
#1510=PLANE('',#28132);
#1511=PLANE('',#28133);
#1512=PLANE('',#28134);
#1513=PLANE('',#28135);
#1514=PLANE('',#28136);
#1515=PLANE('',#28137);
#1516=PLANE('',#28138);
#1517=PLANE('',#28139);
#1518=PLANE('',#28140);
#1519=PLANE('',#28141);
#1520=PLANE('',#28142);
#1521=PLANE('',#28143);
#1522=PLANE('',#28144);
#1523=PLANE('',#28145);
#1524=PLANE('',#28146);
#1525=PLANE('',#28147);
#1526=PLANE('',#28148);
#1527=PLANE('',#28149);
#1528=PLANE('',#28150);
#1529=PLANE('',#28151);
#1530=PLANE('',#28152);
#1531=PLANE('',#28153);
#1532=PLANE('',#28154);
#1533=PLANE('',#28155);
#1534=PLANE('',#28156);
#1535=PLANE('',#28157);
#1536=PLANE('',#28158);
#1537=PLANE('',#28159);
#1538=PLANE('',#28160);
#1539=PLANE('',#28161);
#1540=PLANE('',#28162);
#1541=PLANE('',#28163);
#1542=PLANE('',#28164);
#1543=PLANE('',#28165);
#1544=PLANE('',#28166);
#1545=PLANE('',#28167);
#1546=PLANE('',#28168);
#1547=PLANE('',#28169);
#1548=PLANE('',#28170);
#1549=PLANE('',#28171);
#1550=PLANE('',#28172);
#1551=PLANE('',#28173);
#1552=PLANE('',#28174);
#1553=PLANE('',#28175);
#1554=PLANE('',#28176);
#1555=PLANE('',#28177);
#1556=PLANE('',#28178);
#1557=PLANE('',#28179);
#1558=PLANE('',#28180);
#1559=PLANE('',#28181);
#1560=PLANE('',#28182);
#1561=PLANE('',#28183);
#1562=PLANE('',#28184);
#1563=PLANE('',#28185);
#1564=PLANE('',#28186);
#1565=PLANE('',#28187);
#1566=PLANE('',#28188);
#1567=PLANE('',#28189);
#1568=PLANE('',#28190);
#1569=PLANE('',#28191);
#1570=PLANE('',#28192);
#1571=PLANE('',#28193);
#1572=PLANE('',#28194);
#1573=PLANE('',#28195);
#1574=PLANE('',#28196);
#1575=PLANE('',#28197);
#1576=PLANE('',#28198);
#1577=PLANE('',#28199);
#1578=PLANE('',#28200);
#1579=PLANE('',#28201);
#1580=PLANE('',#28202);
#1581=PLANE('',#28203);
#1582=PLANE('',#28204);
#1583=PLANE('',#28205);
#1584=PLANE('',#28206);
#1585=PLANE('',#28207);
#1586=PLANE('',#28208);
#1587=PLANE('',#28209);
#1588=PLANE('',#28210);
#1589=PLANE('',#28211);
#1590=PLANE('',#28212);
#1591=PLANE('',#28213);
#1592=PLANE('',#28214);
#1593=PLANE('',#28215);
#1594=PLANE('',#28216);
#1595=PLANE('',#28217);
#1596=PLANE('',#28218);
#1597=PLANE('',#28219);
#1598=PLANE('',#28220);
#1599=PLANE('',#28221);
#1600=PLANE('',#28222);
#1601=PLANE('',#28223);
#1602=PLANE('',#28224);
#1603=PLANE('',#28225);
#1604=PLANE('',#28226);
#1605=PLANE('',#28227);
#1606=PLANE('',#28228);
#1607=PLANE('',#28229);
#1608=PLANE('',#28230);
#1609=PLANE('',#28231);
#1610=PLANE('',#28232);
#1611=PLANE('',#28233);
#1612=PLANE('',#28234);
#1613=PLANE('',#28235);
#1614=PLANE('',#28236);
#1615=PLANE('',#28237);
#1616=PLANE('',#28238);
#1617=PLANE('',#28239);
#1618=PLANE('',#28240);
#1619=PLANE('',#28241);
#1620=PLANE('',#28242);
#1621=PLANE('',#28243);
#1622=PLANE('',#28244);
#1623=PLANE('',#28245);
#1624=PLANE('',#28246);
#1625=PLANE('',#28247);
#1626=PLANE('',#28248);
#1627=PLANE('',#28249);
#1628=PLANE('',#28250);
#1629=PLANE('',#28251);
#1630=PLANE('',#28252);
#1631=PLANE('',#28253);
#1632=PLANE('',#28254);
#1633=PLANE('',#28255);
#1634=PLANE('',#28256);
#1635=PLANE('',#28257);
#1636=PLANE('',#28258);
#1637=PLANE('',#28259);
#1638=PLANE('',#28260);
#1639=PLANE('',#28261);
#1640=PLANE('',#28262);
#1641=PLANE('',#28263);
#1642=PLANE('',#28264);
#1643=PLANE('',#28265);
#1644=PLANE('',#28266);
#1645=PLANE('',#28267);
#1646=PLANE('',#28268);
#1647=PLANE('',#28269);
#1648=PLANE('',#28270);
#1649=PLANE('',#28271);
#1650=PLANE('',#28272);
#1651=PLANE('',#28273);
#1652=PLANE('',#28274);
#1653=PLANE('',#28275);
#1654=PLANE('',#28276);
#1655=PLANE('',#28277);
#1656=PLANE('',#28278);
#1657=PLANE('',#28279);
#1658=PLANE('',#28280);
#1659=PLANE('',#28281);
#1660=PLANE('',#28282);
#1661=PLANE('',#28283);
#1662=PLANE('',#28284);
#1663=PLANE('',#28285);
#1664=PLANE('',#28286);
#1665=PLANE('',#28287);
#1666=PLANE('',#28288);
#1667=PLANE('',#28289);
#1668=PLANE('',#28290);
#1669=PLANE('',#28291);
#1670=PLANE('',#28292);
#1671=PLANE('',#28293);
#1672=PLANE('',#28294);
#1673=PLANE('',#28295);
#1674=PLANE('',#28296);
#1675=PLANE('',#28297);
#1676=PLANE('',#28298);
#1677=PLANE('',#28299);
#1678=PLANE('',#28300);
#1679=PLANE('',#28301);
#1680=PLANE('',#28302);
#1681=PLANE('',#28303);
#1682=PLANE('',#28304);
#1683=PLANE('',#28305);
#1684=PLANE('',#28306);
#1685=PLANE('',#28307);
#1686=PLANE('',#28308);
#1687=PLANE('',#28309);
#1688=PLANE('',#28310);
#1689=PLANE('',#28311);
#1690=PLANE('',#28312);
#1691=PLANE('',#28313);
#1692=PLANE('',#28314);
#1693=PLANE('',#28315);
#1694=PLANE('',#28316);
#1695=PLANE('',#28317);
#1696=PLANE('',#28318);
#1697=PLANE('',#28319);
#1698=PLANE('',#28320);
#1699=PLANE('',#28321);
#1700=PLANE('',#28322);
#1701=PLANE('',#28323);
#1702=PLANE('',#28324);
#1703=PLANE('',#28325);
#1704=PLANE('',#28326);
#1705=PLANE('',#28327);
#1706=PLANE('',#28328);
#1707=PLANE('',#28329);
#1708=PLANE('',#28330);
#1709=PLANE('',#28331);
#1710=PLANE('',#28332);
#1711=PLANE('',#28333);
#1712=PLANE('',#28334);
#1713=PLANE('',#28339);
#1714=PLANE('',#28377);
#1715=PLANE('',#28378);
#1716=PLANE('',#28379);
#1717=PLANE('',#28380);
#1718=PLANE('',#28381);
#1719=PLANE('',#28382);
#1720=PLANE('',#28383);
#1721=PLANE('',#28384);
#1722=PLANE('',#28385);
#1723=PLANE('',#28386);
#1724=PLANE('',#28387);
#1725=PLANE('',#28388);
#1726=PLANE('',#28389);
#1727=PLANE('',#28390);
#1728=PLANE('',#28391);
#1729=PLANE('',#28392);
#1730=PLANE('',#28393);
#1731=PLANE('',#28394);
#1732=PLANE('',#28395);
#1733=PLANE('',#28396);
#1734=PLANE('',#28397);
#1735=PLANE('',#28398);
#1736=PLANE('',#28399);
#1737=PLANE('',#28400);
#1738=PLANE('',#28401);
#1739=PLANE('',#28402);
#1740=PLANE('',#28403);
#1741=PLANE('',#28404);
#1742=PLANE('',#28405);
#1743=PLANE('',#28422);
#1744=PLANE('',#28432);
#1745=PLANE('',#28447);
#1746=PLANE('',#28451);
#1747=PLANE('',#28453);
#1748=PLANE('',#28454);
#1749=PLANE('',#28455);
#1750=PLANE('',#28456);
#1751=PLANE('',#28457);
#1752=PLANE('',#28458);
#1753=PLANE('',#28459);
#1754=PLANE('',#28460);
#1755=PLANE('',#28475);
#1756=PLANE('',#28478);
#1757=PLANE('',#28484);
#1758=PLANE('',#28488);
#1759=PLANE('',#28489);
#1760=PLANE('',#28490);
#1761=PLANE('',#28491);
#1762=PLANE('',#28531);
#1763=PLANE('',#28532);
#1764=PLANE('',#28533);
#1765=PLANE('',#28535);
#1766=PLANE('',#28536);
#1767=PLANE('',#28537);
#1768=PLANE('',#28539);
#1769=PLANE('',#28540);
#1770=PLANE('',#28541);
#1771=PLANE('',#28543);
#1772=PLANE('',#28544);
#1773=PLANE('',#28545);
#1774=PLANE('',#28547);
#1775=PLANE('',#28548);
#1776=PLANE('',#28549);
#1777=PLANE('',#28551);
#1778=PLANE('',#28552);
#1779=PLANE('',#28553);
#1780=PLANE('',#28555);
#1781=PLANE('',#28556);
#1782=PLANE('',#28557);
#1783=PLANE('',#28559);
#1784=PLANE('',#28560);
#1785=PLANE('',#28561);
#1786=PLANE('',#28564);
#1787=PLANE('',#28565);
#1788=PLANE('',#28566);
#1789=PLANE('',#28568);
#1790=PLANE('',#28569);
#1791=PLANE('',#28570);
#1792=PLANE('',#28572);
#1793=PLANE('',#28573);
#1794=PLANE('',#28574);
#1795=PLANE('',#28576);
#1796=PLANE('',#28577);
#1797=PLANE('',#28578);
#1798=PLANE('',#28580);
#1799=PLANE('',#28581);
#1800=PLANE('',#28582);
#1801=PLANE('',#28584);
#1802=PLANE('',#28585);
#1803=PLANE('',#28586);
#1804=PLANE('',#28588);
#1805=PLANE('',#28589);
#1806=PLANE('',#28590);
#1807=PLANE('',#28592);
#1808=PLANE('',#28593);
#1809=PLANE('',#28594);
#1810=PLANE('',#28596);
#1811=PLANE('',#28597);
#1812=PLANE('',#28598);
#1813=PLANE('',#28600);
#1814=PLANE('',#28601);
#1815=PLANE('',#28602);
#1816=PLANE('',#28604);
#1817=PLANE('',#28605);
#1818=PLANE('',#28606);
#1819=PLANE('',#28608);
#1820=PLANE('',#28609);
#1821=PLANE('',#28610);
#1822=PLANE('',#28612);
#1823=PLANE('',#28613);
#1824=PLANE('',#28614);
#1825=PLANE('',#28616);
#1826=PLANE('',#28617);
#1827=PLANE('',#28618);
#1828=PLANE('',#28620);
#1829=PLANE('',#28621);
#1830=PLANE('',#28622);
#1831=PLANE('',#28624);
#1832=PLANE('',#28625);
#1833=PLANE('',#28626);
#1834=PLANE('',#28628);
#1835=PLANE('',#28629);
#1836=PLANE('',#28630);
#1837=PLANE('',#28632);
#1838=PLANE('',#28633);
#1839=PLANE('',#28634);
#1840=PLANE('',#28636);
#1841=PLANE('',#28637);
#1842=PLANE('',#28638);
#1843=PLANE('',#28640);
#1844=PLANE('',#28641);
#1845=PLANE('',#28642);
#1846=PLANE('',#28644);
#1847=PLANE('',#28645);
#1848=PLANE('',#28646);
#1849=PLANE('',#28648);
#1850=PLANE('',#28649);
#1851=PLANE('',#28650);
#1852=PLANE('',#28652);
#1853=PLANE('',#28653);
#1854=PLANE('',#28654);
#1855=PLANE('',#28656);
#1856=PLANE('',#28657);
#1857=PLANE('',#28658);
#1858=PLANE('',#28660);
#1859=PLANE('',#28661);
#1860=PLANE('',#28662);
#1861=PLANE('',#28664);
#1862=PLANE('',#28665);
#1863=PLANE('',#28666);
#1864=PLANE('',#28668);
#1865=PLANE('',#28669);
#1866=PLANE('',#28670);
#1867=PLANE('',#28673);
#1868=PLANE('',#28674);
#1869=PLANE('',#28676);
#1870=PLANE('',#28678);
#1871=PLANE('',#28680);
#1872=PLANE('',#28682);
#1873=PLANE('',#28684);
#1874=PLANE('',#28687);
#1875=PLANE('',#28688);
#1876=PLANE('',#28689);
#1877=PLANE('',#28690);
#1878=PLANE('',#28691);
#1879=PLANE('',#28692);
#1880=PLANE('',#28709);
#1881=PLANE('',#28712);
#1882=PLANE('',#28718);
#1883=PLANE('',#28722);
#1884=PLANE('',#28723);
#1885=PLANE('',#28724);
#1886=PLANE('',#28725);
#1887=PLANE('',#28765);
#1888=PLANE('',#28766);
#1889=PLANE('',#28767);
#1890=PLANE('',#28769);
#1891=PLANE('',#28770);
#1892=PLANE('',#28771);
#1893=PLANE('',#28773);
#1894=PLANE('',#28774);
#1895=PLANE('',#28775);
#1896=PLANE('',#28777);
#1897=PLANE('',#28778);
#1898=PLANE('',#28779);
#1899=PLANE('',#28781);
#1900=PLANE('',#28782);
#1901=PLANE('',#28783);
#1902=PLANE('',#28785);
#1903=PLANE('',#28786);
#1904=PLANE('',#28787);
#1905=PLANE('',#28789);
#1906=PLANE('',#28790);
#1907=PLANE('',#28791);
#1908=PLANE('',#28793);
#1909=PLANE('',#28794);
#1910=PLANE('',#28795);
#1911=PLANE('',#28797);
#1912=PLANE('',#28798);
#1913=PLANE('',#28799);
#1914=PLANE('',#28801);
#1915=PLANE('',#28802);
#1916=PLANE('',#28803);
#1917=PLANE('',#28805);
#1918=PLANE('',#28806);
#1919=PLANE('',#28807);
#1920=PLANE('',#28809);
#1921=PLANE('',#28810);
#1922=PLANE('',#28811);
#1923=PLANE('',#28813);
#1924=PLANE('',#28814);
#1925=PLANE('',#28815);
#1926=PLANE('',#28817);
#1927=PLANE('',#28818);
#1928=PLANE('',#28819);
#1929=PLANE('',#28821);
#1930=PLANE('',#28822);
#1931=PLANE('',#28823);
#1932=PLANE('',#28825);
#1933=PLANE('',#28826);
#1934=PLANE('',#28827);
#1935=PLANE('',#28829);
#1936=PLANE('',#28830);
#1937=PLANE('',#28831);
#1938=PLANE('',#28834);
#1939=PLANE('',#28835);
#1940=PLANE('',#28836);
#1941=PLANE('',#28838);
#1942=PLANE('',#28839);
#1943=PLANE('',#28840);
#1944=PLANE('',#28842);
#1945=PLANE('',#28843);
#1946=PLANE('',#28844);
#1947=PLANE('',#28846);
#1948=PLANE('',#28847);
#1949=PLANE('',#28848);
#1950=PLANE('',#28850);
#1951=PLANE('',#28851);
#1952=PLANE('',#28852);
#1953=PLANE('',#28854);
#1954=PLANE('',#28855);
#1955=PLANE('',#28856);
#1956=PLANE('',#28858);
#1957=PLANE('',#28859);
#1958=PLANE('',#28860);
#1959=PLANE('',#28862);
#1960=PLANE('',#28863);
#1961=PLANE('',#28864);
#1962=PLANE('',#28866);
#1963=PLANE('',#28867);
#1964=PLANE('',#28868);
#1965=PLANE('',#28870);
#1966=PLANE('',#28871);
#1967=PLANE('',#28872);
#1968=PLANE('',#28874);
#1969=PLANE('',#28875);
#1970=PLANE('',#28876);
#1971=PLANE('',#28878);
#1972=PLANE('',#28879);
#1973=PLANE('',#28880);
#1974=PLANE('',#28882);
#1975=PLANE('',#28883);
#1976=PLANE('',#28884);
#1977=PLANE('',#28886);
#1978=PLANE('',#28887);
#1979=PLANE('',#28888);
#1980=PLANE('',#28890);
#1981=PLANE('',#28891);
#1982=PLANE('',#28892);
#1983=PLANE('',#28894);
#1984=PLANE('',#28895);
#1985=PLANE('',#28896);
#1986=PLANE('',#28898);
#1987=PLANE('',#28899);
#1988=PLANE('',#28900);
#1989=PLANE('',#28902);
#1990=PLANE('',#28903);
#1991=PLANE('',#28904);
#1992=PLANE('',#28907);
#1993=PLANE('',#28908);
#1994=PLANE('',#28910);
#1995=PLANE('',#28912);
#1996=PLANE('',#28914);
#1997=PLANE('',#28916);
#1998=PLANE('',#28918);
#1999=PLANE('',#28921);
#2000=PLANE('',#28922);
#2001=PLANE('',#28923);
#2002=PLANE('',#28924);
#2003=PLANE('',#28925);
#2004=PLANE('',#28926);
#2005=PLANE('',#28953);
#2006=PLANE('',#28956);
#2007=PLANE('',#28962);
#2008=PLANE('',#28966);
#2009=PLANE('',#28967);
#2010=PLANE('',#28968);
#2011=PLANE('',#28969);
#2012=PLANE('',#29009);
#2013=PLANE('',#29010);
#2014=PLANE('',#29011);
#2015=PLANE('',#29013);
#2016=PLANE('',#29014);
#2017=PLANE('',#29015);
#2018=PLANE('',#29017);
#2019=PLANE('',#29018);
#2020=PLANE('',#29019);
#2021=PLANE('',#29021);
#2022=PLANE('',#29022);
#2023=PLANE('',#29023);
#2024=PLANE('',#29025);
#2025=PLANE('',#29026);
#2026=PLANE('',#29027);
#2027=PLANE('',#29029);
#2028=PLANE('',#29030);
#2029=PLANE('',#29031);
#2030=PLANE('',#29033);
#2031=PLANE('',#29034);
#2032=PLANE('',#29035);
#2033=PLANE('',#29037);
#2034=PLANE('',#29038);
#2035=PLANE('',#29039);
#2036=PLANE('',#29041);
#2037=PLANE('',#29042);
#2038=PLANE('',#29043);
#2039=PLANE('',#29045);
#2040=PLANE('',#29046);
#2041=PLANE('',#29047);
#2042=PLANE('',#29049);
#2043=PLANE('',#29050);
#2044=PLANE('',#29051);
#2045=PLANE('',#29053);
#2046=PLANE('',#29054);
#2047=PLANE('',#29055);
#2048=PLANE('',#29057);
#2049=PLANE('',#29058);
#2050=PLANE('',#29059);
#2051=PLANE('',#29061);
#2052=PLANE('',#29062);
#2053=PLANE('',#29063);
#2054=PLANE('',#29065);
#2055=PLANE('',#29066);
#2056=PLANE('',#29067);
#2057=PLANE('',#29069);
#2058=PLANE('',#29070);
#2059=PLANE('',#29071);
#2060=PLANE('',#29073);
#2061=PLANE('',#29074);
#2062=PLANE('',#29075);
#2063=PLANE('',#29078);
#2064=PLANE('',#29079);
#2065=PLANE('',#29080);
#2066=PLANE('',#29082);
#2067=PLANE('',#29083);
#2068=PLANE('',#29084);
#2069=PLANE('',#29086);
#2070=PLANE('',#29087);
#2071=PLANE('',#29088);
#2072=PLANE('',#29090);
#2073=PLANE('',#29091);
#2074=PLANE('',#29092);
#2075=PLANE('',#29094);
#2076=PLANE('',#29095);
#2077=PLANE('',#29096);
#2078=PLANE('',#29098);
#2079=PLANE('',#29099);
#2080=PLANE('',#29100);
#2081=PLANE('',#29102);
#2082=PLANE('',#29103);
#2083=PLANE('',#29104);
#2084=PLANE('',#29106);
#2085=PLANE('',#29107);
#2086=PLANE('',#29108);
#2087=PLANE('',#29110);
#2088=PLANE('',#29111);
#2089=PLANE('',#29112);
#2090=PLANE('',#29114);
#2091=PLANE('',#29115);
#2092=PLANE('',#29116);
#2093=PLANE('',#29118);
#2094=PLANE('',#29119);
#2095=PLANE('',#29120);
#2096=PLANE('',#29122);
#2097=PLANE('',#29123);
#2098=PLANE('',#29124);
#2099=PLANE('',#29126);
#2100=PLANE('',#29127);
#2101=PLANE('',#29128);
#2102=PLANE('',#29130);
#2103=PLANE('',#29131);
#2104=PLANE('',#29132);
#2105=PLANE('',#29134);
#2106=PLANE('',#29135);
#2107=PLANE('',#29136);
#2108=PLANE('',#29138);
#2109=PLANE('',#29139);
#2110=PLANE('',#29140);
#2111=PLANE('',#29142);
#2112=PLANE('',#29143);
#2113=PLANE('',#29144);
#2114=PLANE('',#29146);
#2115=PLANE('',#29147);
#2116=PLANE('',#29148);
#2117=PLANE('',#29151);
#2118=PLANE('',#29152);
#2119=PLANE('',#29154);
#2120=PLANE('',#29156);
#2121=PLANE('',#29158);
#2122=PLANE('',#29160);
#2123=PLANE('',#29162);
#2124=PLANE('',#29165);
#2125=PLANE('',#29166);
#2126=PLANE('',#29167);
#2127=PLANE('',#29168);
#2128=PLANE('',#29169);
#2129=PLANE('',#29170);
#2130=PLANE('',#29175);
#2131=PLANE('',#29181);
#2132=PLANE('',#29190);
#2133=PLANE('',#29197);
#2134=PLANE('',#29201);
#2135=PLANE('',#29203);
#2136=PLANE('',#29204);
#2137=PLANE('',#29205);
#2138=PLANE('',#29206);
#2139=PLANE('',#29207);
#2140=PLANE('',#29208);
#2141=PLANE('',#29209);
#2142=CYLINDRICAL_SURFACE('',#27103,1.8025);
#2143=CYLINDRICAL_SURFACE('',#27110,1.8025);
#2144=CYLINDRICAL_SURFACE('',#27119,1.8025);
#2145=CYLINDRICAL_SURFACE('',#27126,1.8025);
#2146=CYLINDRICAL_SURFACE('',#27132,1.778);
#2147=CYLINDRICAL_SURFACE('',#27135,1.778);
#2148=CYLINDRICAL_SURFACE('',#27138,1.778);
#2149=CYLINDRICAL_SURFACE('',#27141,1.778);
#2150=CYLINDRICAL_SURFACE('',#27152,1.8025);
#2151=CYLINDRICAL_SURFACE('',#27156,1.8025);
#2152=CYLINDRICAL_SURFACE('',#27160,1.8025);
#2153=CYLINDRICAL_SURFACE('',#27164,1.8025);
#2154=CYLINDRICAL_SURFACE('',#27168,6.363);
#2155=CYLINDRICAL_SURFACE('',#27229,1.778);
#2156=CYLINDRICAL_SURFACE('',#27233,1.778);
#2157=CYLINDRICAL_SURFACE('',#27237,1.778);
#2158=CYLINDRICAL_SURFACE('',#27241,1.778);
#2159=CYLINDRICAL_SURFACE('',#27260,1.8025);
#2160=CYLINDRICAL_SURFACE('',#27263,1.8025);
#2161=CYLINDRICAL_SURFACE('',#27266,1.8025);
#2162=CYLINDRICAL_SURFACE('',#27269,1.8025);
#2163=CYLINDRICAL_SURFACE('',#27306,3.19);
#2164=CYLINDRICAL_SURFACE('',#27308,3.19);
#2165=CYLINDRICAL_SURFACE('',#27333,2.475);
#2166=CYLINDRICAL_SURFACE('',#27336,0.799999999999992);
#2167=CYLINDRICAL_SURFACE('',#27338,0.799999999999994);
#2168=CYLINDRICAL_SURFACE('',#27342,2.475);
#2169=CYLINDRICAL_SURFACE('',#27345,0.799999999999994);
#2170=CYLINDRICAL_SURFACE('',#27347,0.799999999999994);
#2171=CYLINDRICAL_SURFACE('',#27356,3.19);
#2172=CYLINDRICAL_SURFACE('',#27358,3.19);
#2173=CYLINDRICAL_SURFACE('',#27361,2.5);
#2174=CYLINDRICAL_SURFACE('',#27365,2.);
#2175=CYLINDRICAL_SURFACE('',#27368,2.);
#2176=CYLINDRICAL_SURFACE('',#27371,2.);
#2177=CYLINDRICAL_SURFACE('',#27374,2.);
#2178=CYLINDRICAL_SURFACE('',#27380,1.55);
#2179=CYLINDRICAL_SURFACE('',#27385,3.255);
#2180=CYLINDRICAL_SURFACE('',#27389,5.5);
#2181=CYLINDRICAL_SURFACE('',#27396,1.5);
#2182=CYLINDRICAL_SURFACE('',#27399,1.5);
#2183=CYLINDRICAL_SURFACE('',#27403,1.5);
#2184=CYLINDRICAL_SURFACE('',#27406,1.49999999999999);
#2185=CYLINDRICAL_SURFACE('',#27422,0.999999999999992);
#2186=CYLINDRICAL_SURFACE('',#27424,1.);
#2187=CYLINDRICAL_SURFACE('',#27427,0.999999999999999);
#2188=CYLINDRICAL_SURFACE('',#27430,0.999999999999996);
#2189=CYLINDRICAL_SURFACE('',#27438,1.5);
#2190=CYLINDRICAL_SURFACE('',#27442,1.5);
#2191=CYLINDRICAL_SURFACE('',#27446,1.5);
#2192=CYLINDRICAL_SURFACE('',#27449,1.49999999999999);
#2193=CYLINDRICAL_SURFACE('',#27455,7.14399999999837);
#2194=CYLINDRICAL_SURFACE('',#27492,5.358);
#2195=CYLINDRICAL_SURFACE('',#27495,7.14399999999837);
#2196=CYLINDRICAL_SURFACE('',#27498,5.358);
#2197=CYLINDRICAL_SURFACE('',#27501,7.14399999999837);
#2198=CYLINDRICAL_SURFACE('',#27504,5.358);
#2199=CYLINDRICAL_SURFACE('',#27507,7.14399999999837);
#2200=CYLINDRICAL_SURFACE('',#27510,5.358);
#2201=CYLINDRICAL_SURFACE('',#27513,7.14399999999837);
#2202=CYLINDRICAL_SURFACE('',#27516,5.358);
#2203=CYLINDRICAL_SURFACE('',#27519,7.14399999999837);
#2204=CYLINDRICAL_SURFACE('',#27522,5.358);
#2205=CYLINDRICAL_SURFACE('',#27525,7.14399999999837);
#2206=CYLINDRICAL_SURFACE('',#27528,5.358);
#2207=CYLINDRICAL_SURFACE('',#27531,7.14399999999837);
#2208=CYLINDRICAL_SURFACE('',#27534,5.358);
#2209=CYLINDRICAL_SURFACE('',#27537,7.14399999999837);
#2210=CYLINDRICAL_SURFACE('',#27540,5.358);
#2211=CYLINDRICAL_SURFACE('',#27543,7.14399999999837);
#2212=CYLINDRICAL_SURFACE('',#27546,5.358);
#2213=CYLINDRICAL_SURFACE('',#27549,7.14399999999837);
#2214=CYLINDRICAL_SURFACE('',#27552,5.358);
#2215=CYLINDRICAL_SURFACE('',#27555,7.14399999999837);
#2216=CYLINDRICAL_SURFACE('',#27558,5.358);
#2217=CYLINDRICAL_SURFACE('',#27561,7.14399999999837);
#2218=CYLINDRICAL_SURFACE('',#27564,5.358);
#2219=CYLINDRICAL_SURFACE('',#27567,7.14399999999837);
#2220=CYLINDRICAL_SURFACE('',#27570,5.358);
#2221=CYLINDRICAL_SURFACE('',#27574,7.14399999999837);
#2222=CYLINDRICAL_SURFACE('',#27581,5.358);
#2223=CYLINDRICAL_SURFACE('',#27583,7.14399999999837);
#2224=CYLINDRICAL_SURFACE('',#27585,5.358);
#2225=CYLINDRICAL_SURFACE('',#27589,1.6);
#2226=CYLINDRICAL_SURFACE('',#27593,4.477);
#2227=CYLINDRICAL_SURFACE('',#27594,3.261);
#2228=CYLINDRICAL_SURFACE('',#27596,1.17775);
#2229=CYLINDRICAL_SURFACE('',#27598,1.17775);
#2230=CYLINDRICAL_SURFACE('',#27599,1.17775);
#2231=CYLINDRICAL_SURFACE('',#27600,1.17775);
#2232=CYLINDRICAL_SURFACE('',#27601,1.17775);
#2233=CYLINDRICAL_SURFACE('',#27602,1.17775);
#2234=CYLINDRICAL_SURFACE('',#27603,1.17775);
#2235=CYLINDRICAL_SURFACE('',#27604,1.17775);
#2236=CYLINDRICAL_SURFACE('',#27605,1.17775);
#2237=CYLINDRICAL_SURFACE('',#27606,1.17775);
#2238=CYLINDRICAL_SURFACE('',#27607,1.17775);
#2239=CYLINDRICAL_SURFACE('',#27608,1.4635);
#2240=CYLINDRICAL_SURFACE('',#27610,1.4635);
#2241=CYLINDRICAL_SURFACE('',#27611,1.4635);
#2242=CYLINDRICAL_SURFACE('',#27612,1.4635);
#2243=CYLINDRICAL_SURFACE('',#27613,1.4635);
#2244=CYLINDRICAL_SURFACE('',#27614,1.4635);
#2245=CYLINDRICAL_SURFACE('',#27615,1.4635);
#2246=CYLINDRICAL_SURFACE('',#27616,1.4635);
#2247=CYLINDRICAL_SURFACE('',#27617,1.4635);
#2248=CYLINDRICAL_SURFACE('',#27618,1.4635);
#2249=CYLINDRICAL_SURFACE('',#27619,1.4635);
#2250=CYLINDRICAL_SURFACE('',#27620,1.4635);
#2251=CYLINDRICAL_SURFACE('',#27622,1.17775);
#2252=CYLINDRICAL_SURFACE('',#27642,2.75);
#2253=CYLINDRICAL_SURFACE('',#27835,1.39337567297406);
#2254=CYLINDRICAL_SURFACE('',#27837,1.39337567297406);
#2255=CYLINDRICAL_SURFACE('',#27839,1.39337567297406);
#2256=CYLINDRICAL_SURFACE('',#27841,1.39337567297406);
#2257=CYLINDRICAL_SURFACE('',#27843,1.39337567297406);
#2258=CYLINDRICAL_SURFACE('',#27845,1.39337567297406);
#2259=CYLINDRICAL_SURFACE('',#27899,1.778);
#2260=CYLINDRICAL_SURFACE('',#27903,1.778);
#2261=CYLINDRICAL_SURFACE('',#27907,1.778);
#2262=CYLINDRICAL_SURFACE('',#27911,1.778);
#2263=CYLINDRICAL_SURFACE('',#27915,1.778);
#2264=CYLINDRICAL_SURFACE('',#27919,1.778);
#2265=CYLINDRICAL_SURFACE('',#27923,1.778);
#2266=CYLINDRICAL_SURFACE('',#27927,1.778);
#2267=CYLINDRICAL_SURFACE('',#27931,1.778);
#2268=CYLINDRICAL_SURFACE('',#27935,1.778);
#2269=CYLINDRICAL_SURFACE('',#27939,1.778);
#2270=CYLINDRICAL_SURFACE('',#27943,1.778);
#2271=CYLINDRICAL_SURFACE('',#27947,1.778);
#2272=CYLINDRICAL_SURFACE('',#27951,1.778);
#2273=CYLINDRICAL_SURFACE('',#27955,1.778);
#2274=CYLINDRICAL_SURFACE('',#27959,1.778);
#2275=CYLINDRICAL_SURFACE('',#27963,1.778);
#2276=CYLINDRICAL_SURFACE('',#27967,1.778);
#2277=CYLINDRICAL_SURFACE('',#27971,1.778);
#2278=CYLINDRICAL_SURFACE('',#27975,1.778);
#2279=CYLINDRICAL_SURFACE('',#27979,1.778);
#2280=CYLINDRICAL_SURFACE('',#27987,4.7625);
#2281=CYLINDRICAL_SURFACE('',#27997,4.7625);
#2282=CYLINDRICAL_SURFACE('',#28011,4.7625);
#2283=CYLINDRICAL_SURFACE('',#28014,4.7625);
#2284=CYLINDRICAL_SURFACE('',#28024,1.778);
#2285=CYLINDRICAL_SURFACE('',#28027,1.778);
#2286=CYLINDRICAL_SURFACE('',#28030,1.778);
#2287=CYLINDRICAL_SURFACE('',#28033,1.778);
#2288=CYLINDRICAL_SURFACE('',#28036,1.778);
#2289=CYLINDRICAL_SURFACE('',#28039,1.778);
#2290=CYLINDRICAL_SURFACE('',#28042,1.778);
#2291=CYLINDRICAL_SURFACE('',#28045,1.778);
#2292=CYLINDRICAL_SURFACE('',#28048,1.778);
#2293=CYLINDRICAL_SURFACE('',#28051,1.778);
#2294=CYLINDRICAL_SURFACE('',#28347,1.778);
#2295=CYLINDRICAL_SURFACE('',#28351,1.778);
#2296=CYLINDRICAL_SURFACE('',#28355,1.778);
#2297=CYLINDRICAL_SURFACE('',#28359,1.778);
#2298=CYLINDRICAL_SURFACE('',#28363,1.778);
#2299=CYLINDRICAL_SURFACE('',#28367,1.778);
#2300=CYLINDRICAL_SURFACE('',#28371,1.778);
#2301=CYLINDRICAL_SURFACE('',#28375,1.778);
#2302=CYLINDRICAL_SURFACE('',#28407,1.778);
#2303=CYLINDRICAL_SURFACE('',#28410,1.778);
#2304=CYLINDRICAL_SURFACE('',#28416,1.8025);
#2305=CYLINDRICAL_SURFACE('',#28426,1.8025);
#2306=CYLINDRICAL_SURFACE('',#28435,1.8025);
#2307=CYLINDRICAL_SURFACE('',#28441,1.8025);
#2308=CYLINDRICAL_SURFACE('',#28462,1.27);
#2309=CYLINDRICAL_SURFACE('',#28464,1.27);
#2310=CYLINDRICAL_SURFACE('',#28465,1.27);
#2311=CYLINDRICAL_SURFACE('',#28466,1.27);
#2312=CYLINDRICAL_SURFACE('',#28467,1.27);
#2313=CYLINDRICAL_SURFACE('',#28468,1.27);
#2314=CYLINDRICAL_SURFACE('',#28469,1.27);
#2315=CYLINDRICAL_SURFACE('',#28470,1.70434);
#2316=CYLINDRICAL_SURFACE('',#28473,1.27);
#2317=CYLINDRICAL_SURFACE('',#28672,2.8702);
#2318=CYLINDRICAL_SURFACE('',#28694,1.27);
#2319=CYLINDRICAL_SURFACE('',#28696,1.27);
#2320=CYLINDRICAL_SURFACE('',#28697,1.27);
#2321=CYLINDRICAL_SURFACE('',#28698,1.27);
#2322=CYLINDRICAL_SURFACE('',#28699,1.27);
#2323=CYLINDRICAL_SURFACE('',#28700,1.27);
#2324=CYLINDRICAL_SURFACE('',#28701,1.27);
#2325=CYLINDRICAL_SURFACE('',#28702,1.27);
#2326=CYLINDRICAL_SURFACE('',#28703,1.27);
#2327=CYLINDRICAL_SURFACE('',#28704,1.70434);
#2328=CYLINDRICAL_SURFACE('',#28707,1.27);
#2329=CYLINDRICAL_SURFACE('',#28906,2.8702);
#2330=CYLINDRICAL_SURFACE('',#28928,1.26999999999999);
#2331=CYLINDRICAL_SURFACE('',#28930,1.26999999999999);
#2332=CYLINDRICAL_SURFACE('',#28931,1.26999999999999);
#2333=CYLINDRICAL_SURFACE('',#28932,1.26999999999999);
#2334=CYLINDRICAL_SURFACE('',#28933,1.26999999999999);
#2335=CYLINDRICAL_SURFACE('',#28934,1.26999999999999);
#2336=CYLINDRICAL_SURFACE('',#28935,1.26999999999999);
#2337=CYLINDRICAL_SURFACE('',#28936,1.26999999999999);
#2338=CYLINDRICAL_SURFACE('',#28937,1.26999999999999);
#2339=CYLINDRICAL_SURFACE('',#28938,1.26999999999999);
#2340=CYLINDRICAL_SURFACE('',#28939,1.26999999999999);
#2341=CYLINDRICAL_SURFACE('',#28940,1.26999999999999);
#2342=CYLINDRICAL_SURFACE('',#28941,1.26999999999999);
#2343=CYLINDRICAL_SURFACE('',#28942,1.26999999999999);
#2344=CYLINDRICAL_SURFACE('',#28943,1.26999999999999);
#2345=CYLINDRICAL_SURFACE('',#28944,1.26999999999999);
#2346=CYLINDRICAL_SURFACE('',#28945,1.26999999999999);
#2347=CYLINDRICAL_SURFACE('',#28946,1.26999999999999);
#2348=CYLINDRICAL_SURFACE('',#28947,1.26999999999999);
#2349=CYLINDRICAL_SURFACE('',#28948,1.70434);
#2350=CYLINDRICAL_SURFACE('',#28951,1.26999999999999);
#2351=CYLINDRICAL_SURFACE('',#29150,2.8702);
#2352=CYLINDRICAL_SURFACE('',#29177,4.7625);
#2353=CYLINDRICAL_SURFACE('',#29183,1.98119999999999);
#2354=CYLINDRICAL_SURFACE('',#29188,1.80249999999999);
#2355=CYLINDRICAL_SURFACE('',#29192,3.59999999999999);
#2356=CYLINDRICAL_SURFACE('',#29199,1.9);
#2357=FACE_OUTER_BOUND('',#3736,.T.);
#2358=FACE_OUTER_BOUND('',#3737,.T.);
#2359=FACE_OUTER_BOUND('',#3738,.T.);
#2360=FACE_OUTER_BOUND('',#3740,.T.);
#2361=FACE_OUTER_BOUND('',#3741,.T.);
#2362=FACE_OUTER_BOUND('',#3742,.T.);
#2363=FACE_OUTER_BOUND('',#3744,.T.);
#2364=FACE_OUTER_BOUND('',#3745,.T.);
#2365=FACE_OUTER_BOUND('',#3746,.T.);
#2366=FACE_OUTER_BOUND('',#3747,.T.);
#2367=FACE_OUTER_BOUND('',#3748,.T.);
#2368=FACE_OUTER_BOUND('',#3750,.T.);
#2369=FACE_OUTER_BOUND('',#3751,.T.);
#2370=FACE_OUTER_BOUND('',#3752,.T.);
#2371=FACE_OUTER_BOUND('',#3754,.T.);
#2372=FACE_OUTER_BOUND('',#3755,.T.);
#2373=FACE_OUTER_BOUND('',#3756,.T.);
#2374=FACE_OUTER_BOUND('',#3757,.T.);
#2375=FACE_OUTER_BOUND('',#3758,.T.);
#2376=FACE_OUTER_BOUND('',#3759,.T.);
#2377=FACE_OUTER_BOUND('',#3760,.T.);
#2378=FACE_OUTER_BOUND('',#3761,.T.);
#2379=FACE_OUTER_BOUND('',#3771,.T.);
#2380=FACE_OUTER_BOUND('',#3772,.T.);
#2381=FACE_OUTER_BOUND('',#3773,.T.);
#2382=FACE_OUTER_BOUND('',#3774,.T.);
#2383=FACE_OUTER_BOUND('',#3775,.T.);
#2384=FACE_OUTER_BOUND('',#3776,.T.);
#2385=FACE_OUTER_BOUND('',#3777,.T.);
#2386=FACE_OUTER_BOUND('',#3778,.T.);
#2387=FACE_OUTER_BOUND('',#3779,.T.);
#2388=FACE_OUTER_BOUND('',#3780,.T.);
#2389=FACE_OUTER_BOUND('',#3781,.T.);
#2390=FACE_OUTER_BOUND('',#3782,.T.);
#2391=FACE_OUTER_BOUND('',#3783,.T.);
#2392=FACE_OUTER_BOUND('',#3784,.T.);
#2393=FACE_OUTER_BOUND('',#3785,.T.);
#2394=FACE_OUTER_BOUND('',#3786,.T.);
#2395=FACE_OUTER_BOUND('',#3787,.T.);
#2396=FACE_OUTER_BOUND('',#3788,.T.);
#2397=FACE_OUTER_BOUND('',#3789,.T.);
#2398=FACE_OUTER_BOUND('',#3790,.T.);
#2399=FACE_OUTER_BOUND('',#3791,.T.);
#2400=FACE_OUTER_BOUND('',#3792,.T.);
#2401=FACE_OUTER_BOUND('',#3793,.T.);
#2402=FACE_OUTER_BOUND('',#3794,.T.);
#2403=FACE_OUTER_BOUND('',#3795,.T.);
#2404=FACE_OUTER_BOUND('',#3796,.T.);
#2405=FACE_OUTER_BOUND('',#3797,.T.);
#2406=FACE_OUTER_BOUND('',#3798,.T.);
#2407=FACE_OUTER_BOUND('',#3799,.T.);
#2408=FACE_OUTER_BOUND('',#3800,.T.);
#2409=FACE_OUTER_BOUND('',#3801,.T.);
#2410=FACE_OUTER_BOUND('',#3802,.T.);
#2411=FACE_OUTER_BOUND('',#3803,.T.);
#2412=FACE_OUTER_BOUND('',#3804,.T.);
#2413=FACE_OUTER_BOUND('',#3805,.T.);
#2414=FACE_OUTER_BOUND('',#3806,.T.);
#2415=FACE_OUTER_BOUND('',#3807,.T.);
#2416=FACE_OUTER_BOUND('',#3808,.T.);
#2417=FACE_OUTER_BOUND('',#3809,.T.);
#2418=FACE_OUTER_BOUND('',#3810,.T.);
#2419=FACE_OUTER_BOUND('',#3811,.T.);
#2420=FACE_OUTER_BOUND('',#3812,.T.);
#2421=FACE_OUTER_BOUND('',#3813,.T.);
#2422=FACE_OUTER_BOUND('',#3823,.T.);
#2423=FACE_OUTER_BOUND('',#3824,.T.);
#2424=FACE_OUTER_BOUND('',#3825,.T.);
#2425=FACE_OUTER_BOUND('',#3826,.T.);
#2426=FACE_OUTER_BOUND('',#3827,.T.);
#2427=FACE_OUTER_BOUND('',#3837,.T.);
#2428=FACE_OUTER_BOUND('',#3838,.T.);
#2429=FACE_OUTER_BOUND('',#3839,.T.);
#2430=FACE_OUTER_BOUND('',#3840,.T.);
#2431=FACE_OUTER_BOUND('',#3841,.T.);
#2432=FACE_OUTER_BOUND('',#3842,.T.);
#2433=FACE_OUTER_BOUND('',#3843,.T.);
#2434=FACE_OUTER_BOUND('',#3844,.T.);
#2435=FACE_OUTER_BOUND('',#3845,.T.);
#2436=FACE_OUTER_BOUND('',#3855,.T.);
#2437=FACE_OUTER_BOUND('',#3856,.T.);
#2438=FACE_OUTER_BOUND('',#3857,.T.);
#2439=FACE_OUTER_BOUND('',#3858,.T.);
#2440=FACE_OUTER_BOUND('',#3859,.T.);
#2441=FACE_OUTER_BOUND('',#3860,.T.);
#2442=FACE_OUTER_BOUND('',#3861,.T.);
#2443=FACE_OUTER_BOUND('',#3862,.T.);
#2444=FACE_OUTER_BOUND('',#3863,.T.);
#2445=FACE_OUTER_BOUND('',#3864,.T.);
#2446=FACE_OUTER_BOUND('',#3865,.T.);
#2447=FACE_OUTER_BOUND('',#3866,.T.);
#2448=FACE_OUTER_BOUND('',#3867,.T.);
#2449=FACE_OUTER_BOUND('',#3868,.T.);
#2450=FACE_OUTER_BOUND('',#3869,.T.);
#2451=FACE_OUTER_BOUND('',#3870,.T.);
#2452=FACE_OUTER_BOUND('',#3871,.T.);
#2453=FACE_OUTER_BOUND('',#3872,.T.);
#2454=FACE_OUTER_BOUND('',#3873,.T.);
#2455=FACE_OUTER_BOUND('',#3874,.T.);
#2456=FACE_OUTER_BOUND('',#3875,.T.);
#2457=FACE_OUTER_BOUND('',#3876,.T.);
#2458=FACE_OUTER_BOUND('',#3877,.T.);
#2459=FACE_OUTER_BOUND('',#3878,.T.);
#2460=FACE_OUTER_BOUND('',#3879,.T.);
#2461=FACE_OUTER_BOUND('',#3880,.T.);
#2462=FACE_OUTER_BOUND('',#3881,.T.);
#2463=FACE_OUTER_BOUND('',#3882,.T.);
#2464=FACE_OUTER_BOUND('',#3883,.T.);
#2465=FACE_OUTER_BOUND('',#3884,.T.);
#2466=FACE_OUTER_BOUND('',#3885,.T.);
#2467=FACE_OUTER_BOUND('',#3886,.T.);
#2468=FACE_OUTER_BOUND('',#3887,.T.);
#2469=FACE_OUTER_BOUND('',#3888,.T.);
#2470=FACE_OUTER_BOUND('',#3889,.T.);
#2471=FACE_OUTER_BOUND('',#3890,.T.);
#2472=FACE_OUTER_BOUND('',#3891,.T.);
#2473=FACE_OUTER_BOUND('',#3892,.T.);
#2474=FACE_OUTER_BOUND('',#3893,.T.);
#2475=FACE_OUTER_BOUND('',#3894,.T.);
#2476=FACE_OUTER_BOUND('',#3895,.T.);
#2477=FACE_OUTER_BOUND('',#3896,.T.);
#2478=FACE_OUTER_BOUND('',#3897,.T.);
#2479=FACE_OUTER_BOUND('',#3898,.T.);
#2480=FACE_OUTER_BOUND('',#3899,.T.);
#2481=FACE_OUTER_BOUND('',#3900,.T.);
#2482=FACE_OUTER_BOUND('',#3901,.T.);
#2483=FACE_OUTER_BOUND('',#3902,.T.);
#2484=FACE_OUTER_BOUND('',#3903,.T.);
#2485=FACE_OUTER_BOUND('',#3904,.T.);
#2486=FACE_OUTER_BOUND('',#3905,.T.);
#2487=FACE_OUTER_BOUND('',#3906,.T.);
#2488=FACE_OUTER_BOUND('',#3907,.T.);
#2489=FACE_OUTER_BOUND('',#3908,.T.);
#2490=FACE_OUTER_BOUND('',#3909,.T.);
#2491=FACE_OUTER_BOUND('',#3910,.T.);
#2492=FACE_OUTER_BOUND('',#3911,.T.);
#2493=FACE_OUTER_BOUND('',#3912,.T.);
#2494=FACE_OUTER_BOUND('',#3913,.T.);
#2495=FACE_OUTER_BOUND('',#3914,.T.);
#2496=FACE_OUTER_BOUND('',#3915,.T.);
#2497=FACE_OUTER_BOUND('',#3916,.T.);
#2498=FACE_OUTER_BOUND('',#3917,.T.);
#2499=FACE_OUTER_BOUND('',#3918,.T.);
#2500=FACE_OUTER_BOUND('',#3919,.T.);
#2501=FACE_OUTER_BOUND('',#3920,.T.);
#2502=FACE_OUTER_BOUND('',#3921,.T.);
#2503=FACE_OUTER_BOUND('',#3922,.T.);
#2504=FACE_OUTER_BOUND('',#3923,.T.);
#2505=FACE_OUTER_BOUND('',#3924,.T.);
#2506=FACE_OUTER_BOUND('',#3925,.T.);
#2507=FACE_OUTER_BOUND('',#3926,.T.);
#2508=FACE_OUTER_BOUND('',#3927,.T.);
#2509=FACE_OUTER_BOUND('',#3928,.T.);
#2510=FACE_OUTER_BOUND('',#3929,.T.);
#2511=FACE_OUTER_BOUND('',#3930,.T.);
#2512=FACE_OUTER_BOUND('',#3931,.T.);
#2513=FACE_OUTER_BOUND('',#3932,.T.);
#2514=FACE_OUTER_BOUND('',#3933,.T.);
#2515=FACE_OUTER_BOUND('',#3934,.T.);
#2516=FACE_OUTER_BOUND('',#3935,.T.);
#2517=FACE_OUTER_BOUND('',#3936,.T.);
#2518=FACE_OUTER_BOUND('',#3937,.T.);
#2519=FACE_OUTER_BOUND('',#3938,.T.);
#2520=FACE_OUTER_BOUND('',#3939,.T.);
#2521=FACE_OUTER_BOUND('',#3940,.T.);
#2522=FACE_OUTER_BOUND('',#3941,.T.);
#2523=FACE_OUTER_BOUND('',#3942,.T.);
#2524=FACE_OUTER_BOUND('',#3943,.T.);
#2525=FACE_OUTER_BOUND('',#3944,.T.);
#2526=FACE_OUTER_BOUND('',#3945,.T.);
#2527=FACE_OUTER_BOUND('',#3946,.T.);
#2528=FACE_OUTER_BOUND('',#3947,.T.);
#2529=FACE_OUTER_BOUND('',#3948,.T.);
#2530=FACE_OUTER_BOUND('',#3949,.T.);
#2531=FACE_OUTER_BOUND('',#3950,.T.);
#2532=FACE_OUTER_BOUND('',#3952,.T.);
#2533=FACE_OUTER_BOUND('',#3953,.T.);
#2534=FACE_OUTER_BOUND('',#3954,.T.);
#2535=FACE_OUTER_BOUND('',#3955,.T.);
#2536=FACE_OUTER_BOUND('',#3956,.T.);
#2537=FACE_OUTER_BOUND('',#3958,.T.);
#2538=FACE_OUTER_BOUND('',#3959,.T.);
#2539=FACE_OUTER_BOUND('',#3960,.T.);
#2540=FACE_OUTER_BOUND('',#3961,.T.);
#2541=FACE_OUTER_BOUND('',#3962,.T.);
#2542=FACE_OUTER_BOUND('',#3963,.T.);
#2543=FACE_OUTER_BOUND('',#3964,.T.);
#2544=FACE_OUTER_BOUND('',#3965,.T.);
#2545=FACE_OUTER_BOUND('',#3967,.T.);
#2546=FACE_OUTER_BOUND('',#3970,.T.);
#2547=FACE_OUTER_BOUND('',#3973,.T.);
#2548=FACE_OUTER_BOUND('',#3976,.T.);
#2549=FACE_OUTER_BOUND('',#3977,.T.);
#2550=FACE_OUTER_BOUND('',#3978,.T.);
#2551=FACE_OUTER_BOUND('',#3979,.T.);
#2552=FACE_OUTER_BOUND('',#3980,.T.);
#2553=FACE_OUTER_BOUND('',#3981,.T.);
#2554=FACE_OUTER_BOUND('',#3982,.T.);
#2555=FACE_OUTER_BOUND('',#3983,.T.);
#2556=FACE_OUTER_BOUND('',#3984,.T.);
#2557=FACE_OUTER_BOUND('',#3987,.T.);
#2558=FACE_OUTER_BOUND('',#3988,.T.);
#2559=FACE_OUTER_BOUND('',#3989,.T.);
#2560=FACE_OUTER_BOUND('',#3990,.T.);
#2561=FACE_OUTER_BOUND('',#3991,.T.);
#2562=FACE_OUTER_BOUND('',#3992,.T.);
#2563=FACE_OUTER_BOUND('',#3994,.T.);
#2564=FACE_OUTER_BOUND('',#3995,.T.);
#2565=FACE_OUTER_BOUND('',#3996,.T.);
#2566=FACE_OUTER_BOUND('',#3997,.T.);
#2567=FACE_OUTER_BOUND('',#3998,.T.);
#2568=FACE_OUTER_BOUND('',#3999,.T.);
#2569=FACE_OUTER_BOUND('',#4000,.T.);
#2570=FACE_OUTER_BOUND('',#4001,.T.);
#2571=FACE_OUTER_BOUND('',#4002,.T.);
#2572=FACE_OUTER_BOUND('',#4003,.T.);
#2573=FACE_OUTER_BOUND('',#4004,.T.);
#2574=FACE_OUTER_BOUND('',#4006,.T.);
#2575=FACE_OUTER_BOUND('',#4007,.T.);
#2576=FACE_OUTER_BOUND('',#4008,.T.);
#2577=FACE_OUTER_BOUND('',#4009,.T.);
#2578=FACE_OUTER_BOUND('',#4010,.T.);
#2579=FACE_OUTER_BOUND('',#4011,.T.);
#2580=FACE_OUTER_BOUND('',#4012,.T.);
#2581=FACE_OUTER_BOUND('',#4013,.T.);
#2582=FACE_OUTER_BOUND('',#4014,.T.);
#2583=FACE_OUTER_BOUND('',#4015,.T.);
#2584=FACE_OUTER_BOUND('',#4016,.T.);
#2585=FACE_OUTER_BOUND('',#4017,.T.);
#2586=FACE_OUTER_BOUND('',#4018,.T.);
#2587=FACE_OUTER_BOUND('',#4019,.T.);
#2588=FACE_OUTER_BOUND('',#4020,.T.);
#2589=FACE_OUTER_BOUND('',#4021,.T.);
#2590=FACE_OUTER_BOUND('',#4022,.T.);
#2591=FACE_OUTER_BOUND('',#4023,.T.);
#2592=FACE_OUTER_BOUND('',#4024,.T.);
#2593=FACE_OUTER_BOUND('',#4025,.T.);
#2594=FACE_OUTER_BOUND('',#4026,.T.);
#2595=FACE_OUTER_BOUND('',#4027,.T.);
#2596=FACE_OUTER_BOUND('',#4028,.T.);
#2597=FACE_OUTER_BOUND('',#4029,.T.);
#2598=FACE_OUTER_BOUND('',#4030,.T.);
#2599=FACE_OUTER_BOUND('',#4031,.T.);
#2600=FACE_OUTER_BOUND('',#4032,.T.);
#2601=FACE_OUTER_BOUND('',#4033,.T.);
#2602=FACE_OUTER_BOUND('',#4034,.T.);
#2603=FACE_OUTER_BOUND('',#4035,.T.);
#2604=FACE_OUTER_BOUND('',#4036,.T.);
#2605=FACE_OUTER_BOUND('',#4037,.T.);
#2606=FACE_OUTER_BOUND('',#4038,.T.);
#2607=FACE_OUTER_BOUND('',#4039,.T.);
#2608=FACE_OUTER_BOUND('',#4040,.T.);
#2609=FACE_OUTER_BOUND('',#4041,.T.);
#2610=FACE_OUTER_BOUND('',#4042,.T.);
#2611=FACE_OUTER_BOUND('',#4043,.T.);
#2612=FACE_OUTER_BOUND('',#4044,.T.);
#2613=FACE_OUTER_BOUND('',#4045,.T.);
#2614=FACE_OUTER_BOUND('',#4046,.T.);
#2615=FACE_OUTER_BOUND('',#4047,.T.);
#2616=FACE_OUTER_BOUND('',#4048,.T.);
#2617=FACE_OUTER_BOUND('',#4049,.T.);
#2618=FACE_OUTER_BOUND('',#4050,.T.);
#2619=FACE_OUTER_BOUND('',#4051,.T.);
#2620=FACE_OUTER_BOUND('',#4052,.T.);
#2621=FACE_OUTER_BOUND('',#4053,.T.);
#2622=FACE_OUTER_BOUND('',#4054,.T.);
#2623=FACE_OUTER_BOUND('',#4055,.T.);
#2624=FACE_OUTER_BOUND('',#4056,.T.);
#2625=FACE_OUTER_BOUND('',#4057,.T.);
#2626=FACE_OUTER_BOUND('',#4058,.T.);
#2627=FACE_OUTER_BOUND('',#4059,.T.);
#2628=FACE_OUTER_BOUND('',#4060,.T.);
#2629=FACE_OUTER_BOUND('',#4061,.T.);
#2630=FACE_OUTER_BOUND('',#4062,.T.);
#2631=FACE_OUTER_BOUND('',#4063,.T.);
#2632=FACE_OUTER_BOUND('',#4064,.T.);
#2633=FACE_OUTER_BOUND('',#4065,.T.);
#2634=FACE_OUTER_BOUND('',#4066,.T.);
#2635=FACE_OUTER_BOUND('',#4067,.T.);
#2636=FACE_OUTER_BOUND('',#4068,.T.);
#2637=FACE_OUTER_BOUND('',#4069,.T.);
#2638=FACE_OUTER_BOUND('',#4070,.T.);
#2639=FACE_OUTER_BOUND('',#4071,.T.);
#2640=FACE_OUTER_BOUND('',#4072,.T.);
#2641=FACE_OUTER_BOUND('',#4073,.T.);
#2642=FACE_OUTER_BOUND('',#4074,.T.);
#2643=FACE_OUTER_BOUND('',#4075,.T.);
#2644=FACE_OUTER_BOUND('',#4076,.T.);
#2645=FACE_OUTER_BOUND('',#4077,.T.);
#2646=FACE_OUTER_BOUND('',#4078,.T.);
#2647=FACE_OUTER_BOUND('',#4079,.T.);
#2648=FACE_OUTER_BOUND('',#4080,.T.);
#2649=FACE_OUTER_BOUND('',#4081,.T.);
#2650=FACE_OUTER_BOUND('',#4082,.T.);
#2651=FACE_OUTER_BOUND('',#4083,.T.);
#2652=FACE_OUTER_BOUND('',#4084,.T.);
#2653=FACE_OUTER_BOUND('',#4085,.T.);
#2654=FACE_OUTER_BOUND('',#4086,.T.);
#2655=FACE_OUTER_BOUND('',#4087,.T.);
#2656=FACE_OUTER_BOUND('',#4088,.T.);
#2657=FACE_OUTER_BOUND('',#4089,.T.);
#2658=FACE_OUTER_BOUND('',#4090,.T.);
#2659=FACE_OUTER_BOUND('',#4092,.T.);
#2660=FACE_OUTER_BOUND('',#4093,.T.);
#2661=FACE_OUTER_BOUND('',#4094,.T.);
#2662=FACE_OUTER_BOUND('',#4095,.T.);
#2663=FACE_OUTER_BOUND('',#4096,.T.);
#2664=FACE_OUTER_BOUND('',#4097,.T.);
#2665=FACE_OUTER_BOUND('',#4098,.T.);
#2666=FACE_OUTER_BOUND('',#4099,.T.);
#2667=FACE_OUTER_BOUND('',#4101,.T.);
#2668=FACE_OUTER_BOUND('',#4102,.T.);
#2669=FACE_OUTER_BOUND('',#4104,.T.);
#2670=FACE_OUTER_BOUND('',#4105,.T.);
#2671=FACE_OUTER_BOUND('',#4106,.T.);
#2672=FACE_OUTER_BOUND('',#4107,.T.);
#2673=FACE_OUTER_BOUND('',#4108,.T.);
#2674=FACE_OUTER_BOUND('',#4109,.T.);
#2675=FACE_OUTER_BOUND('',#4110,.T.);
#2676=FACE_OUTER_BOUND('',#4111,.T.);
#2677=FACE_OUTER_BOUND('',#4112,.T.);
#2678=FACE_OUTER_BOUND('',#4113,.T.);
#2679=FACE_OUTER_BOUND('',#4114,.T.);
#2680=FACE_OUTER_BOUND('',#4115,.T.);
#2681=FACE_OUTER_BOUND('',#4116,.T.);
#2682=FACE_OUTER_BOUND('',#4117,.T.);
#2683=FACE_OUTER_BOUND('',#4118,.T.);
#2684=FACE_OUTER_BOUND('',#4119,.T.);
#2685=FACE_OUTER_BOUND('',#4120,.T.);
#2686=FACE_OUTER_BOUND('',#4121,.T.);
#2687=FACE_OUTER_BOUND('',#4122,.T.);
#2688=FACE_OUTER_BOUND('',#4123,.T.);
#2689=FACE_OUTER_BOUND('',#4124,.T.);
#2690=FACE_OUTER_BOUND('',#4125,.T.);
#2691=FACE_OUTER_BOUND('',#4126,.T.);
#2692=FACE_OUTER_BOUND('',#4127,.T.);
#2693=FACE_OUTER_BOUND('',#4128,.T.);
#2694=FACE_OUTER_BOUND('',#4129,.T.);
#2695=FACE_OUTER_BOUND('',#4130,.T.);
#2696=FACE_OUTER_BOUND('',#4131,.T.);
#2697=FACE_OUTER_BOUND('',#4132,.T.);
#2698=FACE_OUTER_BOUND('',#4133,.T.);
#2699=FACE_OUTER_BOUND('',#4134,.T.);
#2700=FACE_OUTER_BOUND('',#4135,.T.);
#2701=FACE_OUTER_BOUND('',#4137,.T.);
#2702=FACE_OUTER_BOUND('',#4138,.T.);
#2703=FACE_OUTER_BOUND('',#4139,.T.);
#2704=FACE_OUTER_BOUND('',#4140,.T.);
#2705=FACE_OUTER_BOUND('',#4141,.T.);
#2706=FACE_OUTER_BOUND('',#4142,.T.);
#2707=FACE_OUTER_BOUND('',#4143,.T.);
#2708=FACE_OUTER_BOUND('',#4144,.T.);
#2709=FACE_OUTER_BOUND('',#4145,.T.);
#2710=FACE_OUTER_BOUND('',#4146,.T.);
#2711=FACE_OUTER_BOUND('',#4147,.T.);
#2712=FACE_OUTER_BOUND('',#4148,.T.);
#2713=FACE_OUTER_BOUND('',#4149,.T.);
#2714=FACE_OUTER_BOUND('',#4150,.T.);
#2715=FACE_OUTER_BOUND('',#4151,.T.);
#2716=FACE_OUTER_BOUND('',#4152,.T.);
#2717=FACE_OUTER_BOUND('',#4153,.T.);
#2718=FACE_OUTER_BOUND('',#4154,.T.);
#2719=FACE_OUTER_BOUND('',#4155,.T.);
#2720=FACE_OUTER_BOUND('',#4156,.T.);
#2721=FACE_OUTER_BOUND('',#4157,.T.);
#2722=FACE_OUTER_BOUND('',#4158,.T.);
#2723=FACE_OUTER_BOUND('',#4159,.T.);
#2724=FACE_OUTER_BOUND('',#4160,.T.);
#2725=FACE_OUTER_BOUND('',#4161,.T.);
#2726=FACE_OUTER_BOUND('',#4162,.T.);
#2727=FACE_OUTER_BOUND('',#4163,.T.);
#2728=FACE_OUTER_BOUND('',#4164,.T.);
#2729=FACE_OUTER_BOUND('',#4165,.T.);
#2730=FACE_OUTER_BOUND('',#4166,.T.);
#2731=FACE_OUTER_BOUND('',#4167,.T.);
#2732=FACE_OUTER_BOUND('',#4168,.T.);
#2733=FACE_OUTER_BOUND('',#4169,.T.);
#2734=FACE_OUTER_BOUND('',#4170,.T.);
#2735=FACE_OUTER_BOUND('',#4171,.T.);
#2736=FACE_OUTER_BOUND('',#4172,.T.);
#2737=FACE_OUTER_BOUND('',#4173,.T.);
#2738=FACE_OUTER_BOUND('',#4174,.T.);
#2739=FACE_OUTER_BOUND('',#4175,.T.);
#2740=FACE_OUTER_BOUND('',#4176,.T.);
#2741=FACE_OUTER_BOUND('',#4177,.T.);
#2742=FACE_OUTER_BOUND('',#4178,.T.);
#2743=FACE_OUTER_BOUND('',#4179,.T.);
#2744=FACE_OUTER_BOUND('',#4180,.T.);
#2745=FACE_OUTER_BOUND('',#4181,.T.);
#2746=FACE_OUTER_BOUND('',#4182,.T.);
#2747=FACE_OUTER_BOUND('',#4183,.T.);
#2748=FACE_OUTER_BOUND('',#4184,.T.);
#2749=FACE_OUTER_BOUND('',#4185,.T.);
#2750=FACE_OUTER_BOUND('',#4186,.T.);
#2751=FACE_OUTER_BOUND('',#4187,.T.);
#2752=FACE_OUTER_BOUND('',#4188,.T.);
#2753=FACE_OUTER_BOUND('',#4189,.T.);
#2754=FACE_OUTER_BOUND('',#4190,.T.);
#2755=FACE_OUTER_BOUND('',#4191,.T.);
#2756=FACE_OUTER_BOUND('',#4192,.T.);
#2757=FACE_OUTER_BOUND('',#4193,.T.);
#2758=FACE_OUTER_BOUND('',#4194,.T.);
#2759=FACE_OUTER_BOUND('',#4195,.T.);
#2760=FACE_OUTER_BOUND('',#4196,.T.);
#2761=FACE_OUTER_BOUND('',#4197,.T.);
#2762=FACE_OUTER_BOUND('',#4198,.T.);
#2763=FACE_OUTER_BOUND('',#4199,.T.);
#2764=FACE_OUTER_BOUND('',#4200,.T.);
#2765=FACE_OUTER_BOUND('',#4201,.T.);
#2766=FACE_OUTER_BOUND('',#4202,.T.);
#2767=FACE_OUTER_BOUND('',#4203,.T.);
#2768=FACE_OUTER_BOUND('',#4204,.T.);
#2769=FACE_OUTER_BOUND('',#4205,.T.);
#2770=FACE_OUTER_BOUND('',#4206,.T.);
#2771=FACE_OUTER_BOUND('',#4207,.T.);
#2772=FACE_OUTER_BOUND('',#4208,.T.);
#2773=FACE_OUTER_BOUND('',#4209,.T.);
#2774=FACE_OUTER_BOUND('',#4210,.T.);
#2775=FACE_OUTER_BOUND('',#4211,.T.);
#2776=FACE_OUTER_BOUND('',#4212,.T.);
#2777=FACE_OUTER_BOUND('',#4213,.T.);
#2778=FACE_OUTER_BOUND('',#4214,.T.);
#2779=FACE_OUTER_BOUND('',#4215,.T.);
#2780=FACE_OUTER_BOUND('',#4216,.T.);
#2781=FACE_OUTER_BOUND('',#4217,.T.);
#2782=FACE_OUTER_BOUND('',#4218,.T.);
#2783=FACE_OUTER_BOUND('',#4219,.T.);
#2784=FACE_OUTER_BOUND('',#4220,.T.);
#2785=FACE_OUTER_BOUND('',#4221,.T.);
#2786=FACE_OUTER_BOUND('',#4222,.T.);
#2787=FACE_OUTER_BOUND('',#4223,.T.);
#2788=FACE_OUTER_BOUND('',#4224,.T.);
#2789=FACE_OUTER_BOUND('',#4225,.T.);
#2790=FACE_OUTER_BOUND('',#4226,.T.);
#2791=FACE_OUTER_BOUND('',#4227,.T.);
#2792=FACE_OUTER_BOUND('',#4228,.T.);
#2793=FACE_OUTER_BOUND('',#4229,.T.);
#2794=FACE_OUTER_BOUND('',#4230,.T.);
#2795=FACE_OUTER_BOUND('',#4231,.T.);
#2796=FACE_OUTER_BOUND('',#4232,.T.);
#2797=FACE_OUTER_BOUND('',#4233,.T.);
#2798=FACE_OUTER_BOUND('',#4234,.T.);
#2799=FACE_OUTER_BOUND('',#4235,.T.);
#2800=FACE_OUTER_BOUND('',#4236,.T.);
#2801=FACE_OUTER_BOUND('',#4237,.T.);
#2802=FACE_OUTER_BOUND('',#4238,.T.);
#2803=FACE_OUTER_BOUND('',#4239,.T.);
#2804=FACE_OUTER_BOUND('',#4240,.T.);
#2805=FACE_OUTER_BOUND('',#4241,.T.);
#2806=FACE_OUTER_BOUND('',#4242,.T.);
#2807=FACE_OUTER_BOUND('',#4243,.T.);
#2808=FACE_OUTER_BOUND('',#4244,.T.);
#2809=FACE_OUTER_BOUND('',#4245,.T.);
#2810=FACE_OUTER_BOUND('',#4246,.T.);
#2811=FACE_OUTER_BOUND('',#4247,.T.);
#2812=FACE_OUTER_BOUND('',#4248,.T.);
#2813=FACE_OUTER_BOUND('',#4249,.T.);
#2814=FACE_OUTER_BOUND('',#4250,.T.);
#2815=FACE_OUTER_BOUND('',#4252,.T.);
#2816=FACE_OUTER_BOUND('',#4253,.T.);
#2817=FACE_OUTER_BOUND('',#4254,.T.);
#2818=FACE_OUTER_BOUND('',#4255,.T.);
#2819=FACE_OUTER_BOUND('',#4256,.T.);
#2820=FACE_OUTER_BOUND('',#4257,.T.);
#2821=FACE_OUTER_BOUND('',#4258,.T.);
#2822=FACE_OUTER_BOUND('',#4259,.T.);
#2823=FACE_OUTER_BOUND('',#4260,.T.);
#2824=FACE_OUTER_BOUND('',#4261,.T.);
#2825=FACE_OUTER_BOUND('',#4262,.T.);
#2826=FACE_OUTER_BOUND('',#4263,.T.);
#2827=FACE_OUTER_BOUND('',#4264,.T.);
#2828=FACE_OUTER_BOUND('',#4265,.T.);
#2829=FACE_OUTER_BOUND('',#4266,.T.);
#2830=FACE_OUTER_BOUND('',#4267,.T.);
#2831=FACE_OUTER_BOUND('',#4268,.T.);
#2832=FACE_OUTER_BOUND('',#4269,.T.);
#2833=FACE_OUTER_BOUND('',#4270,.T.);
#2834=FACE_OUTER_BOUND('',#4271,.T.);
#2835=FACE_OUTER_BOUND('',#4272,.T.);
#2836=FACE_OUTER_BOUND('',#4273,.T.);
#2837=FACE_OUTER_BOUND('',#4274,.T.);
#2838=FACE_OUTER_BOUND('',#4275,.T.);
#2839=FACE_OUTER_BOUND('',#4276,.T.);
#2840=FACE_OUTER_BOUND('',#4277,.T.);
#2841=FACE_OUTER_BOUND('',#4278,.T.);
#2842=FACE_OUTER_BOUND('',#4279,.T.);
#2843=FACE_OUTER_BOUND('',#4301,.T.);
#2844=FACE_OUTER_BOUND('',#4302,.T.);
#2845=FACE_OUTER_BOUND('',#4303,.T.);
#2846=FACE_OUTER_BOUND('',#4304,.T.);
#2847=FACE_OUTER_BOUND('',#4305,.T.);
#2848=FACE_OUTER_BOUND('',#4306,.T.);
#2849=FACE_OUTER_BOUND('',#4307,.T.);
#2850=FACE_OUTER_BOUND('',#4308,.T.);
#2851=FACE_OUTER_BOUND('',#4309,.T.);
#2852=FACE_OUTER_BOUND('',#4310,.T.);
#2853=FACE_OUTER_BOUND('',#4311,.T.);
#2854=FACE_OUTER_BOUND('',#4312,.T.);
#2855=FACE_OUTER_BOUND('',#4313,.T.);
#2856=FACE_OUTER_BOUND('',#4314,.T.);
#2857=FACE_OUTER_BOUND('',#4315,.T.);
#2858=FACE_OUTER_BOUND('',#4316,.T.);
#2859=FACE_OUTER_BOUND('',#4317,.T.);
#2860=FACE_OUTER_BOUND('',#4318,.T.);
#2861=FACE_OUTER_BOUND('',#4319,.T.);
#2862=FACE_OUTER_BOUND('',#4320,.T.);
#2863=FACE_OUTER_BOUND('',#4321,.T.);
#2864=FACE_OUTER_BOUND('',#4322,.T.);
#2865=FACE_OUTER_BOUND('',#4323,.T.);
#2866=FACE_OUTER_BOUND('',#4324,.T.);
#2867=FACE_OUTER_BOUND('',#4325,.T.);
#2868=FACE_OUTER_BOUND('',#4326,.T.);
#2869=FACE_OUTER_BOUND('',#4327,.T.);
#2870=FACE_OUTER_BOUND('',#4328,.T.);
#2871=FACE_OUTER_BOUND('',#4329,.T.);
#2872=FACE_OUTER_BOUND('',#4330,.T.);
#2873=FACE_OUTER_BOUND('',#4331,.T.);
#2874=FACE_OUTER_BOUND('',#4332,.T.);
#2875=FACE_OUTER_BOUND('',#4333,.T.);
#2876=FACE_OUTER_BOUND('',#4334,.T.);
#2877=FACE_OUTER_BOUND('',#4335,.T.);
#2878=FACE_OUTER_BOUND('',#4336,.T.);
#2879=FACE_OUTER_BOUND('',#4337,.T.);
#2880=FACE_OUTER_BOUND('',#4338,.T.);
#2881=FACE_OUTER_BOUND('',#4339,.T.);
#2882=FACE_OUTER_BOUND('',#4340,.T.);
#2883=FACE_OUTER_BOUND('',#4341,.T.);
#2884=FACE_OUTER_BOUND('',#4342,.T.);
#2885=FACE_OUTER_BOUND('',#4343,.T.);
#2886=FACE_OUTER_BOUND('',#4344,.T.);
#2887=FACE_OUTER_BOUND('',#4345,.T.);
#2888=FACE_OUTER_BOUND('',#4346,.T.);
#2889=FACE_OUTER_BOUND('',#4347,.T.);
#2890=FACE_OUTER_BOUND('',#4348,.T.);
#2891=FACE_OUTER_BOUND('',#4349,.T.);
#2892=FACE_OUTER_BOUND('',#4350,.T.);
#2893=FACE_OUTER_BOUND('',#4351,.T.);
#2894=FACE_OUTER_BOUND('',#4352,.T.);
#2895=FACE_OUTER_BOUND('',#4353,.T.);
#2896=FACE_OUTER_BOUND('',#4375,.T.);
#2897=FACE_OUTER_BOUND('',#4376,.T.);
#2898=FACE_OUTER_BOUND('',#4377,.T.);
#2899=FACE_OUTER_BOUND('',#4378,.T.);
#2900=FACE_OUTER_BOUND('',#4379,.T.);
#2901=FACE_OUTER_BOUND('',#4380,.T.);
#2902=FACE_OUTER_BOUND('',#4381,.T.);
#2903=FACE_OUTER_BOUND('',#4382,.T.);
#2904=FACE_OUTER_BOUND('',#4383,.T.);
#2905=FACE_OUTER_BOUND('',#4384,.T.);
#2906=FACE_OUTER_BOUND('',#4385,.T.);
#2907=FACE_OUTER_BOUND('',#4386,.T.);
#2908=FACE_OUTER_BOUND('',#4387,.T.);
#2909=FACE_OUTER_BOUND('',#4388,.T.);
#2910=FACE_OUTER_BOUND('',#4389,.T.);
#2911=FACE_OUTER_BOUND('',#4390,.T.);
#2912=FACE_OUTER_BOUND('',#4391,.T.);
#2913=FACE_OUTER_BOUND('',#4392,.T.);
#2914=FACE_OUTER_BOUND('',#4393,.T.);
#2915=FACE_OUTER_BOUND('',#4394,.T.);
#2916=FACE_OUTER_BOUND('',#4395,.T.);
#2917=FACE_OUTER_BOUND('',#4396,.T.);
#2918=FACE_OUTER_BOUND('',#4397,.T.);
#2919=FACE_OUTER_BOUND('',#4398,.T.);
#2920=FACE_OUTER_BOUND('',#4399,.T.);
#2921=FACE_OUTER_BOUND('',#4400,.T.);
#2922=FACE_OUTER_BOUND('',#4401,.T.);
#2923=FACE_OUTER_BOUND('',#4402,.T.);
#2924=FACE_OUTER_BOUND('',#4403,.T.);
#2925=FACE_OUTER_BOUND('',#4404,.T.);
#2926=FACE_OUTER_BOUND('',#4405,.T.);
#2927=FACE_OUTER_BOUND('',#4406,.T.);
#2928=FACE_OUTER_BOUND('',#4407,.T.);
#2929=FACE_OUTER_BOUND('',#4408,.T.);
#2930=FACE_OUTER_BOUND('',#4409,.T.);
#2931=FACE_OUTER_BOUND('',#4410,.T.);
#2932=FACE_OUTER_BOUND('',#4411,.T.);
#2933=FACE_OUTER_BOUND('',#4412,.T.);
#2934=FACE_OUTER_BOUND('',#4413,.T.);
#2935=FACE_OUTER_BOUND('',#4414,.T.);
#2936=FACE_OUTER_BOUND('',#4415,.T.);
#2937=FACE_OUTER_BOUND('',#4416,.T.);
#2938=FACE_OUTER_BOUND('',#4417,.T.);
#2939=FACE_OUTER_BOUND('',#4418,.T.);
#2940=FACE_OUTER_BOUND('',#4419,.T.);
#2941=FACE_OUTER_BOUND('',#4420,.T.);
#2942=FACE_OUTER_BOUND('',#4421,.T.);
#2943=FACE_OUTER_BOUND('',#4422,.T.);
#2944=FACE_OUTER_BOUND('',#4423,.T.);
#2945=FACE_OUTER_BOUND('',#4424,.T.);
#2946=FACE_OUTER_BOUND('',#4425,.T.);
#2947=FACE_OUTER_BOUND('',#4426,.T.);
#2948=FACE_OUTER_BOUND('',#4427,.T.);
#2949=FACE_OUTER_BOUND('',#4428,.T.);
#2950=FACE_OUTER_BOUND('',#4429,.T.);
#2951=FACE_OUTER_BOUND('',#4430,.T.);
#2952=FACE_OUTER_BOUND('',#4431,.T.);
#2953=FACE_OUTER_BOUND('',#4432,.T.);
#2954=FACE_OUTER_BOUND('',#4433,.T.);
#2955=FACE_OUTER_BOUND('',#4434,.T.);
#2956=FACE_OUTER_BOUND('',#4435,.T.);
#2957=FACE_OUTER_BOUND('',#4436,.T.);
#2958=FACE_OUTER_BOUND('',#4437,.T.);
#2959=FACE_OUTER_BOUND('',#4438,.T.);
#2960=FACE_OUTER_BOUND('',#4439,.T.);
#2961=FACE_OUTER_BOUND('',#4440,.T.);
#2962=FACE_OUTER_BOUND('',#4441,.T.);
#2963=FACE_OUTER_BOUND('',#4442,.T.);
#2964=FACE_OUTER_BOUND('',#4443,.T.);
#2965=FACE_OUTER_BOUND('',#4444,.T.);
#2966=FACE_OUTER_BOUND('',#4445,.T.);
#2967=FACE_OUTER_BOUND('',#4446,.T.);
#2968=FACE_OUTER_BOUND('',#4447,.T.);
#2969=FACE_OUTER_BOUND('',#4448,.T.);
#2970=FACE_OUTER_BOUND('',#4449,.T.);
#2971=FACE_OUTER_BOUND('',#4450,.T.);
#2972=FACE_OUTER_BOUND('',#4451,.T.);
#2973=FACE_OUTER_BOUND('',#4452,.T.);
#2974=FACE_OUTER_BOUND('',#4453,.T.);
#2975=FACE_OUTER_BOUND('',#4454,.T.);
#2976=FACE_OUTER_BOUND('',#4455,.T.);
#2977=FACE_OUTER_BOUND('',#4456,.T.);
#2978=FACE_OUTER_BOUND('',#4457,.T.);
#2979=FACE_OUTER_BOUND('',#4458,.T.);
#2980=FACE_OUTER_BOUND('',#4459,.T.);
#2981=FACE_OUTER_BOUND('',#4460,.T.);
#2982=FACE_OUTER_BOUND('',#4461,.T.);
#2983=FACE_OUTER_BOUND('',#4462,.T.);
#2984=FACE_OUTER_BOUND('',#4463,.T.);
#2985=FACE_OUTER_BOUND('',#4464,.T.);
#2986=FACE_OUTER_BOUND('',#4465,.T.);
#2987=FACE_OUTER_BOUND('',#4466,.T.);
#2988=FACE_OUTER_BOUND('',#4467,.T.);
#2989=FACE_OUTER_BOUND('',#4468,.T.);
#2990=FACE_OUTER_BOUND('',#4469,.T.);
#2991=FACE_OUTER_BOUND('',#4470,.T.);
#2992=FACE_OUTER_BOUND('',#4471,.T.);
#2993=FACE_OUTER_BOUND('',#4472,.T.);
#2994=FACE_OUTER_BOUND('',#4473,.T.);
#2995=FACE_OUTER_BOUND('',#4474,.T.);
#2996=FACE_OUTER_BOUND('',#4475,.T.);
#2997=FACE_OUTER_BOUND('',#4476,.T.);
#2998=FACE_OUTER_BOUND('',#4477,.T.);
#2999=FACE_OUTER_BOUND('',#4478,.T.);
#3000=FACE_OUTER_BOUND('',#4479,.T.);
#3001=FACE_OUTER_BOUND('',#4480,.T.);
#3002=FACE_OUTER_BOUND('',#4481,.T.);
#3003=FACE_OUTER_BOUND('',#4482,.T.);
#3004=FACE_OUTER_BOUND('',#4483,.T.);
#3005=FACE_OUTER_BOUND('',#4484,.T.);
#3006=FACE_OUTER_BOUND('',#4485,.T.);
#3007=FACE_OUTER_BOUND('',#4486,.T.);
#3008=FACE_OUTER_BOUND('',#4487,.T.);
#3009=FACE_OUTER_BOUND('',#4488,.T.);
#3010=FACE_OUTER_BOUND('',#4489,.T.);
#3011=FACE_OUTER_BOUND('',#4490,.T.);
#3012=FACE_OUTER_BOUND('',#4491,.T.);
#3013=FACE_OUTER_BOUND('',#4492,.T.);
#3014=FACE_OUTER_BOUND('',#4493,.T.);
#3015=FACE_OUTER_BOUND('',#4494,.T.);
#3016=FACE_OUTER_BOUND('',#4495,.T.);
#3017=FACE_OUTER_BOUND('',#4496,.T.);
#3018=FACE_OUTER_BOUND('',#4497,.T.);
#3019=FACE_OUTER_BOUND('',#4498,.T.);
#3020=FACE_OUTER_BOUND('',#4499,.T.);
#3021=FACE_OUTER_BOUND('',#4500,.T.);
#3022=FACE_OUTER_BOUND('',#4501,.T.);
#3023=FACE_OUTER_BOUND('',#4502,.T.);
#3024=FACE_OUTER_BOUND('',#4503,.T.);
#3025=FACE_OUTER_BOUND('',#4504,.T.);
#3026=FACE_OUTER_BOUND('',#4505,.T.);
#3027=FACE_OUTER_BOUND('',#4506,.T.);
#3028=FACE_OUTER_BOUND('',#4507,.T.);
#3029=FACE_OUTER_BOUND('',#4508,.T.);
#3030=FACE_OUTER_BOUND('',#4509,.T.);
#3031=FACE_OUTER_BOUND('',#4510,.T.);
#3032=FACE_OUTER_BOUND('',#4511,.T.);
#3033=FACE_OUTER_BOUND('',#4512,.T.);
#3034=FACE_OUTER_BOUND('',#4513,.T.);
#3035=FACE_OUTER_BOUND('',#4514,.T.);
#3036=FACE_OUTER_BOUND('',#4515,.T.);
#3037=FACE_OUTER_BOUND('',#4516,.T.);
#3038=FACE_OUTER_BOUND('',#4517,.T.);
#3039=FACE_OUTER_BOUND('',#4518,.T.);
#3040=FACE_OUTER_BOUND('',#4519,.T.);
#3041=FACE_OUTER_BOUND('',#4520,.T.);
#3042=FACE_OUTER_BOUND('',#4521,.T.);
#3043=FACE_OUTER_BOUND('',#4522,.T.);
#3044=FACE_OUTER_BOUND('',#4523,.T.);
#3045=FACE_OUTER_BOUND('',#4524,.T.);
#3046=FACE_OUTER_BOUND('',#4525,.T.);
#3047=FACE_OUTER_BOUND('',#4526,.T.);
#3048=FACE_OUTER_BOUND('',#4527,.T.);
#3049=FACE_OUTER_BOUND('',#4528,.T.);
#3050=FACE_OUTER_BOUND('',#4529,.T.);
#3051=FACE_OUTER_BOUND('',#4530,.T.);
#3052=FACE_OUTER_BOUND('',#4531,.T.);
#3053=FACE_OUTER_BOUND('',#4532,.T.);
#3054=FACE_OUTER_BOUND('',#4533,.T.);
#3055=FACE_OUTER_BOUND('',#4534,.T.);
#3056=FACE_OUTER_BOUND('',#4535,.T.);
#3057=FACE_OUTER_BOUND('',#4536,.T.);
#3058=FACE_OUTER_BOUND('',#4537,.T.);
#3059=FACE_OUTER_BOUND('',#4538,.T.);
#3060=FACE_OUTER_BOUND('',#4539,.T.);
#3061=FACE_OUTER_BOUND('',#4540,.T.);
#3062=FACE_OUTER_BOUND('',#4541,.T.);
#3063=FACE_OUTER_BOUND('',#4542,.T.);
#3064=FACE_OUTER_BOUND('',#4543,.T.);
#3065=FACE_OUTER_BOUND('',#4544,.T.);
#3066=FACE_OUTER_BOUND('',#4545,.T.);
#3067=FACE_OUTER_BOUND('',#4546,.T.);
#3068=FACE_OUTER_BOUND('',#4547,.T.);
#3069=FACE_OUTER_BOUND('',#4548,.T.);
#3070=FACE_OUTER_BOUND('',#4549,.T.);
#3071=FACE_OUTER_BOUND('',#4550,.T.);
#3072=FACE_OUTER_BOUND('',#4551,.T.);
#3073=FACE_OUTER_BOUND('',#4552,.T.);
#3074=FACE_OUTER_BOUND('',#4553,.T.);
#3075=FACE_OUTER_BOUND('',#4554,.T.);
#3076=FACE_OUTER_BOUND('',#4555,.T.);
#3077=FACE_OUTER_BOUND('',#4556,.T.);
#3078=FACE_OUTER_BOUND('',#4557,.T.);
#3079=FACE_OUTER_BOUND('',#4558,.T.);
#3080=FACE_OUTER_BOUND('',#4559,.T.);
#3081=FACE_OUTER_BOUND('',#4560,.T.);
#3082=FACE_OUTER_BOUND('',#4561,.T.);
#3083=FACE_OUTER_BOUND('',#4562,.T.);
#3084=FACE_OUTER_BOUND('',#4563,.T.);
#3085=FACE_OUTER_BOUND('',#4564,.T.);
#3086=FACE_OUTER_BOUND('',#4565,.T.);
#3087=FACE_OUTER_BOUND('',#4566,.T.);
#3088=FACE_OUTER_BOUND('',#4567,.T.);
#3089=FACE_OUTER_BOUND('',#4568,.T.);
#3090=FACE_OUTER_BOUND('',#4569,.T.);
#3091=FACE_OUTER_BOUND('',#4570,.T.);
#3092=FACE_OUTER_BOUND('',#4571,.T.);
#3093=FACE_OUTER_BOUND('',#4572,.T.);
#3094=FACE_OUTER_BOUND('',#4573,.T.);
#3095=FACE_OUTER_BOUND('',#4574,.T.);
#3096=FACE_OUTER_BOUND('',#4575,.T.);
#3097=FACE_OUTER_BOUND('',#4576,.T.);
#3098=FACE_OUTER_BOUND('',#4577,.T.);
#3099=FACE_OUTER_BOUND('',#4578,.T.);
#3100=FACE_OUTER_BOUND('',#4579,.T.);
#3101=FACE_OUTER_BOUND('',#4580,.T.);
#3102=FACE_OUTER_BOUND('',#4581,.T.);
#3103=FACE_OUTER_BOUND('',#4582,.T.);
#3104=FACE_OUTER_BOUND('',#4583,.T.);
#3105=FACE_OUTER_BOUND('',#4584,.T.);
#3106=FACE_OUTER_BOUND('',#4585,.T.);
#3107=FACE_OUTER_BOUND('',#4586,.T.);
#3108=FACE_OUTER_BOUND('',#4587,.T.);
#3109=FACE_OUTER_BOUND('',#4588,.T.);
#3110=FACE_OUTER_BOUND('',#4589,.T.);
#3111=FACE_OUTER_BOUND('',#4590,.T.);
#3112=FACE_OUTER_BOUND('',#4591,.T.);
#3113=FACE_OUTER_BOUND('',#4592,.T.);
#3114=FACE_OUTER_BOUND('',#4593,.T.);
#3115=FACE_OUTER_BOUND('',#4594,.T.);
#3116=FACE_OUTER_BOUND('',#4595,.T.);
#3117=FACE_OUTER_BOUND('',#4596,.T.);
#3118=FACE_OUTER_BOUND('',#4597,.T.);
#3119=FACE_OUTER_BOUND('',#4598,.T.);
#3120=FACE_OUTER_BOUND('',#4599,.T.);
#3121=FACE_OUTER_BOUND('',#4600,.T.);
#3122=FACE_OUTER_BOUND('',#4601,.T.);
#3123=FACE_OUTER_BOUND('',#4602,.T.);
#3124=FACE_OUTER_BOUND('',#4603,.T.);
#3125=FACE_OUTER_BOUND('',#4604,.T.);
#3126=FACE_OUTER_BOUND('',#4605,.T.);
#3127=FACE_OUTER_BOUND('',#4606,.T.);
#3128=FACE_OUTER_BOUND('',#4607,.T.);
#3129=FACE_OUTER_BOUND('',#4608,.T.);
#3130=FACE_OUTER_BOUND('',#4609,.T.);
#3131=FACE_OUTER_BOUND('',#4610,.T.);
#3132=FACE_OUTER_BOUND('',#4611,.T.);
#3133=FACE_OUTER_BOUND('',#4612,.T.);
#3134=FACE_OUTER_BOUND('',#4613,.T.);
#3135=FACE_OUTER_BOUND('',#4614,.T.);
#3136=FACE_OUTER_BOUND('',#4615,.T.);
#3137=FACE_OUTER_BOUND('',#4616,.T.);
#3138=FACE_OUTER_BOUND('',#4617,.T.);
#3139=FACE_OUTER_BOUND('',#4618,.T.);
#3140=FACE_OUTER_BOUND('',#4619,.T.);
#3141=FACE_OUTER_BOUND('',#4620,.T.);
#3142=FACE_OUTER_BOUND('',#4621,.T.);
#3143=FACE_OUTER_BOUND('',#4622,.T.);
#3144=FACE_OUTER_BOUND('',#4623,.T.);
#3145=FACE_OUTER_BOUND('',#4624,.T.);
#3146=FACE_OUTER_BOUND('',#4625,.T.);
#3147=FACE_OUTER_BOUND('',#4626,.T.);
#3148=FACE_OUTER_BOUND('',#4627,.T.);
#3149=FACE_OUTER_BOUND('',#4628,.T.);
#3150=FACE_OUTER_BOUND('',#4629,.T.);
#3151=FACE_OUTER_BOUND('',#4630,.T.);
#3152=FACE_OUTER_BOUND('',#4631,.T.);
#3153=FACE_OUTER_BOUND('',#4632,.T.);
#3154=FACE_OUTER_BOUND('',#4633,.T.);
#3155=FACE_OUTER_BOUND('',#4634,.T.);
#3156=FACE_OUTER_BOUND('',#4635,.T.);
#3157=FACE_OUTER_BOUND('',#4636,.T.);
#3158=FACE_OUTER_BOUND('',#4637,.T.);
#3159=FACE_OUTER_BOUND('',#4638,.T.);
#3160=FACE_OUTER_BOUND('',#4639,.T.);
#3161=FACE_OUTER_BOUND('',#4640,.T.);
#3162=FACE_OUTER_BOUND('',#4641,.T.);
#3163=FACE_OUTER_BOUND('',#4642,.T.);
#3164=FACE_OUTER_BOUND('',#4643,.T.);
#3165=FACE_OUTER_BOUND('',#4644,.T.);
#3166=FACE_OUTER_BOUND('',#4645,.T.);
#3167=FACE_OUTER_BOUND('',#4646,.T.);
#3168=FACE_OUTER_BOUND('',#4647,.T.);
#3169=FACE_OUTER_BOUND('',#4648,.T.);
#3170=FACE_OUTER_BOUND('',#4649,.T.);
#3171=FACE_OUTER_BOUND('',#4650,.T.);
#3172=FACE_OUTER_BOUND('',#4651,.T.);
#3173=FACE_OUTER_BOUND('',#4652,.T.);
#3174=FACE_OUTER_BOUND('',#4653,.T.);
#3175=FACE_OUTER_BOUND('',#4654,.T.);
#3176=FACE_OUTER_BOUND('',#4655,.T.);
#3177=FACE_OUTER_BOUND('',#4656,.T.);
#3178=FACE_OUTER_BOUND('',#4657,.T.);
#3179=FACE_OUTER_BOUND('',#4658,.T.);
#3180=FACE_OUTER_BOUND('',#4659,.T.);
#3181=FACE_OUTER_BOUND('',#4660,.T.);
#3182=FACE_OUTER_BOUND('',#4661,.T.);
#3183=FACE_OUTER_BOUND('',#4662,.T.);
#3184=FACE_OUTER_BOUND('',#4663,.T.);
#3185=FACE_OUTER_BOUND('',#4664,.T.);
#3186=FACE_OUTER_BOUND('',#4665,.T.);
#3187=FACE_OUTER_BOUND('',#4666,.T.);
#3188=FACE_OUTER_BOUND('',#4667,.T.);
#3189=FACE_OUTER_BOUND('',#4668,.T.);
#3190=FACE_OUTER_BOUND('',#4669,.T.);
#3191=FACE_OUTER_BOUND('',#4670,.T.);
#3192=FACE_OUTER_BOUND('',#4671,.T.);
#3193=FACE_OUTER_BOUND('',#4672,.T.);
#3194=FACE_OUTER_BOUND('',#4673,.T.);
#3195=FACE_OUTER_BOUND('',#4674,.T.);
#3196=FACE_OUTER_BOUND('',#4675,.T.);
#3197=FACE_OUTER_BOUND('',#4676,.T.);
#3198=FACE_OUTER_BOUND('',#4677,.T.);
#3199=FACE_OUTER_BOUND('',#4678,.T.);
#3200=FACE_OUTER_BOUND('',#4679,.T.);
#3201=FACE_OUTER_BOUND('',#4680,.T.);
#3202=FACE_OUTER_BOUND('',#4691,.T.);
#3203=FACE_OUTER_BOUND('',#4702,.T.);
#3204=FACE_OUTER_BOUND('',#4703,.T.);
#3205=FACE_OUTER_BOUND('',#4714,.T.);
#3206=FACE_OUTER_BOUND('',#4715,.T.);
#3207=FACE_OUTER_BOUND('',#4716,.T.);
#3208=FACE_OUTER_BOUND('',#4717,.T.);
#3209=FACE_OUTER_BOUND('',#4718,.T.);
#3210=FACE_OUTER_BOUND('',#4719,.T.);
#3211=FACE_OUTER_BOUND('',#4720,.T.);
#3212=FACE_OUTER_BOUND('',#4721,.T.);
#3213=FACE_OUTER_BOUND('',#4722,.T.);
#3214=FACE_OUTER_BOUND('',#4723,.T.);
#3215=FACE_OUTER_BOUND('',#4724,.T.);
#3216=FACE_OUTER_BOUND('',#4725,.T.);
#3217=FACE_OUTER_BOUND('',#4726,.T.);
#3218=FACE_OUTER_BOUND('',#4727,.T.);
#3219=FACE_OUTER_BOUND('',#4728,.T.);
#3220=FACE_OUTER_BOUND('',#4729,.T.);
#3221=FACE_OUTER_BOUND('',#4730,.T.);
#3222=FACE_OUTER_BOUND('',#4731,.T.);
#3223=FACE_OUTER_BOUND('',#4732,.T.);
#3224=FACE_OUTER_BOUND('',#4733,.T.);
#3225=FACE_OUTER_BOUND('',#4734,.T.);
#3226=FACE_OUTER_BOUND('',#4735,.T.);
#3227=FACE_OUTER_BOUND('',#4736,.T.);
#3228=FACE_OUTER_BOUND('',#4737,.T.);
#3229=FACE_OUTER_BOUND('',#4738,.T.);
#3230=FACE_OUTER_BOUND('',#4739,.T.);
#3231=FACE_OUTER_BOUND('',#4740,.T.);
#3232=FACE_OUTER_BOUND('',#4741,.T.);
#3233=FACE_OUTER_BOUND('',#4742,.T.);
#3234=FACE_OUTER_BOUND('',#4743,.T.);
#3235=FACE_OUTER_BOUND('',#4744,.T.);
#3236=FACE_OUTER_BOUND('',#4745,.T.);
#3237=FACE_OUTER_BOUND('',#4746,.T.);
#3238=FACE_OUTER_BOUND('',#4747,.T.);
#3239=FACE_OUTER_BOUND('',#4748,.T.);
#3240=FACE_OUTER_BOUND('',#4749,.T.);
#3241=FACE_OUTER_BOUND('',#4750,.T.);
#3242=FACE_OUTER_BOUND('',#4751,.T.);
#3243=FACE_OUTER_BOUND('',#4752,.T.);
#3244=FACE_OUTER_BOUND('',#4753,.T.);
#3245=FACE_OUTER_BOUND('',#4754,.T.);
#3246=FACE_OUTER_BOUND('',#4755,.T.);
#3247=FACE_OUTER_BOUND('',#4756,.T.);
#3248=FACE_OUTER_BOUND('',#4757,.T.);
#3249=FACE_OUTER_BOUND('',#4768,.T.);
#3250=FACE_OUTER_BOUND('',#4769,.T.);
#3251=FACE_OUTER_BOUND('',#4770,.T.);
#3252=FACE_OUTER_BOUND('',#4771,.T.);
#3253=FACE_OUTER_BOUND('',#4772,.T.);
#3254=FACE_OUTER_BOUND('',#4774,.T.);
#3255=FACE_OUTER_BOUND('',#4775,.T.);
#3256=FACE_OUTER_BOUND('',#4776,.T.);
#3257=FACE_OUTER_BOUND('',#4778,.T.);
#3258=FACE_OUTER_BOUND('',#4779,.T.);
#3259=FACE_OUTER_BOUND('',#4780,.T.);
#3260=FACE_OUTER_BOUND('',#4782,.T.);
#3261=FACE_OUTER_BOUND('',#4783,.T.);
#3262=FACE_OUTER_BOUND('',#4784,.T.);
#3263=FACE_OUTER_BOUND('',#4786,.T.);
#3264=FACE_OUTER_BOUND('',#4787,.T.);
#3265=FACE_OUTER_BOUND('',#4789,.T.);
#3266=FACE_OUTER_BOUND('',#4790,.T.);
#3267=FACE_OUTER_BOUND('',#4791,.T.);
#3268=FACE_OUTER_BOUND('',#4793,.T.);
#3269=FACE_OUTER_BOUND('',#4794,.T.);
#3270=FACE_OUTER_BOUND('',#4795,.T.);
#3271=FACE_OUTER_BOUND('',#4796,.T.);
#3272=FACE_OUTER_BOUND('',#4797,.T.);
#3273=FACE_OUTER_BOUND('',#4798,.T.);
#3274=FACE_OUTER_BOUND('',#4799,.T.);
#3275=FACE_OUTER_BOUND('',#4800,.T.);
#3276=FACE_OUTER_BOUND('',#4803,.T.);
#3277=FACE_OUTER_BOUND('',#4806,.T.);
#3278=FACE_OUTER_BOUND('',#4807,.T.);
#3279=FACE_OUTER_BOUND('',#4808,.T.);
#3280=FACE_OUTER_BOUND('',#4809,.T.);
#3281=FACE_OUTER_BOUND('',#4810,.T.);
#3282=FACE_OUTER_BOUND('',#4811,.T.);
#3283=FACE_OUTER_BOUND('',#4812,.T.);
#3284=FACE_OUTER_BOUND('',#4813,.T.);
#3285=FACE_OUTER_BOUND('',#4814,.T.);
#3286=FACE_OUTER_BOUND('',#4815,.T.);
#3287=FACE_OUTER_BOUND('',#4816,.T.);
#3288=FACE_OUTER_BOUND('',#4817,.T.);
#3289=FACE_OUTER_BOUND('',#4818,.T.);
#3290=FACE_OUTER_BOUND('',#4819,.T.);
#3291=FACE_OUTER_BOUND('',#4820,.T.);
#3292=FACE_OUTER_BOUND('',#4822,.T.);
#3293=FACE_OUTER_BOUND('',#4823,.T.);
#3294=FACE_OUTER_BOUND('',#4824,.T.);
#3295=FACE_OUTER_BOUND('',#4825,.T.);
#3296=FACE_OUTER_BOUND('',#4826,.T.);
#3297=FACE_OUTER_BOUND('',#4827,.T.);
#3298=FACE_OUTER_BOUND('',#4828,.T.);
#3299=FACE_OUTER_BOUND('',#4829,.T.);
#3300=FACE_OUTER_BOUND('',#4830,.T.);
#3301=FACE_OUTER_BOUND('',#4831,.T.);
#3302=FACE_OUTER_BOUND('',#4832,.T.);
#3303=FACE_OUTER_BOUND('',#4833,.T.);
#3304=FACE_OUTER_BOUND('',#4834,.T.);
#3305=FACE_OUTER_BOUND('',#4835,.T.);
#3306=FACE_OUTER_BOUND('',#4836,.T.);
#3307=FACE_OUTER_BOUND('',#4837,.T.);
#3308=FACE_OUTER_BOUND('',#4838,.T.);
#3309=FACE_OUTER_BOUND('',#4839,.T.);
#3310=FACE_OUTER_BOUND('',#4840,.T.);
#3311=FACE_OUTER_BOUND('',#4841,.T.);
#3312=FACE_OUTER_BOUND('',#4842,.T.);
#3313=FACE_OUTER_BOUND('',#4843,.T.);
#3314=FACE_OUTER_BOUND('',#4844,.T.);
#3315=FACE_OUTER_BOUND('',#4845,.T.);
#3316=FACE_OUTER_BOUND('',#4846,.T.);
#3317=FACE_OUTER_BOUND('',#4847,.T.);
#3318=FACE_OUTER_BOUND('',#4848,.T.);
#3319=FACE_OUTER_BOUND('',#4849,.T.);
#3320=FACE_OUTER_BOUND('',#4850,.T.);
#3321=FACE_OUTER_BOUND('',#4851,.T.);
#3322=FACE_OUTER_BOUND('',#4852,.T.);
#3323=FACE_OUTER_BOUND('',#4853,.T.);
#3324=FACE_OUTER_BOUND('',#4854,.T.);
#3325=FACE_OUTER_BOUND('',#4855,.T.);
#3326=FACE_OUTER_BOUND('',#4856,.T.);
#3327=FACE_OUTER_BOUND('',#4857,.T.);
#3328=FACE_OUTER_BOUND('',#4858,.T.);
#3329=FACE_OUTER_BOUND('',#4859,.T.);
#3330=FACE_OUTER_BOUND('',#4860,.T.);
#3331=FACE_OUTER_BOUND('',#4861,.T.);
#3332=FACE_OUTER_BOUND('',#4862,.T.);
#3333=FACE_OUTER_BOUND('',#4863,.T.);
#3334=FACE_OUTER_BOUND('',#4864,.T.);
#3335=FACE_OUTER_BOUND('',#4865,.T.);
#3336=FACE_OUTER_BOUND('',#4866,.T.);
#3337=FACE_OUTER_BOUND('',#4867,.T.);
#3338=FACE_OUTER_BOUND('',#4868,.T.);
#3339=FACE_OUTER_BOUND('',#4869,.T.);
#3340=FACE_OUTER_BOUND('',#4870,.T.);
#3341=FACE_OUTER_BOUND('',#4871,.T.);
#3342=FACE_OUTER_BOUND('',#4872,.T.);
#3343=FACE_OUTER_BOUND('',#4873,.T.);
#3344=FACE_OUTER_BOUND('',#4874,.T.);
#3345=FACE_OUTER_BOUND('',#4875,.T.);
#3346=FACE_OUTER_BOUND('',#4876,.T.);
#3347=FACE_OUTER_BOUND('',#4877,.T.);
#3348=FACE_OUTER_BOUND('',#4878,.T.);
#3349=FACE_OUTER_BOUND('',#4879,.T.);
#3350=FACE_OUTER_BOUND('',#4880,.T.);
#3351=FACE_OUTER_BOUND('',#4881,.T.);
#3352=FACE_OUTER_BOUND('',#4882,.T.);
#3353=FACE_OUTER_BOUND('',#4883,.T.);
#3354=FACE_OUTER_BOUND('',#4884,.T.);
#3355=FACE_OUTER_BOUND('',#4885,.T.);
#3356=FACE_OUTER_BOUND('',#4886,.T.);
#3357=FACE_OUTER_BOUND('',#4887,.T.);
#3358=FACE_OUTER_BOUND('',#4888,.T.);
#3359=FACE_OUTER_BOUND('',#4889,.T.);
#3360=FACE_OUTER_BOUND('',#4890,.T.);
#3361=FACE_OUTER_BOUND('',#4891,.T.);
#3362=FACE_OUTER_BOUND('',#4892,.T.);
#3363=FACE_OUTER_BOUND('',#4893,.T.);
#3364=FACE_OUTER_BOUND('',#4894,.T.);
#3365=FACE_OUTER_BOUND('',#4895,.T.);
#3366=FACE_OUTER_BOUND('',#4896,.T.);
#3367=FACE_OUTER_BOUND('',#4897,.T.);
#3368=FACE_OUTER_BOUND('',#4898,.T.);
#3369=FACE_OUTER_BOUND('',#4899,.T.);
#3370=FACE_OUTER_BOUND('',#4900,.T.);
#3371=FACE_OUTER_BOUND('',#4901,.T.);
#3372=FACE_OUTER_BOUND('',#4902,.T.);
#3373=FACE_OUTER_BOUND('',#4903,.T.);
#3374=FACE_OUTER_BOUND('',#4904,.T.);
#3375=FACE_OUTER_BOUND('',#4905,.T.);
#3376=FACE_OUTER_BOUND('',#4906,.T.);
#3377=FACE_OUTER_BOUND('',#4907,.T.);
#3378=FACE_OUTER_BOUND('',#4908,.T.);
#3379=FACE_OUTER_BOUND('',#4909,.T.);
#3380=FACE_OUTER_BOUND('',#4910,.T.);
#3381=FACE_OUTER_BOUND('',#4911,.T.);
#3382=FACE_OUTER_BOUND('',#4912,.T.);
#3383=FACE_OUTER_BOUND('',#4913,.T.);
#3384=FACE_OUTER_BOUND('',#4914,.T.);
#3385=FACE_OUTER_BOUND('',#4915,.T.);
#3386=FACE_OUTER_BOUND('',#4916,.T.);
#3387=FACE_OUTER_BOUND('',#4917,.T.);
#3388=FACE_OUTER_BOUND('',#4918,.T.);
#3389=FACE_OUTER_BOUND('',#4919,.T.);
#3390=FACE_OUTER_BOUND('',#4920,.T.);
#3391=FACE_OUTER_BOUND('',#4921,.T.);
#3392=FACE_OUTER_BOUND('',#4922,.T.);
#3393=FACE_OUTER_BOUND('',#4923,.T.);
#3394=FACE_OUTER_BOUND('',#4924,.T.);
#3395=FACE_OUTER_BOUND('',#4925,.T.);
#3396=FACE_OUTER_BOUND('',#4926,.T.);
#3397=FACE_OUTER_BOUND('',#4927,.T.);
#3398=FACE_OUTER_BOUND('',#4928,.T.);
#3399=FACE_OUTER_BOUND('',#4929,.T.);
#3400=FACE_OUTER_BOUND('',#4930,.T.);
#3401=FACE_OUTER_BOUND('',#4931,.T.);
#3402=FACE_OUTER_BOUND('',#4932,.T.);
#3403=FACE_OUTER_BOUND('',#4933,.T.);
#3404=FACE_OUTER_BOUND('',#4934,.T.);
#3405=FACE_OUTER_BOUND('',#4936,.T.);
#3406=FACE_OUTER_BOUND('',#4937,.T.);
#3407=FACE_OUTER_BOUND('',#4938,.T.);
#3408=FACE_OUTER_BOUND('',#4939,.T.);
#3409=FACE_OUTER_BOUND('',#4940,.T.);
#3410=FACE_OUTER_BOUND('',#4941,.T.);
#3411=FACE_OUTER_BOUND('',#4942,.T.);
#3412=FACE_OUTER_BOUND('',#4943,.T.);
#3413=FACE_OUTER_BOUND('',#4944,.T.);
#3414=FACE_OUTER_BOUND('',#4945,.T.);
#3415=FACE_OUTER_BOUND('',#4946,.T.);
#3416=FACE_OUTER_BOUND('',#4947,.T.);
#3417=FACE_OUTER_BOUND('',#4948,.T.);
#3418=FACE_OUTER_BOUND('',#4949,.T.);
#3419=FACE_OUTER_BOUND('',#4950,.T.);
#3420=FACE_OUTER_BOUND('',#4951,.T.);
#3421=FACE_OUTER_BOUND('',#4952,.T.);
#3422=FACE_OUTER_BOUND('',#4953,.T.);
#3423=FACE_OUTER_BOUND('',#4954,.T.);
#3424=FACE_OUTER_BOUND('',#4955,.T.);
#3425=FACE_OUTER_BOUND('',#4956,.T.);
#3426=FACE_OUTER_BOUND('',#4957,.T.);
#3427=FACE_OUTER_BOUND('',#4958,.T.);
#3428=FACE_OUTER_BOUND('',#4959,.T.);
#3429=FACE_OUTER_BOUND('',#4960,.T.);
#3430=FACE_OUTER_BOUND('',#4961,.T.);
#3431=FACE_OUTER_BOUND('',#4962,.T.);
#3432=FACE_OUTER_BOUND('',#4963,.T.);
#3433=FACE_OUTER_BOUND('',#4964,.T.);
#3434=FACE_OUTER_BOUND('',#4965,.T.);
#3435=FACE_OUTER_BOUND('',#4967,.T.);
#3436=FACE_OUTER_BOUND('',#4968,.T.);
#3437=FACE_OUTER_BOUND('',#4969,.T.);
#3438=FACE_OUTER_BOUND('',#4970,.T.);
#3439=FACE_OUTER_BOUND('',#4971,.T.);
#3440=FACE_OUTER_BOUND('',#4972,.T.);
#3441=FACE_OUTER_BOUND('',#4973,.T.);
#3442=FACE_OUTER_BOUND('',#4974,.T.);
#3443=FACE_OUTER_BOUND('',#4975,.T.);
#3444=FACE_OUTER_BOUND('',#4976,.T.);
#3445=FACE_OUTER_BOUND('',#4977,.T.);
#3446=FACE_OUTER_BOUND('',#4978,.T.);
#3447=FACE_OUTER_BOUND('',#4979,.T.);
#3448=FACE_OUTER_BOUND('',#4980,.T.);
#3449=FACE_OUTER_BOUND('',#4981,.T.);
#3450=FACE_OUTER_BOUND('',#4982,.T.);
#3451=FACE_OUTER_BOUND('',#4983,.T.);
#3452=FACE_OUTER_BOUND('',#4984,.T.);
#3453=FACE_OUTER_BOUND('',#4985,.T.);
#3454=FACE_OUTER_BOUND('',#4986,.T.);
#3455=FACE_OUTER_BOUND('',#4987,.T.);
#3456=FACE_OUTER_BOUND('',#4988,.T.);
#3457=FACE_OUTER_BOUND('',#4989,.T.);
#3458=FACE_OUTER_BOUND('',#4990,.T.);
#3459=FACE_OUTER_BOUND('',#4991,.T.);
#3460=FACE_OUTER_BOUND('',#4992,.T.);
#3461=FACE_OUTER_BOUND('',#4993,.T.);
#3462=FACE_OUTER_BOUND('',#4994,.T.);
#3463=FACE_OUTER_BOUND('',#4995,.T.);
#3464=FACE_OUTER_BOUND('',#4996,.T.);
#3465=FACE_OUTER_BOUND('',#4997,.T.);
#3466=FACE_OUTER_BOUND('',#4998,.T.);
#3467=FACE_OUTER_BOUND('',#4999,.T.);
#3468=FACE_OUTER_BOUND('',#5000,.T.);
#3469=FACE_OUTER_BOUND('',#5001,.T.);
#3470=FACE_OUTER_BOUND('',#5002,.T.);
#3471=FACE_OUTER_BOUND('',#5003,.T.);
#3472=FACE_OUTER_BOUND('',#5004,.T.);
#3473=FACE_OUTER_BOUND('',#5005,.T.);
#3474=FACE_OUTER_BOUND('',#5006,.T.);
#3475=FACE_OUTER_BOUND('',#5007,.T.);
#3476=FACE_OUTER_BOUND('',#5008,.T.);
#3477=FACE_OUTER_BOUND('',#5009,.T.);
#3478=FACE_OUTER_BOUND('',#5010,.T.);
#3479=FACE_OUTER_BOUND('',#5011,.T.);
#3480=FACE_OUTER_BOUND('',#5012,.T.);
#3481=FACE_OUTER_BOUND('',#5013,.T.);
#3482=FACE_OUTER_BOUND('',#5014,.T.);
#3483=FACE_OUTER_BOUND('',#5015,.T.);
#3484=FACE_OUTER_BOUND('',#5016,.T.);
#3485=FACE_OUTER_BOUND('',#5017,.T.);
#3486=FACE_OUTER_BOUND('',#5018,.T.);
#3487=FACE_OUTER_BOUND('',#5019,.T.);
#3488=FACE_OUTER_BOUND('',#5020,.T.);
#3489=FACE_OUTER_BOUND('',#5021,.T.);
#3490=FACE_OUTER_BOUND('',#5022,.T.);
#3491=FACE_OUTER_BOUND('',#5023,.T.);
#3492=FACE_OUTER_BOUND('',#5024,.T.);
#3493=FACE_OUTER_BOUND('',#5025,.T.);
#3494=FACE_OUTER_BOUND('',#5026,.T.);
#3495=FACE_OUTER_BOUND('',#5027,.T.);
#3496=FACE_OUTER_BOUND('',#5028,.T.);
#3497=FACE_OUTER_BOUND('',#5029,.T.);
#3498=FACE_OUTER_BOUND('',#5030,.T.);
#3499=FACE_OUTER_BOUND('',#5031,.T.);
#3500=FACE_OUTER_BOUND('',#5032,.T.);
#3501=FACE_OUTER_BOUND('',#5033,.T.);
#3502=FACE_OUTER_BOUND('',#5034,.T.);
#3503=FACE_OUTER_BOUND('',#5035,.T.);
#3504=FACE_OUTER_BOUND('',#5036,.T.);
#3505=FACE_OUTER_BOUND('',#5037,.T.);
#3506=FACE_OUTER_BOUND('',#5038,.T.);
#3507=FACE_OUTER_BOUND('',#5039,.T.);
#3508=FACE_OUTER_BOUND('',#5040,.T.);
#3509=FACE_OUTER_BOUND('',#5041,.T.);
#3510=FACE_OUTER_BOUND('',#5042,.T.);
#3511=FACE_OUTER_BOUND('',#5043,.T.);
#3512=FACE_OUTER_BOUND('',#5044,.T.);
#3513=FACE_OUTER_BOUND('',#5045,.T.);
#3514=FACE_OUTER_BOUND('',#5046,.T.);
#3515=FACE_OUTER_BOUND('',#5047,.T.);
#3516=FACE_OUTER_BOUND('',#5048,.T.);
#3517=FACE_OUTER_BOUND('',#5049,.T.);
#3518=FACE_OUTER_BOUND('',#5050,.T.);
#3519=FACE_OUTER_BOUND('',#5051,.T.);
#3520=FACE_OUTER_BOUND('',#5052,.T.);
#3521=FACE_OUTER_BOUND('',#5053,.T.);
#3522=FACE_OUTER_BOUND('',#5054,.T.);
#3523=FACE_OUTER_BOUND('',#5055,.T.);
#3524=FACE_OUTER_BOUND('',#5056,.T.);
#3525=FACE_OUTER_BOUND('',#5057,.T.);
#3526=FACE_OUTER_BOUND('',#5058,.T.);
#3527=FACE_OUTER_BOUND('',#5059,.T.);
#3528=FACE_OUTER_BOUND('',#5060,.T.);
#3529=FACE_OUTER_BOUND('',#5061,.T.);
#3530=FACE_OUTER_BOUND('',#5062,.T.);
#3531=FACE_OUTER_BOUND('',#5063,.T.);
#3532=FACE_OUTER_BOUND('',#5064,.T.);
#3533=FACE_OUTER_BOUND('',#5065,.T.);
#3534=FACE_OUTER_BOUND('',#5066,.T.);
#3535=FACE_OUTER_BOUND('',#5067,.T.);
#3536=FACE_OUTER_BOUND('',#5068,.T.);
#3537=FACE_OUTER_BOUND('',#5069,.T.);
#3538=FACE_OUTER_BOUND('',#5070,.T.);
#3539=FACE_OUTER_BOUND('',#5071,.T.);
#3540=FACE_OUTER_BOUND('',#5072,.T.);
#3541=FACE_OUTER_BOUND('',#5073,.T.);
#3542=FACE_OUTER_BOUND('',#5074,.T.);
#3543=FACE_OUTER_BOUND('',#5075,.T.);
#3544=FACE_OUTER_BOUND('',#5076,.T.);
#3545=FACE_OUTER_BOUND('',#5077,.T.);
#3546=FACE_OUTER_BOUND('',#5078,.T.);
#3547=FACE_OUTER_BOUND('',#5079,.T.);
#3548=FACE_OUTER_BOUND('',#5081,.T.);
#3549=FACE_OUTER_BOUND('',#5082,.T.);
#3550=FACE_OUTER_BOUND('',#5083,.T.);
#3551=FACE_OUTER_BOUND('',#5084,.T.);
#3552=FACE_OUTER_BOUND('',#5085,.T.);
#3553=FACE_OUTER_BOUND('',#5086,.T.);
#3554=FACE_OUTER_BOUND('',#5087,.T.);
#3555=FACE_OUTER_BOUND('',#5088,.T.);
#3556=FACE_OUTER_BOUND('',#5089,.T.);
#3557=FACE_OUTER_BOUND('',#5090,.T.);
#3558=FACE_OUTER_BOUND('',#5091,.T.);
#3559=FACE_OUTER_BOUND('',#5092,.T.);
#3560=FACE_OUTER_BOUND('',#5093,.T.);
#3561=FACE_OUTER_BOUND('',#5094,.T.);
#3562=FACE_OUTER_BOUND('',#5095,.T.);
#3563=FACE_OUTER_BOUND('',#5096,.T.);
#3564=FACE_OUTER_BOUND('',#5097,.T.);
#3565=FACE_OUTER_BOUND('',#5098,.T.);
#3566=FACE_OUTER_BOUND('',#5099,.T.);
#3567=FACE_OUTER_BOUND('',#5100,.T.);
#3568=FACE_OUTER_BOUND('',#5101,.T.);
#3569=FACE_OUTER_BOUND('',#5102,.T.);
#3570=FACE_OUTER_BOUND('',#5103,.T.);
#3571=FACE_OUTER_BOUND('',#5104,.T.);
#3572=FACE_OUTER_BOUND('',#5105,.T.);
#3573=FACE_OUTER_BOUND('',#5106,.T.);
#3574=FACE_OUTER_BOUND('',#5107,.T.);
#3575=FACE_OUTER_BOUND('',#5108,.T.);
#3576=FACE_OUTER_BOUND('',#5109,.T.);
#3577=FACE_OUTER_BOUND('',#5110,.T.);
#3578=FACE_OUTER_BOUND('',#5111,.T.);
#3579=FACE_OUTER_BOUND('',#5112,.T.);
#3580=FACE_OUTER_BOUND('',#5113,.T.);
#3581=FACE_OUTER_BOUND('',#5114,.T.);
#3582=FACE_OUTER_BOUND('',#5115,.T.);
#3583=FACE_OUTER_BOUND('',#5116,.T.);
#3584=FACE_OUTER_BOUND('',#5117,.T.);
#3585=FACE_OUTER_BOUND('',#5118,.T.);
#3586=FACE_OUTER_BOUND('',#5119,.T.);
#3587=FACE_OUTER_BOUND('',#5120,.T.);
#3588=FACE_OUTER_BOUND('',#5122,.T.);
#3589=FACE_OUTER_BOUND('',#5123,.T.);
#3590=FACE_OUTER_BOUND('',#5124,.T.);
#3591=FACE_OUTER_BOUND('',#5125,.T.);
#3592=FACE_OUTER_BOUND('',#5126,.T.);
#3593=FACE_OUTER_BOUND('',#5127,.T.);
#3594=FACE_OUTER_BOUND('',#5128,.T.);
#3595=FACE_OUTER_BOUND('',#5129,.T.);
#3596=FACE_OUTER_BOUND('',#5130,.T.);
#3597=FACE_OUTER_BOUND('',#5131,.T.);
#3598=FACE_OUTER_BOUND('',#5132,.T.);
#3599=FACE_OUTER_BOUND('',#5133,.T.);
#3600=FACE_OUTER_BOUND('',#5134,.T.);
#3601=FACE_OUTER_BOUND('',#5135,.T.);
#3602=FACE_OUTER_BOUND('',#5136,.T.);
#3603=FACE_OUTER_BOUND('',#5137,.T.);
#3604=FACE_OUTER_BOUND('',#5138,.T.);
#3605=FACE_OUTER_BOUND('',#5139,.T.);
#3606=FACE_OUTER_BOUND('',#5140,.T.);
#3607=FACE_OUTER_BOUND('',#5141,.T.);
#3608=FACE_OUTER_BOUND('',#5142,.T.);
#3609=FACE_OUTER_BOUND('',#5143,.T.);
#3610=FACE_OUTER_BOUND('',#5144,.T.);
#3611=FACE_OUTER_BOUND('',#5145,.T.);
#3612=FACE_OUTER_BOUND('',#5146,.T.);
#3613=FACE_OUTER_BOUND('',#5147,.T.);
#3614=FACE_OUTER_BOUND('',#5148,.T.);
#3615=FACE_OUTER_BOUND('',#5149,.T.);
#3616=FACE_OUTER_BOUND('',#5150,.T.);
#3617=FACE_OUTER_BOUND('',#5151,.T.);
#3618=FACE_OUTER_BOUND('',#5152,.T.);
#3619=FACE_OUTER_BOUND('',#5153,.T.);
#3620=FACE_OUTER_BOUND('',#5154,.T.);
#3621=FACE_OUTER_BOUND('',#5155,.T.);
#3622=FACE_OUTER_BOUND('',#5156,.T.);
#3623=FACE_OUTER_BOUND('',#5157,.T.);
#3624=FACE_OUTER_BOUND('',#5158,.T.);
#3625=FACE_OUTER_BOUND('',#5159,.T.);
#3626=FACE_OUTER_BOUND('',#5160,.T.);
#3627=FACE_OUTER_BOUND('',#5161,.T.);
#3628=FACE_OUTER_BOUND('',#5162,.T.);
#3629=FACE_OUTER_BOUND('',#5163,.T.);
#3630=FACE_OUTER_BOUND('',#5164,.T.);
#3631=FACE_OUTER_BOUND('',#5165,.T.);
#3632=FACE_OUTER_BOUND('',#5166,.T.);
#3633=FACE_OUTER_BOUND('',#5167,.T.);
#3634=FACE_OUTER_BOUND('',#5168,.T.);
#3635=FACE_OUTER_BOUND('',#5169,.T.);
#3636=FACE_OUTER_BOUND('',#5170,.T.);
#3637=FACE_OUTER_BOUND('',#5171,.T.);
#3638=FACE_OUTER_BOUND('',#5172,.T.);
#3639=FACE_OUTER_BOUND('',#5173,.T.);
#3640=FACE_OUTER_BOUND('',#5174,.T.);
#3641=FACE_OUTER_BOUND('',#5175,.T.);
#3642=FACE_OUTER_BOUND('',#5176,.T.);
#3643=FACE_OUTER_BOUND('',#5177,.T.);
#3644=FACE_OUTER_BOUND('',#5178,.T.);
#3645=FACE_OUTER_BOUND('',#5179,.T.);
#3646=FACE_OUTER_BOUND('',#5180,.T.);
#3647=FACE_OUTER_BOUND('',#5181,.T.);
#3648=FACE_OUTER_BOUND('',#5182,.T.);
#3649=FACE_OUTER_BOUND('',#5183,.T.);
#3650=FACE_OUTER_BOUND('',#5184,.T.);
#3651=FACE_OUTER_BOUND('',#5185,.T.);
#3652=FACE_OUTER_BOUND('',#5186,.T.);
#3653=FACE_OUTER_BOUND('',#5187,.T.);
#3654=FACE_OUTER_BOUND('',#5188,.T.);
#3655=FACE_OUTER_BOUND('',#5189,.T.);
#3656=FACE_OUTER_BOUND('',#5190,.T.);
#3657=FACE_OUTER_BOUND('',#5191,.T.);
#3658=FACE_OUTER_BOUND('',#5192,.T.);
#3659=FACE_OUTER_BOUND('',#5193,.T.);
#3660=FACE_OUTER_BOUND('',#5194,.T.);
#3661=FACE_OUTER_BOUND('',#5195,.T.);
#3662=FACE_OUTER_BOUND('',#5196,.T.);
#3663=FACE_OUTER_BOUND('',#5197,.T.);
#3664=FACE_OUTER_BOUND('',#5198,.T.);
#3665=FACE_OUTER_BOUND('',#5199,.T.);
#3666=FACE_OUTER_BOUND('',#5200,.T.);
#3667=FACE_OUTER_BOUND('',#5201,.T.);
#3668=FACE_OUTER_BOUND('',#5202,.T.);
#3669=FACE_OUTER_BOUND('',#5203,.T.);
#3670=FACE_OUTER_BOUND('',#5204,.T.);
#3671=FACE_OUTER_BOUND('',#5205,.T.);
#3672=FACE_OUTER_BOUND('',#5206,.T.);
#3673=FACE_OUTER_BOUND('',#5207,.T.);
#3674=FACE_OUTER_BOUND('',#5208,.T.);
#3675=FACE_OUTER_BOUND('',#5209,.T.);
#3676=FACE_OUTER_BOUND('',#5210,.T.);
#3677=FACE_OUTER_BOUND('',#5211,.T.);
#3678=FACE_OUTER_BOUND('',#5212,.T.);
#3679=FACE_OUTER_BOUND('',#5213,.T.);
#3680=FACE_OUTER_BOUND('',#5214,.T.);
#3681=FACE_OUTER_BOUND('',#5215,.T.);
#3682=FACE_OUTER_BOUND('',#5216,.T.);
#3683=FACE_OUTER_BOUND('',#5217,.T.);
#3684=FACE_OUTER_BOUND('',#5218,.T.);
#3685=FACE_OUTER_BOUND('',#5219,.T.);
#3686=FACE_OUTER_BOUND('',#5220,.T.);
#3687=FACE_OUTER_BOUND('',#5221,.T.);
#3688=FACE_OUTER_BOUND('',#5222,.T.);
#3689=FACE_OUTER_BOUND('',#5223,.T.);
#3690=FACE_OUTER_BOUND('',#5224,.T.);
#3691=FACE_OUTER_BOUND('',#5225,.T.);
#3692=FACE_OUTER_BOUND('',#5226,.T.);
#3693=FACE_OUTER_BOUND('',#5227,.T.);
#3694=FACE_OUTER_BOUND('',#5228,.T.);
#3695=FACE_OUTER_BOUND('',#5229,.T.);
#3696=FACE_OUTER_BOUND('',#5230,.T.);
#3697=FACE_OUTER_BOUND('',#5231,.T.);
#3698=FACE_OUTER_BOUND('',#5232,.T.);
#3699=FACE_OUTER_BOUND('',#5233,.T.);
#3700=FACE_OUTER_BOUND('',#5234,.T.);
#3701=FACE_OUTER_BOUND('',#5236,.T.);
#3702=FACE_OUTER_BOUND('',#5237,.T.);
#3703=FACE_OUTER_BOUND('',#5238,.T.);
#3704=FACE_OUTER_BOUND('',#5239,.T.);
#3705=FACE_OUTER_BOUND('',#5240,.T.);
#3706=FACE_OUTER_BOUND('',#5241,.T.);
#3707=FACE_OUTER_BOUND('',#5242,.T.);
#3708=FACE_OUTER_BOUND('',#5243,.T.);
#3709=FACE_OUTER_BOUND('',#5244,.T.);
#3710=FACE_OUTER_BOUND('',#5245,.T.);
#3711=FACE_OUTER_BOUND('',#5246,.T.);
#3712=FACE_OUTER_BOUND('',#5247,.T.);
#3713=FACE_OUTER_BOUND('',#5248,.T.);
#3714=FACE_OUTER_BOUND('',#5249,.T.);
#3715=FACE_OUTER_BOUND('',#5250,.T.);
#3716=FACE_OUTER_BOUND('',#5252,.T.);
#3717=FACE_OUTER_BOUND('',#5253,.T.);
#3718=FACE_OUTER_BOUND('',#5254,.T.);
#3719=FACE_OUTER_BOUND('',#5256,.T.);
#3720=FACE_OUTER_BOUND('',#5257,.T.);
#3721=FACE_OUTER_BOUND('',#5258,.T.);
#3722=FACE_OUTER_BOUND('',#5259,.T.);
#3723=FACE_OUTER_BOUND('',#5261,.T.);
#3724=FACE_OUTER_BOUND('',#5262,.T.);
#3725=FACE_OUTER_BOUND('',#5263,.T.);
#3726=FACE_OUTER_BOUND('',#5265,.T.);
#3727=FACE_OUTER_BOUND('',#5266,.T.);
#3728=FACE_OUTER_BOUND('',#5268,.T.);
#3729=FACE_OUTER_BOUND('',#5269,.T.);
#3730=FACE_OUTER_BOUND('',#5270,.T.);
#3731=FACE_OUTER_BOUND('',#5271,.T.);
#3732=FACE_OUTER_BOUND('',#5272,.T.);
#3733=FACE_OUTER_BOUND('',#5273,.T.);
#3734=FACE_OUTER_BOUND('',#5274,.T.);
#3735=FACE_OUTER_BOUND('',#5275,.T.);
#3736=EDGE_LOOP('',(#17586,#17587,#17588,#17589));
#3737=EDGE_LOOP('',(#17590,#17591,#17592,#17593,#17594));
#3738=EDGE_LOOP('',(#17595,#17596,#17597,#17598));
#3739=EDGE_LOOP('',(#17599));
#3740=EDGE_LOOP('',(#17600,#17601,#17602,#17603));
#3741=EDGE_LOOP('',(#17604,#17605,#17606,#17607,#17608));
#3742=EDGE_LOOP('',(#17609,#17610,#17611,#17612));
#3743=EDGE_LOOP('',(#17613));
#3744=EDGE_LOOP('',(#17614,#17615,#17616,#17617));
#3745=EDGE_LOOP('',(#17618,#17619,#17620,#17621));
#3746=EDGE_LOOP('',(#17622,#17623,#17624,#17625));
#3747=EDGE_LOOP('',(#17626,#17627,#17628,#17629,#17630));
#3748=EDGE_LOOP('',(#17631,#17632,#17633,#17634));
#3749=EDGE_LOOP('',(#17635));
#3750=EDGE_LOOP('',(#17636,#17637,#17638,#17639));
#3751=EDGE_LOOP('',(#17640,#17641,#17642,#17643,#17644));
#3752=EDGE_LOOP('',(#17645,#17646,#17647,#17648));
#3753=EDGE_LOOP('',(#17649));
#3754=EDGE_LOOP('',(#17650,#17651,#17652,#17653));
#3755=EDGE_LOOP('',(#17654,#17655,#17656,#17657));
#3756=EDGE_LOOP('',(#17658,#17659,#17660,#17661));
#3757=EDGE_LOOP('',(#17662,#17663,#17664,#17665));
#3758=EDGE_LOOP('',(#17666,#17667,#17668,#17669));
#3759=EDGE_LOOP('',(#17670,#17671,#17672,#17673));
#3760=EDGE_LOOP('',(#17674,#17675,#17676,#17677));
#3761=EDGE_LOOP('',(#17678,#17679,#17680,#17681,#17682,#17683,#17684,#17685,
#17686,#17687,#17688,#17689,#17690,#17691,#17692,#17693,#17694,#17695,#17696,
#17697));
#3762=EDGE_LOOP('',(#17698));
#3763=EDGE_LOOP('',(#17699));
#3764=EDGE_LOOP('',(#17700));
#3765=EDGE_LOOP('',(#17701));
#3766=EDGE_LOOP('',(#17702));
#3767=EDGE_LOOP('',(#17703));
#3768=EDGE_LOOP('',(#17704));
#3769=EDGE_LOOP('',(#17705));
#3770=EDGE_LOOP('',(#17706));
#3771=EDGE_LOOP('',(#17707,#17708,#17709,#17710));
#3772=EDGE_LOOP('',(#17711,#17712,#17713,#17714));
#3773=EDGE_LOOP('',(#17715,#17716,#17717,#17718));
#3774=EDGE_LOOP('',(#17719,#17720,#17721,#17722));
#3775=EDGE_LOOP('',(#17723,#17724,#17725,#17726));
#3776=EDGE_LOOP('',(#17727,#17728,#17729,#17730));
#3777=EDGE_LOOP('',(#17731,#17732,#17733,#17734));
#3778=EDGE_LOOP('',(#17735,#17736,#17737,#17738));
#3779=EDGE_LOOP('',(#17739,#17740,#17741,#17742));
#3780=EDGE_LOOP('',(#17743,#17744,#17745,#17746));
#3781=EDGE_LOOP('',(#17747,#17748,#17749,#17750));
#3782=EDGE_LOOP('',(#17751,#17752,#17753,#17754));
#3783=EDGE_LOOP('',(#17755,#17756,#17757,#17758));
#3784=EDGE_LOOP('',(#17759,#17760,#17761,#17762));
#3785=EDGE_LOOP('',(#17763,#17764,#17765,#17766));
#3786=EDGE_LOOP('',(#17767,#17768,#17769,#17770));
#3787=EDGE_LOOP('',(#17771,#17772,#17773,#17774));
#3788=EDGE_LOOP('',(#17775,#17776,#17777,#17778));
#3789=EDGE_LOOP('',(#17779,#17780,#17781,#17782));
#3790=EDGE_LOOP('',(#17783,#17784,#17785,#17786));
#3791=EDGE_LOOP('',(#17787,#17788,#17789,#17790));
#3792=EDGE_LOOP('',(#17791,#17792,#17793,#17794));
#3793=EDGE_LOOP('',(#17795,#17796,#17797,#17798));
#3794=EDGE_LOOP('',(#17799,#17800,#17801,#17802));
#3795=EDGE_LOOP('',(#17803,#17804,#17805,#17806));
#3796=EDGE_LOOP('',(#17807,#17808,#17809,#17810));
#3797=EDGE_LOOP('',(#17811,#17812,#17813,#17814));
#3798=EDGE_LOOP('',(#17815,#17816,#17817,#17818));
#3799=EDGE_LOOP('',(#17819,#17820,#17821,#17822));
#3800=EDGE_LOOP('',(#17823,#17824,#17825,#17826));
#3801=EDGE_LOOP('',(#17827,#17828,#17829,#17830));
#3802=EDGE_LOOP('',(#17831,#17832,#17833,#17834));
#3803=EDGE_LOOP('',(#17835,#17836,#17837,#17838));
#3804=EDGE_LOOP('',(#17839,#17840,#17841,#17842));
#3805=EDGE_LOOP('',(#17843,#17844,#17845,#17846));
#3806=EDGE_LOOP('',(#17847,#17848,#17849,#17850));
#3807=EDGE_LOOP('',(#17851,#17852,#17853,#17854));
#3808=EDGE_LOOP('',(#17855,#17856,#17857,#17858));
#3809=EDGE_LOOP('',(#17859,#17860,#17861,#17862));
#3810=EDGE_LOOP('',(#17863,#17864,#17865,#17866));
#3811=EDGE_LOOP('',(#17867,#17868,#17869,#17870));
#3812=EDGE_LOOP('',(#17871,#17872,#17873,#17874));
#3813=EDGE_LOOP('',(#17875,#17876,#17877,#17878,#17879,#17880,#17881,#17882,
#17883,#17884,#17885,#17886,#17887,#17888,#17889,#17890,#17891,#17892,#17893,
#17894));
#3814=EDGE_LOOP('',(#17895));
#3815=EDGE_LOOP('',(#17896));
#3816=EDGE_LOOP('',(#17897));
#3817=EDGE_LOOP('',(#17898));
#3818=EDGE_LOOP('',(#17899));
#3819=EDGE_LOOP('',(#17900));
#3820=EDGE_LOOP('',(#17901));
#3821=EDGE_LOOP('',(#17902));
#3822=EDGE_LOOP('',(#17903));
#3823=EDGE_LOOP('',(#17904,#17905,#17906,#17907));
#3824=EDGE_LOOP('',(#17908,#17909,#17910,#17911));
#3825=EDGE_LOOP('',(#17912,#17913,#17914,#17915));
#3826=EDGE_LOOP('',(#17916,#17917,#17918,#17919));
#3827=EDGE_LOOP('',(#17920,#17921,#17922,#17923,#17924,#17925,#17926,#17927,
#17928,#17929,#17930,#17931,#17932,#17933,#17934,#17935,#17936,#17937,#17938,
#17939,#17940,#17941,#17942,#17943));
#3828=EDGE_LOOP('',(#17944));
#3829=EDGE_LOOP('',(#17945));
#3830=EDGE_LOOP('',(#17946));
#3831=EDGE_LOOP('',(#17947));
#3832=EDGE_LOOP('',(#17948));
#3833=EDGE_LOOP('',(#17949));
#3834=EDGE_LOOP('',(#17950,#17951,#17952,#17953,#17954,#17955,#17956,#17957,
#17958,#17959,#17960,#17961,#17962,#17963,#17964,#17965));
#3835=EDGE_LOOP('',(#17966));
#3836=EDGE_LOOP('',(#17967));
#3837=EDGE_LOOP('',(#17968,#17969,#17970,#17971));
#3838=EDGE_LOOP('',(#17972,#17973,#17974,#17975));
#3839=EDGE_LOOP('',(#17976,#17977,#17978,#17979));
#3840=EDGE_LOOP('',(#17980,#17981,#17982,#17983));
#3841=EDGE_LOOP('',(#17984,#17985,#17986,#17987));
#3842=EDGE_LOOP('',(#17988,#17989,#17990,#17991));
#3843=EDGE_LOOP('',(#17992,#17993,#17994,#17995));
#3844=EDGE_LOOP('',(#17996,#17997,#17998,#17999));
#3845=EDGE_LOOP('',(#18000,#18001,#18002,#18003,#18004,#18005,#18006,#18007,
#18008,#18009,#18010,#18011,#18012,#18013,#18014,#18015,#18016,#18017,#18018,
#18019,#18020,#18021,#18022,#18023));
#3846=EDGE_LOOP('',(#18024));
#3847=EDGE_LOOP('',(#18025));
#3848=EDGE_LOOP('',(#18026,#18027,#18028,#18029,#18030,#18031,#18032,#18033,
#18034,#18035,#18036,#18037,#18038,#18039,#18040,#18041));
#3849=EDGE_LOOP('',(#18042));
#3850=EDGE_LOOP('',(#18043));
#3851=EDGE_LOOP('',(#18044));
#3852=EDGE_LOOP('',(#18045));
#3853=EDGE_LOOP('',(#18046));
#3854=EDGE_LOOP('',(#18047));
#3855=EDGE_LOOP('',(#18048,#18049,#18050,#18051));
#3856=EDGE_LOOP('',(#18052,#18053,#18054,#18055));
#3857=EDGE_LOOP('',(#18056,#18057,#18058,#18059));
#3858=EDGE_LOOP('',(#18060,#18061,#18062,#18063));
#3859=EDGE_LOOP('',(#18064,#18065,#18066,#18067));
#3860=EDGE_LOOP('',(#18068,#18069,#18070,#18071));
#3861=EDGE_LOOP('',(#18072,#18073,#18074,#18075));
#3862=EDGE_LOOP('',(#18076,#18077,#18078,#18079));
#3863=EDGE_LOOP('',(#18080,#18081,#18082,#18083));
#3864=EDGE_LOOP('',(#18084,#18085,#18086,#18087));
#3865=EDGE_LOOP('',(#18088,#18089,#18090,#18091));
#3866=EDGE_LOOP('',(#18092,#18093,#18094,#18095));
#3867=EDGE_LOOP('',(#18096,#18097,#18098,#18099));
#3868=EDGE_LOOP('',(#18100,#18101,#18102,#18103));
#3869=EDGE_LOOP('',(#18104,#18105,#18106,#18107));
#3870=EDGE_LOOP('',(#18108,#18109,#18110,#18111));
#3871=EDGE_LOOP('',(#18112,#18113,#18114,#18115));
#3872=EDGE_LOOP('',(#18116,#18117,#18118,#18119));
#3873=EDGE_LOOP('',(#18120,#18121,#18122,#18123));
#3874=EDGE_LOOP('',(#18124,#18125,#18126,#18127));
#3875=EDGE_LOOP('',(#18128,#18129,#18130,#18131));
#3876=EDGE_LOOP('',(#18132,#18133,#18134,#18135));
#3877=EDGE_LOOP('',(#18136,#18137,#18138,#18139));
#3878=EDGE_LOOP('',(#18140,#18141,#18142,#18143));
#3879=EDGE_LOOP('',(#18144,#18145,#18146,#18147));
#3880=EDGE_LOOP('',(#18148,#18149,#18150,#18151));
#3881=EDGE_LOOP('',(#18152,#18153,#18154,#18155));
#3882=EDGE_LOOP('',(#18156,#18157,#18158,#18159));
#3883=EDGE_LOOP('',(#18160,#18161,#18162,#18163));
#3884=EDGE_LOOP('',(#18164,#18165,#18166,#18167));
#3885=EDGE_LOOP('',(#18168,#18169,#18170,#18171));
#3886=EDGE_LOOP('',(#18172,#18173,#18174,#18175));
#3887=EDGE_LOOP('',(#18176,#18177,#18178,#18179));
#3888=EDGE_LOOP('',(#18180,#18181,#18182,#18183));
#3889=EDGE_LOOP('',(#18184,#18185,#18186,#18187));
#3890=EDGE_LOOP('',(#18188,#18189,#18190,#18191));
#3891=EDGE_LOOP('',(#18192,#18193,#18194,#18195));
#3892=EDGE_LOOP('',(#18196,#18197,#18198,#18199));
#3893=EDGE_LOOP('',(#18200,#18201,#18202,#18203));
#3894=EDGE_LOOP('',(#18204,#18205,#18206,#18207));
#3895=EDGE_LOOP('',(#18208,#18209,#18210,#18211));
#3896=EDGE_LOOP('',(#18212,#18213,#18214,#18215));
#3897=EDGE_LOOP('',(#18216,#18217,#18218,#18219));
#3898=EDGE_LOOP('',(#18220,#18221,#18222,#18223));
#3899=EDGE_LOOP('',(#18224,#18225,#18226,#18227));
#3900=EDGE_LOOP('',(#18228,#18229,#18230,#18231));
#3901=EDGE_LOOP('',(#18232,#18233,#18234,#18235));
#3902=EDGE_LOOP('',(#18236,#18237,#18238,#18239));
#3903=EDGE_LOOP('',(#18240,#18241,#18242,#18243));
#3904=EDGE_LOOP('',(#18244,#18245,#18246,#18247));
#3905=EDGE_LOOP('',(#18248,#18249,#18250,#18251));
#3906=EDGE_LOOP('',(#18252,#18253,#18254,#18255));
#3907=EDGE_LOOP('',(#18256,#18257,#18258,#18259));
#3908=EDGE_LOOP('',(#18260,#18261,#18262,#18263));
#3909=EDGE_LOOP('',(#18264,#18265,#18266,#18267));
#3910=EDGE_LOOP('',(#18268,#18269,#18270,#18271));
#3911=EDGE_LOOP('',(#18272,#18273,#18274,#18275));
#3912=EDGE_LOOP('',(#18276,#18277,#18278,#18279));
#3913=EDGE_LOOP('',(#18280,#18281,#18282,#18283));
#3914=EDGE_LOOP('',(#18284,#18285,#18286,#18287));
#3915=EDGE_LOOP('',(#18288,#18289,#18290,#18291));
#3916=EDGE_LOOP('',(#18292,#18293,#18294,#18295));
#3917=EDGE_LOOP('',(#18296,#18297,#18298,#18299));
#3918=EDGE_LOOP('',(#18300,#18301,#18302,#18303));
#3919=EDGE_LOOP('',(#18304,#18305,#18306,#18307));
#3920=EDGE_LOOP('',(#18308,#18309,#18310,#18311));
#3921=EDGE_LOOP('',(#18312,#18313,#18314,#18315));
#3922=EDGE_LOOP('',(#18316,#18317,#18318,#18319));
#3923=EDGE_LOOP('',(#18320,#18321,#18322,#18323));
#3924=EDGE_LOOP('',(#18324,#18325,#18326,#18327));
#3925=EDGE_LOOP('',(#18328,#18329,#18330,#18331));
#3926=EDGE_LOOP('',(#18332,#18333,#18334,#18335));
#3927=EDGE_LOOP('',(#18336,#18337,#18338,#18339));
#3928=EDGE_LOOP('',(#18340,#18341,#18342,#18343));
#3929=EDGE_LOOP('',(#18344,#18345,#18346,#18347));
#3930=EDGE_LOOP('',(#18348,#18349,#18350,#18351));
#3931=EDGE_LOOP('',(#18352,#18353,#18354,#18355));
#3932=EDGE_LOOP('',(#18356,#18357,#18358,#18359));
#3933=EDGE_LOOP('',(#18360,#18361,#18362,#18363));
#3934=EDGE_LOOP('',(#18364,#18365,#18366,#18367));
#3935=EDGE_LOOP('',(#18368,#18369,#18370,#18371));
#3936=EDGE_LOOP('',(#18372,#18373,#18374,#18375));
#3937=EDGE_LOOP('',(#18376,#18377,#18378,#18379));
#3938=EDGE_LOOP('',(#18380,#18381,#18382,#18383));
#3939=EDGE_LOOP('',(#18384,#18385,#18386,#18387));
#3940=EDGE_LOOP('',(#18388,#18389,#18390,#18391));
#3941=EDGE_LOOP('',(#18392,#18393,#18394,#18395));
#3942=EDGE_LOOP('',(#18396,#18397,#18398,#18399));
#3943=EDGE_LOOP('',(#18400));
#3944=EDGE_LOOP('',(#18401,#18402,#18403,#18404));
#3945=EDGE_LOOP('',(#18405,#18406,#18407,#18408));
#3946=EDGE_LOOP('',(#18409,#18410,#18411,#18412));
#3947=EDGE_LOOP('',(#18413,#18414,#18415,#18416));
#3948=EDGE_LOOP('',(#18417,#18418,#18419,#18420));
#3949=EDGE_LOOP('',(#18421,#18422,#18423,#18424));
#3950=EDGE_LOOP('',(#18425));
#3951=EDGE_LOOP('',(#18426));
#3952=EDGE_LOOP('',(#18427,#18428,#18429));
#3953=EDGE_LOOP('',(#18430,#18431,#18432,#18433));
#3954=EDGE_LOOP('',(#18434,#18435,#18436,#18437));
#3955=EDGE_LOOP('',(#18438,#18439,#18440,#18441));
#3956=EDGE_LOOP('',(#18442));
#3957=EDGE_LOOP('',(#18443));
#3958=EDGE_LOOP('',(#18444,#18445,#18446,#18447));
#3959=EDGE_LOOP('',(#18448,#18449,#18450,#18451));
#3960=EDGE_LOOP('',(#18452,#18453,#18454,#18455));
#3961=EDGE_LOOP('',(#18456,#18457,#18458,#18459));
#3962=EDGE_LOOP('',(#18460,#18461,#18462,#18463));
#3963=EDGE_LOOP('',(#18464,#18465,#18466,#18467));
#3964=EDGE_LOOP('',(#18468,#18469,#18470,#18471));
#3965=EDGE_LOOP('',(#18472,#18473,#18474,#18475,#18476,#18477,#18478,#18479));
#3966=EDGE_LOOP('',(#18480));
#3967=EDGE_LOOP('',(#18481,#18482,#18483,#18484,#18485,#18486,#18487,#18488));
#3968=EDGE_LOOP('',(#18489));
#3969=EDGE_LOOP('',(#18490));
#3970=EDGE_LOOP('',(#18491,#18492,#18493,#18494,#18495,#18496,#18497,#18498));
#3971=EDGE_LOOP('',(#18499));
#3972=EDGE_LOOP('',(#18500));
#3973=EDGE_LOOP('',(#18501,#18502,#18503,#18504,#18505,#18506,#18507,#18508));
#3974=EDGE_LOOP('',(#18509));
#3975=EDGE_LOOP('',(#18510));
#3976=EDGE_LOOP('',(#18511,#18512,#18513,#18514));
#3977=EDGE_LOOP('',(#18515,#18516,#18517,#18518));
#3978=EDGE_LOOP('',(#18519,#18520,#18521,#18522,#18523,#18524,#18525,#18526,
#18527,#18528));
#3979=EDGE_LOOP('',(#18529,#18530,#18531,#18532));
#3980=EDGE_LOOP('',(#18533,#18534,#18535,#18536));
#3981=EDGE_LOOP('',(#18537,#18538,#18539,#18540));
#3982=EDGE_LOOP('',(#18541,#18542,#18543,#18544,#18545,#18546,#18547,#18548,
#18549,#18550));
#3983=EDGE_LOOP('',(#18551,#18552,#18553,#18554));
#3984=EDGE_LOOP('',(#18555,#18556,#18557,#18558,#18559,#18560,#18561,#18562));
#3985=EDGE_LOOP('',(#18563));
#3986=EDGE_LOOP('',(#18564));
#3987=EDGE_LOOP('',(#18565,#18566,#18567,#18568));
#3988=EDGE_LOOP('',(#18569,#18570,#18571,#18572));
#3989=EDGE_LOOP('',(#18573,#18574,#18575,#18576,#18577));
#3990=EDGE_LOOP('',(#18578,#18579,#18580,#18581));
#3991=EDGE_LOOP('',(#18582,#18583,#18584,#18585,#18586));
#3992=EDGE_LOOP('',(#18587,#18588,#18589,#18590));
#3993=EDGE_LOOP('',(#18591));
#3994=EDGE_LOOP('',(#18592,#18593,#18594,#18595,#18596));
#3995=EDGE_LOOP('',(#18597,#18598,#18599,#18600));
#3996=EDGE_LOOP('',(#18601,#18602,#18603,#18604,#18605));
#3997=EDGE_LOOP('',(#18606,#18607,#18608,#18609));
#3998=EDGE_LOOP('',(#18610,#18611,#18612,#18613,#18614,#18615,#18616,#18617));
#3999=EDGE_LOOP('',(#18618,#18619,#18620,#18621));
#4000=EDGE_LOOP('',(#18622,#18623,#18624,#18625));
#4001=EDGE_LOOP('',(#18626,#18627,#18628,#18629));
#4002=EDGE_LOOP('',(#18630,#18631,#18632,#18633));
#4003=EDGE_LOOP('',(#18634,#18635,#18636,#18637));
#4004=EDGE_LOOP('',(#18638,#18639,#18640,#18641,#18642,#18643,#18644,#18645,
#18646,#18647,#18648,#18649,#18650,#18651,#18652,#18653,#18654,#18655,#18656,
#18657,#18658,#18659,#18660,#18661,#18662,#18663,#18664,#18665,#18666,#18667,
#18668,#18669,#18670,#18671,#18672,#18673,#18674,#18675,#18676,#18677,#18678,
#18679,#18680,#18681,#18682,#18683,#18684,#18685,#18686,#18687,#18688,#18689,
#18690,#18691,#18692,#18693,#18694,#18695,#18696,#18697,#18698,#18699,#18700,
#18701,#18702,#18703,#18704,#18705,#18706,#18707,#18708,#18709,#18710,#18711,
#18712,#18713,#18714,#18715,#18716,#18717,#18718,#18719,#18720,#18721,#18722,
#18723,#18724,#18725,#18726,#18727,#18728,#18729,#18730,#18731,#18732,#18733));
#4005=EDGE_LOOP('',(#18734));
#4006=EDGE_LOOP('',(#18735,#18736,#18737,#18738));
#4007=EDGE_LOOP('',(#18739,#18740,#18741,#18742));
#4008=EDGE_LOOP('',(#18743,#18744,#18745,#18746));
#4009=EDGE_LOOP('',(#18747,#18748,#18749,#18750));
#4010=EDGE_LOOP('',(#18751,#18752,#18753,#18754));
#4011=EDGE_LOOP('',(#18755,#18756,#18757,#18758));
#4012=EDGE_LOOP('',(#18759,#18760,#18761,#18762));
#4013=EDGE_LOOP('',(#18763,#18764,#18765,#18766));
#4014=EDGE_LOOP('',(#18767,#18768,#18769,#18770));
#4015=EDGE_LOOP('',(#18771,#18772,#18773,#18774));
#4016=EDGE_LOOP('',(#18775,#18776,#18777,#18778));
#4017=EDGE_LOOP('',(#18779,#18780,#18781,#18782));
#4018=EDGE_LOOP('',(#18783,#18784,#18785,#18786));
#4019=EDGE_LOOP('',(#18787,#18788,#18789,#18790));
#4020=EDGE_LOOP('',(#18791,#18792,#18793,#18794));
#4021=EDGE_LOOP('',(#18795,#18796,#18797,#18798));
#4022=EDGE_LOOP('',(#18799,#18800,#18801,#18802));
#4023=EDGE_LOOP('',(#18803,#18804,#18805,#18806));
#4024=EDGE_LOOP('',(#18807,#18808,#18809,#18810));
#4025=EDGE_LOOP('',(#18811,#18812,#18813,#18814));
#4026=EDGE_LOOP('',(#18815,#18816,#18817,#18818));
#4027=EDGE_LOOP('',(#18819,#18820,#18821,#18822));
#4028=EDGE_LOOP('',(#18823,#18824,#18825,#18826));
#4029=EDGE_LOOP('',(#18827,#18828,#18829,#18830));
#4030=EDGE_LOOP('',(#18831,#18832,#18833,#18834));
#4031=EDGE_LOOP('',(#18835,#18836,#18837,#18838));
#4032=EDGE_LOOP('',(#18839,#18840,#18841,#18842));
#4033=EDGE_LOOP('',(#18843,#18844,#18845,#18846));
#4034=EDGE_LOOP('',(#18847,#18848,#18849,#18850));
#4035=EDGE_LOOP('',(#18851,#18852,#18853,#18854));
#4036=EDGE_LOOP('',(#18855,#18856,#18857,#18858));
#4037=EDGE_LOOP('',(#18859,#18860,#18861,#18862));
#4038=EDGE_LOOP('',(#18863,#18864,#18865,#18866));
#4039=EDGE_LOOP('',(#18867,#18868,#18869,#18870));
#4040=EDGE_LOOP('',(#18871,#18872,#18873,#18874));
#4041=EDGE_LOOP('',(#18875,#18876,#18877,#18878));
#4042=EDGE_LOOP('',(#18879,#18880,#18881,#18882));
#4043=EDGE_LOOP('',(#18883,#18884,#18885,#18886));
#4044=EDGE_LOOP('',(#18887,#18888,#18889,#18890));
#4045=EDGE_LOOP('',(#18891,#18892,#18893,#18894));
#4046=EDGE_LOOP('',(#18895,#18896,#18897,#18898));
#4047=EDGE_LOOP('',(#18899,#18900,#18901,#18902));
#4048=EDGE_LOOP('',(#18903,#18904,#18905,#18906));
#4049=EDGE_LOOP('',(#18907,#18908,#18909,#18910));
#4050=EDGE_LOOP('',(#18911,#18912,#18913,#18914));
#4051=EDGE_LOOP('',(#18915,#18916,#18917,#18918));
#4052=EDGE_LOOP('',(#18919,#18920,#18921,#18922));
#4053=EDGE_LOOP('',(#18923,#18924,#18925,#18926));
#4054=EDGE_LOOP('',(#18927,#18928,#18929,#18930));
#4055=EDGE_LOOP('',(#18931,#18932,#18933,#18934));
#4056=EDGE_LOOP('',(#18935,#18936,#18937,#18938));
#4057=EDGE_LOOP('',(#18939,#18940,#18941,#18942));
#4058=EDGE_LOOP('',(#18943,#18944,#18945,#18946));
#4059=EDGE_LOOP('',(#18947,#18948,#18949,#18950));
#4060=EDGE_LOOP('',(#18951,#18952,#18953,#18954));
#4061=EDGE_LOOP('',(#18955,#18956,#18957,#18958));
#4062=EDGE_LOOP('',(#18959,#18960,#18961,#18962));
#4063=EDGE_LOOP('',(#18963,#18964,#18965,#18966));
#4064=EDGE_LOOP('',(#18967,#18968,#18969,#18970));
#4065=EDGE_LOOP('',(#18971,#18972,#18973,#18974));
#4066=EDGE_LOOP('',(#18975,#18976,#18977,#18978));
#4067=EDGE_LOOP('',(#18979,#18980,#18981,#18982));
#4068=EDGE_LOOP('',(#18983,#18984,#18985,#18986));
#4069=EDGE_LOOP('',(#18987,#18988,#18989,#18990));
#4070=EDGE_LOOP('',(#18991,#18992,#18993,#18994));
#4071=EDGE_LOOP('',(#18995,#18996,#18997,#18998));
#4072=EDGE_LOOP('',(#18999,#19000,#19001,#19002));
#4073=EDGE_LOOP('',(#19003,#19004,#19005,#19006));
#4074=EDGE_LOOP('',(#19007,#19008,#19009,#19010));
#4075=EDGE_LOOP('',(#19011,#19012,#19013,#19014));
#4076=EDGE_LOOP('',(#19015,#19016,#19017,#19018));
#4077=EDGE_LOOP('',(#19019,#19020,#19021,#19022));
#4078=EDGE_LOOP('',(#19023,#19024,#19025,#19026));
#4079=EDGE_LOOP('',(#19027,#19028,#19029,#19030));
#4080=EDGE_LOOP('',(#19031,#19032,#19033,#19034));
#4081=EDGE_LOOP('',(#19035,#19036,#19037,#19038));
#4082=EDGE_LOOP('',(#19039,#19040,#19041,#19042));
#4083=EDGE_LOOP('',(#19043,#19044,#19045,#19046));
#4084=EDGE_LOOP('',(#19047,#19048,#19049,#19050));
#4085=EDGE_LOOP('',(#19051,#19052,#19053,#19054));
#4086=EDGE_LOOP('',(#19055,#19056,#19057,#19058));
#4087=EDGE_LOOP('',(#19059,#19060,#19061,#19062));
#4088=EDGE_LOOP('',(#19063,#19064,#19065,#19066));
#4089=EDGE_LOOP('',(#19067,#19068,#19069,#19070));
#4090=EDGE_LOOP('',(#19071,#19072,#19073,#19074,#19075,#19076,#19077,#19078,
#19079,#19080,#19081,#19082,#19083,#19084,#19085,#19086,#19087,#19088,#19089,
#19090,#19091,#19092,#19093,#19094,#19095,#19096,#19097,#19098,#19099,#19100,
#19101,#19102,#19103,#19104,#19105,#19106,#19107,#19108,#19109,#19110,#19111,
#19112,#19113,#19114,#19115,#19116,#19117,#19118,#19119,#19120,#19121,#19122,
#19123,#19124,#19125,#19126,#19127,#19128,#19129,#19130,#19131,#19132,#19133,
#19134,#19135,#19136,#19137,#19138,#19139,#19140,#19141,#19142,#19143,#19144,
#19145,#19146,#19147,#19148,#19149,#19150,#19151,#19152,#19153,#19154,#19155,
#19156,#19157,#19158,#19159,#19160,#19161,#19162,#19163,#19164,#19165,#19166));
#4091=EDGE_LOOP('',(#19167));
#4092=EDGE_LOOP('',(#19168,#19169,#19170,#19171));
#4093=EDGE_LOOP('',(#19172,#19173,#19174,#19175));
#4094=EDGE_LOOP('',(#19176,#19177,#19178,#19179));
#4095=EDGE_LOOP('',(#19180,#19181,#19182,#19183));
#4096=EDGE_LOOP('',(#19184,#19185,#19186,#19187));
#4097=EDGE_LOOP('',(#19188,#19189,#19190,#19191));
#4098=EDGE_LOOP('',(#19192,#19193,#19194,#19195));
#4099=EDGE_LOOP('',(#19196));
#4100=EDGE_LOOP('',(#19197));
#4101=EDGE_LOOP('',(#19198,#19199,#19200,#19201));
#4102=EDGE_LOOP('',(#19202));
#4103=EDGE_LOOP('',(#19203));
#4104=EDGE_LOOP('',(#19204,#19205,#19206,#19207));
#4105=EDGE_LOOP('',(#19208,#19209,#19210,#19211));
#4106=EDGE_LOOP('',(#19212,#19213,#19214,#19215));
#4107=EDGE_LOOP('',(#19216,#19217,#19218,#19219,#19220,#19221));
#4108=EDGE_LOOP('',(#19222,#19223,#19224,#19225,#19226));
#4109=EDGE_LOOP('',(#19227,#19228,#19229,#19230,#19231,#19232));
#4110=EDGE_LOOP('',(#19233,#19234,#19235,#19236));
#4111=EDGE_LOOP('',(#19237,#19238,#19239,#19240,#19241,#19242));
#4112=EDGE_LOOP('',(#19243,#19244,#19245,#19246));
#4113=EDGE_LOOP('',(#19247,#19248,#19249,#19250,#19251,#19252));
#4114=EDGE_LOOP('',(#19253,#19254,#19255,#19256,#19257));
#4115=EDGE_LOOP('',(#19258,#19259,#19260,#19261,#19262));
#4116=EDGE_LOOP('',(#19263,#19264,#19265,#19266,#19267,#19268));
#4117=EDGE_LOOP('',(#19269,#19270,#19271,#19272));
#4118=EDGE_LOOP('',(#19273,#19274,#19275,#19276));
#4119=EDGE_LOOP('',(#19277,#19278,#19279,#19280));
#4120=EDGE_LOOP('',(#19281,#19282,#19283,#19284));
#4121=EDGE_LOOP('',(#19285,#19286,#19287,#19288));
#4122=EDGE_LOOP('',(#19289,#19290,#19291,#19292));
#4123=EDGE_LOOP('',(#19293,#19294,#19295,#19296));
#4124=EDGE_LOOP('',(#19297,#19298,#19299,#19300));
#4125=EDGE_LOOP('',(#19301,#19302,#19303,#19304));
#4126=EDGE_LOOP('',(#19305,#19306,#19307,#19308));
#4127=EDGE_LOOP('',(#19309,#19310,#19311,#19312));
#4128=EDGE_LOOP('',(#19313,#19314,#19315,#19316));
#4129=EDGE_LOOP('',(#19317,#19318,#19319,#19320,#19321,#19322));
#4130=EDGE_LOOP('',(#19323,#19324,#19325,#19326,#19327));
#4131=EDGE_LOOP('',(#19328,#19329,#19330,#19331,#19332,#19333,#19334,#19335,
#19336,#19337,#19338,#19339,#19340,#19341,#19342,#19343,#19344,#19345,#19346,
#19347,#19348,#19349,#19350,#19351,#19352,#19353,#19354,#19355,#19356,#19357,
#19358,#19359,#19360,#19361,#19362));
#4132=EDGE_LOOP('',(#19363,#19364,#19365,#19366,#19367));
#4133=EDGE_LOOP('',(#19368,#19369,#19370,#19371,#19372,#19373,#19374,#19375,
#19376,#19377,#19378,#19379,#19380,#19381,#19382,#19383,#19384,#19385,#19386,
#19387,#19388,#19389,#19390,#19391,#19392,#19393,#19394,#19395,#19396,#19397,
#19398,#19399,#19400,#19401));
#4134=EDGE_LOOP('',(#19402,#19403,#19404,#19405,#19406,#19407,#19408));
#4135=EDGE_LOOP('',(#19409));
#4136=EDGE_LOOP('',(#19410));
#4137=EDGE_LOOP('',(#19411,#19412,#19413,#19414,#19415,#19416,#19417));
#4138=EDGE_LOOP('',(#19418));
#4139=EDGE_LOOP('',(#19419,#19420,#19421,#19422));
#4140=EDGE_LOOP('',(#19423,#19424,#19425));
#4141=EDGE_LOOP('',(#19426,#19427,#19428,#19429));
#4142=EDGE_LOOP('',(#19430,#19431,#19432,#19433,#19434,#19435,#19436,#19437,
#19438,#19439,#19440,#19441,#19442,#19443,#19444,#19445,#19446,#19447,#19448,
#19449,#19450,#19451,#19452,#19453,#19454,#19455,#19456,#19457,#19458,#19459,
#19460,#19461,#19462,#19463,#19464,#19465,#19466,#19467,#19468,#19469,#19470,
#19471,#19472,#19473,#19474,#19475,#19476,#19477,#19478,#19479,#19480,#19481,
#19482,#19483,#19484,#19485,#19486,#19487,#19488,#19489,#19490,#19491,#19492,
#19493,#19494,#19495,#19496,#19497,#19498,#19499,#19500,#19501,#19502,#19503,
#19504,#19505,#19506,#19507,#19508,#19509,#19510,#19511,#19512,#19513,#19514,
#19515,#19516,#19517,#19518,#19519,#19520,#19521,#19522,#19523,#19524,#19525,
#19526,#19527,#19528,#19529,#19530,#19531,#19532,#19533,#19534,#19535,#19536,
#19537,#19538,#19539,#19540,#19541,#19542,#19543,#19544,#19545,#19546,#19547,
#19548,#19549,#19550,#19551,#19552,#19553,#19554,#19555,#19556,#19557,#19558,
#19559,#19560,#19561,#19562,#19563,#19564,#19565,#19566,#19567,#19568,#19569,
#19570,#19571,#19572,#19573,#19574,#19575,#19576,#19577,#19578));
#4143=EDGE_LOOP('',(#19579,#19580,#19581,#19582));
#4144=EDGE_LOOP('',(#19583,#19584,#19585));
#4145=EDGE_LOOP('',(#19586,#19587,#19588,#19589));
#4146=EDGE_LOOP('',(#19590,#19591,#19592,#19593));
#4147=EDGE_LOOP('',(#19594,#19595,#19596));
#4148=EDGE_LOOP('',(#19597,#19598,#19599,#19600));
#4149=EDGE_LOOP('',(#19601,#19602,#19603,#19604));
#4150=EDGE_LOOP('',(#19605,#19606,#19607));
#4151=EDGE_LOOP('',(#19608,#19609,#19610,#19611));
#4152=EDGE_LOOP('',(#19612,#19613,#19614,#19615));
#4153=EDGE_LOOP('',(#19616,#19617,#19618));
#4154=EDGE_LOOP('',(#19619,#19620,#19621,#19622));
#4155=EDGE_LOOP('',(#19623,#19624,#19625,#19626));
#4156=EDGE_LOOP('',(#19627,#19628,#19629));
#4157=EDGE_LOOP('',(#19630,#19631,#19632,#19633));
#4158=EDGE_LOOP('',(#19634,#19635,#19636,#19637));
#4159=EDGE_LOOP('',(#19638,#19639,#19640));
#4160=EDGE_LOOP('',(#19641,#19642,#19643,#19644));
#4161=EDGE_LOOP('',(#19645,#19646,#19647,#19648));
#4162=EDGE_LOOP('',(#19649,#19650,#19651));
#4163=EDGE_LOOP('',(#19652,#19653,#19654,#19655));
#4164=EDGE_LOOP('',(#19656,#19657,#19658,#19659));
#4165=EDGE_LOOP('',(#19660,#19661,#19662));
#4166=EDGE_LOOP('',(#19663,#19664,#19665,#19666));
#4167=EDGE_LOOP('',(#19667,#19668,#19669,#19670));
#4168=EDGE_LOOP('',(#19671,#19672,#19673));
#4169=EDGE_LOOP('',(#19674,#19675,#19676,#19677));
#4170=EDGE_LOOP('',(#19678,#19679,#19680,#19681));
#4171=EDGE_LOOP('',(#19682,#19683,#19684));
#4172=EDGE_LOOP('',(#19685,#19686,#19687,#19688));
#4173=EDGE_LOOP('',(#19689,#19690,#19691,#19692));
#4174=EDGE_LOOP('',(#19693,#19694,#19695));
#4175=EDGE_LOOP('',(#19696,#19697,#19698,#19699));
#4176=EDGE_LOOP('',(#19700,#19701,#19702,#19703));
#4177=EDGE_LOOP('',(#19704,#19705,#19706));
#4178=EDGE_LOOP('',(#19707,#19708,#19709,#19710));
#4179=EDGE_LOOP('',(#19711,#19712,#19713,#19714));
#4180=EDGE_LOOP('',(#19715,#19716,#19717));
#4181=EDGE_LOOP('',(#19718,#19719,#19720,#19721));
#4182=EDGE_LOOP('',(#19722,#19723,#19724,#19725));
#4183=EDGE_LOOP('',(#19726,#19727,#19728));
#4184=EDGE_LOOP('',(#19729,#19730,#19731,#19732));
#4185=EDGE_LOOP('',(#19733,#19734,#19735,#19736));
#4186=EDGE_LOOP('',(#19737,#19738,#19739));
#4187=EDGE_LOOP('',(#19740,#19741,#19742,#19743));
#4188=EDGE_LOOP('',(#19744,#19745,#19746,#19747));
#4189=EDGE_LOOP('',(#19748,#19749,#19750));
#4190=EDGE_LOOP('',(#19751,#19752,#19753,#19754));
#4191=EDGE_LOOP('',(#19755,#19756,#19757,#19758));
#4192=EDGE_LOOP('',(#19759,#19760,#19761,#19762));
#4193=EDGE_LOOP('',(#19763,#19764,#19765,#19766));
#4194=EDGE_LOOP('',(#19767,#19768,#19769,#19770));
#4195=EDGE_LOOP('',(#19771,#19772,#19773));
#4196=EDGE_LOOP('',(#19774,#19775,#19776,#19777));
#4197=EDGE_LOOP('',(#19778,#19779,#19780,#19781));
#4198=EDGE_LOOP('',(#19782,#19783,#19784));
#4199=EDGE_LOOP('',(#19785,#19786,#19787,#19788));
#4200=EDGE_LOOP('',(#19789,#19790,#19791,#19792));
#4201=EDGE_LOOP('',(#19793,#19794,#19795));
#4202=EDGE_LOOP('',(#19796,#19797,#19798,#19799));
#4203=EDGE_LOOP('',(#19800,#19801,#19802,#19803));
#4204=EDGE_LOOP('',(#19804,#19805,#19806));
#4205=EDGE_LOOP('',(#19807,#19808,#19809,#19810));
#4206=EDGE_LOOP('',(#19811,#19812,#19813,#19814));
#4207=EDGE_LOOP('',(#19815,#19816,#19817));
#4208=EDGE_LOOP('',(#19818,#19819,#19820,#19821));
#4209=EDGE_LOOP('',(#19822,#19823,#19824,#19825));
#4210=EDGE_LOOP('',(#19826,#19827,#19828));
#4211=EDGE_LOOP('',(#19829,#19830,#19831,#19832));
#4212=EDGE_LOOP('',(#19833,#19834,#19835,#19836));
#4213=EDGE_LOOP('',(#19837,#19838,#19839));
#4214=EDGE_LOOP('',(#19840,#19841,#19842,#19843));
#4215=EDGE_LOOP('',(#19844,#19845,#19846,#19847));
#4216=EDGE_LOOP('',(#19848,#19849,#19850));
#4217=EDGE_LOOP('',(#19851,#19852,#19853,#19854));
#4218=EDGE_LOOP('',(#19855,#19856,#19857,#19858));
#4219=EDGE_LOOP('',(#19859,#19860,#19861));
#4220=EDGE_LOOP('',(#19862,#19863,#19864,#19865));
#4221=EDGE_LOOP('',(#19866,#19867,#19868,#19869));
#4222=EDGE_LOOP('',(#19870,#19871,#19872));
#4223=EDGE_LOOP('',(#19873,#19874,#19875,#19876));
#4224=EDGE_LOOP('',(#19877,#19878,#19879,#19880));
#4225=EDGE_LOOP('',(#19881,#19882,#19883));
#4226=EDGE_LOOP('',(#19884,#19885,#19886,#19887));
#4227=EDGE_LOOP('',(#19888,#19889,#19890,#19891));
#4228=EDGE_LOOP('',(#19892,#19893,#19894));
#4229=EDGE_LOOP('',(#19895,#19896,#19897,#19898));
#4230=EDGE_LOOP('',(#19899,#19900,#19901,#19902));
#4231=EDGE_LOOP('',(#19903,#19904,#19905));
#4232=EDGE_LOOP('',(#19906,#19907,#19908,#19909));
#4233=EDGE_LOOP('',(#19910,#19911,#19912,#19913));
#4234=EDGE_LOOP('',(#19914,#19915,#19916));
#4235=EDGE_LOOP('',(#19917,#19918,#19919,#19920));
#4236=EDGE_LOOP('',(#19921,#19922,#19923,#19924));
#4237=EDGE_LOOP('',(#19925,#19926,#19927));
#4238=EDGE_LOOP('',(#19928,#19929,#19930,#19931));
#4239=EDGE_LOOP('',(#19932,#19933,#19934,#19935));
#4240=EDGE_LOOP('',(#19936,#19937,#19938));
#4241=EDGE_LOOP('',(#19939,#19940,#19941,#19942));
#4242=EDGE_LOOP('',(#19943,#19944,#19945,#19946));
#4243=EDGE_LOOP('',(#19947,#19948,#19949));
#4244=EDGE_LOOP('',(#19950,#19951,#19952,#19953));
#4245=EDGE_LOOP('',(#19954,#19955,#19956,#19957));
#4246=EDGE_LOOP('',(#19958,#19959,#19960));
#4247=EDGE_LOOP('',(#19961,#19962,#19963,#19964));
#4248=EDGE_LOOP('',(#19965,#19966,#19967,#19968,#19969));
#4249=EDGE_LOOP('',(#19970,#19971,#19972,#19973,#19974,#19975,#19976,#19977,
#19978,#19979,#19980,#19981,#19982,#19983,#19984,#19985,#19986,#19987,#19988,
#19989,#19990,#19991,#19992,#19993,#19994,#19995,#19996,#19997,#19998,#19999,
#20000,#20001,#20002,#20003,#20004,#20005,#20006,#20007,#20008,#20009,#20010,
#20011,#20012,#20013,#20014,#20015,#20016,#20017,#20018,#20019,#20020,#20021,
#20022,#20023,#20024,#20025,#20026,#20027,#20028,#20029,#20030,#20031,#20032,
#20033,#20034,#20035,#20036,#20037,#20038,#20039,#20040,#20041,#20042,#20043,
#20044,#20045,#20046,#20047,#20048,#20049,#20050,#20051,#20052,#20053,#20054,
#20055,#20056,#20057,#20058,#20059,#20060,#20061,#20062,#20063,#20064,#20065,
#20066,#20067,#20068,#20069,#20070,#20071,#20072,#20073,#20074,#20075,#20076,
#20077,#20078,#20079,#20080));
#4250=EDGE_LOOP('',(#20081));
#4251=EDGE_LOOP('',(#20082));
#4252=EDGE_LOOP('',(#20083,#20084,#20085,#20086,#20087,#20088,#20089,#20090,
#20091,#20092,#20093,#20094,#20095,#20096,#20097,#20098,#20099,#20100,#20101,
#20102,#20103));
#4253=EDGE_LOOP('',(#20104,#20105,#20106,#20107));
#4254=EDGE_LOOP('',(#20108,#20109,#20110,#20111));
#4255=EDGE_LOOP('',(#20112,#20113,#20114,#20115));
#4256=EDGE_LOOP('',(#20116,#20117,#20118,#20119));
#4257=EDGE_LOOP('',(#20120,#20121,#20122,#20123));
#4258=EDGE_LOOP('',(#20124,#20125,#20126,#20127));
#4259=EDGE_LOOP('',(#20128,#20129,#20130,#20131,#20132,#20133,#20134,#20135));
#4260=EDGE_LOOP('',(#20136,#20137,#20138,#20139,#20140,#20141,#20142,#20143));
#4261=EDGE_LOOP('',(#20144,#20145,#20146,#20147,#20148,#20149,#20150,#20151));
#4262=EDGE_LOOP('',(#20152,#20153));
#4263=EDGE_LOOP('',(#20154,#20155));
#4264=EDGE_LOOP('',(#20156,#20157));
#4265=EDGE_LOOP('',(#20158,#20159));
#4266=EDGE_LOOP('',(#20160,#20161));
#4267=EDGE_LOOP('',(#20162,#20163));
#4268=EDGE_LOOP('',(#20164,#20165));
#4269=EDGE_LOOP('',(#20166,#20167));
#4270=EDGE_LOOP('',(#20168,#20169));
#4271=EDGE_LOOP('',(#20170,#20171));
#4272=EDGE_LOOP('',(#20172,#20173));
#4273=EDGE_LOOP('',(#20174,#20175));
#4274=EDGE_LOOP('',(#20176,#20177,#20178,#20179,#20180,#20181,#20182,#20183));
#4275=EDGE_LOOP('',(#20184,#20185,#20186,#20187,#20188,#20189,#20190,#20191));
#4276=EDGE_LOOP('',(#20192,#20193,#20194,#20195,#20196,#20197,#20198,#20199));
#4277=EDGE_LOOP('',(#20200,#20201,#20202,#20203,#20204,#20205,#20206,#20207));
#4278=EDGE_LOOP('',(#20208,#20209,#20210,#20211));
#4279=EDGE_LOOP('',(#20212,#20213,#20214,#20215));
#4280=EDGE_LOOP('',(#20216));
#4281=EDGE_LOOP('',(#20217));
#4282=EDGE_LOOP('',(#20218));
#4283=EDGE_LOOP('',(#20219));
#4284=EDGE_LOOP('',(#20220));
#4285=EDGE_LOOP('',(#20221));
#4286=EDGE_LOOP('',(#20222));
#4287=EDGE_LOOP('',(#20223));
#4288=EDGE_LOOP('',(#20224));
#4289=EDGE_LOOP('',(#20225));
#4290=EDGE_LOOP('',(#20226));
#4291=EDGE_LOOP('',(#20227));
#4292=EDGE_LOOP('',(#20228));
#4293=EDGE_LOOP('',(#20229));
#4294=EDGE_LOOP('',(#20230));
#4295=EDGE_LOOP('',(#20231));
#4296=EDGE_LOOP('',(#20232));
#4297=EDGE_LOOP('',(#20233));
#4298=EDGE_LOOP('',(#20234));
#4299=EDGE_LOOP('',(#20235));
#4300=EDGE_LOOP('',(#20236));
#4301=EDGE_LOOP('',(#20237,#20238,#20239,#20240));
#4302=EDGE_LOOP('',(#20241,#20242,#20243,#20244));
#4303=EDGE_LOOP('',(#20245,#20246,#20247,#20248));
#4304=EDGE_LOOP('',(#20249,#20250,#20251,#20252));
#4305=EDGE_LOOP('',(#20253,#20254,#20255,#20256));
#4306=EDGE_LOOP('',(#20257,#20258,#20259,#20260));
#4307=EDGE_LOOP('',(#20261,#20262,#20263,#20264));
#4308=EDGE_LOOP('',(#20265,#20266,#20267,#20268));
#4309=EDGE_LOOP('',(#20269,#20270,#20271,#20272));
#4310=EDGE_LOOP('',(#20273,#20274,#20275,#20276));
#4311=EDGE_LOOP('',(#20277,#20278,#20279,#20280));
#4312=EDGE_LOOP('',(#20281,#20282,#20283,#20284));
#4313=EDGE_LOOP('',(#20285,#20286,#20287,#20288));
#4314=EDGE_LOOP('',(#20289,#20290,#20291,#20292));
#4315=EDGE_LOOP('',(#20293,#20294,#20295,#20296));
#4316=EDGE_LOOP('',(#20297,#20298,#20299,#20300));
#4317=EDGE_LOOP('',(#20301,#20302,#20303,#20304));
#4318=EDGE_LOOP('',(#20305,#20306,#20307,#20308));
#4319=EDGE_LOOP('',(#20309,#20310,#20311,#20312));
#4320=EDGE_LOOP('',(#20313,#20314,#20315,#20316));
#4321=EDGE_LOOP('',(#20317,#20318,#20319,#20320));
#4322=EDGE_LOOP('',(#20321,#20322,#20323,#20324));
#4323=EDGE_LOOP('',(#20325,#20326,#20327,#20328));
#4324=EDGE_LOOP('',(#20329,#20330,#20331,#20332));
#4325=EDGE_LOOP('',(#20333,#20334,#20335,#20336));
#4326=EDGE_LOOP('',(#20337,#20338,#20339,#20340));
#4327=EDGE_LOOP('',(#20341,#20342,#20343,#20344));
#4328=EDGE_LOOP('',(#20345,#20346,#20347,#20348));
#4329=EDGE_LOOP('',(#20349,#20350,#20351,#20352));
#4330=EDGE_LOOP('',(#20353,#20354,#20355,#20356));
#4331=EDGE_LOOP('',(#20357,#20358,#20359,#20360));
#4332=EDGE_LOOP('',(#20361,#20362,#20363,#20364));
#4333=EDGE_LOOP('',(#20365,#20366,#20367,#20368));
#4334=EDGE_LOOP('',(#20369,#20370,#20371,#20372));
#4335=EDGE_LOOP('',(#20373,#20374,#20375,#20376));
#4336=EDGE_LOOP('',(#20377,#20378,#20379,#20380));
#4337=EDGE_LOOP('',(#20381,#20382,#20383,#20384));
#4338=EDGE_LOOP('',(#20385,#20386,#20387,#20388));
#4339=EDGE_LOOP('',(#20389,#20390,#20391,#20392));
#4340=EDGE_LOOP('',(#20393,#20394,#20395,#20396));
#4341=EDGE_LOOP('',(#20397,#20398,#20399,#20400));
#4342=EDGE_LOOP('',(#20401,#20402,#20403,#20404));
#4343=EDGE_LOOP('',(#20405,#20406,#20407,#20408));
#4344=EDGE_LOOP('',(#20409,#20410,#20411,#20412));
#4345=EDGE_LOOP('',(#20413,#20414,#20415,#20416));
#4346=EDGE_LOOP('',(#20417,#20418,#20419,#20420));
#4347=EDGE_LOOP('',(#20421,#20422,#20423,#20424));
#4348=EDGE_LOOP('',(#20425,#20426,#20427,#20428));
#4349=EDGE_LOOP('',(#20429,#20430,#20431,#20432));
#4350=EDGE_LOOP('',(#20433,#20434,#20435,#20436));
#4351=EDGE_LOOP('',(#20437,#20438,#20439,#20440));
#4352=EDGE_LOOP('',(#20441,#20442,#20443,#20444));
#4353=EDGE_LOOP('',(#20445,#20446,#20447,#20448));
#4354=EDGE_LOOP('',(#20449));
#4355=EDGE_LOOP('',(#20450));
#4356=EDGE_LOOP('',(#20451));
#4357=EDGE_LOOP('',(#20452));
#4358=EDGE_LOOP('',(#20453));
#4359=EDGE_LOOP('',(#20454));
#4360=EDGE_LOOP('',(#20455));
#4361=EDGE_LOOP('',(#20456));
#4362=EDGE_LOOP('',(#20457));
#4363=EDGE_LOOP('',(#20458));
#4364=EDGE_LOOP('',(#20459));
#4365=EDGE_LOOP('',(#20460));
#4366=EDGE_LOOP('',(#20461));
#4367=EDGE_LOOP('',(#20462));
#4368=EDGE_LOOP('',(#20463));
#4369=EDGE_LOOP('',(#20464));
#4370=EDGE_LOOP('',(#20465));
#4371=EDGE_LOOP('',(#20466));
#4372=EDGE_LOOP('',(#20467));
#4373=EDGE_LOOP('',(#20468));
#4374=EDGE_LOOP('',(#20469));
#4375=EDGE_LOOP('',(#20470,#20471,#20472,#20473));
#4376=EDGE_LOOP('',(#20474,#20475,#20476,#20477));
#4377=EDGE_LOOP('',(#20478,#20479,#20480,#20481));
#4378=EDGE_LOOP('',(#20482,#20483,#20484,#20485));
#4379=EDGE_LOOP('',(#20486,#20487,#20488,#20489));
#4380=EDGE_LOOP('',(#20490,#20491,#20492,#20493));
#4381=EDGE_LOOP('',(#20494,#20495,#20496,#20497));
#4382=EDGE_LOOP('',(#20498,#20499,#20500,#20501));
#4383=EDGE_LOOP('',(#20502,#20503,#20504,#20505));
#4384=EDGE_LOOP('',(#20506,#20507,#20508,#20509));
#4385=EDGE_LOOP('',(#20510,#20511,#20512,#20513));
#4386=EDGE_LOOP('',(#20514,#20515,#20516,#20517));
#4387=EDGE_LOOP('',(#20518,#20519,#20520,#20521));
#4388=EDGE_LOOP('',(#20522,#20523,#20524,#20525));
#4389=EDGE_LOOP('',(#20526,#20527,#20528,#20529));
#4390=EDGE_LOOP('',(#20530,#20531,#20532,#20533));
#4391=EDGE_LOOP('',(#20534,#20535,#20536,#20537));
#4392=EDGE_LOOP('',(#20538,#20539,#20540,#20541));
#4393=EDGE_LOOP('',(#20542,#20543,#20544,#20545));
#4394=EDGE_LOOP('',(#20546,#20547,#20548,#20549));
#4395=EDGE_LOOP('',(#20550,#20551,#20552,#20553));
#4396=EDGE_LOOP('',(#20554,#20555,#20556,#20557));
#4397=EDGE_LOOP('',(#20558,#20559,#20560,#20561));
#4398=EDGE_LOOP('',(#20562,#20563,#20564,#20565));
#4399=EDGE_LOOP('',(#20566,#20567,#20568,#20569));
#4400=EDGE_LOOP('',(#20570,#20571,#20572,#20573));
#4401=EDGE_LOOP('',(#20574,#20575,#20576,#20577,#20578,#20579));
#4402=EDGE_LOOP('',(#20580,#20581,#20582,#20583));
#4403=EDGE_LOOP('',(#20584,#20585,#20586,#20587));
#4404=EDGE_LOOP('',(#20588,#20589,#20590,#20591));
#4405=EDGE_LOOP('',(#20592,#20593,#20594,#20595));
#4406=EDGE_LOOP('',(#20596,#20597,#20598,#20599));
#4407=EDGE_LOOP('',(#20600,#20601,#20602,#20603));
#4408=EDGE_LOOP('',(#20604,#20605,#20606,#20607));
#4409=EDGE_LOOP('',(#20608,#20609,#20610,#20611));
#4410=EDGE_LOOP('',(#20612,#20613,#20614,#20615));
#4411=EDGE_LOOP('',(#20616,#20617,#20618,#20619));
#4412=EDGE_LOOP('',(#20620,#20621,#20622,#20623));
#4413=EDGE_LOOP('',(#20624,#20625,#20626,#20627));
#4414=EDGE_LOOP('',(#20628,#20629,#20630,#20631));
#4415=EDGE_LOOP('',(#20632,#20633,#20634,#20635));
#4416=EDGE_LOOP('',(#20636,#20637,#20638,#20639));
#4417=EDGE_LOOP('',(#20640,#20641,#20642,#20643));
#4418=EDGE_LOOP('',(#20644,#20645,#20646,#20647));
#4419=EDGE_LOOP('',(#20648,#20649,#20650,#20651));
#4420=EDGE_LOOP('',(#20652,#20653,#20654,#20655));
#4421=EDGE_LOOP('',(#20656,#20657,#20658,#20659));
#4422=EDGE_LOOP('',(#20660,#20661,#20662,#20663));
#4423=EDGE_LOOP('',(#20664,#20665,#20666,#20667));
#4424=EDGE_LOOP('',(#20668,#20669,#20670,#20671));
#4425=EDGE_LOOP('',(#20672,#20673,#20674,#20675));
#4426=EDGE_LOOP('',(#20676,#20677,#20678,#20679));
#4427=EDGE_LOOP('',(#20680,#20681,#20682,#20683));
#4428=EDGE_LOOP('',(#20684,#20685,#20686,#20687));
#4429=EDGE_LOOP('',(#20688,#20689,#20690,#20691));
#4430=EDGE_LOOP('',(#20692,#20693,#20694,#20695));
#4431=EDGE_LOOP('',(#20696,#20697,#20698,#20699));
#4432=EDGE_LOOP('',(#20700,#20701,#20702,#20703));
#4433=EDGE_LOOP('',(#20704,#20705,#20706,#20707));
#4434=EDGE_LOOP('',(#20708,#20709,#20710,#20711));
#4435=EDGE_LOOP('',(#20712,#20713,#20714,#20715));
#4436=EDGE_LOOP('',(#20716,#20717,#20718,#20719));
#4437=EDGE_LOOP('',(#20720,#20721,#20722,#20723));
#4438=EDGE_LOOP('',(#20724,#20725,#20726,#20727));
#4439=EDGE_LOOP('',(#20728,#20729,#20730,#20731));
#4440=EDGE_LOOP('',(#20732,#20733,#20734,#20735));
#4441=EDGE_LOOP('',(#20736,#20737,#20738,#20739));
#4442=EDGE_LOOP('',(#20740,#20741,#20742,#20743));
#4443=EDGE_LOOP('',(#20744,#20745,#20746,#20747));
#4444=EDGE_LOOP('',(#20748,#20749,#20750,#20751));
#4445=EDGE_LOOP('',(#20752,#20753,#20754,#20755));
#4446=EDGE_LOOP('',(#20756,#20757,#20758,#20759));
#4447=EDGE_LOOP('',(#20760,#20761,#20762,#20763));
#4448=EDGE_LOOP('',(#20764,#20765,#20766,#20767));
#4449=EDGE_LOOP('',(#20768,#20769,#20770,#20771));
#4450=EDGE_LOOP('',(#20772,#20773,#20774,#20775));
#4451=EDGE_LOOP('',(#20776,#20777,#20778,#20779));
#4452=EDGE_LOOP('',(#20780,#20781,#20782,#20783));
#4453=EDGE_LOOP('',(#20784,#20785,#20786,#20787));
#4454=EDGE_LOOP('',(#20788,#20789,#20790,#20791));
#4455=EDGE_LOOP('',(#20792,#20793,#20794,#20795));
#4456=EDGE_LOOP('',(#20796,#20797,#20798,#20799));
#4457=EDGE_LOOP('',(#20800,#20801,#20802,#20803));
#4458=EDGE_LOOP('',(#20804,#20805,#20806,#20807));
#4459=EDGE_LOOP('',(#20808,#20809,#20810,#20811));
#4460=EDGE_LOOP('',(#20812,#20813,#20814,#20815));
#4461=EDGE_LOOP('',(#20816,#20817,#20818,#20819));
#4462=EDGE_LOOP('',(#20820,#20821,#20822,#20823));
#4463=EDGE_LOOP('',(#20824,#20825,#20826,#20827));
#4464=EDGE_LOOP('',(#20828,#20829,#20830,#20831));
#4465=EDGE_LOOP('',(#20832,#20833,#20834,#20835));
#4466=EDGE_LOOP('',(#20836,#20837,#20838,#20839));
#4467=EDGE_LOOP('',(#20840,#20841,#20842,#20843));
#4468=EDGE_LOOP('',(#20844,#20845,#20846,#20847));
#4469=EDGE_LOOP('',(#20848,#20849,#20850,#20851));
#4470=EDGE_LOOP('',(#20852,#20853,#20854,#20855));
#4471=EDGE_LOOP('',(#20856,#20857,#20858,#20859));
#4472=EDGE_LOOP('',(#20860,#20861,#20862,#20863));
#4473=EDGE_LOOP('',(#20864,#20865,#20866,#20867));
#4474=EDGE_LOOP('',(#20868,#20869,#20870,#20871));
#4475=EDGE_LOOP('',(#20872,#20873,#20874,#20875));
#4476=EDGE_LOOP('',(#20876,#20877,#20878,#20879));
#4477=EDGE_LOOP('',(#20880,#20881,#20882,#20883));
#4478=EDGE_LOOP('',(#20884,#20885,#20886,#20887));
#4479=EDGE_LOOP('',(#20888,#20889,#20890,#20891));
#4480=EDGE_LOOP('',(#20892,#20893,#20894,#20895));
#4481=EDGE_LOOP('',(#20896,#20897,#20898,#20899));
#4482=EDGE_LOOP('',(#20900,#20901,#20902,#20903));
#4483=EDGE_LOOP('',(#20904,#20905,#20906,#20907));
#4484=EDGE_LOOP('',(#20908,#20909,#20910,#20911));
#4485=EDGE_LOOP('',(#20912,#20913,#20914,#20915));
#4486=EDGE_LOOP('',(#20916,#20917,#20918,#20919));
#4487=EDGE_LOOP('',(#20920,#20921,#20922,#20923));
#4488=EDGE_LOOP('',(#20924,#20925,#20926,#20927));
#4489=EDGE_LOOP('',(#20928,#20929,#20930,#20931));
#4490=EDGE_LOOP('',(#20932,#20933,#20934,#20935));
#4491=EDGE_LOOP('',(#20936,#20937,#20938,#20939));
#4492=EDGE_LOOP('',(#20940,#20941,#20942,#20943));
#4493=EDGE_LOOP('',(#20944,#20945,#20946,#20947));
#4494=EDGE_LOOP('',(#20948,#20949,#20950,#20951));
#4495=EDGE_LOOP('',(#20952,#20953,#20954,#20955));
#4496=EDGE_LOOP('',(#20956,#20957,#20958,#20959));
#4497=EDGE_LOOP('',(#20960,#20961,#20962,#20963));
#4498=EDGE_LOOP('',(#20964,#20965,#20966,#20967));
#4499=EDGE_LOOP('',(#20968,#20969,#20970,#20971));
#4500=EDGE_LOOP('',(#20972,#20973,#20974,#20975));
#4501=EDGE_LOOP('',(#20976,#20977,#20978,#20979));
#4502=EDGE_LOOP('',(#20980,#20981,#20982,#20983));
#4503=EDGE_LOOP('',(#20984,#20985,#20986,#20987));
#4504=EDGE_LOOP('',(#20988,#20989,#20990,#20991));
#4505=EDGE_LOOP('',(#20992,#20993,#20994,#20995));
#4506=EDGE_LOOP('',(#20996,#20997,#20998,#20999));
#4507=EDGE_LOOP('',(#21000,#21001,#21002,#21003));
#4508=EDGE_LOOP('',(#21004,#21005,#21006,#21007));
#4509=EDGE_LOOP('',(#21008,#21009,#21010,#21011));
#4510=EDGE_LOOP('',(#21012,#21013,#21014,#21015));
#4511=EDGE_LOOP('',(#21016,#21017,#21018,#21019));
#4512=EDGE_LOOP('',(#21020,#21021,#21022,#21023));
#4513=EDGE_LOOP('',(#21024,#21025,#21026,#21027));
#4514=EDGE_LOOP('',(#21028,#21029,#21030,#21031));
#4515=EDGE_LOOP('',(#21032,#21033,#21034,#21035));
#4516=EDGE_LOOP('',(#21036,#21037,#21038,#21039));
#4517=EDGE_LOOP('',(#21040,#21041,#21042,#21043));
#4518=EDGE_LOOP('',(#21044,#21045,#21046,#21047));
#4519=EDGE_LOOP('',(#21048,#21049,#21050,#21051));
#4520=EDGE_LOOP('',(#21052,#21053,#21054,#21055));
#4521=EDGE_LOOP('',(#21056,#21057,#21058,#21059));
#4522=EDGE_LOOP('',(#21060,#21061,#21062,#21063));
#4523=EDGE_LOOP('',(#21064,#21065,#21066,#21067));
#4524=EDGE_LOOP('',(#21068,#21069,#21070,#21071));
#4525=EDGE_LOOP('',(#21072,#21073,#21074,#21075));
#4526=EDGE_LOOP('',(#21076,#21077,#21078,#21079));
#4527=EDGE_LOOP('',(#21080,#21081,#21082,#21083));
#4528=EDGE_LOOP('',(#21084,#21085,#21086,#21087));
#4529=EDGE_LOOP('',(#21088,#21089,#21090,#21091));
#4530=EDGE_LOOP('',(#21092,#21093,#21094,#21095));
#4531=EDGE_LOOP('',(#21096,#21097,#21098,#21099));
#4532=EDGE_LOOP('',(#21100,#21101,#21102,#21103));
#4533=EDGE_LOOP('',(#21104,#21105,#21106,#21107));
#4534=EDGE_LOOP('',(#21108,#21109,#21110,#21111));
#4535=EDGE_LOOP('',(#21112,#21113,#21114,#21115));
#4536=EDGE_LOOP('',(#21116,#21117,#21118,#21119));
#4537=EDGE_LOOP('',(#21120,#21121,#21122,#21123));
#4538=EDGE_LOOP('',(#21124,#21125,#21126,#21127));
#4539=EDGE_LOOP('',(#21128,#21129,#21130,#21131));
#4540=EDGE_LOOP('',(#21132,#21133,#21134,#21135));
#4541=EDGE_LOOP('',(#21136,#21137,#21138,#21139));
#4542=EDGE_LOOP('',(#21140,#21141,#21142,#21143));
#4543=EDGE_LOOP('',(#21144,#21145,#21146,#21147));
#4544=EDGE_LOOP('',(#21148,#21149,#21150,#21151));
#4545=EDGE_LOOP('',(#21152,#21153,#21154,#21155));
#4546=EDGE_LOOP('',(#21156,#21157,#21158,#21159));
#4547=EDGE_LOOP('',(#21160,#21161,#21162,#21163));
#4548=EDGE_LOOP('',(#21164,#21165,#21166,#21167));
#4549=EDGE_LOOP('',(#21168,#21169,#21170,#21171));
#4550=EDGE_LOOP('',(#21172,#21173,#21174,#21175));
#4551=EDGE_LOOP('',(#21176,#21177,#21178,#21179));
#4552=EDGE_LOOP('',(#21180,#21181,#21182,#21183));
#4553=EDGE_LOOP('',(#21184,#21185,#21186,#21187));
#4554=EDGE_LOOP('',(#21188,#21189,#21190,#21191));
#4555=EDGE_LOOP('',(#21192,#21193,#21194,#21195));
#4556=EDGE_LOOP('',(#21196,#21197,#21198,#21199));
#4557=EDGE_LOOP('',(#21200,#21201,#21202,#21203));
#4558=EDGE_LOOP('',(#21204,#21205,#21206,#21207));
#4559=EDGE_LOOP('',(#21208,#21209,#21210,#21211));
#4560=EDGE_LOOP('',(#21212,#21213,#21214,#21215));
#4561=EDGE_LOOP('',(#21216,#21217,#21218,#21219));
#4562=EDGE_LOOP('',(#21220,#21221,#21222,#21223));
#4563=EDGE_LOOP('',(#21224,#21225,#21226,#21227));
#4564=EDGE_LOOP('',(#21228,#21229,#21230,#21231));
#4565=EDGE_LOOP('',(#21232,#21233,#21234,#21235));
#4566=EDGE_LOOP('',(#21236,#21237,#21238,#21239));
#4567=EDGE_LOOP('',(#21240,#21241,#21242,#21243));
#4568=EDGE_LOOP('',(#21244,#21245,#21246,#21247));
#4569=EDGE_LOOP('',(#21248,#21249,#21250,#21251));
#4570=EDGE_LOOP('',(#21252,#21253,#21254,#21255));
#4571=EDGE_LOOP('',(#21256,#21257,#21258,#21259));
#4572=EDGE_LOOP('',(#21260,#21261,#21262,#21263));
#4573=EDGE_LOOP('',(#21264,#21265,#21266,#21267));
#4574=EDGE_LOOP('',(#21268,#21269,#21270,#21271));
#4575=EDGE_LOOP('',(#21272,#21273,#21274,#21275));
#4576=EDGE_LOOP('',(#21276,#21277,#21278,#21279));
#4577=EDGE_LOOP('',(#21280,#21281,#21282,#21283));
#4578=EDGE_LOOP('',(#21284,#21285,#21286,#21287));
#4579=EDGE_LOOP('',(#21288,#21289,#21290,#21291));
#4580=EDGE_LOOP('',(#21292,#21293,#21294,#21295));
#4581=EDGE_LOOP('',(#21296,#21297,#21298,#21299));
#4582=EDGE_LOOP('',(#21300,#21301,#21302,#21303));
#4583=EDGE_LOOP('',(#21304,#21305,#21306,#21307));
#4584=EDGE_LOOP('',(#21308,#21309,#21310,#21311));
#4585=EDGE_LOOP('',(#21312,#21313,#21314,#21315));
#4586=EDGE_LOOP('',(#21316,#21317,#21318,#21319));
#4587=EDGE_LOOP('',(#21320,#21321,#21322,#21323));
#4588=EDGE_LOOP('',(#21324,#21325,#21326,#21327));
#4589=EDGE_LOOP('',(#21328,#21329,#21330,#21331));
#4590=EDGE_LOOP('',(#21332,#21333,#21334,#21335));
#4591=EDGE_LOOP('',(#21336,#21337,#21338,#21339));
#4592=EDGE_LOOP('',(#21340,#21341,#21342,#21343));
#4593=EDGE_LOOP('',(#21344,#21345,#21346,#21347));
#4594=EDGE_LOOP('',(#21348,#21349,#21350,#21351));
#4595=EDGE_LOOP('',(#21352,#21353,#21354,#21355));
#4596=EDGE_LOOP('',(#21356,#21357,#21358,#21359));
#4597=EDGE_LOOP('',(#21360,#21361,#21362,#21363));
#4598=EDGE_LOOP('',(#21364,#21365,#21366,#21367));
#4599=EDGE_LOOP('',(#21368,#21369,#21370,#21371));
#4600=EDGE_LOOP('',(#21372,#21373,#21374,#21375));
#4601=EDGE_LOOP('',(#21376,#21377,#21378,#21379));
#4602=EDGE_LOOP('',(#21380,#21381,#21382,#21383));
#4603=EDGE_LOOP('',(#21384,#21385,#21386,#21387));
#4604=EDGE_LOOP('',(#21388,#21389,#21390,#21391));
#4605=EDGE_LOOP('',(#21392,#21393,#21394,#21395));
#4606=EDGE_LOOP('',(#21396,#21397,#21398,#21399));
#4607=EDGE_LOOP('',(#21400,#21401,#21402,#21403));
#4608=EDGE_LOOP('',(#21404,#21405,#21406,#21407));
#4609=EDGE_LOOP('',(#21408,#21409,#21410,#21411));
#4610=EDGE_LOOP('',(#21412,#21413,#21414,#21415));
#4611=EDGE_LOOP('',(#21416,#21417,#21418,#21419));
#4612=EDGE_LOOP('',(#21420,#21421,#21422,#21423));
#4613=EDGE_LOOP('',(#21424,#21425,#21426,#21427));
#4614=EDGE_LOOP('',(#21428,#21429,#21430,#21431));
#4615=EDGE_LOOP('',(#21432,#21433,#21434,#21435));
#4616=EDGE_LOOP('',(#21436,#21437,#21438,#21439));
#4617=EDGE_LOOP('',(#21440,#21441,#21442,#21443));
#4618=EDGE_LOOP('',(#21444,#21445,#21446,#21447));
#4619=EDGE_LOOP('',(#21448,#21449,#21450,#21451));
#4620=EDGE_LOOP('',(#21452,#21453,#21454,#21455));
#4621=EDGE_LOOP('',(#21456,#21457,#21458,#21459));
#4622=EDGE_LOOP('',(#21460,#21461,#21462,#21463));
#4623=EDGE_LOOP('',(#21464,#21465,#21466,#21467));
#4624=EDGE_LOOP('',(#21468,#21469,#21470,#21471));
#4625=EDGE_LOOP('',(#21472,#21473,#21474,#21475));
#4626=EDGE_LOOP('',(#21476,#21477,#21478,#21479));
#4627=EDGE_LOOP('',(#21480,#21481,#21482,#21483));
#4628=EDGE_LOOP('',(#21484,#21485,#21486,#21487));
#4629=EDGE_LOOP('',(#21488,#21489,#21490,#21491));
#4630=EDGE_LOOP('',(#21492,#21493,#21494,#21495));
#4631=EDGE_LOOP('',(#21496,#21497,#21498,#21499));
#4632=EDGE_LOOP('',(#21500,#21501,#21502,#21503));
#4633=EDGE_LOOP('',(#21504,#21505,#21506,#21507));
#4634=EDGE_LOOP('',(#21508,#21509,#21510,#21511));
#4635=EDGE_LOOP('',(#21512,#21513,#21514,#21515));
#4636=EDGE_LOOP('',(#21516,#21517,#21518,#21519));
#4637=EDGE_LOOP('',(#21520,#21521,#21522,#21523));
#4638=EDGE_LOOP('',(#21524,#21525,#21526,#21527));
#4639=EDGE_LOOP('',(#21528,#21529,#21530,#21531));
#4640=EDGE_LOOP('',(#21532,#21533,#21534,#21535));
#4641=EDGE_LOOP('',(#21536,#21537,#21538,#21539));
#4642=EDGE_LOOP('',(#21540,#21541,#21542,#21543));
#4643=EDGE_LOOP('',(#21544,#21545,#21546,#21547));
#4644=EDGE_LOOP('',(#21548,#21549,#21550,#21551));
#4645=EDGE_LOOP('',(#21552,#21553,#21554,#21555));
#4646=EDGE_LOOP('',(#21556,#21557,#21558,#21559));
#4647=EDGE_LOOP('',(#21560,#21561,#21562,#21563));
#4648=EDGE_LOOP('',(#21564,#21565,#21566,#21567));
#4649=EDGE_LOOP('',(#21568,#21569,#21570,#21571));
#4650=EDGE_LOOP('',(#21572,#21573,#21574,#21575));
#4651=EDGE_LOOP('',(#21576,#21577,#21578,#21579));
#4652=EDGE_LOOP('',(#21580,#21581,#21582,#21583));
#4653=EDGE_LOOP('',(#21584,#21585,#21586,#21587));
#4654=EDGE_LOOP('',(#21588,#21589,#21590,#21591));
#4655=EDGE_LOOP('',(#21592,#21593,#21594,#21595));
#4656=EDGE_LOOP('',(#21596,#21597,#21598,#21599));
#4657=EDGE_LOOP('',(#21600,#21601,#21602,#21603));
#4658=EDGE_LOOP('',(#21604,#21605,#21606,#21607));
#4659=EDGE_LOOP('',(#21608,#21609,#21610,#21611));
#4660=EDGE_LOOP('',(#21612,#21613,#21614,#21615));
#4661=EDGE_LOOP('',(#21616,#21617,#21618,#21619));
#4662=EDGE_LOOP('',(#21620,#21621,#21622,#21623));
#4663=EDGE_LOOP('',(#21624,#21625,#21626,#21627));
#4664=EDGE_LOOP('',(#21628,#21629,#21630,#21631));
#4665=EDGE_LOOP('',(#21632,#21633,#21634,#21635));
#4666=EDGE_LOOP('',(#21636,#21637,#21638,#21639));
#4667=EDGE_LOOP('',(#21640,#21641,#21642,#21643));
#4668=EDGE_LOOP('',(#21644,#21645,#21646,#21647));
#4669=EDGE_LOOP('',(#21648,#21649,#21650,#21651));
#4670=EDGE_LOOP('',(#21652,#21653,#21654,#21655));
#4671=EDGE_LOOP('',(#21656,#21657,#21658,#21659));
#4672=EDGE_LOOP('',(#21660,#21661,#21662,#21663));
#4673=EDGE_LOOP('',(#21664,#21665,#21666,#21667));
#4674=EDGE_LOOP('',(#21668,#21669,#21670,#21671));
#4675=EDGE_LOOP('',(#21672,#21673,#21674,#21675));
#4676=EDGE_LOOP('',(#21676,#21677,#21678,#21679));
#4677=EDGE_LOOP('',(#21680,#21681,#21682,#21683));
#4678=EDGE_LOOP('',(#21684,#21685,#21686,#21687));
#4679=EDGE_LOOP('',(#21688,#21689,#21690,#21691,#21692,#21693));
#4680=EDGE_LOOP('',(#21694,#21695,#21696,#21697,#21698,#21699,#21700,#21701,
#21702,#21703,#21704,#21705,#21706,#21707,#21708,#21709,#21710,#21711,#21712,
#21713,#21714,#21715,#21716,#21717,#21718,#21719,#21720,#21721,#21722,#21723,
#21724,#21725,#21726,#21727,#21728,#21729,#21730,#21731,#21732,#21733,#21734,
#21735,#21736,#21737,#21738,#21739,#21740,#21741,#21742,#21743,#21744,#21745,
#21746,#21747,#21748,#21749,#21750,#21751,#21752,#21753,#21754,#21755,#21756,
#21757,#21758,#21759,#21760,#21761,#21762,#21763,#21764,#21765,#21766,#21767,
#21768,#21769,#21770,#21771,#21772,#21773,#21774,#21775,#21776,#21777,#21778,
#21779,#21780,#21781,#21782,#21783,#21784,#21785,#21786,#21787,#21788,#21789,
#21790,#21791,#21792,#21793,#21794,#21795,#21796,#21797,#21798,#21799,#21800,
#21801,#21802,#21803,#21804,#21805,#21806,#21807,#21808,#21809,#21810,#21811,
#21812,#21813,#21814,#21815,#21816,#21817,#21818,#21819,#21820,#21821,#21822,
#21823,#21824,#21825,#21826,#21827,#21828,#21829,#21830,#21831,#21832,#21833,
#21834,#21835,#21836,#21837,#21838,#21839,#21840,#21841,#21842,#21843,#21844,
#21845,#21846,#21847,#21848,#21849,#21850,#21851,#21852,#21853,#21854,#21855,
#21856,#21857,#21858,#21859,#21860,#21861,#21862,#21863,#21864,#21865,#21866,
#21867,#21868,#21869,#21870,#21871,#21872,#21873,#21874,#21875,#21876,#21877,
#21878,#21879,#21880,#21881,#21882,#21883,#21884,#21885,#21886,#21887,#21888,
#21889,#21890,#21891,#21892,#21893,#21894,#21895,#21896,#21897,#21898,#21899,
#21900,#21901,#21902,#21903,#21904,#21905,#21906,#21907,#21908,#21909,#21910,
#21911,#21912,#21913,#21914,#21915,#21916,#21917,#21918,#21919,#21920,#21921,
#21922,#21923,#21924,#21925,#21926,#21927,#21928,#21929,#21930,#21931,#21932,
#21933,#21934,#21935,#21936,#21937,#21938,#21939,#21940,#21941,#21942,#21943,
#21944,#21945,#21946,#21947,#21948,#21949,#21950,#21951,#21952,#21953,#21954,
#21955,#21956,#21957,#21958,#21959,#21960,#21961,#21962,#21963,#21964,#21965,
#21966,#21967,#21968,#21969,#21970,#21971,#21972,#21973,#21974,#21975,#21976,
#21977));
#4681=EDGE_LOOP('',(#21978));
#4682=EDGE_LOOP('',(#21979));
#4683=EDGE_LOOP('',(#21980));
#4684=EDGE_LOOP('',(#21981));
#4685=EDGE_LOOP('',(#21982));
#4686=EDGE_LOOP('',(#21983));
#4687=EDGE_LOOP('',(#21984));
#4688=EDGE_LOOP('',(#21985));
#4689=EDGE_LOOP('',(#21986));
#4690=EDGE_LOOP('',(#21987));
#4691=EDGE_LOOP('',(#21988,#21989,#21990,#21991,#21992,#21993,#21994,#21995,
#21996,#21997,#21998,#21999,#22000,#22001,#22002,#22003,#22004,#22005,#22006,
#22007,#22008,#22009,#22010,#22011,#22012,#22013,#22014,#22015,#22016,#22017,
#22018,#22019,#22020,#22021,#22022,#22023,#22024,#22025,#22026,#22027,#22028,
#22029,#22030,#22031,#22032,#22033,#22034,#22035,#22036,#22037,#22038,#22039,
#22040,#22041,#22042,#22043,#22044,#22045,#22046,#22047,#22048,#22049,#22050,
#22051,#22052,#22053,#22054,#22055,#22056,#22057,#22058,#22059,#22060,#22061,
#22062,#22063,#22064,#22065,#22066,#22067,#22068,#22069,#22070,#22071,#22072,
#22073,#22074,#22075,#22076,#22077,#22078,#22079,#22080,#22081,#22082,#22083,
#22084,#22085,#22086,#22087,#22088,#22089,#22090,#22091,#22092,#22093,#22094,
#22095,#22096,#22097,#22098,#22099,#22100,#22101,#22102,#22103,#22104,#22105,
#22106,#22107,#22108,#22109,#22110,#22111,#22112,#22113,#22114,#22115,#22116,
#22117,#22118,#22119,#22120,#22121,#22122,#22123,#22124,#22125,#22126,#22127,
#22128,#22129,#22130,#22131,#22132,#22133,#22134,#22135,#22136,#22137,#22138,
#22139,#22140,#22141,#22142,#22143,#22144,#22145,#22146,#22147,#22148,#22149,
#22150,#22151,#22152,#22153,#22154,#22155,#22156,#22157,#22158,#22159,#22160,
#22161,#22162,#22163,#22164,#22165,#22166,#22167,#22168,#22169,#22170,#22171,
#22172,#22173,#22174,#22175,#22176,#22177,#22178,#22179,#22180,#22181,#22182,
#22183,#22184,#22185,#22186,#22187,#22188,#22189,#22190,#22191,#22192,#22193,
#22194,#22195,#22196,#22197,#22198,#22199,#22200,#22201,#22202,#22203,#22204,
#22205,#22206,#22207,#22208,#22209,#22210,#22211,#22212,#22213,#22214,#22215,
#22216,#22217,#22218,#22219,#22220,#22221,#22222,#22223,#22224,#22225,#22226,
#22227,#22228,#22229,#22230,#22231,#22232,#22233,#22234,#22235,#22236,#22237,
#22238,#22239,#22240,#22241,#22242,#22243,#22244,#22245,#22246,#22247,#22248,
#22249,#22250,#22251,#22252,#22253,#22254,#22255,#22256,#22257,#22258,#22259,
#22260,#22261,#22262,#22263,#22264,#22265,#22266,#22267,#22268,#22269,#22270,
#22271));
#4692=EDGE_LOOP('',(#22272));
#4693=EDGE_LOOP('',(#22273));
#4694=EDGE_LOOP('',(#22274));
#4695=EDGE_LOOP('',(#22275));
#4696=EDGE_LOOP('',(#22276));
#4697=EDGE_LOOP('',(#22277));
#4698=EDGE_LOOP('',(#22278));
#4699=EDGE_LOOP('',(#22279));
#4700=EDGE_LOOP('',(#22280));
#4701=EDGE_LOOP('',(#22281));
#4702=EDGE_LOOP('',(#22282,#22283,#22284,#22285));
#4703=EDGE_LOOP('',(#22286,#22287,#22288,#22289,#22290,#22291,#22292,#22293));
#4704=EDGE_LOOP('',(#22294));
#4705=EDGE_LOOP('',(#22295));
#4706=EDGE_LOOP('',(#22296));
#4707=EDGE_LOOP('',(#22297));
#4708=EDGE_LOOP('',(#22298,#22299,#22300,#22301,#22302,#22303));
#4709=EDGE_LOOP('',(#22304,#22305,#22306,#22307,#22308,#22309));
#4710=EDGE_LOOP('',(#22310));
#4711=EDGE_LOOP('',(#22311));
#4712=EDGE_LOOP('',(#22312));
#4713=EDGE_LOOP('',(#22313));
#4714=EDGE_LOOP('',(#22314,#22315,#22316,#22317));
#4715=EDGE_LOOP('',(#22318,#22319,#22320,#22321));
#4716=EDGE_LOOP('',(#22322,#22323,#22324,#22325));
#4717=EDGE_LOOP('',(#22326,#22327,#22328,#22329));
#4718=EDGE_LOOP('',(#22330,#22331,#22332,#22333));
#4719=EDGE_LOOP('',(#22334,#22335,#22336,#22337));
#4720=EDGE_LOOP('',(#22338,#22339,#22340,#22341));
#4721=EDGE_LOOP('',(#22342,#22343,#22344,#22345));
#4722=EDGE_LOOP('',(#22346,#22347,#22348,#22349));
#4723=EDGE_LOOP('',(#22350,#22351,#22352,#22353));
#4724=EDGE_LOOP('',(#22354,#22355,#22356,#22357));
#4725=EDGE_LOOP('',(#22358,#22359,#22360,#22361));
#4726=EDGE_LOOP('',(#22362,#22363,#22364,#22365));
#4727=EDGE_LOOP('',(#22366,#22367,#22368,#22369));
#4728=EDGE_LOOP('',(#22370,#22371,#22372,#22373));
#4729=EDGE_LOOP('',(#22374,#22375,#22376,#22377));
#4730=EDGE_LOOP('',(#22378,#22379,#22380,#22381));
#4731=EDGE_LOOP('',(#22382,#22383,#22384,#22385));
#4732=EDGE_LOOP('',(#22386,#22387,#22388,#22389));
#4733=EDGE_LOOP('',(#22390,#22391,#22392,#22393));
#4734=EDGE_LOOP('',(#22394,#22395,#22396,#22397));
#4735=EDGE_LOOP('',(#22398,#22399,#22400,#22401));
#4736=EDGE_LOOP('',(#22402,#22403,#22404,#22405));
#4737=EDGE_LOOP('',(#22406,#22407,#22408,#22409));
#4738=EDGE_LOOP('',(#22410,#22411,#22412,#22413));
#4739=EDGE_LOOP('',(#22414,#22415,#22416,#22417));
#4740=EDGE_LOOP('',(#22418,#22419,#22420,#22421));
#4741=EDGE_LOOP('',(#22422,#22423,#22424,#22425));
#4742=EDGE_LOOP('',(#22426,#22427,#22428,#22429));
#4743=EDGE_LOOP('',(#22430,#22431,#22432,#22433));
#4744=EDGE_LOOP('',(#22434,#22435,#22436,#22437));
#4745=EDGE_LOOP('',(#22438,#22439,#22440,#22441));
#4746=EDGE_LOOP('',(#22442,#22443,#22444,#22445));
#4747=EDGE_LOOP('',(#22446,#22447,#22448,#22449));
#4748=EDGE_LOOP('',(#22450,#22451,#22452,#22453));
#4749=EDGE_LOOP('',(#22454,#22455,#22456,#22457));
#4750=EDGE_LOOP('',(#22458,#22459,#22460,#22461));
#4751=EDGE_LOOP('',(#22462,#22463,#22464,#22465));
#4752=EDGE_LOOP('',(#22466,#22467,#22468,#22469));
#4753=EDGE_LOOP('',(#22470,#22471,#22472,#22473));
#4754=EDGE_LOOP('',(#22474,#22475,#22476,#22477));
#4755=EDGE_LOOP('',(#22478,#22479,#22480,#22481));
#4756=EDGE_LOOP('',(#22482,#22483,#22484,#22485));
#4757=EDGE_LOOP('',(#22486,#22487,#22488,#22489,#22490,#22491,#22492,#22493));
#4758=EDGE_LOOP('',(#22494,#22495,#22496,#22497,#22498,#22499));
#4759=EDGE_LOOP('',(#22500,#22501,#22502,#22503,#22504,#22505));
#4760=EDGE_LOOP('',(#22506));
#4761=EDGE_LOOP('',(#22507));
#4762=EDGE_LOOP('',(#22508));
#4763=EDGE_LOOP('',(#22509));
#4764=EDGE_LOOP('',(#22510));
#4765=EDGE_LOOP('',(#22511));
#4766=EDGE_LOOP('',(#22512));
#4767=EDGE_LOOP('',(#22513));
#4768=EDGE_LOOP('',(#22514,#22515,#22516,#22517));
#4769=EDGE_LOOP('',(#22518,#22519,#22520,#22521));
#4770=EDGE_LOOP('',(#22522,#22523,#22524,#22525));
#4771=EDGE_LOOP('',(#22526,#22527,#22528,#22529,#22530,#22531,#22532,#22533));
#4772=EDGE_LOOP('',(#22534,#22535,#22536,#22537));
#4773=EDGE_LOOP('',(#22538));
#4774=EDGE_LOOP('',(#22539,#22540,#22541,#22542));
#4775=EDGE_LOOP('',(#22543,#22544,#22545,#22546,#22547,#22548,#22549,#22550));
#4776=EDGE_LOOP('',(#22551,#22552,#22553,#22554));
#4777=EDGE_LOOP('',(#22555));
#4778=EDGE_LOOP('',(#22556,#22557));
#4779=EDGE_LOOP('',(#22558,#22559));
#4780=EDGE_LOOP('',(#22560,#22561,#22562,#22563,#22564));
#4781=EDGE_LOOP('',(#22565,#22566,#22567,#22568,#22569));
#4782=EDGE_LOOP('',(#22570,#22571));
#4783=EDGE_LOOP('',(#22572,#22573));
#4784=EDGE_LOOP('',(#22574,#22575,#22576,#22577,#22578));
#4785=EDGE_LOOP('',(#22579,#22580,#22581,#22582,#22583));
#4786=EDGE_LOOP('',(#22584,#22585,#22586,#22587));
#4787=EDGE_LOOP('',(#22588,#22589,#22590,#22591,#22592,#22593));
#4788=EDGE_LOOP('',(#22594));
#4789=EDGE_LOOP('',(#22595,#22596,#22597,#22598));
#4790=EDGE_LOOP('',(#22599,#22600,#22601,#22602));
#4791=EDGE_LOOP('',(#22603,#22604,#22605,#22606,#22607,#22608));
#4792=EDGE_LOOP('',(#22609));
#4793=EDGE_LOOP('',(#22610,#22611,#22612,#22613));
#4794=EDGE_LOOP('',(#22614,#22615,#22616,#22617));
#4795=EDGE_LOOP('',(#22618,#22619,#22620,#22621));
#4796=EDGE_LOOP('',(#22622,#22623,#22624,#22625));
#4797=EDGE_LOOP('',(#22626,#22627,#22628,#22629));
#4798=EDGE_LOOP('',(#22630,#22631,#22632,#22633));
#4799=EDGE_LOOP('',(#22634,#22635,#22636,#22637));
#4800=EDGE_LOOP('',(#22638,#22639,#22640,#22641,#22642,#22643,#22644,#22645));
#4801=EDGE_LOOP('',(#22646));
#4802=EDGE_LOOP('',(#22647));
#4803=EDGE_LOOP('',(#22648,#22649,#22650,#22651,#22652,#22653,#22654,#22655));
#4804=EDGE_LOOP('',(#22656));
#4805=EDGE_LOOP('',(#22657));
#4806=EDGE_LOOP('',(#22658,#22659,#22660,#22661));
#4807=EDGE_LOOP('',(#22662,#22663,#22664,#22665));
#4808=EDGE_LOOP('',(#22666,#22667,#22668,#22669,#22670,#22671));
#4809=EDGE_LOOP('',(#22672,#22673,#22674,#22675));
#4810=EDGE_LOOP('',(#22676,#22677,#22678,#22679,#22680,#22681));
#4811=EDGE_LOOP('',(#22682,#22683,#22684,#22685));
#4812=EDGE_LOOP('',(#22686,#22687,#22688,#22689,#22690,#22691));
#4813=EDGE_LOOP('',(#22692,#22693,#22694,#22695,#22696,#22697,#22698,#22699,
#22700,#22701,#22702,#22703,#22704,#22705,#22706,#22707,#22708,#22709,#22710,
#22711));
#4814=EDGE_LOOP('',(#22712,#22713,#22714,#22715));
#4815=EDGE_LOOP('',(#22716,#22717,#22718,#22719,#22720,#22721));
#4816=EDGE_LOOP('',(#22722,#22723,#22724,#22725,#22726,#22727,#22728,#22729,
#22730,#22731,#22732,#22733,#22734,#22735,#22736,#22737,#22738,#22739,#22740,
#22741,#22742,#22743,#22744,#22745));
#4817=EDGE_LOOP('',(#22746,#22747,#22748,#22749,#22750,#22751));
#4818=EDGE_LOOP('',(#22752,#22753,#22754,#22755,#22756,#22757,#22758,#22759,
#22760,#22761,#22762,#22763,#22764,#22765,#22766,#22767,#22768,#22769,#22770,
#22771,#22772,#22773,#22774,#22775));
#4819=EDGE_LOOP('',(#22776,#22777,#22778,#22779,#22780,#22781,#22782));
#4820=EDGE_LOOP('',(#22783));
#4821=EDGE_LOOP('',(#22784));
#4822=EDGE_LOOP('',(#22785,#22786,#22787,#22788,#22789,#22790,#22791));
#4823=EDGE_LOOP('',(#22792));
#4824=EDGE_LOOP('',(#22793,#22794,#22795,#22796));
#4825=EDGE_LOOP('',(#22797,#22798,#22799,#22800));
#4826=EDGE_LOOP('',(#22801,#22802,#22803));
#4827=EDGE_LOOP('',(#22804,#22805,#22806,#22807,#22808,#22809,#22810,#22811,
#22812,#22813,#22814,#22815,#22816,#22817,#22818,#22819,#22820,#22821,#22822,
#22823,#22824,#22825,#22826,#22827,#22828,#22829,#22830,#22831,#22832,#22833,
#22834,#22835,#22836,#22837,#22838,#22839,#22840,#22841,#22842,#22843,#22844,
#22845,#22846,#22847,#22848,#22849,#22850,#22851,#22852,#22853,#22854,#22855,
#22856,#22857,#22858,#22859,#22860,#22861,#22862,#22863,#22864,#22865,#22866,
#22867,#22868,#22869,#22870,#22871,#22872,#22873,#22874,#22875,#22876,#22877,
#22878,#22879,#22880,#22881,#22882,#22883,#22884,#22885,#22886,#22887,#22888,
#22889,#22890,#22891,#22892,#22893,#22894,#22895,#22896,#22897,#22898,#22899,
#22900,#22901,#22902,#22903,#22904,#22905,#22906,#22907,#22908,#22909,#22910,
#22911,#22912,#22913,#22914));
#4828=EDGE_LOOP('',(#22915,#22916,#22917,#22918));
#4829=EDGE_LOOP('',(#22919,#22920,#22921,#22922));
#4830=EDGE_LOOP('',(#22923,#22924,#22925));
#4831=EDGE_LOOP('',(#22926,#22927,#22928,#22929));
#4832=EDGE_LOOP('',(#22930,#22931,#22932,#22933));
#4833=EDGE_LOOP('',(#22934,#22935,#22936));
#4834=EDGE_LOOP('',(#22937,#22938,#22939,#22940));
#4835=EDGE_LOOP('',(#22941,#22942,#22943,#22944));
#4836=EDGE_LOOP('',(#22945,#22946,#22947));
#4837=EDGE_LOOP('',(#22948,#22949,#22950,#22951));
#4838=EDGE_LOOP('',(#22952,#22953,#22954,#22955));
#4839=EDGE_LOOP('',(#22956,#22957,#22958));
#4840=EDGE_LOOP('',(#22959,#22960,#22961,#22962));
#4841=EDGE_LOOP('',(#22963,#22964,#22965,#22966));
#4842=EDGE_LOOP('',(#22967,#22968,#22969));
#4843=EDGE_LOOP('',(#22970,#22971,#22972,#22973));
#4844=EDGE_LOOP('',(#22974,#22975,#22976,#22977));
#4845=EDGE_LOOP('',(#22978,#22979,#22980));
#4846=EDGE_LOOP('',(#22981,#22982,#22983,#22984));
#4847=EDGE_LOOP('',(#22985,#22986,#22987,#22988));
#4848=EDGE_LOOP('',(#22989,#22990,#22991));
#4849=EDGE_LOOP('',(#22992,#22993,#22994,#22995));
#4850=EDGE_LOOP('',(#22996,#22997,#22998,#22999));
#4851=EDGE_LOOP('',(#23000,#23001,#23002,#23003));
#4852=EDGE_LOOP('',(#23004,#23005,#23006,#23007));
#4853=EDGE_LOOP('',(#23008,#23009,#23010,#23011));
#4854=EDGE_LOOP('',(#23012,#23013,#23014));
#4855=EDGE_LOOP('',(#23015,#23016,#23017,#23018));
#4856=EDGE_LOOP('',(#23019,#23020,#23021,#23022));
#4857=EDGE_LOOP('',(#23023,#23024,#23025));
#4858=EDGE_LOOP('',(#23026,#23027,#23028,#23029));
#4859=EDGE_LOOP('',(#23030,#23031,#23032,#23033));
#4860=EDGE_LOOP('',(#23034,#23035,#23036));
#4861=EDGE_LOOP('',(#23037,#23038,#23039,#23040));
#4862=EDGE_LOOP('',(#23041,#23042,#23043,#23044));
#4863=EDGE_LOOP('',(#23045,#23046,#23047));
#4864=EDGE_LOOP('',(#23048,#23049,#23050,#23051));
#4865=EDGE_LOOP('',(#23052,#23053,#23054,#23055));
#4866=EDGE_LOOP('',(#23056,#23057,#23058));
#4867=EDGE_LOOP('',(#23059,#23060,#23061,#23062));
#4868=EDGE_LOOP('',(#23063,#23064,#23065,#23066));
#4869=EDGE_LOOP('',(#23067,#23068,#23069));
#4870=EDGE_LOOP('',(#23070,#23071,#23072,#23073));
#4871=EDGE_LOOP('',(#23074,#23075,#23076,#23077));
#4872=EDGE_LOOP('',(#23078,#23079,#23080));
#4873=EDGE_LOOP('',(#23081,#23082,#23083,#23084));
#4874=EDGE_LOOP('',(#23085,#23086,#23087,#23088));
#4875=EDGE_LOOP('',(#23089,#23090,#23091));
#4876=EDGE_LOOP('',(#23092,#23093,#23094,#23095));
#4877=EDGE_LOOP('',(#23096,#23097,#23098,#23099));
#4878=EDGE_LOOP('',(#23100,#23101,#23102));
#4879=EDGE_LOOP('',(#23103,#23104,#23105,#23106));
#4880=EDGE_LOOP('',(#23107,#23108,#23109,#23110));
#4881=EDGE_LOOP('',(#23111,#23112,#23113));
#4882=EDGE_LOOP('',(#23114,#23115,#23116,#23117));
#4883=EDGE_LOOP('',(#23118,#23119,#23120,#23121));
#4884=EDGE_LOOP('',(#23122,#23123,#23124));
#4885=EDGE_LOOP('',(#23125,#23126,#23127,#23128));
#4886=EDGE_LOOP('',(#23129,#23130,#23131,#23132));
#4887=EDGE_LOOP('',(#23133,#23134,#23135));
#4888=EDGE_LOOP('',(#23136,#23137,#23138,#23139));
#4889=EDGE_LOOP('',(#23140,#23141,#23142,#23143));
#4890=EDGE_LOOP('',(#23144,#23145,#23146));
#4891=EDGE_LOOP('',(#23147,#23148,#23149,#23150));
#4892=EDGE_LOOP('',(#23151,#23152,#23153,#23154));
#4893=EDGE_LOOP('',(#23155,#23156,#23157));
#4894=EDGE_LOOP('',(#23158,#23159,#23160,#23161));
#4895=EDGE_LOOP('',(#23162,#23163,#23164,#23165));
#4896=EDGE_LOOP('',(#23166,#23167,#23168));
#4897=EDGE_LOOP('',(#23169,#23170,#23171,#23172));
#4898=EDGE_LOOP('',(#23173,#23174,#23175,#23176));
#4899=EDGE_LOOP('',(#23177,#23178,#23179));
#4900=EDGE_LOOP('',(#23180,#23181,#23182,#23183));
#4901=EDGE_LOOP('',(#23184,#23185,#23186,#23187));
#4902=EDGE_LOOP('',(#23188,#23189,#23190));
#4903=EDGE_LOOP('',(#23191,#23192,#23193,#23194));
#4904=EDGE_LOOP('',(#23195,#23196,#23197,#23198));
#4905=EDGE_LOOP('',(#23199,#23200,#23201));
#4906=EDGE_LOOP('',(#23202,#23203,#23204,#23205));
#4907=EDGE_LOOP('',(#23206,#23207,#23208,#23209));
#4908=EDGE_LOOP('',(#23210,#23211,#23212));
#4909=EDGE_LOOP('',(#23213,#23214,#23215,#23216));
#4910=EDGE_LOOP('',(#23217,#23218,#23219,#23220));
#4911=EDGE_LOOP('',(#23221,#23222,#23223));
#4912=EDGE_LOOP('',(#23224,#23225,#23226,#23227));
#4913=EDGE_LOOP('',(#23228,#23229,#23230,#23231));
#4914=EDGE_LOOP('',(#23232,#23233,#23234));
#4915=EDGE_LOOP('',(#23235,#23236,#23237,#23238));
#4916=EDGE_LOOP('',(#23239,#23240,#23241,#23242));
#4917=EDGE_LOOP('',(#23243,#23244,#23245));
#4918=EDGE_LOOP('',(#23246,#23247,#23248,#23249));
#4919=EDGE_LOOP('',(#23250,#23251,#23252,#23253));
#4920=EDGE_LOOP('',(#23254,#23255,#23256));
#4921=EDGE_LOOP('',(#23257,#23258,#23259,#23260));
#4922=EDGE_LOOP('',(#23261,#23262,#23263,#23264));
#4923=EDGE_LOOP('',(#23265,#23266,#23267));
#4924=EDGE_LOOP('',(#23268,#23269,#23270,#23271));
#4925=EDGE_LOOP('',(#23272,#23273,#23274,#23275));
#4926=EDGE_LOOP('',(#23276,#23277,#23278));
#4927=EDGE_LOOP('',(#23279,#23280,#23281,#23282));
#4928=EDGE_LOOP('',(#23283,#23284,#23285,#23286));
#4929=EDGE_LOOP('',(#23287,#23288,#23289));
#4930=EDGE_LOOP('',(#23290,#23291,#23292,#23293));
#4931=EDGE_LOOP('',(#23294,#23295,#23296,#23297));
#4932=EDGE_LOOP('',(#23298,#23299,#23300));
#4933=EDGE_LOOP('',(#23301,#23302,#23303,#23304,#23305,#23306,#23307,#23308,
#23309,#23310,#23311,#23312,#23313,#23314,#23315,#23316,#23317,#23318,#23319,
#23320,#23321,#23322,#23323,#23324,#23325,#23326,#23327,#23328,#23329,#23330,
#23331,#23332,#23333,#23334,#23335,#23336,#23337,#23338,#23339,#23340,#23341,
#23342,#23343,#23344,#23345,#23346,#23347,#23348,#23349,#23350,#23351,#23352,
#23353,#23354,#23355,#23356,#23357,#23358,#23359,#23360,#23361,#23362,#23363,
#23364,#23365,#23366,#23367,#23368,#23369,#23370,#23371,#23372,#23373,#23374,
#23375,#23376,#23377,#23378,#23379,#23380,#23381,#23382,#23383,#23384,#23385,
#23386,#23387,#23388,#23389,#23390,#23391,#23392,#23393,#23394,#23395,#23396,
#23397,#23398,#23399,#23400,#23401,#23402,#23403,#23404,#23405,#23406,#23407,
#23408,#23409,#23410,#23411,#23412,#23413,#23414,#23415,#23416,#23417,#23418,
#23419,#23420,#23421,#23422,#23423,#23424,#23425,#23426,#23427,#23428,#23429,
#23430,#23431,#23432,#23433,#23434,#23435,#23436,#23437,#23438,#23439,#23440,
#23441,#23442,#23443,#23444,#23445,#23446,#23447,#23448));
#4934=EDGE_LOOP('',(#23449));
#4935=EDGE_LOOP('',(#23450,#23451,#23452,#23453,#23454,#23455));
#4936=EDGE_LOOP('',(#23456,#23457));
#4937=EDGE_LOOP('',(#23458,#23459));
#4938=EDGE_LOOP('',(#23460,#23461));
#4939=EDGE_LOOP('',(#23462,#23463));
#4940=EDGE_LOOP('',(#23464,#23465));
#4941=EDGE_LOOP('',(#23466,#23467));
#4942=EDGE_LOOP('',(#23468,#23469,#23470,#23471,#23472,#23473,#23474,#23475));
#4943=EDGE_LOOP('',(#23476,#23477,#23478,#23479));
#4944=EDGE_LOOP('',(#23480,#23481,#23482,#23483));
#4945=EDGE_LOOP('',(#23484,#23485,#23486,#23487));
#4946=EDGE_LOOP('',(#23488,#23489,#23490,#23491));
#4947=EDGE_LOOP('',(#23492,#23493,#23494,#23495));
#4948=EDGE_LOOP('',(#23496,#23497,#23498,#23499));
#4949=EDGE_LOOP('',(#23500,#23501,#23502,#23503));
#4950=EDGE_LOOP('',(#23504,#23505,#23506,#23507,#23508,#23509));
#4951=EDGE_LOOP('',(#23510,#23511,#23512,#23513,#23514));
#4952=EDGE_LOOP('',(#23515,#23516,#23517,#23518,#23519,#23520));
#4953=EDGE_LOOP('',(#23521,#23522,#23523,#23524,#23525,#23526));
#4954=EDGE_LOOP('',(#23527,#23528,#23529,#23530,#23531));
#4955=EDGE_LOOP('',(#23532,#23533,#23534,#23535,#23536));
#4956=EDGE_LOOP('',(#23537,#23538,#23539,#23540,#23541));
#4957=EDGE_LOOP('',(#23542,#23543,#23544,#23545,#23546));
#4958=EDGE_LOOP('',(#23547,#23548,#23549,#23550,#23551,#23552,#23553,#23554,
#23555,#23556,#23557,#23558,#23559,#23560,#23561,#23562,#23563,#23564,#23565,
#23566,#23567,#23568,#23569,#23570));
#4959=EDGE_LOOP('',(#23571,#23572,#23573,#23574,#23575,#23576));
#4960=EDGE_LOOP('',(#23577,#23578,#23579,#23580,#23581));
#4961=EDGE_LOOP('',(#23582,#23583,#23584,#23585,#23586,#23587,#23588,#23589,
#23590,#23591,#23592,#23593,#23594,#23595,#23596,#23597,#23598,#23599,#23600,
#23601,#23602,#23603,#23604,#23605,#23606,#23607,#23608,#23609,#23610,#23611,
#23612));
#4962=EDGE_LOOP('',(#23613,#23614,#23615,#23616,#23617));
#4963=EDGE_LOOP('',(#23618,#23619,#23620,#23621,#23622,#23623,#23624,#23625,
#23626,#23627,#23628,#23629,#23630,#23631,#23632,#23633,#23634,#23635,#23636,
#23637,#23638,#23639,#23640,#23641,#23642,#23643,#23644,#23645,#23646,#23647));
#4964=EDGE_LOOP('',(#23648,#23649,#23650,#23651,#23652,#23653,#23654));
#4965=EDGE_LOOP('',(#23655));
#4966=EDGE_LOOP('',(#23656));
#4967=EDGE_LOOP('',(#23657,#23658,#23659,#23660,#23661,#23662,#23663));
#4968=EDGE_LOOP('',(#23664));
#4969=EDGE_LOOP('',(#23665,#23666,#23667,#23668));
#4970=EDGE_LOOP('',(#23669,#23670,#23671,#23672));
#4971=EDGE_LOOP('',(#23673,#23674,#23675));
#4972=EDGE_LOOP('',(#23676,#23677,#23678,#23679,#23680,#23681,#23682,#23683,
#23684,#23685,#23686,#23687,#23688,#23689,#23690,#23691,#23692,#23693,#23694,
#23695,#23696,#23697,#23698,#23699,#23700,#23701,#23702,#23703,#23704,#23705,
#23706,#23707,#23708,#23709,#23710,#23711,#23712,#23713,#23714,#23715,#23716,
#23717,#23718,#23719,#23720,#23721,#23722,#23723,#23724,#23725,#23726,#23727,
#23728,#23729,#23730,#23731,#23732,#23733,#23734,#23735,#23736,#23737,#23738,
#23739,#23740,#23741,#23742,#23743,#23744,#23745,#23746,#23747,#23748,#23749,
#23750,#23751,#23752,#23753,#23754,#23755,#23756,#23757,#23758,#23759,#23760,
#23761,#23762,#23763,#23764,#23765,#23766,#23767,#23768,#23769,#23770,#23771,
#23772,#23773,#23774,#23775,#23776,#23777,#23778,#23779,#23780,#23781,#23782,
#23783,#23784,#23785,#23786));
#4973=EDGE_LOOP('',(#23787,#23788,#23789,#23790));
#4974=EDGE_LOOP('',(#23791,#23792,#23793,#23794));
#4975=EDGE_LOOP('',(#23795,#23796,#23797));
#4976=EDGE_LOOP('',(#23798,#23799,#23800,#23801));
#4977=EDGE_LOOP('',(#23802,#23803,#23804,#23805));
#4978=EDGE_LOOP('',(#23806,#23807,#23808));
#4979=EDGE_LOOP('',(#23809,#23810,#23811,#23812));
#4980=EDGE_LOOP('',(#23813,#23814,#23815,#23816));
#4981=EDGE_LOOP('',(#23817,#23818,#23819));
#4982=EDGE_LOOP('',(#23820,#23821,#23822,#23823));
#4983=EDGE_LOOP('',(#23824,#23825,#23826,#23827));
#4984=EDGE_LOOP('',(#23828,#23829,#23830));
#4985=EDGE_LOOP('',(#23831,#23832,#23833,#23834));
#4986=EDGE_LOOP('',(#23835,#23836,#23837,#23838));
#4987=EDGE_LOOP('',(#23839,#23840,#23841));
#4988=EDGE_LOOP('',(#23842,#23843,#23844,#23845));
#4989=EDGE_LOOP('',(#23846,#23847,#23848,#23849));
#4990=EDGE_LOOP('',(#23850,#23851,#23852));
#4991=EDGE_LOOP('',(#23853,#23854,#23855,#23856));
#4992=EDGE_LOOP('',(#23857,#23858,#23859,#23860));
#4993=EDGE_LOOP('',(#23861,#23862,#23863));
#4994=EDGE_LOOP('',(#23864,#23865,#23866,#23867));
#4995=EDGE_LOOP('',(#23868,#23869,#23870,#23871));
#4996=EDGE_LOOP('',(#23872,#23873,#23874));
#4997=EDGE_LOOP('',(#23875,#23876,#23877,#23878));
#4998=EDGE_LOOP('',(#23879,#23880,#23881,#23882));
#4999=EDGE_LOOP('',(#23883,#23884,#23885));
#5000=EDGE_LOOP('',(#23886,#23887,#23888,#23889));
#5001=EDGE_LOOP('',(#23890,#23891,#23892,#23893));
#5002=EDGE_LOOP('',(#23894,#23895,#23896));
#5003=EDGE_LOOP('',(#23897,#23898,#23899,#23900));
#5004=EDGE_LOOP('',(#23901,#23902,#23903,#23904));
#5005=EDGE_LOOP('',(#23905,#23906,#23907));
#5006=EDGE_LOOP('',(#23908,#23909,#23910,#23911));
#5007=EDGE_LOOP('',(#23912,#23913,#23914,#23915));
#5008=EDGE_LOOP('',(#23916,#23917,#23918));
#5009=EDGE_LOOP('',(#23919,#23920,#23921,#23922));
#5010=EDGE_LOOP('',(#23923,#23924,#23925,#23926));
#5011=EDGE_LOOP('',(#23927,#23928,#23929));
#5012=EDGE_LOOP('',(#23930,#23931,#23932,#23933));
#5013=EDGE_LOOP('',(#23934,#23935,#23936,#23937));
#5014=EDGE_LOOP('',(#23938,#23939,#23940));
#5015=EDGE_LOOP('',(#23941,#23942,#23943,#23944));
#5016=EDGE_LOOP('',(#23945,#23946,#23947,#23948));
#5017=EDGE_LOOP('',(#23949,#23950,#23951));
#5018=EDGE_LOOP('',(#23952,#23953,#23954,#23955));
#5019=EDGE_LOOP('',(#23956,#23957,#23958,#23959));
#5020=EDGE_LOOP('',(#23960,#23961,#23962));
#5021=EDGE_LOOP('',(#23963,#23964,#23965,#23966));
#5022=EDGE_LOOP('',(#23967,#23968,#23969,#23970));
#5023=EDGE_LOOP('',(#23971,#23972,#23973,#23974));
#5024=EDGE_LOOP('',(#23975,#23976,#23977,#23978));
#5025=EDGE_LOOP('',(#23979,#23980,#23981,#23982));
#5026=EDGE_LOOP('',(#23983,#23984,#23985));
#5027=EDGE_LOOP('',(#23986,#23987,#23988,#23989));
#5028=EDGE_LOOP('',(#23990,#23991,#23992,#23993));
#5029=EDGE_LOOP('',(#23994,#23995,#23996));
#5030=EDGE_LOOP('',(#23997,#23998,#23999,#24000));
#5031=EDGE_LOOP('',(#24001,#24002,#24003,#24004));
#5032=EDGE_LOOP('',(#24005,#24006,#24007));
#5033=EDGE_LOOP('',(#24008,#24009,#24010,#24011));
#5034=EDGE_LOOP('',(#24012,#24013,#24014,#24015));
#5035=EDGE_LOOP('',(#24016,#24017,#24018));
#5036=EDGE_LOOP('',(#24019,#24020,#24021,#24022));
#5037=EDGE_LOOP('',(#24023,#24024,#24025,#24026));
#5038=EDGE_LOOP('',(#24027,#24028,#24029));
#5039=EDGE_LOOP('',(#24030,#24031,#24032,#24033));
#5040=EDGE_LOOP('',(#24034,#24035,#24036,#24037));
#5041=EDGE_LOOP('',(#24038,#24039,#24040));
#5042=EDGE_LOOP('',(#24041,#24042,#24043,#24044));
#5043=EDGE_LOOP('',(#24045,#24046,#24047,#24048));
#5044=EDGE_LOOP('',(#24049,#24050,#24051));
#5045=EDGE_LOOP('',(#24052,#24053,#24054,#24055));
#5046=EDGE_LOOP('',(#24056,#24057,#24058,#24059));
#5047=EDGE_LOOP('',(#24060,#24061,#24062));
#5048=EDGE_LOOP('',(#24063,#24064,#24065,#24066));
#5049=EDGE_LOOP('',(#24067,#24068,#24069,#24070));
#5050=EDGE_LOOP('',(#24071,#24072,#24073));
#5051=EDGE_LOOP('',(#24074,#24075,#24076,#24077));
#5052=EDGE_LOOP('',(#24078,#24079,#24080,#24081));
#5053=EDGE_LOOP('',(#24082,#24083,#24084));
#5054=EDGE_LOOP('',(#24085,#24086,#24087,#24088));
#5055=EDGE_LOOP('',(#24089,#24090,#24091,#24092));
#5056=EDGE_LOOP('',(#24093,#24094,#24095));
#5057=EDGE_LOOP('',(#24096,#24097,#24098,#24099));
#5058=EDGE_LOOP('',(#24100,#24101,#24102,#24103));
#5059=EDGE_LOOP('',(#24104,#24105,#24106));
#5060=EDGE_LOOP('',(#24107,#24108,#24109,#24110));
#5061=EDGE_LOOP('',(#24111,#24112,#24113,#24114));
#5062=EDGE_LOOP('',(#24115,#24116,#24117));
#5063=EDGE_LOOP('',(#24118,#24119,#24120,#24121));
#5064=EDGE_LOOP('',(#24122,#24123,#24124,#24125));
#5065=EDGE_LOOP('',(#24126,#24127,#24128));
#5066=EDGE_LOOP('',(#24129,#24130,#24131,#24132));
#5067=EDGE_LOOP('',(#24133,#24134,#24135,#24136));
#5068=EDGE_LOOP('',(#24137,#24138,#24139));
#5069=EDGE_LOOP('',(#24140,#24141,#24142,#24143));
#5070=EDGE_LOOP('',(#24144,#24145,#24146,#24147));
#5071=EDGE_LOOP('',(#24148,#24149,#24150));
#5072=EDGE_LOOP('',(#24151,#24152,#24153,#24154));
#5073=EDGE_LOOP('',(#24155,#24156,#24157,#24158));
#5074=EDGE_LOOP('',(#24159,#24160,#24161));
#5075=EDGE_LOOP('',(#24162,#24163,#24164,#24165));
#5076=EDGE_LOOP('',(#24166,#24167,#24168,#24169));
#5077=EDGE_LOOP('',(#24170,#24171,#24172));
#5078=EDGE_LOOP('',(#24173,#24174,#24175,#24176,#24177,#24178,#24179,#24180,
#24181,#24182,#24183,#24184,#24185,#24186,#24187,#24188,#24189,#24190,#24191,
#24192,#24193,#24194,#24195,#24196,#24197,#24198,#24199,#24200,#24201,#24202,
#24203,#24204,#24205,#24206,#24207,#24208,#24209,#24210,#24211,#24212,#24213,
#24214,#24215,#24216,#24217,#24218,#24219,#24220,#24221,#24222,#24223,#24224,
#24225,#24226,#24227,#24228,#24229,#24230,#24231,#24232,#24233,#24234,#24235,
#24236,#24237,#24238,#24239,#24240,#24241,#24242,#24243,#24244,#24245,#24246,
#24247,#24248,#24249,#24250,#24251,#24252,#24253,#24254,#24255,#24256,#24257,
#24258,#24259,#24260,#24261,#24262,#24263,#24264,#24265,#24266,#24267,#24268,
#24269,#24270,#24271,#24272,#24273,#24274,#24275,#24276,#24277,#24278,#24279,
#24280,#24281,#24282,#24283,#24284,#24285,#24286,#24287,#24288,#24289,#24290,
#24291,#24292,#24293,#24294,#24295,#24296,#24297,#24298,#24299,#24300,#24301,
#24302,#24303,#24304,#24305,#24306,#24307,#24308,#24309,#24310,#24311,#24312,
#24313,#24314,#24315,#24316,#24317,#24318,#24319,#24320));
#5079=EDGE_LOOP('',(#24321));
#5080=EDGE_LOOP('',(#24322,#24323,#24324,#24325,#24326,#24327));
#5081=EDGE_LOOP('',(#24328,#24329));
#5082=EDGE_LOOP('',(#24330,#24331));
#5083=EDGE_LOOP('',(#24332,#24333));
#5084=EDGE_LOOP('',(#24334,#24335));
#5085=EDGE_LOOP('',(#24336,#24337));
#5086=EDGE_LOOP('',(#24338,#24339));
#5087=EDGE_LOOP('',(#24340,#24341,#24342,#24343,#24344,#24345,#24346,#24347));
#5088=EDGE_LOOP('',(#24348,#24349,#24350,#24351));
#5089=EDGE_LOOP('',(#24352,#24353,#24354,#24355));
#5090=EDGE_LOOP('',(#24356,#24357,#24358,#24359));
#5091=EDGE_LOOP('',(#24360,#24361,#24362,#24363));
#5092=EDGE_LOOP('',(#24364,#24365,#24366,#24367));
#5093=EDGE_LOOP('',(#24368,#24369,#24370,#24371));
#5094=EDGE_LOOP('',(#24372,#24373,#24374,#24375));
#5095=EDGE_LOOP('',(#24376,#24377,#24378,#24379));
#5096=EDGE_LOOP('',(#24380,#24381,#24382,#24383,#24384,#24385));
#5097=EDGE_LOOP('',(#24386,#24387,#24388,#24389,#24390));
#5098=EDGE_LOOP('',(#24391,#24392,#24393,#24394,#24395,#24396));
#5099=EDGE_LOOP('',(#24397,#24398,#24399,#24400));
#5100=EDGE_LOOP('',(#24401,#24402,#24403,#24404,#24405,#24406));
#5101=EDGE_LOOP('',(#24407,#24408,#24409,#24410));
#5102=EDGE_LOOP('',(#24411,#24412,#24413,#24414,#24415,#24416));
#5103=EDGE_LOOP('',(#24417,#24418,#24419,#24420,#24421));
#5104=EDGE_LOOP('',(#24422,#24423,#24424,#24425,#24426,#24427));
#5105=EDGE_LOOP('',(#24428,#24429,#24430,#24431,#24432));
#5106=EDGE_LOOP('',(#24433,#24434,#24435,#24436,#24437));
#5107=EDGE_LOOP('',(#24438,#24439,#24440,#24441,#24442));
#5108=EDGE_LOOP('',(#24443,#24444,#24445,#24446,#24447));
#5109=EDGE_LOOP('',(#24448,#24449,#24450,#24451));
#5110=EDGE_LOOP('',(#24452,#24453,#24454,#24455,#24456,#24457));
#5111=EDGE_LOOP('',(#24458,#24459,#24460,#24461,#24462));
#5112=EDGE_LOOP('',(#24463,#24464,#24465,#24466,#24467,#24468));
#5113=EDGE_LOOP('',(#24469,#24470,#24471,#24472,#24473,#24474,#24475,#24476,
#24477,#24478,#24479,#24480,#24481,#24482,#24483,#24484,#24485,#24486,#24487,
#24488,#24489,#24490,#24491,#24492,#24493,#24494,#24495,#24496,#24497,#24498,
#24499,#24500,#24501,#24502,#24503,#24504,#24505,#24506,#24507,#24508,#24509,
#24510,#24511,#24512));
#5114=EDGE_LOOP('',(#24513,#24514,#24515,#24516));
#5115=EDGE_LOOP('',(#24517,#24518,#24519,#24520,#24521,#24522));
#5116=EDGE_LOOP('',(#24523,#24524,#24525,#24526,#24527,#24528,#24529,#24530,
#24531,#24532,#24533,#24534,#24535,#24536,#24537,#24538,#24539,#24540,#24541,
#24542,#24543,#24544,#24545,#24546,#24547,#24548,#24549,#24550,#24551,#24552,
#24553,#24554,#24555,#24556,#24557,#24558,#24559,#24560,#24561,#24562,#24563,
#24564,#24565,#24566,#24567,#24568,#24569,#24570,#24571,#24572,#24573,#24574,
#24575,#24576,#24577,#24578));
#5117=EDGE_LOOP('',(#24579,#24580,#24581,#24582,#24583,#24584));
#5118=EDGE_LOOP('',(#24585,#24586,#24587,#24588,#24589,#24590,#24591,#24592,
#24593,#24594,#24595,#24596,#24597,#24598,#24599,#24600,#24601,#24602,#24603,
#24604,#24605,#24606,#24607,#24608,#24609,#24610,#24611,#24612,#24613,#24614,
#24615,#24616,#24617,#24618,#24619,#24620,#24621,#24622,#24623,#24624,#24625,
#24626,#24627,#24628,#24629,#24630,#24631,#24632,#24633,#24634,#24635,#24636,
#24637,#24638,#24639));
#5119=EDGE_LOOP('',(#24640,#24641,#24642,#24643,#24644,#24645,#24646));
#5120=EDGE_LOOP('',(#24647));
#5121=EDGE_LOOP('',(#24648));
#5122=EDGE_LOOP('',(#24649,#24650,#24651,#24652,#24653,#24654,#24655));
#5123=EDGE_LOOP('',(#24656));
#5124=EDGE_LOOP('',(#24657,#24658,#24659,#24660));
#5125=EDGE_LOOP('',(#24661,#24662,#24663,#24664));
#5126=EDGE_LOOP('',(#24665,#24666,#24667));
#5127=EDGE_LOOP('',(#24668,#24669,#24670,#24671,#24672,#24673,#24674,#24675,
#24676,#24677,#24678,#24679,#24680,#24681,#24682,#24683,#24684,#24685,#24686,
#24687,#24688,#24689,#24690,#24691,#24692,#24693,#24694,#24695,#24696,#24697,
#24698,#24699,#24700,#24701,#24702,#24703,#24704,#24705,#24706,#24707,#24708,
#24709,#24710,#24711,#24712,#24713,#24714,#24715,#24716,#24717,#24718,#24719,
#24720,#24721,#24722,#24723,#24724,#24725,#24726,#24727,#24728,#24729,#24730,
#24731,#24732,#24733,#24734,#24735,#24736,#24737,#24738,#24739,#24740,#24741,
#24742,#24743,#24744,#24745,#24746,#24747,#24748,#24749,#24750,#24751,#24752,
#24753,#24754,#24755,#24756,#24757,#24758,#24759,#24760,#24761,#24762,#24763,
#24764,#24765,#24766,#24767,#24768,#24769,#24770,#24771,#24772,#24773,#24774,
#24775,#24776,#24777,#24778));
#5128=EDGE_LOOP('',(#24779,#24780,#24781,#24782));
#5129=EDGE_LOOP('',(#24783,#24784,#24785,#24786));
#5130=EDGE_LOOP('',(#24787,#24788,#24789));
#5131=EDGE_LOOP('',(#24790,#24791,#24792,#24793));
#5132=EDGE_LOOP('',(#24794,#24795,#24796,#24797));
#5133=EDGE_LOOP('',(#24798,#24799,#24800));
#5134=EDGE_LOOP('',(#24801,#24802,#24803,#24804));
#5135=EDGE_LOOP('',(#24805,#24806,#24807,#24808));
#5136=EDGE_LOOP('',(#24809,#24810,#24811));
#5137=EDGE_LOOP('',(#24812,#24813,#24814,#24815));
#5138=EDGE_LOOP('',(#24816,#24817,#24818,#24819));
#5139=EDGE_LOOP('',(#24820,#24821,#24822));
#5140=EDGE_LOOP('',(#24823,#24824,#24825,#24826));
#5141=EDGE_LOOP('',(#24827,#24828,#24829,#24830));
#5142=EDGE_LOOP('',(#24831,#24832,#24833));
#5143=EDGE_LOOP('',(#24834,#24835,#24836,#24837));
#5144=EDGE_LOOP('',(#24838,#24839,#24840,#24841));
#5145=EDGE_LOOP('',(#24842,#24843,#24844));
#5146=EDGE_LOOP('',(#24845,#24846,#24847,#24848));
#5147=EDGE_LOOP('',(#24849,#24850,#24851,#24852));
#5148=EDGE_LOOP('',(#24853,#24854,#24855));
#5149=EDGE_LOOP('',(#24856,#24857,#24858,#24859));
#5150=EDGE_LOOP('',(#24860,#24861,#24862,#24863));
#5151=EDGE_LOOP('',(#24864,#24865,#24866));
#5152=EDGE_LOOP('',(#24867,#24868,#24869,#24870));
#5153=EDGE_LOOP('',(#24871,#24872,#24873,#24874));
#5154=EDGE_LOOP('',(#24875,#24876,#24877));
#5155=EDGE_LOOP('',(#24878,#24879,#24880,#24881));
#5156=EDGE_LOOP('',(#24882,#24883,#24884,#24885));
#5157=EDGE_LOOP('',(#24886,#24887,#24888));
#5158=EDGE_LOOP('',(#24889,#24890,#24891,#24892));
#5159=EDGE_LOOP('',(#24893,#24894,#24895,#24896));
#5160=EDGE_LOOP('',(#24897,#24898,#24899));
#5161=EDGE_LOOP('',(#24900,#24901,#24902,#24903));
#5162=EDGE_LOOP('',(#24904,#24905,#24906,#24907));
#5163=EDGE_LOOP('',(#24908,#24909,#24910));
#5164=EDGE_LOOP('',(#24911,#24912,#24913,#24914));
#5165=EDGE_LOOP('',(#24915,#24916,#24917,#24918));
#5166=EDGE_LOOP('',(#24919,#24920,#24921));
#5167=EDGE_LOOP('',(#24922,#24923,#24924,#24925));
#5168=EDGE_LOOP('',(#24926,#24927,#24928,#24929));
#5169=EDGE_LOOP('',(#24930,#24931,#24932));
#5170=EDGE_LOOP('',(#24933,#24934,#24935,#24936));
#5171=EDGE_LOOP('',(#24937,#24938,#24939,#24940));
#5172=EDGE_LOOP('',(#24941,#24942,#24943));
#5173=EDGE_LOOP('',(#24944,#24945,#24946,#24947));
#5174=EDGE_LOOP('',(#24948,#24949,#24950,#24951));
#5175=EDGE_LOOP('',(#24952,#24953,#24954));
#5176=EDGE_LOOP('',(#24955,#24956,#24957,#24958));
#5177=EDGE_LOOP('',(#24959,#24960,#24961,#24962));
#5178=EDGE_LOOP('',(#24963,#24964,#24965,#24966));
#5179=EDGE_LOOP('',(#24967,#24968,#24969,#24970));
#5180=EDGE_LOOP('',(#24971,#24972,#24973,#24974));
#5181=EDGE_LOOP('',(#24975,#24976,#24977));
#5182=EDGE_LOOP('',(#24978,#24979,#24980,#24981));
#5183=EDGE_LOOP('',(#24982,#24983,#24984,#24985));
#5184=EDGE_LOOP('',(#24986,#24987,#24988));
#5185=EDGE_LOOP('',(#24989,#24990,#24991,#24992));
#5186=EDGE_LOOP('',(#24993,#24994,#24995,#24996));
#5187=EDGE_LOOP('',(#24997,#24998,#24999));
#5188=EDGE_LOOP('',(#25000,#25001,#25002,#25003));
#5189=EDGE_LOOP('',(#25004,#25005,#25006,#25007));
#5190=EDGE_LOOP('',(#25008,#25009,#25010));
#5191=EDGE_LOOP('',(#25011,#25012,#25013,#25014));
#5192=EDGE_LOOP('',(#25015,#25016,#25017,#25018));
#5193=EDGE_LOOP('',(#25019,#25020,#25021));
#5194=EDGE_LOOP('',(#25022,#25023,#25024,#25025));
#5195=EDGE_LOOP('',(#25026,#25027,#25028,#25029));
#5196=EDGE_LOOP('',(#25030,#25031,#25032));
#5197=EDGE_LOOP('',(#25033,#25034,#25035,#25036));
#5198=EDGE_LOOP('',(#25037,#25038,#25039,#25040));
#5199=EDGE_LOOP('',(#25041,#25042,#25043));
#5200=EDGE_LOOP('',(#25044,#25045,#25046,#25047));
#5201=EDGE_LOOP('',(#25048,#25049,#25050,#25051));
#5202=EDGE_LOOP('',(#25052,#25053,#25054));
#5203=EDGE_LOOP('',(#25055,#25056,#25057,#25058));
#5204=EDGE_LOOP('',(#25059,#25060,#25061,#25062));
#5205=EDGE_LOOP('',(#25063,#25064,#25065));
#5206=EDGE_LOOP('',(#25066,#25067,#25068,#25069));
#5207=EDGE_LOOP('',(#25070,#25071,#25072,#25073));
#5208=EDGE_LOOP('',(#25074,#25075,#25076));
#5209=EDGE_LOOP('',(#25077,#25078,#25079,#25080));
#5210=EDGE_LOOP('',(#25081,#25082,#25083,#25084));
#5211=EDGE_LOOP('',(#25085,#25086,#25087));
#5212=EDGE_LOOP('',(#25088,#25089,#25090,#25091));
#5213=EDGE_LOOP('',(#25092,#25093,#25094,#25095));
#5214=EDGE_LOOP('',(#25096,#25097,#25098));
#5215=EDGE_LOOP('',(#25099,#25100,#25101,#25102));
#5216=EDGE_LOOP('',(#25103,#25104,#25105,#25106));
#5217=EDGE_LOOP('',(#25107,#25108,#25109));
#5218=EDGE_LOOP('',(#25110,#25111,#25112,#25113));
#5219=EDGE_LOOP('',(#25114,#25115,#25116,#25117));
#5220=EDGE_LOOP('',(#25118,#25119,#25120));
#5221=EDGE_LOOP('',(#25121,#25122,#25123,#25124));
#5222=EDGE_LOOP('',(#25125,#25126,#25127,#25128));
#5223=EDGE_LOOP('',(#25129,#25130,#25131));
#5224=EDGE_LOOP('',(#25132,#25133,#25134,#25135));
#5225=EDGE_LOOP('',(#25136,#25137,#25138,#25139));
#5226=EDGE_LOOP('',(#25140,#25141,#25142));
#5227=EDGE_LOOP('',(#25143,#25144,#25145,#25146));
#5228=EDGE_LOOP('',(#25147,#25148,#25149,#25150));
#5229=EDGE_LOOP('',(#25151,#25152,#25153));
#5230=EDGE_LOOP('',(#25154,#25155,#25156,#25157));
#5231=EDGE_LOOP('',(#25158,#25159,#25160,#25161));
#5232=EDGE_LOOP('',(#25162,#25163,#25164));
#5233=EDGE_LOOP('',(#25165,#25166,#25167,#25168,#25169,#25170,#25171,#25172,
#25173,#25174,#25175,#25176,#25177,#25178,#25179,#25180,#25181,#25182,#25183,
#25184,#25185,#25186,#25187,#25188,#25189,#25190,#25191,#25192,#25193,#25194,
#25195,#25196,#25197,#25198,#25199,#25200,#25201,#25202,#25203,#25204,#25205,
#25206,#25207,#25208,#25209,#25210,#25211,#25212,#25213,#25214,#25215,#25216,
#25217,#25218,#25219,#25220,#25221,#25222,#25223,#25224,#25225,#25226,#25227,
#25228,#25229,#25230,#25231,#25232,#25233,#25234,#25235,#25236,#25237,#25238,
#25239,#25240,#25241,#25242,#25243,#25244,#25245,#25246,#25247,#25248,#25249,
#25250,#25251,#25252,#25253,#25254,#25255,#25256,#25257,#25258,#25259,#25260,
#25261,#25262,#25263,#25264,#25265,#25266,#25267,#25268,#25269,#25270,#25271,
#25272,#25273,#25274,#25275,#25276,#25277,#25278,#25279,#25280,#25281,#25282,
#25283,#25284,#25285,#25286,#25287,#25288,#25289,#25290,#25291,#25292,#25293,
#25294,#25295,#25296,#25297,#25298,#25299,#25300,#25301,#25302,#25303,#25304,
#25305,#25306,#25307,#25308,#25309,#25310,#25311,#25312));
#5234=EDGE_LOOP('',(#25313));
#5235=EDGE_LOOP('',(#25314,#25315,#25316,#25317,#25318,#25319));
#5236=EDGE_LOOP('',(#25320,#25321));
#5237=EDGE_LOOP('',(#25322,#25323));
#5238=EDGE_LOOP('',(#25324,#25325));
#5239=EDGE_LOOP('',(#25326,#25327));
#5240=EDGE_LOOP('',(#25328,#25329));
#5241=EDGE_LOOP('',(#25330,#25331));
#5242=EDGE_LOOP('',(#25332,#25333,#25334,#25335,#25336,#25337,#25338,#25339));
#5243=EDGE_LOOP('',(#25340,#25341,#25342,#25343));
#5244=EDGE_LOOP('',(#25344,#25345,#25346,#25347));
#5245=EDGE_LOOP('',(#25348,#25349,#25350,#25351));
#5246=EDGE_LOOP('',(#25352,#25353,#25354,#25355));
#5247=EDGE_LOOP('',(#25356,#25357,#25358,#25359));
#5248=EDGE_LOOP('',(#25360,#25361,#25362,#25363));
#5249=EDGE_LOOP('',(#25364,#25365,#25366,#25367));
#5250=EDGE_LOOP('',(#25368));
#5251=EDGE_LOOP('',(#25369));
#5252=EDGE_LOOP('',(#25370,#25371,#25372,#25373));
#5253=EDGE_LOOP('',(#25374,#25375,#25376,#25377));
#5254=EDGE_LOOP('',(#25378));
#5255=EDGE_LOOP('',(#25379));
#5256=EDGE_LOOP('',(#25380,#25381,#25382,#25383));
#5257=EDGE_LOOP('',(#25384,#25385,#25386,#25387));
#5258=EDGE_LOOP('',(#25388,#25389,#25390,#25391));
#5259=EDGE_LOOP('',(#25392));
#5260=EDGE_LOOP('',(#25393));
#5261=EDGE_LOOP('',(#25394,#25395,#25396,#25397));
#5262=EDGE_LOOP('',(#25398,#25399,#25400,#25401));
#5263=EDGE_LOOP('',(#25402));
#5264=EDGE_LOOP('',(#25403));
#5265=EDGE_LOOP('',(#25404,#25405,#25406,#25407));
#5266=EDGE_LOOP('',(#25408));
#5267=EDGE_LOOP('',(#25409));
#5268=EDGE_LOOP('',(#25410,#25411,#25412,#25413,#25414,#25415,#25416,#25417,
#25418));
#5269=EDGE_LOOP('',(#25419,#25420,#25421,#25422));
#5270=EDGE_LOOP('',(#25423,#25424,#25425,#25426));
#5271=EDGE_LOOP('',(#25427,#25428,#25429,#25430));
#5272=EDGE_LOOP('',(#25431,#25432,#25433,#25434));
#5273=EDGE_LOOP('',(#25435,#25436,#25437,#25438));
#5274=EDGE_LOOP('',(#25439,#25440,#25441,#25442));
#5275=EDGE_LOOP('',(#25443,#25444,#25445,#25446,#25447,#25448));
#5276=EDGE_LOOP('',(#25449));
#5277=LINE('',#36086,#7788);
#5278=LINE('',#36090,#7789);
#5279=LINE('',#36097,#7790);
#5280=LINE('',#36099,#7791);
#5281=LINE('',#36101,#7792);
#5282=LINE('',#36102,#7793);
#5283=LINE('',#36107,#7794);
#5284=LINE('',#36111,#7795);
#5285=LINE('',#36118,#7796);
#5286=LINE('',#36120,#7797);
#5287=LINE('',#36122,#7798);
#5288=LINE('',#36123,#7799);
#5289=LINE('',#36126,#7800);
#5290=LINE('',#36129,#7801);
#5291=LINE('',#36134,#7802);
#5292=LINE('',#36138,#7803);
#5293=LINE('',#36145,#7804);
#5294=LINE('',#36147,#7805);
#5295=LINE('',#36149,#7806);
#5296=LINE('',#36150,#7807);
#5297=LINE('',#36155,#7808);
#5298=LINE('',#36159,#7809);
#5299=LINE('',#36166,#7810);
#5300=LINE('',#36168,#7811);
#5301=LINE('',#36170,#7812);
#5302=LINE('',#36171,#7813);
#5303=LINE('',#36174,#7814);
#5304=LINE('',#36177,#7815);
#5305=LINE('',#36182,#7816);
#5306=LINE('',#36188,#7817);
#5307=LINE('',#36194,#7818);
#5308=LINE('',#36200,#7819);
#5309=LINE('',#36206,#7820);
#5310=LINE('',#36211,#7821);
#5311=LINE('',#36213,#7822);
#5312=LINE('',#36215,#7823);
#5313=LINE('',#36217,#7824);
#5314=LINE('',#36219,#7825);
#5315=LINE('',#36221,#7826);
#5316=LINE('',#36223,#7827);
#5317=LINE('',#36225,#7828);
#5318=LINE('',#36227,#7829);
#5319=LINE('',#36229,#7830);
#5320=LINE('',#36231,#7831);
#5321=LINE('',#36233,#7832);
#5322=LINE('',#36235,#7833);
#5323=LINE('',#36237,#7834);
#5324=LINE('',#36239,#7835);
#5325=LINE('',#36241,#7836);
#5326=LINE('',#36243,#7837);
#5327=LINE('',#36245,#7838);
#5328=LINE('',#36247,#7839);
#5329=LINE('',#36248,#7840);
#5330=LINE('',#36259,#7841);
#5331=LINE('',#36264,#7842);
#5332=LINE('',#36267,#7843);
#5333=LINE('',#36272,#7844);
#5334=LINE('',#36275,#7845);
#5335=LINE('',#36280,#7846);
#5336=LINE('',#36283,#7847);
#5337=LINE('',#36288,#7848);
#5338=LINE('',#36291,#7849);
#5339=LINE('',#36295,#7850);
#5340=LINE('',#36297,#7851);
#5341=LINE('',#36298,#7852);
#5342=LINE('',#36300,#7853);
#5343=LINE('',#36301,#7854);
#5344=LINE('',#36303,#7855);
#5345=LINE('',#36307,#7856);
#5346=LINE('',#36308,#7857);
#5347=LINE('',#36309,#7858);
#5348=LINE('',#36312,#7859);
#5349=LINE('',#36313,#7860);
#5350=LINE('',#36315,#7861);
#5351=LINE('',#36317,#7862);
#5352=LINE('',#36318,#7863);
#5353=LINE('',#36320,#7864);
#5354=LINE('',#36324,#7865);
#5355=LINE('',#36325,#7866);
#5356=LINE('',#36326,#7867);
#5357=LINE('',#36329,#7868);
#5358=LINE('',#36330,#7869);
#5359=LINE('',#36333,#7870);
#5360=LINE('',#36334,#7871);
#5361=LINE('',#36336,#7872);
#5362=LINE('',#36338,#7873);
#5363=LINE('',#36339,#7874);
#5364=LINE('',#36341,#7875);
#5365=LINE('',#36343,#7876);
#5366=LINE('',#36345,#7877);
#5367=LINE('',#36347,#7878);
#5368=LINE('',#36348,#7879);
#5369=LINE('',#36350,#7880);
#5370=LINE('',#36353,#7881);
#5371=LINE('',#36354,#7882);
#5372=LINE('',#36357,#7883);
#5373=LINE('',#36358,#7884);
#5374=LINE('',#36360,#7885);
#5375=LINE('',#36363,#7886);
#5376=LINE('',#36364,#7887);
#5377=LINE('',#36367,#7888);
#5378=LINE('',#36368,#7889);
#5379=LINE('',#36371,#7890);
#5380=LINE('',#36372,#7891);
#5381=LINE('',#36374,#7892);
#5382=LINE('',#36377,#7893);
#5383=LINE('',#36378,#7894);
#5384=LINE('',#36381,#7895);
#5385=LINE('',#36382,#7896);
#5386=LINE('',#36385,#7897);
#5387=LINE('',#36386,#7898);
#5388=LINE('',#36389,#7899);
#5389=LINE('',#36390,#7900);
#5390=LINE('',#36393,#7901);
#5391=LINE('',#36395,#7902);
#5392=LINE('',#36396,#7903);
#5393=LINE('',#36399,#7904);
#5394=LINE('',#36400,#7905);
#5395=LINE('',#36402,#7906);
#5396=LINE('',#36404,#7907);
#5397=LINE('',#36406,#7908);
#5398=LINE('',#36409,#7909);
#5399=LINE('',#36411,#7910);
#5400=LINE('',#36412,#7911);
#5401=LINE('',#36414,#7912);
#5402=LINE('',#36415,#7913);
#5403=LINE('',#36423,#7914);
#5404=LINE('',#36428,#7915);
#5405=LINE('',#36432,#7916);
#5406=LINE('',#36436,#7917);
#5407=LINE('',#36438,#7918);
#5408=LINE('',#36440,#7919);
#5409=LINE('',#36442,#7920);
#5410=LINE('',#36444,#7921);
#5411=LINE('',#36446,#7922);
#5412=LINE('',#36448,#7923);
#5413=LINE('',#36450,#7924);
#5414=LINE('',#36452,#7925);
#5415=LINE('',#36456,#7926);
#5416=LINE('',#36460,#7927);
#5417=LINE('',#36462,#7928);
#5418=LINE('',#36464,#7929);
#5419=LINE('',#36466,#7930);
#5420=LINE('',#36468,#7931);
#5421=LINE('',#36470,#7932);
#5422=LINE('',#36472,#7933);
#5423=LINE('',#36473,#7934);
#5424=LINE('',#36488,#7935);
#5425=LINE('',#36490,#7936);
#5426=LINE('',#36494,#7937);
#5427=LINE('',#36498,#7938);
#5428=LINE('',#36500,#7939);
#5429=LINE('',#36504,#7940);
#5430=LINE('',#36506,#7941);
#5431=LINE('',#36510,#7942);
#5432=LINE('',#36514,#7943);
#5433=LINE('',#36516,#7944);
#5434=LINE('',#36523,#7945);
#5435=LINE('',#36527,#7946);
#5436=LINE('',#36531,#7947);
#5437=LINE('',#36535,#7948);
#5438=LINE('',#36539,#7949);
#5439=LINE('',#36543,#7950);
#5440=LINE('',#36547,#7951);
#5441=LINE('',#36552,#7952);
#5442=LINE('',#36557,#7953);
#5443=LINE('',#36561,#7954);
#5444=LINE('',#36565,#7955);
#5445=LINE('',#36567,#7956);
#5446=LINE('',#36569,#7957);
#5447=LINE('',#36571,#7958);
#5448=LINE('',#36573,#7959);
#5449=LINE('',#36575,#7960);
#5450=LINE('',#36577,#7961);
#5451=LINE('',#36579,#7962);
#5452=LINE('',#36581,#7963);
#5453=LINE('',#36585,#7964);
#5454=LINE('',#36589,#7965);
#5455=LINE('',#36591,#7966);
#5456=LINE('',#36593,#7967);
#5457=LINE('',#36595,#7968);
#5458=LINE('',#36597,#7969);
#5459=LINE('',#36599,#7970);
#5460=LINE('',#36601,#7971);
#5461=LINE('',#36602,#7972);
#5462=LINE('',#36607,#7973);
#5463=LINE('',#36611,#7974);
#5464=LINE('',#36615,#7975);
#5465=LINE('',#36617,#7976);
#5466=LINE('',#36621,#7977);
#5467=LINE('',#36623,#7978);
#5468=LINE('',#36627,#7979);
#5469=LINE('',#36631,#7980);
#5470=LINE('',#36633,#7981);
#5471=LINE('',#36636,#7982);
#5472=LINE('',#36642,#7983);
#5473=LINE('',#36646,#7984);
#5474=LINE('',#36648,#7985);
#5475=LINE('',#36652,#7986);
#5476=LINE('',#36654,#7987);
#5477=LINE('',#36658,#7988);
#5478=LINE('',#36660,#7989);
#5479=LINE('',#36663,#7990);
#5480=LINE('',#36665,#7991);
#5481=LINE('',#36666,#7992);
#5482=LINE('',#36669,#7993);
#5483=LINE('',#36670,#7994);
#5484=LINE('',#36673,#7995);
#5485=LINE('',#36674,#7996);
#5486=LINE('',#36677,#7997);
#5487=LINE('',#36678,#7998);
#5488=LINE('',#36682,#7999);
#5489=LINE('',#36683,#8000);
#5490=LINE('',#36684,#8001);
#5491=LINE('',#36687,#8002);
#5492=LINE('',#36688,#8003);
#5493=LINE('',#36691,#8004);
#5494=LINE('',#36692,#8005);
#5495=LINE('',#36695,#8006);
#5496=LINE('',#36696,#8007);
#5497=LINE('',#36699,#8008);
#5498=LINE('',#36700,#8009);
#5499=LINE('',#36703,#8010);
#5500=LINE('',#36704,#8011);
#5501=LINE('',#36707,#8012);
#5502=LINE('',#36708,#8013);
#5503=LINE('',#36711,#8014);
#5504=LINE('',#36712,#8015);
#5505=LINE('',#36716,#8016);
#5506=LINE('',#36717,#8017);
#5507=LINE('',#36718,#8018);
#5508=LINE('',#36721,#8019);
#5509=LINE('',#36725,#8020);
#5510=LINE('',#36726,#8021);
#5511=LINE('',#36729,#8022);
#5512=LINE('',#36732,#8023);
#5513=LINE('',#36735,#8024);
#5514=LINE('',#36739,#8025);
#5515=LINE('',#36740,#8026);
#5516=LINE('',#36743,#8027);
#5517=LINE('',#36746,#8028);
#5518=LINE('',#36749,#8029);
#5519=LINE('',#36750,#8030);
#5520=LINE('',#36753,#8031);
#5521=LINE('',#36754,#8032);
#5522=LINE('',#36756,#8033);
#5523=LINE('',#36758,#8034);
#5524=LINE('',#36759,#8035);
#5525=LINE('',#36761,#8036);
#5526=LINE('',#36763,#8037);
#5527=LINE('',#36765,#8038);
#5528=LINE('',#36767,#8039);
#5529=LINE('',#36769,#8040);
#5530=LINE('',#36771,#8041);
#5531=LINE('',#36773,#8042);
#5532=LINE('',#36775,#8043);
#5533=LINE('',#36777,#8044);
#5534=LINE('',#36779,#8045);
#5535=LINE('',#36781,#8046);
#5536=LINE('',#36785,#8047);
#5537=LINE('',#36786,#8048);
#5538=LINE('',#36787,#8049);
#5539=LINE('',#36791,#8050);
#5540=LINE('',#36792,#8051);
#5541=LINE('',#36793,#8052);
#5542=LINE('',#36797,#8053);
#5543=LINE('',#36798,#8054);
#5544=LINE('',#36799,#8055);
#5545=LINE('',#36802,#8056);
#5546=LINE('',#36805,#8057);
#5547=LINE('',#36809,#8058);
#5548=LINE('',#36810,#8059);
#5549=LINE('',#36811,#8060);
#5550=LINE('',#36814,#8061);
#5551=LINE('',#36818,#8062);
#5552=LINE('',#36819,#8063);
#5553=LINE('',#36822,#8064);
#5554=LINE('',#36825,#8065);
#5555=LINE('',#36828,#8066);
#5556=LINE('',#36832,#8067);
#5557=LINE('',#36833,#8068);
#5558=LINE('',#36836,#8069);
#5559=LINE('',#36839,#8070);
#5560=LINE('',#36842,#8071);
#5561=LINE('',#36845,#8072);
#5562=LINE('',#36847,#8073);
#5563=LINE('',#36848,#8074);
#5564=LINE('',#36850,#8075);
#5565=LINE('',#36852,#8076);
#5566=LINE('',#36854,#8077);
#5567=LINE('',#36856,#8078);
#5568=LINE('',#36858,#8079);
#5569=LINE('',#36860,#8080);
#5570=LINE('',#36862,#8081);
#5571=LINE('',#36864,#8082);
#5572=LINE('',#36866,#8083);
#5573=LINE('',#36867,#8084);
#5574=LINE('',#36870,#8085);
#5575=LINE('',#36872,#8086);
#5576=LINE('',#36874,#8087);
#5577=LINE('',#36876,#8088);
#5578=LINE('',#36879,#8089);
#5579=LINE('',#36881,#8090);
#5580=LINE('',#36882,#8091);
#5581=LINE('',#36885,#8092);
#5582=LINE('',#36887,#8093);
#5583=LINE('',#36888,#8094);
#5584=LINE('',#36890,#8095);
#5585=LINE('',#36893,#8096);
#5586=LINE('',#36895,#8097);
#5587=LINE('',#36897,#8098);
#5588=LINE('',#36899,#8099);
#5589=LINE('',#36906,#8100);
#5590=LINE('',#36913,#8101);
#5591=LINE('',#36919,#8102);
#5592=LINE('',#36925,#8103);
#5593=LINE('',#36931,#8104);
#5594=LINE('',#36937,#8105);
#5595=LINE('',#36941,#8106);
#5596=LINE('',#36948,#8107);
#5597=LINE('',#36953,#8108);
#5598=LINE('',#36956,#8109);
#5599=LINE('',#36961,#8110);
#5600=LINE('',#36967,#8111);
#5601=LINE('',#36971,#8112);
#5602=LINE('',#36973,#8113);
#5603=LINE('',#36975,#8114);
#5604=LINE('',#36976,#8115);
#5605=LINE('',#36982,#8116);
#5606=LINE('',#36988,#8117);
#5607=LINE('',#36991,#8118);
#5608=LINE('',#36994,#8119);
#5609=LINE('',#36996,#8120);
#5610=LINE('',#36997,#8121);
#5611=LINE('',#37003,#8122);
#5612=LINE('',#37008,#8123);
#5613=LINE('',#37011,#8124);
#5614=LINE('',#37012,#8125);
#5615=LINE('',#37015,#8126);
#5616=LINE('',#37019,#8127);
#5617=LINE('',#37022,#8128);
#5618=LINE('',#37025,#8129);
#5619=LINE('',#37029,#8130);
#5620=LINE('',#37032,#8131);
#5621=LINE('',#37038,#8132);
#5622=LINE('',#37042,#8133);
#5623=LINE('',#37046,#8134);
#5624=LINE('',#37049,#8135);
#5625=LINE('',#37051,#8136);
#5626=LINE('',#37052,#8137);
#5627=LINE('',#37054,#8138);
#5628=LINE('',#37057,#8139);
#5629=LINE('',#37059,#8140);
#5630=LINE('',#37060,#8141);
#5631=LINE('',#37064,#8142);
#5632=LINE('',#37067,#8143);
#5633=LINE('',#37068,#8144);
#5634=LINE('',#37072,#8145);
#5635=LINE('',#37075,#8146);
#5636=LINE('',#37076,#8147);
#5637=LINE('',#37077,#8148);
#5638=LINE('',#37084,#8149);
#5639=LINE('',#37089,#8150);
#5640=LINE('',#37094,#8151);
#5641=LINE('',#37095,#8152);
#5642=LINE('',#37096,#8153);
#5643=LINE('',#37102,#8154);
#5644=LINE('',#37105,#8155);
#5645=LINE('',#37107,#8156);
#5646=LINE('',#37108,#8157);
#5647=LINE('',#37113,#8158);
#5648=LINE('',#37116,#8159);
#5649=LINE('',#37117,#8160);
#5650=LINE('',#37121,#8161);
#5651=LINE('',#37124,#8162);
#5652=LINE('',#37125,#8163);
#5653=LINE('',#37134,#8164);
#5654=LINE('',#37136,#8165);
#5655=LINE('',#37138,#8166);
#5656=LINE('',#37139,#8167);
#5657=LINE('',#37145,#8168);
#5658=LINE('',#37148,#8169);
#5659=LINE('',#37291,#8170);
#5660=LINE('',#37295,#8171);
#5661=LINE('',#37296,#8172);
#5662=LINE('',#37297,#8173);
#5663=LINE('',#37442,#8174);
#5664=LINE('',#37518,#8175);
#5665=LINE('',#37522,#8176);
#5666=LINE('',#37598,#8177);
#5667=LINE('',#37602,#8178);
#5668=LINE('',#37678,#8179);
#5669=LINE('',#37682,#8180);
#5670=LINE('',#37758,#8181);
#5671=LINE('',#37762,#8182);
#5672=LINE('',#37838,#8183);
#5673=LINE('',#37842,#8184);
#5674=LINE('',#37918,#8185);
#5675=LINE('',#37922,#8186);
#5676=LINE('',#37998,#8187);
#5677=LINE('',#38002,#8188);
#5678=LINE('',#38078,#8189);
#5679=LINE('',#38082,#8190);
#5680=LINE('',#38158,#8191);
#5681=LINE('',#38162,#8192);
#5682=LINE('',#38238,#8193);
#5683=LINE('',#38242,#8194);
#5684=LINE('',#38318,#8195);
#5685=LINE('',#38322,#8196);
#5686=LINE('',#38398,#8197);
#5687=LINE('',#38402,#8198);
#5688=LINE('',#38478,#8199);
#5689=LINE('',#38482,#8200);
#5690=LINE('',#38558,#8201);
#5691=LINE('',#38562,#8202);
#5692=LINE('',#38638,#8203);
#5693=LINE('',#38645,#8204);
#5694=LINE('',#38648,#8205);
#5695=LINE('',#38649,#8206);
#5696=LINE('',#38652,#8207);
#5697=LINE('',#38655,#8208);
#5698=LINE('',#38762,#8209);
#5699=LINE('',#38765,#8210);
#5700=LINE('',#38766,#8211);
#5701=LINE('',#38875,#8212);
#5702=LINE('',#38878,#8213);
#5703=LINE('',#38879,#8214);
#5704=LINE('',#38882,#8215);
#5705=LINE('',#38885,#8216);
#5706=LINE('',#38992,#8217);
#5707=LINE('',#38995,#8218);
#5708=LINE('',#38996,#8219);
#5709=LINE('',#39105,#8220);
#5710=LINE('',#39108,#8221);
#5711=LINE('',#39109,#8222);
#5712=LINE('',#39112,#8223);
#5713=LINE('',#39115,#8224);
#5714=LINE('',#39222,#8225);
#5715=LINE('',#39225,#8226);
#5716=LINE('',#39226,#8227);
#5717=LINE('',#39335,#8228);
#5718=LINE('',#39338,#8229);
#5719=LINE('',#39339,#8230);
#5720=LINE('',#39342,#8231);
#5721=LINE('',#39345,#8232);
#5722=LINE('',#39452,#8233);
#5723=LINE('',#39455,#8234);
#5724=LINE('',#39456,#8235);
#5725=LINE('',#39565,#8236);
#5726=LINE('',#39568,#8237);
#5727=LINE('',#39569,#8238);
#5728=LINE('',#39572,#8239);
#5729=LINE('',#39575,#8240);
#5730=LINE('',#39682,#8241);
#5731=LINE('',#39685,#8242);
#5732=LINE('',#39686,#8243);
#5733=LINE('',#39795,#8244);
#5734=LINE('',#39798,#8245);
#5735=LINE('',#39799,#8246);
#5736=LINE('',#39802,#8247);
#5737=LINE('',#39805,#8248);
#5738=LINE('',#39912,#8249);
#5739=LINE('',#39915,#8250);
#5740=LINE('',#39916,#8251);
#5741=LINE('',#40025,#8252);
#5742=LINE('',#40028,#8253);
#5743=LINE('',#40029,#8254);
#5744=LINE('',#40032,#8255);
#5745=LINE('',#40035,#8256);
#5746=LINE('',#40142,#8257);
#5747=LINE('',#40145,#8258);
#5748=LINE('',#40146,#8259);
#5749=LINE('',#40255,#8260);
#5750=LINE('',#40258,#8261);
#5751=LINE('',#40259,#8262);
#5752=LINE('',#40262,#8263);
#5753=LINE('',#40265,#8264);
#5754=LINE('',#40372,#8265);
#5755=LINE('',#40375,#8266);
#5756=LINE('',#40376,#8267);
#5757=LINE('',#40485,#8268);
#5758=LINE('',#40488,#8269);
#5759=LINE('',#40489,#8270);
#5760=LINE('',#40492,#8271);
#5761=LINE('',#40495,#8272);
#5762=LINE('',#40602,#8273);
#5763=LINE('',#40605,#8274);
#5764=LINE('',#40606,#8275);
#5765=LINE('',#40715,#8276);
#5766=LINE('',#40718,#8277);
#5767=LINE('',#40719,#8278);
#5768=LINE('',#40722,#8279);
#5769=LINE('',#40725,#8280);
#5770=LINE('',#40832,#8281);
#5771=LINE('',#40835,#8282);
#5772=LINE('',#40836,#8283);
#5773=LINE('',#40945,#8284);
#5774=LINE('',#40948,#8285);
#5775=LINE('',#40949,#8286);
#5776=LINE('',#40952,#8287);
#5777=LINE('',#40955,#8288);
#5778=LINE('',#41062,#8289);
#5779=LINE('',#41065,#8290);
#5780=LINE('',#41066,#8291);
#5781=LINE('',#41175,#8292);
#5782=LINE('',#41178,#8293);
#5783=LINE('',#41179,#8294);
#5784=LINE('',#41182,#8295);
#5785=LINE('',#41185,#8296);
#5786=LINE('',#41292,#8297);
#5787=LINE('',#41295,#8298);
#5788=LINE('',#41296,#8299);
#5789=LINE('',#41405,#8300);
#5790=LINE('',#41408,#8301);
#5791=LINE('',#41409,#8302);
#5792=LINE('',#41412,#8303);
#5793=LINE('',#41415,#8304);
#5794=LINE('',#41522,#8305);
#5795=LINE('',#41525,#8306);
#5796=LINE('',#41526,#8307);
#5797=LINE('',#41635,#8308);
#5798=LINE('',#41638,#8309);
#5799=LINE('',#41640,#8310);
#5800=LINE('',#41641,#8311);
#5801=LINE('',#41644,#8312);
#5802=LINE('',#41645,#8313);
#5803=LINE('',#41648,#8314);
#5804=LINE('',#41651,#8315);
#5805=LINE('',#41866,#8316);
#5806=LINE('',#41942,#8317);
#5807=LINE('',#41947,#8318);
#5808=LINE('',#41949,#8319);
#5809=LINE('',#41951,#8320);
#5810=LINE('',#41952,#8321);
#5811=LINE('',#42024,#8322);
#5812=LINE('',#42025,#8323);
#5813=LINE('',#42105,#8324);
#5814=LINE('',#42110,#8325);
#5815=LINE('',#42112,#8326);
#5816=LINE('',#42117,#8327);
#5817=LINE('',#42282,#8328);
#5818=LINE('',#42526,#8329);
#5819=LINE('',#42839,#8330);
#5820=LINE('',#43222,#8331);
#5821=LINE('',#43578,#8332);
#5822=LINE('',#43954,#8333);
#5823=LINE('',#44326,#8334);
#5824=LINE('',#44574,#8335);
#5825=LINE('',#44903,#8336);
#5826=LINE('',#45264,#8337);
#5827=LINE('',#45507,#8338);
#5828=LINE('',#45577,#8339);
#5829=LINE('',#45925,#8340);
#5830=LINE('',#46111,#8341);
#5831=LINE('',#46459,#8342);
#5832=LINE('',#46807,#8343);
#5833=LINE('',#46993,#8344);
#5834=LINE('',#47179,#8345);
#5835=LINE('',#47527,#8346);
#5836=LINE('',#47713,#8347);
#5837=LINE('',#48061,#8348);
#5838=LINE('',#49710,#8349);
#5839=LINE('',#49720,#8350);
#5840=LINE('',#49722,#8351);
#5841=LINE('',#49723,#8352);
#5842=LINE('',#49727,#8353);
#5843=LINE('',#49733,#8354);
#5844=LINE('',#49739,#8355);
#5845=LINE('',#49746,#8356);
#5846=LINE('',#49750,#8357);
#5847=LINE('',#49754,#8358);
#5848=LINE('',#49758,#8359);
#5849=LINE('',#49762,#8360);
#5850=LINE('',#49766,#8361);
#5851=LINE('',#49770,#8362);
#5852=LINE('',#49774,#8363);
#5853=LINE('',#49778,#8364);
#5854=LINE('',#49782,#8365);
#5855=LINE('',#49786,#8366);
#5856=LINE('',#49790,#8367);
#5857=LINE('',#49794,#8368);
#5858=LINE('',#49798,#8369);
#5859=LINE('',#49802,#8370);
#5860=LINE('',#49806,#8371);
#5861=LINE('',#49810,#8372);
#5862=LINE('',#49814,#8373);
#5863=LINE('',#49818,#8374);
#5864=LINE('',#49822,#8375);
#5865=LINE('',#49826,#8376);
#5866=LINE('',#49830,#8377);
#5867=LINE('',#49834,#8378);
#5868=LINE('',#49838,#8379);
#5869=LINE('',#49842,#8380);
#5870=LINE('',#49846,#8381);
#5871=LINE('',#49850,#8382);
#5872=LINE('',#49854,#8383);
#5873=LINE('',#49858,#8384);
#5874=LINE('',#49862,#8385);
#5875=LINE('',#49866,#8386);
#5876=LINE('',#49870,#8387);
#5877=LINE('',#49874,#8388);
#5878=LINE('',#49879,#8389);
#5879=LINE('',#49883,#8390);
#5880=LINE('',#49887,#8391);
#5881=LINE('',#49891,#8392);
#5882=LINE('',#49895,#8393);
#5883=LINE('',#49899,#8394);
#5884=LINE('',#49903,#8395);
#5885=LINE('',#49907,#8396);
#5886=LINE('',#49911,#8397);
#5887=LINE('',#49915,#8398);
#5888=LINE('',#49919,#8399);
#5889=LINE('',#49923,#8400);
#5890=LINE('',#49927,#8401);
#5891=LINE('',#49931,#8402);
#5892=LINE('',#49935,#8403);
#5893=LINE('',#49939,#8404);
#5894=LINE('',#49943,#8405);
#5895=LINE('',#49947,#8406);
#5896=LINE('',#49951,#8407);
#5897=LINE('',#49955,#8408);
#5898=LINE('',#49959,#8409);
#5899=LINE('',#49963,#8410);
#5900=LINE('',#49967,#8411);
#5901=LINE('',#49971,#8412);
#5902=LINE('',#49975,#8413);
#5903=LINE('',#49979,#8414);
#5904=LINE('',#49983,#8415);
#5905=LINE('',#49987,#8416);
#5906=LINE('',#49991,#8417);
#5907=LINE('',#49995,#8418);
#5908=LINE('',#49999,#8419);
#5909=LINE('',#50003,#8420);
#5910=LINE('',#50007,#8421);
#5911=LINE('',#50011,#8422);
#5912=LINE('',#50015,#8423);
#5913=LINE('',#50019,#8424);
#5914=LINE('',#50022,#8425);
#5915=LINE('',#50029,#8426);
#5916=LINE('',#50030,#8427);
#5917=LINE('',#50032,#8428);
#5918=LINE('',#50043,#8429);
#5919=LINE('',#50044,#8430);
#5920=LINE('',#50046,#8431);
#5921=LINE('',#50057,#8432);
#5922=LINE('',#50058,#8433);
#5923=LINE('',#50060,#8434);
#5924=LINE('',#50071,#8435);
#5925=LINE('',#50072,#8436);
#5926=LINE('',#50074,#8437);
#5927=LINE('',#50085,#8438);
#5928=LINE('',#50086,#8439);
#5929=LINE('',#50088,#8440);
#5930=LINE('',#50099,#8441);
#5931=LINE('',#50100,#8442);
#5932=LINE('',#50102,#8443);
#5933=LINE('',#50113,#8444);
#5934=LINE('',#50114,#8445);
#5935=LINE('',#50116,#8446);
#5936=LINE('',#50127,#8447);
#5937=LINE('',#50128,#8448);
#5938=LINE('',#50130,#8449);
#5939=LINE('',#50141,#8450);
#5940=LINE('',#50142,#8451);
#5941=LINE('',#50144,#8452);
#5942=LINE('',#50155,#8453);
#5943=LINE('',#50156,#8454);
#5944=LINE('',#50158,#8455);
#5945=LINE('',#50169,#8456);
#5946=LINE('',#50170,#8457);
#5947=LINE('',#50172,#8458);
#5948=LINE('',#50183,#8459);
#5949=LINE('',#50184,#8460);
#5950=LINE('',#50186,#8461);
#5951=LINE('',#50197,#8462);
#5952=LINE('',#50198,#8463);
#5953=LINE('',#50200,#8464);
#5954=LINE('',#50211,#8465);
#5955=LINE('',#50212,#8466);
#5956=LINE('',#50214,#8467);
#5957=LINE('',#50225,#8468);
#5958=LINE('',#50226,#8469);
#5959=LINE('',#50228,#8470);
#5960=LINE('',#50239,#8471);
#5961=LINE('',#50240,#8472);
#5962=LINE('',#50242,#8473);
#5963=LINE('',#50253,#8474);
#5964=LINE('',#50254,#8475);
#5965=LINE('',#50256,#8476);
#5966=LINE('',#50267,#8477);
#5967=LINE('',#50268,#8478);
#5968=LINE('',#50270,#8479);
#5969=LINE('',#50281,#8480);
#5970=LINE('',#50282,#8481);
#5971=LINE('',#50284,#8482);
#5972=LINE('',#50295,#8483);
#5973=LINE('',#50296,#8484);
#5974=LINE('',#50298,#8485);
#5975=LINE('',#50309,#8486);
#5976=LINE('',#50310,#8487);
#5977=LINE('',#50312,#8488);
#5978=LINE('',#50323,#8489);
#5979=LINE('',#50324,#8490);
#5980=LINE('',#50326,#8491);
#5981=LINE('',#50337,#8492);
#5982=LINE('',#50338,#8493);
#5983=LINE('',#50340,#8494);
#5984=LINE('',#50351,#8495);
#5985=LINE('',#50352,#8496);
#5986=LINE('',#50354,#8497);
#5987=LINE('',#50365,#8498);
#5988=LINE('',#50366,#8499);
#5989=LINE('',#50368,#8500);
#5990=LINE('',#50379,#8501);
#5991=LINE('',#50380,#8502);
#5992=LINE('',#50382,#8503);
#5993=LINE('',#50393,#8504);
#5994=LINE('',#50394,#8505);
#5995=LINE('',#50396,#8506);
#5996=LINE('',#50407,#8507);
#5997=LINE('',#50408,#8508);
#5998=LINE('',#50410,#8509);
#5999=LINE('',#50421,#8510);
#6000=LINE('',#50422,#8511);
#6001=LINE('',#50424,#8512);
#6002=LINE('',#50435,#8513);
#6003=LINE('',#50436,#8514);
#6004=LINE('',#50438,#8515);
#6005=LINE('',#50449,#8516);
#6006=LINE('',#50450,#8517);
#6007=LINE('',#50452,#8518);
#6008=LINE('',#50463,#8519);
#6009=LINE('',#50464,#8520);
#6010=LINE('',#50466,#8521);
#6011=LINE('',#50477,#8522);
#6012=LINE('',#50478,#8523);
#6013=LINE('',#50480,#8524);
#6014=LINE('',#50491,#8525);
#6015=LINE('',#50492,#8526);
#6016=LINE('',#50494,#8527);
#6017=LINE('',#50505,#8528);
#6018=LINE('',#50506,#8529);
#6019=LINE('',#50508,#8530);
#6020=LINE('',#50517,#8531);
#6021=LINE('',#50583,#8532);
#6022=LINE('',#50586,#8533);
#6023=LINE('',#50588,#8534);
#6024=LINE('',#50592,#8535);
#6025=LINE('',#50594,#8536);
#6026=LINE('',#50598,#8537);
#6027=LINE('',#50601,#8538);
#6028=LINE('',#50604,#8539);
#6029=LINE('',#50606,#8540);
#6030=LINE('',#50610,#8541);
#6031=LINE('',#50613,#8542);
#6032=LINE('',#50616,#8543);
#6033=LINE('',#50619,#8544);
#6034=LINE('',#50621,#8545);
#6035=LINE('',#50623,#8546);
#6036=LINE('',#50625,#8547);
#6037=LINE('',#50626,#8548);
#6038=LINE('',#50628,#8549);
#6039=LINE('',#50630,#8550);
#6040=LINE('',#50631,#8551);
#6041=LINE('',#50633,#8552);
#6042=LINE('',#50635,#8553);
#6043=LINE('',#50636,#8554);
#6044=LINE('',#50640,#8555);
#6045=LINE('',#50643,#8556);
#6046=LINE('',#50645,#8557);
#6047=LINE('',#50648,#8558);
#6048=LINE('',#50658,#8559);
#6049=LINE('',#50661,#8560);
#6050=LINE('',#50665,#8561);
#6051=LINE('',#50667,#8562);
#6052=LINE('',#50669,#8563);
#6053=LINE('',#50676,#8564);
#6054=LINE('',#50681,#8565);
#6055=LINE('',#50685,#8566);
#6056=LINE('',#50729,#8567);
#6057=LINE('',#50734,#8568);
#6058=LINE('',#50737,#8569);
#6059=LINE('',#50742,#8570);
#6060=LINE('',#50745,#8571);
#6061=LINE('',#50750,#8572);
#6062=LINE('',#50753,#8573);
#6063=LINE('',#50758,#8574);
#6064=LINE('',#50761,#8575);
#6065=LINE('',#50766,#8576);
#6066=LINE('',#50769,#8577);
#6067=LINE('',#50774,#8578);
#6068=LINE('',#50777,#8579);
#6069=LINE('',#50782,#8580);
#6070=LINE('',#50785,#8581);
#6071=LINE('',#50790,#8582);
#6072=LINE('',#50793,#8583);
#6073=LINE('',#50798,#8584);
#6074=LINE('',#50801,#8585);
#6075=LINE('',#50806,#8586);
#6076=LINE('',#50809,#8587);
#6077=LINE('',#50814,#8588);
#6078=LINE('',#50817,#8589);
#6079=LINE('',#50822,#8590);
#6080=LINE('',#50825,#8591);
#6081=LINE('',#50830,#8592);
#6082=LINE('',#50833,#8593);
#6083=LINE('',#50838,#8594);
#6084=LINE('',#50841,#8595);
#6085=LINE('',#50846,#8596);
#6086=LINE('',#50849,#8597);
#6087=LINE('',#50854,#8598);
#6088=LINE('',#50857,#8599);
#6089=LINE('',#50862,#8600);
#6090=LINE('',#50865,#8601);
#6091=LINE('',#50870,#8602);
#6092=LINE('',#50873,#8603);
#6093=LINE('',#50878,#8604);
#6094=LINE('',#50881,#8605);
#6095=LINE('',#50886,#8606);
#6096=LINE('',#50889,#8607);
#6097=LINE('',#50893,#8608);
#6098=LINE('',#50895,#8609);
#6099=LINE('',#50896,#8610);
#6100=LINE('',#50899,#8611);
#6101=LINE('',#50903,#8612);
#6102=LINE('',#50904,#8613);
#6103=LINE('',#50909,#8614);
#6104=LINE('',#50912,#8615);
#6105=LINE('',#50915,#8616);
#6106=LINE('',#50916,#8617);
#6107=LINE('',#50919,#8618);
#6108=LINE('',#50921,#8619);
#6109=LINE('',#50922,#8620);
#6110=LINE('',#50927,#8621);
#6111=LINE('',#50931,#8622);
#6112=LINE('',#50932,#8623);
#6113=LINE('',#50933,#8624);
#6114=LINE('',#50937,#8625);
#6115=LINE('',#50944,#8626);
#6116=LINE('',#50946,#8627);
#6117=LINE('',#50948,#8628);
#6118=LINE('',#50949,#8629);
#6119=LINE('',#50953,#8630);
#6120=LINE('',#50959,#8631);
#6121=LINE('',#50960,#8632);
#6122=LINE('',#50961,#8633);
#6123=LINE('',#50965,#8634);
#6124=LINE('',#50971,#8635);
#6125=LINE('',#50972,#8636);
#6126=LINE('',#50973,#8637);
#6127=LINE('',#50976,#8638);
#6128=LINE('',#50978,#8639);
#6129=LINE('',#50979,#8640);
#6130=LINE('',#50982,#8641);
#6131=LINE('',#50986,#8642);
#6132=LINE('',#50987,#8643);
#6133=LINE('',#50990,#8644);
#6134=LINE('',#50994,#8645);
#6135=LINE('',#50995,#8646);
#6136=LINE('',#50998,#8647);
#6137=LINE('',#51000,#8648);
#6138=LINE('',#51001,#8649);
#6139=LINE('',#51004,#8650);
#6140=LINE('',#51008,#8651);
#6141=LINE('',#51009,#8652);
#6142=LINE('',#51012,#8653);
#6143=LINE('',#51016,#8654);
#6144=LINE('',#51017,#8655);
#6145=LINE('',#51022,#8656);
#6146=LINE('',#51028,#8657);
#6147=LINE('',#51034,#8658);
#6148=LINE('',#51040,#8659);
#6149=LINE('',#51046,#8660);
#6150=LINE('',#51052,#8661);
#6151=LINE('',#51058,#8662);
#6152=LINE('',#51064,#8663);
#6153=LINE('',#51070,#8664);
#6154=LINE('',#51076,#8665);
#6155=LINE('',#51080,#8666);
#6156=LINE('',#51082,#8667);
#6157=LINE('',#51083,#8668);
#6158=LINE('',#51086,#8669);
#6159=LINE('',#51088,#8670);
#6160=LINE('',#51089,#8671);
#6161=LINE('',#51092,#8672);
#6162=LINE('',#51094,#8673);
#6163=LINE('',#51095,#8674);
#6164=LINE('',#51098,#8675);
#6165=LINE('',#51100,#8676);
#6166=LINE('',#51101,#8677);
#6167=LINE('',#51104,#8678);
#6168=LINE('',#51106,#8679);
#6169=LINE('',#51107,#8680);
#6170=LINE('',#51110,#8681);
#6171=LINE('',#51112,#8682);
#6172=LINE('',#51113,#8683);
#6173=LINE('',#51116,#8684);
#6174=LINE('',#51118,#8685);
#6175=LINE('',#51119,#8686);
#6176=LINE('',#51122,#8687);
#6177=LINE('',#51124,#8688);
#6178=LINE('',#51125,#8689);
#6179=LINE('',#51128,#8690);
#6180=LINE('',#51130,#8691);
#6181=LINE('',#51131,#8692);
#6182=LINE('',#51134,#8693);
#6183=LINE('',#51136,#8694);
#6184=LINE('',#51137,#8695);
#6185=LINE('',#51140,#8696);
#6186=LINE('',#51142,#8697);
#6187=LINE('',#51143,#8698);
#6188=LINE('',#51146,#8699);
#6189=LINE('',#51148,#8700);
#6190=LINE('',#51149,#8701);
#6191=LINE('',#51152,#8702);
#6192=LINE('',#51154,#8703);
#6193=LINE('',#51155,#8704);
#6194=LINE('',#51158,#8705);
#6195=LINE('',#51160,#8706);
#6196=LINE('',#51161,#8707);
#6197=LINE('',#51164,#8708);
#6198=LINE('',#51166,#8709);
#6199=LINE('',#51167,#8710);
#6200=LINE('',#51170,#8711);
#6201=LINE('',#51172,#8712);
#6202=LINE('',#51173,#8713);
#6203=LINE('',#51176,#8714);
#6204=LINE('',#51178,#8715);
#6205=LINE('',#51179,#8716);
#6206=LINE('',#51182,#8717);
#6207=LINE('',#51184,#8718);
#6208=LINE('',#51185,#8719);
#6209=LINE('',#51188,#8720);
#6210=LINE('',#51190,#8721);
#6211=LINE('',#51191,#8722);
#6212=LINE('',#51194,#8723);
#6213=LINE('',#51196,#8724);
#6214=LINE('',#51197,#8725);
#6215=LINE('',#51200,#8726);
#6216=LINE('',#51202,#8727);
#6217=LINE('',#51203,#8728);
#6218=LINE('',#51206,#8729);
#6219=LINE('',#51208,#8730);
#6220=LINE('',#51209,#8731);
#6221=LINE('',#51212,#8732);
#6222=LINE('',#51214,#8733);
#6223=LINE('',#51215,#8734);
#6224=LINE('',#51218,#8735);
#6225=LINE('',#51220,#8736);
#6226=LINE('',#51221,#8737);
#6227=LINE('',#51224,#8738);
#6228=LINE('',#51226,#8739);
#6229=LINE('',#51227,#8740);
#6230=LINE('',#51230,#8741);
#6231=LINE('',#51232,#8742);
#6232=LINE('',#51233,#8743);
#6233=LINE('',#51236,#8744);
#6234=LINE('',#51238,#8745);
#6235=LINE('',#51239,#8746);
#6236=LINE('',#51242,#8747);
#6237=LINE('',#51244,#8748);
#6238=LINE('',#51245,#8749);
#6239=LINE('',#51248,#8750);
#6240=LINE('',#51250,#8751);
#6241=LINE('',#51251,#8752);
#6242=LINE('',#51254,#8753);
#6243=LINE('',#51256,#8754);
#6244=LINE('',#51257,#8755);
#6245=LINE('',#51260,#8756);
#6246=LINE('',#51262,#8757);
#6247=LINE('',#51263,#8758);
#6248=LINE('',#51266,#8759);
#6249=LINE('',#51268,#8760);
#6250=LINE('',#51269,#8761);
#6251=LINE('',#51272,#8762);
#6252=LINE('',#51274,#8763);
#6253=LINE('',#51275,#8764);
#6254=LINE('',#51278,#8765);
#6255=LINE('',#51280,#8766);
#6256=LINE('',#51281,#8767);
#6257=LINE('',#51284,#8768);
#6258=LINE('',#51286,#8769);
#6259=LINE('',#51287,#8770);
#6260=LINE('',#51290,#8771);
#6261=LINE('',#51292,#8772);
#6262=LINE('',#51293,#8773);
#6263=LINE('',#51296,#8774);
#6264=LINE('',#51298,#8775);
#6265=LINE('',#51299,#8776);
#6266=LINE('',#51302,#8777);
#6267=LINE('',#51304,#8778);
#6268=LINE('',#51305,#8779);
#6269=LINE('',#51308,#8780);
#6270=LINE('',#51310,#8781);
#6271=LINE('',#51311,#8782);
#6272=LINE('',#51314,#8783);
#6273=LINE('',#51316,#8784);
#6274=LINE('',#51317,#8785);
#6275=LINE('',#51320,#8786);
#6276=LINE('',#51322,#8787);
#6277=LINE('',#51323,#8788);
#6278=LINE('',#51326,#8789);
#6279=LINE('',#51328,#8790);
#6280=LINE('',#51329,#8791);
#6281=LINE('',#51332,#8792);
#6282=LINE('',#51334,#8793);
#6283=LINE('',#51335,#8794);
#6284=LINE('',#51338,#8795);
#6285=LINE('',#51340,#8796);
#6286=LINE('',#51341,#8797);
#6287=LINE('',#51344,#8798);
#6288=LINE('',#51346,#8799);
#6289=LINE('',#51347,#8800);
#6290=LINE('',#51350,#8801);
#6291=LINE('',#51352,#8802);
#6292=LINE('',#51353,#8803);
#6293=LINE('',#51356,#8804);
#6294=LINE('',#51358,#8805);
#6295=LINE('',#51359,#8806);
#6296=LINE('',#51362,#8807);
#6297=LINE('',#51364,#8808);
#6298=LINE('',#51365,#8809);
#6299=LINE('',#51368,#8810);
#6300=LINE('',#51370,#8811);
#6301=LINE('',#51371,#8812);
#6302=LINE('',#51374,#8813);
#6303=LINE('',#51376,#8814);
#6304=LINE('',#51377,#8815);
#6305=LINE('',#51380,#8816);
#6306=LINE('',#51382,#8817);
#6307=LINE('',#51383,#8818);
#6308=LINE('',#51386,#8819);
#6309=LINE('',#51388,#8820);
#6310=LINE('',#51389,#8821);
#6311=LINE('',#51392,#8822);
#6312=LINE('',#51394,#8823);
#6313=LINE('',#51395,#8824);
#6314=LINE('',#51398,#8825);
#6315=LINE('',#51400,#8826);
#6316=LINE('',#51401,#8827);
#6317=LINE('',#51404,#8828);
#6318=LINE('',#51406,#8829);
#6319=LINE('',#51407,#8830);
#6320=LINE('',#51410,#8831);
#6321=LINE('',#51412,#8832);
#6322=LINE('',#51413,#8833);
#6323=LINE('',#51416,#8834);
#6324=LINE('',#51418,#8835);
#6325=LINE('',#51419,#8836);
#6326=LINE('',#51422,#8837);
#6327=LINE('',#51424,#8838);
#6328=LINE('',#51425,#8839);
#6329=LINE('',#51428,#8840);
#6330=LINE('',#51430,#8841);
#6331=LINE('',#51431,#8842);
#6332=LINE('',#51434,#8843);
#6333=LINE('',#51436,#8844);
#6334=LINE('',#51437,#8845);
#6335=LINE('',#51440,#8846);
#6336=LINE('',#51442,#8847);
#6337=LINE('',#51443,#8848);
#6338=LINE('',#51446,#8849);
#6339=LINE('',#51448,#8850);
#6340=LINE('',#51449,#8851);
#6341=LINE('',#51452,#8852);
#6342=LINE('',#51454,#8853);
#6343=LINE('',#51455,#8854);
#6344=LINE('',#51458,#8855);
#6345=LINE('',#51460,#8856);
#6346=LINE('',#51461,#8857);
#6347=LINE('',#51464,#8858);
#6348=LINE('',#51466,#8859);
#6349=LINE('',#51467,#8860);
#6350=LINE('',#51470,#8861);
#6351=LINE('',#51472,#8862);
#6352=LINE('',#51473,#8863);
#6353=LINE('',#51476,#8864);
#6354=LINE('',#51478,#8865);
#6355=LINE('',#51479,#8866);
#6356=LINE('',#51482,#8867);
#6357=LINE('',#51484,#8868);
#6358=LINE('',#51485,#8869);
#6359=LINE('',#51488,#8870);
#6360=LINE('',#51490,#8871);
#6361=LINE('',#51491,#8872);
#6362=LINE('',#51494,#8873);
#6363=LINE('',#51496,#8874);
#6364=LINE('',#51497,#8875);
#6365=LINE('',#51500,#8876);
#6366=LINE('',#51502,#8877);
#6367=LINE('',#51503,#8878);
#6368=LINE('',#51506,#8879);
#6369=LINE('',#51508,#8880);
#6370=LINE('',#51509,#8881);
#6371=LINE('',#51512,#8882);
#6372=LINE('',#51514,#8883);
#6373=LINE('',#51515,#8884);
#6374=LINE('',#51518,#8885);
#6375=LINE('',#51520,#8886);
#6376=LINE('',#51521,#8887);
#6377=LINE('',#51524,#8888);
#6378=LINE('',#51526,#8889);
#6379=LINE('',#51527,#8890);
#6380=LINE('',#51530,#8891);
#6381=LINE('',#51532,#8892);
#6382=LINE('',#51533,#8893);
#6383=LINE('',#51536,#8894);
#6384=LINE('',#51538,#8895);
#6385=LINE('',#51539,#8896);
#6386=LINE('',#51542,#8897);
#6387=LINE('',#51544,#8898);
#6388=LINE('',#51545,#8899);
#6389=LINE('',#51548,#8900);
#6390=LINE('',#51550,#8901);
#6391=LINE('',#51551,#8902);
#6392=LINE('',#51554,#8903);
#6393=LINE('',#51556,#8904);
#6394=LINE('',#51557,#8905);
#6395=LINE('',#51560,#8906);
#6396=LINE('',#51562,#8907);
#6397=LINE('',#51563,#8908);
#6398=LINE('',#51566,#8909);
#6399=LINE('',#51568,#8910);
#6400=LINE('',#51569,#8911);
#6401=LINE('',#51572,#8912);
#6402=LINE('',#51574,#8913);
#6403=LINE('',#51575,#8914);
#6404=LINE('',#51578,#8915);
#6405=LINE('',#51580,#8916);
#6406=LINE('',#51581,#8917);
#6407=LINE('',#51584,#8918);
#6408=LINE('',#51586,#8919);
#6409=LINE('',#51587,#8920);
#6410=LINE('',#51590,#8921);
#6411=LINE('',#51592,#8922);
#6412=LINE('',#51593,#8923);
#6413=LINE('',#51596,#8924);
#6414=LINE('',#51598,#8925);
#6415=LINE('',#51599,#8926);
#6416=LINE('',#51602,#8927);
#6417=LINE('',#51604,#8928);
#6418=LINE('',#51605,#8929);
#6419=LINE('',#51608,#8930);
#6420=LINE('',#51610,#8931);
#6421=LINE('',#51611,#8932);
#6422=LINE('',#51614,#8933);
#6423=LINE('',#51616,#8934);
#6424=LINE('',#51617,#8935);
#6425=LINE('',#51620,#8936);
#6426=LINE('',#51622,#8937);
#6427=LINE('',#51623,#8938);
#6428=LINE('',#51626,#8939);
#6429=LINE('',#51628,#8940);
#6430=LINE('',#51629,#8941);
#6431=LINE('',#51632,#8942);
#6432=LINE('',#51634,#8943);
#6433=LINE('',#51635,#8944);
#6434=LINE('',#51638,#8945);
#6435=LINE('',#51640,#8946);
#6436=LINE('',#51641,#8947);
#6437=LINE('',#51644,#8948);
#6438=LINE('',#51646,#8949);
#6439=LINE('',#51647,#8950);
#6440=LINE('',#51650,#8951);
#6441=LINE('',#51652,#8952);
#6442=LINE('',#51653,#8953);
#6443=LINE('',#51656,#8954);
#6444=LINE('',#51658,#8955);
#6445=LINE('',#51659,#8956);
#6446=LINE('',#51662,#8957);
#6447=LINE('',#51664,#8958);
#6448=LINE('',#51665,#8959);
#6449=LINE('',#51668,#8960);
#6450=LINE('',#51670,#8961);
#6451=LINE('',#51671,#8962);
#6452=LINE('',#51674,#8963);
#6453=LINE('',#51676,#8964);
#6454=LINE('',#51677,#8965);
#6455=LINE('',#51680,#8966);
#6456=LINE('',#51682,#8967);
#6457=LINE('',#51683,#8968);
#6458=LINE('',#51686,#8969);
#6459=LINE('',#51688,#8970);
#6460=LINE('',#51689,#8971);
#6461=LINE('',#51692,#8972);
#6462=LINE('',#51694,#8973);
#6463=LINE('',#51695,#8974);
#6464=LINE('',#51698,#8975);
#6465=LINE('',#51700,#8976);
#6466=LINE('',#51701,#8977);
#6467=LINE('',#51704,#8978);
#6468=LINE('',#51706,#8979);
#6469=LINE('',#51707,#8980);
#6470=LINE('',#51710,#8981);
#6471=LINE('',#51712,#8982);
#6472=LINE('',#51713,#8983);
#6473=LINE('',#51716,#8984);
#6474=LINE('',#51718,#8985);
#6475=LINE('',#51719,#8986);
#6476=LINE('',#51722,#8987);
#6477=LINE('',#51724,#8988);
#6478=LINE('',#51725,#8989);
#6479=LINE('',#51728,#8990);
#6480=LINE('',#51730,#8991);
#6481=LINE('',#51731,#8992);
#6482=LINE('',#51734,#8993);
#6483=LINE('',#51736,#8994);
#6484=LINE('',#51737,#8995);
#6485=LINE('',#51740,#8996);
#6486=LINE('',#51742,#8997);
#6487=LINE('',#51743,#8998);
#6488=LINE('',#51746,#8999);
#6489=LINE('',#51748,#9000);
#6490=LINE('',#51749,#9001);
#6491=LINE('',#51752,#9002);
#6492=LINE('',#51754,#9003);
#6493=LINE('',#51755,#9004);
#6494=LINE('',#51758,#9005);
#6495=LINE('',#51760,#9006);
#6496=LINE('',#51761,#9007);
#6497=LINE('',#51764,#9008);
#6498=LINE('',#51766,#9009);
#6499=LINE('',#51767,#9010);
#6500=LINE('',#51770,#9011);
#6501=LINE('',#51772,#9012);
#6502=LINE('',#51773,#9013);
#6503=LINE('',#51776,#9014);
#6504=LINE('',#51778,#9015);
#6505=LINE('',#51779,#9016);
#6506=LINE('',#51782,#9017);
#6507=LINE('',#51784,#9018);
#6508=LINE('',#51785,#9019);
#6509=LINE('',#51788,#9020);
#6510=LINE('',#51790,#9021);
#6511=LINE('',#51791,#9022);
#6512=LINE('',#51794,#9023);
#6513=LINE('',#51796,#9024);
#6514=LINE('',#51797,#9025);
#6515=LINE('',#51800,#9026);
#6516=LINE('',#51802,#9027);
#6517=LINE('',#51803,#9028);
#6518=LINE('',#51806,#9029);
#6519=LINE('',#51808,#9030);
#6520=LINE('',#51809,#9031);
#6521=LINE('',#51812,#9032);
#6522=LINE('',#51814,#9033);
#6523=LINE('',#51815,#9034);
#6524=LINE('',#51818,#9035);
#6525=LINE('',#51820,#9036);
#6526=LINE('',#51821,#9037);
#6527=LINE('',#51824,#9038);
#6528=LINE('',#51826,#9039);
#6529=LINE('',#51827,#9040);
#6530=LINE('',#51830,#9041);
#6531=LINE('',#51832,#9042);
#6532=LINE('',#51833,#9043);
#6533=LINE('',#51836,#9044);
#6534=LINE('',#51838,#9045);
#6535=LINE('',#51839,#9046);
#6536=LINE('',#51842,#9047);
#6537=LINE('',#51844,#9048);
#6538=LINE('',#51845,#9049);
#6539=LINE('',#51848,#9050);
#6540=LINE('',#51850,#9051);
#6541=LINE('',#51851,#9052);
#6542=LINE('',#51854,#9053);
#6543=LINE('',#51856,#9054);
#6544=LINE('',#51857,#9055);
#6545=LINE('',#51860,#9056);
#6546=LINE('',#51862,#9057);
#6547=LINE('',#51863,#9058);
#6548=LINE('',#51866,#9059);
#6549=LINE('',#51868,#9060);
#6550=LINE('',#51869,#9061);
#6551=LINE('',#51872,#9062);
#6552=LINE('',#51874,#9063);
#6553=LINE('',#51875,#9064);
#6554=LINE('',#51878,#9065);
#6555=LINE('',#51880,#9066);
#6556=LINE('',#51881,#9067);
#6557=LINE('',#51884,#9068);
#6558=LINE('',#51886,#9069);
#6559=LINE('',#51887,#9070);
#6560=LINE('',#51890,#9071);
#6561=LINE('',#51892,#9072);
#6562=LINE('',#51893,#9073);
#6563=LINE('',#51896,#9074);
#6564=LINE('',#51898,#9075);
#6565=LINE('',#51899,#9076);
#6566=LINE('',#51902,#9077);
#6567=LINE('',#51904,#9078);
#6568=LINE('',#51905,#9079);
#6569=LINE('',#51908,#9080);
#6570=LINE('',#51910,#9081);
#6571=LINE('',#51911,#9082);
#6572=LINE('',#51914,#9083);
#6573=LINE('',#51916,#9084);
#6574=LINE('',#51917,#9085);
#6575=LINE('',#51920,#9086);
#6576=LINE('',#51922,#9087);
#6577=LINE('',#51923,#9088);
#6578=LINE('',#51926,#9089);
#6579=LINE('',#51928,#9090);
#6580=LINE('',#51929,#9091);
#6581=LINE('',#51932,#9092);
#6582=LINE('',#51934,#9093);
#6583=LINE('',#51935,#9094);
#6584=LINE('',#51938,#9095);
#6585=LINE('',#51940,#9096);
#6586=LINE('',#51941,#9097);
#6587=LINE('',#51944,#9098);
#6588=LINE('',#51946,#9099);
#6589=LINE('',#51947,#9100);
#6590=LINE('',#51950,#9101);
#6591=LINE('',#51952,#9102);
#6592=LINE('',#51953,#9103);
#6593=LINE('',#51956,#9104);
#6594=LINE('',#51958,#9105);
#6595=LINE('',#51959,#9106);
#6596=LINE('',#51962,#9107);
#6597=LINE('',#51964,#9108);
#6598=LINE('',#51965,#9109);
#6599=LINE('',#51968,#9110);
#6600=LINE('',#51970,#9111);
#6601=LINE('',#51971,#9112);
#6602=LINE('',#51974,#9113);
#6603=LINE('',#51976,#9114);
#6604=LINE('',#51977,#9115);
#6605=LINE('',#51980,#9116);
#6606=LINE('',#51982,#9117);
#6607=LINE('',#51983,#9118);
#6608=LINE('',#51986,#9119);
#6609=LINE('',#51988,#9120);
#6610=LINE('',#51989,#9121);
#6611=LINE('',#51992,#9122);
#6612=LINE('',#51994,#9123);
#6613=LINE('',#51995,#9124);
#6614=LINE('',#51998,#9125);
#6615=LINE('',#52000,#9126);
#6616=LINE('',#52001,#9127);
#6617=LINE('',#52004,#9128);
#6618=LINE('',#52006,#9129);
#6619=LINE('',#52007,#9130);
#6620=LINE('',#52010,#9131);
#6621=LINE('',#52012,#9132);
#6622=LINE('',#52013,#9133);
#6623=LINE('',#52016,#9134);
#6624=LINE('',#52018,#9135);
#6625=LINE('',#52019,#9136);
#6626=LINE('',#52022,#9137);
#6627=LINE('',#52024,#9138);
#6628=LINE('',#52025,#9139);
#6629=LINE('',#52028,#9140);
#6630=LINE('',#52030,#9141);
#6631=LINE('',#52031,#9142);
#6632=LINE('',#52034,#9143);
#6633=LINE('',#52036,#9144);
#6634=LINE('',#52037,#9145);
#6635=LINE('',#52040,#9146);
#6636=LINE('',#52042,#9147);
#6637=LINE('',#52043,#9148);
#6638=LINE('',#52046,#9149);
#6639=LINE('',#52048,#9150);
#6640=LINE('',#52049,#9151);
#6641=LINE('',#52052,#9152);
#6642=LINE('',#52054,#9153);
#6643=LINE('',#52055,#9154);
#6644=LINE('',#52058,#9155);
#6645=LINE('',#52060,#9156);
#6646=LINE('',#52061,#9157);
#6647=LINE('',#52064,#9158);
#6648=LINE('',#52066,#9159);
#6649=LINE('',#52067,#9160);
#6650=LINE('',#52070,#9161);
#6651=LINE('',#52072,#9162);
#6652=LINE('',#52073,#9163);
#6653=LINE('',#52076,#9164);
#6654=LINE('',#52078,#9165);
#6655=LINE('',#52079,#9166);
#6656=LINE('',#52082,#9167);
#6657=LINE('',#52084,#9168);
#6658=LINE('',#52085,#9169);
#6659=LINE('',#52088,#9170);
#6660=LINE('',#52090,#9171);
#6661=LINE('',#52091,#9172);
#6662=LINE('',#52094,#9173);
#6663=LINE('',#52096,#9174);
#6664=LINE('',#52097,#9175);
#6665=LINE('',#52100,#9176);
#6666=LINE('',#52102,#9177);
#6667=LINE('',#52103,#9178);
#6668=LINE('',#52106,#9179);
#6669=LINE('',#52108,#9180);
#6670=LINE('',#52109,#9181);
#6671=LINE('',#52112,#9182);
#6672=LINE('',#52114,#9183);
#6673=LINE('',#52115,#9184);
#6674=LINE('',#52118,#9185);
#6675=LINE('',#52120,#9186);
#6676=LINE('',#52121,#9187);
#6677=LINE('',#52124,#9188);
#6678=LINE('',#52126,#9189);
#6679=LINE('',#52127,#9190);
#6680=LINE('',#52130,#9191);
#6681=LINE('',#52132,#9192);
#6682=LINE('',#52133,#9193);
#6683=LINE('',#52136,#9194);
#6684=LINE('',#52138,#9195);
#6685=LINE('',#52139,#9196);
#6686=LINE('',#52142,#9197);
#6687=LINE('',#52144,#9198);
#6688=LINE('',#52145,#9199);
#6689=LINE('',#52148,#9200);
#6690=LINE('',#52150,#9201);
#6691=LINE('',#52151,#9202);
#6692=LINE('',#52154,#9203);
#6693=LINE('',#52156,#9204);
#6694=LINE('',#52157,#9205);
#6695=LINE('',#52160,#9206);
#6696=LINE('',#52162,#9207);
#6697=LINE('',#52163,#9208);
#6698=LINE('',#52166,#9209);
#6699=LINE('',#52168,#9210);
#6700=LINE('',#52169,#9211);
#6701=LINE('',#52172,#9212);
#6702=LINE('',#52174,#9213);
#6703=LINE('',#52175,#9214);
#6704=LINE('',#52178,#9215);
#6705=LINE('',#52180,#9216);
#6706=LINE('',#52181,#9217);
#6707=LINE('',#52184,#9218);
#6708=LINE('',#52186,#9219);
#6709=LINE('',#52187,#9220);
#6710=LINE('',#52190,#9221);
#6711=LINE('',#52192,#9222);
#6712=LINE('',#52193,#9223);
#6713=LINE('',#52196,#9224);
#6714=LINE('',#52198,#9225);
#6715=LINE('',#52199,#9226);
#6716=LINE('',#52202,#9227);
#6717=LINE('',#52204,#9228);
#6718=LINE('',#52205,#9229);
#6719=LINE('',#52208,#9230);
#6720=LINE('',#52210,#9231);
#6721=LINE('',#52211,#9232);
#6722=LINE('',#52214,#9233);
#6723=LINE('',#52216,#9234);
#6724=LINE('',#52217,#9235);
#6725=LINE('',#52220,#9236);
#6726=LINE('',#52222,#9237);
#6727=LINE('',#52223,#9238);
#6728=LINE('',#52226,#9239);
#6729=LINE('',#52228,#9240);
#6730=LINE('',#52229,#9241);
#6731=LINE('',#52232,#9242);
#6732=LINE('',#52234,#9243);
#6733=LINE('',#52235,#9244);
#6734=LINE('',#52238,#9245);
#6735=LINE('',#52240,#9246);
#6736=LINE('',#52241,#9247);
#6737=LINE('',#52244,#9248);
#6738=LINE('',#52246,#9249);
#6739=LINE('',#52247,#9250);
#6740=LINE('',#52250,#9251);
#6741=LINE('',#52252,#9252);
#6742=LINE('',#52253,#9253);
#6743=LINE('',#52256,#9254);
#6744=LINE('',#52258,#9255);
#6745=LINE('',#52259,#9256);
#6746=LINE('',#52262,#9257);
#6747=LINE('',#52264,#9258);
#6748=LINE('',#52265,#9259);
#6749=LINE('',#52268,#9260);
#6750=LINE('',#52270,#9261);
#6751=LINE('',#52271,#9262);
#6752=LINE('',#52274,#9263);
#6753=LINE('',#52276,#9264);
#6754=LINE('',#52277,#9265);
#6755=LINE('',#52280,#9266);
#6756=LINE('',#52282,#9267);
#6757=LINE('',#52283,#9268);
#6758=LINE('',#52286,#9269);
#6759=LINE('',#52288,#9270);
#6760=LINE('',#52289,#9271);
#6761=LINE('',#52292,#9272);
#6762=LINE('',#52294,#9273);
#6763=LINE('',#52295,#9274);
#6764=LINE('',#52298,#9275);
#6765=LINE('',#52300,#9276);
#6766=LINE('',#52301,#9277);
#6767=LINE('',#52304,#9278);
#6768=LINE('',#52306,#9279);
#6769=LINE('',#52307,#9280);
#6770=LINE('',#52310,#9281);
#6771=LINE('',#52312,#9282);
#6772=LINE('',#52313,#9283);
#6773=LINE('',#52316,#9284);
#6774=LINE('',#52318,#9285);
#6775=LINE('',#52319,#9286);
#6776=LINE('',#52322,#9287);
#6777=LINE('',#52324,#9288);
#6778=LINE('',#52325,#9289);
#6779=LINE('',#52328,#9290);
#6780=LINE('',#52330,#9291);
#6781=LINE('',#52331,#9292);
#6782=LINE('',#52334,#9293);
#6783=LINE('',#52336,#9294);
#6784=LINE('',#52337,#9295);
#6785=LINE('',#52340,#9296);
#6786=LINE('',#52342,#9297);
#6787=LINE('',#52343,#9298);
#6788=LINE('',#52346,#9299);
#6789=LINE('',#52348,#9300);
#6790=LINE('',#52349,#9301);
#6791=LINE('',#52352,#9302);
#6792=LINE('',#52354,#9303);
#6793=LINE('',#52355,#9304);
#6794=LINE('',#52358,#9305);
#6795=LINE('',#52360,#9306);
#6796=LINE('',#52361,#9307);
#6797=LINE('',#52364,#9308);
#6798=LINE('',#52366,#9309);
#6799=LINE('',#52367,#9310);
#6800=LINE('',#52370,#9311);
#6801=LINE('',#52372,#9312);
#6802=LINE('',#52373,#9313);
#6803=LINE('',#52376,#9314);
#6804=LINE('',#52378,#9315);
#6805=LINE('',#52379,#9316);
#6806=LINE('',#52382,#9317);
#6807=LINE('',#52384,#9318);
#6808=LINE('',#52385,#9319);
#6809=LINE('',#52388,#9320);
#6810=LINE('',#52390,#9321);
#6811=LINE('',#52391,#9322);
#6812=LINE('',#52394,#9323);
#6813=LINE('',#52396,#9324);
#6814=LINE('',#52397,#9325);
#6815=LINE('',#52400,#9326);
#6816=LINE('',#52402,#9327);
#6817=LINE('',#52403,#9328);
#6818=LINE('',#52406,#9329);
#6819=LINE('',#52408,#9330);
#6820=LINE('',#52409,#9331);
#6821=LINE('',#52412,#9332);
#6822=LINE('',#52414,#9333);
#6823=LINE('',#52415,#9334);
#6824=LINE('',#52418,#9335);
#6825=LINE('',#52420,#9336);
#6826=LINE('',#52421,#9337);
#6827=LINE('',#52424,#9338);
#6828=LINE('',#52426,#9339);
#6829=LINE('',#52427,#9340);
#6830=LINE('',#52430,#9341);
#6831=LINE('',#52432,#9342);
#6832=LINE('',#52433,#9343);
#6833=LINE('',#52436,#9344);
#6834=LINE('',#52438,#9345);
#6835=LINE('',#52439,#9346);
#6836=LINE('',#52442,#9347);
#6837=LINE('',#52444,#9348);
#6838=LINE('',#52445,#9349);
#6839=LINE('',#52448,#9350);
#6840=LINE('',#52450,#9351);
#6841=LINE('',#52451,#9352);
#6842=LINE('',#52454,#9353);
#6843=LINE('',#52456,#9354);
#6844=LINE('',#52457,#9355);
#6845=LINE('',#52460,#9356);
#6846=LINE('',#52462,#9357);
#6847=LINE('',#52463,#9358);
#6848=LINE('',#52466,#9359);
#6849=LINE('',#52468,#9360);
#6850=LINE('',#52469,#9361);
#6851=LINE('',#52472,#9362);
#6852=LINE('',#52474,#9363);
#6853=LINE('',#52475,#9364);
#6854=LINE('',#52478,#9365);
#6855=LINE('',#52480,#9366);
#6856=LINE('',#52481,#9367);
#6857=LINE('',#52484,#9368);
#6858=LINE('',#52486,#9369);
#6859=LINE('',#52487,#9370);
#6860=LINE('',#52490,#9371);
#6861=LINE('',#52492,#9372);
#6862=LINE('',#52493,#9373);
#6863=LINE('',#52496,#9374);
#6864=LINE('',#52498,#9375);
#6865=LINE('',#52499,#9376);
#6866=LINE('',#52502,#9377);
#6867=LINE('',#52504,#9378);
#6868=LINE('',#52505,#9379);
#6869=LINE('',#52508,#9380);
#6870=LINE('',#52510,#9381);
#6871=LINE('',#52511,#9382);
#6872=LINE('',#52514,#9383);
#6873=LINE('',#52516,#9384);
#6874=LINE('',#52517,#9385);
#6875=LINE('',#52520,#9386);
#6876=LINE('',#52522,#9387);
#6877=LINE('',#52523,#9388);
#6878=LINE('',#52526,#9389);
#6879=LINE('',#52528,#9390);
#6880=LINE('',#52529,#9391);
#6881=LINE('',#52532,#9392);
#6882=LINE('',#52534,#9393);
#6883=LINE('',#52535,#9394);
#6884=LINE('',#52538,#9395);
#6885=LINE('',#52540,#9396);
#6886=LINE('',#52541,#9397);
#6887=LINE('',#52544,#9398);
#6888=LINE('',#52546,#9399);
#6889=LINE('',#52547,#9400);
#6890=LINE('',#52550,#9401);
#6891=LINE('',#52552,#9402);
#6892=LINE('',#52553,#9403);
#6893=LINE('',#52556,#9404);
#6894=LINE('',#52558,#9405);
#6895=LINE('',#52559,#9406);
#6896=LINE('',#52562,#9407);
#6897=LINE('',#52564,#9408);
#6898=LINE('',#52565,#9409);
#6899=LINE('',#52568,#9410);
#6900=LINE('',#52570,#9411);
#6901=LINE('',#52571,#9412);
#6902=LINE('',#52574,#9413);
#6903=LINE('',#52576,#9414);
#6904=LINE('',#52577,#9415);
#6905=LINE('',#52580,#9416);
#6906=LINE('',#52582,#9417);
#6907=LINE('',#52583,#9418);
#6908=LINE('',#52586,#9419);
#6909=LINE('',#52588,#9420);
#6910=LINE('',#52589,#9421);
#6911=LINE('',#52592,#9422);
#6912=LINE('',#52594,#9423);
#6913=LINE('',#52595,#9424);
#6914=LINE('',#52598,#9425);
#6915=LINE('',#52600,#9426);
#6916=LINE('',#52601,#9427);
#6917=LINE('',#52604,#9428);
#6918=LINE('',#52606,#9429);
#6919=LINE('',#52607,#9430);
#6920=LINE('',#52610,#9431);
#6921=LINE('',#52612,#9432);
#6922=LINE('',#52613,#9433);
#6923=LINE('',#52616,#9434);
#6924=LINE('',#52618,#9435);
#6925=LINE('',#52619,#9436);
#6926=LINE('',#52622,#9437);
#6927=LINE('',#52624,#9438);
#6928=LINE('',#52625,#9439);
#6929=LINE('',#52628,#9440);
#6930=LINE('',#52630,#9441);
#6931=LINE('',#52631,#9442);
#6932=LINE('',#52634,#9443);
#6933=LINE('',#52636,#9444);
#6934=LINE('',#52637,#9445);
#6935=LINE('',#52640,#9446);
#6936=LINE('',#52642,#9447);
#6937=LINE('',#52643,#9448);
#6938=LINE('',#52646,#9449);
#6939=LINE('',#52648,#9450);
#6940=LINE('',#52649,#9451);
#6941=LINE('',#52652,#9452);
#6942=LINE('',#52654,#9453);
#6943=LINE('',#52655,#9454);
#6944=LINE('',#52658,#9455);
#6945=LINE('',#52660,#9456);
#6946=LINE('',#52661,#9457);
#6947=LINE('',#52664,#9458);
#6948=LINE('',#52666,#9459);
#6949=LINE('',#52667,#9460);
#6950=LINE('',#52670,#9461);
#6951=LINE('',#52672,#9462);
#6952=LINE('',#52673,#9463);
#6953=LINE('',#52676,#9464);
#6954=LINE('',#52678,#9465);
#6955=LINE('',#52679,#9466);
#6956=LINE('',#52682,#9467);
#6957=LINE('',#52684,#9468);
#6958=LINE('',#52685,#9469);
#6959=LINE('',#52688,#9470);
#6960=LINE('',#52690,#9471);
#6961=LINE('',#52691,#9472);
#6962=LINE('',#52694,#9473);
#6963=LINE('',#52696,#9474);
#6964=LINE('',#52697,#9475);
#6965=LINE('',#52700,#9476);
#6966=LINE('',#52702,#9477);
#6967=LINE('',#52703,#9478);
#6968=LINE('',#52706,#9479);
#6969=LINE('',#52708,#9480);
#6970=LINE('',#52709,#9481);
#6971=LINE('',#52712,#9482);
#6972=LINE('',#52714,#9483);
#6973=LINE('',#52715,#9484);
#6974=LINE('',#52718,#9485);
#6975=LINE('',#52720,#9486);
#6976=LINE('',#52721,#9487);
#6977=LINE('',#52724,#9488);
#6978=LINE('',#52726,#9489);
#6979=LINE('',#52727,#9490);
#6980=LINE('',#52730,#9491);
#6981=LINE('',#52732,#9492);
#6982=LINE('',#52733,#9493);
#6983=LINE('',#52736,#9494);
#6984=LINE('',#52738,#9495);
#6985=LINE('',#52739,#9496);
#6986=LINE('',#52742,#9497);
#6987=LINE('',#52744,#9498);
#6988=LINE('',#52745,#9499);
#6989=LINE('',#52747,#9500);
#6990=LINE('',#52748,#9501);
#6991=LINE('',#52756,#9502);
#6992=LINE('',#52761,#9503);
#6993=LINE('',#52763,#9504);
#6994=LINE('',#52765,#9505);
#6995=LINE('',#52767,#9506);
#6996=LINE('',#52769,#9507);
#6997=LINE('',#52771,#9508);
#6998=LINE('',#52773,#9509);
#6999=LINE('',#52774,#9510);
#7000=LINE('',#52785,#9511);
#7001=LINE('',#52787,#9512);
#7002=LINE('',#52789,#9513);
#7003=LINE('',#52791,#9514);
#7004=LINE('',#52793,#9515);
#7005=LINE('',#52794,#9516);
#7006=LINE('',#52797,#9517);
#7007=LINE('',#52799,#9518);
#7008=LINE('',#52801,#9519);
#7009=LINE('',#52803,#9520);
#7010=LINE('',#52805,#9521);
#7011=LINE('',#52806,#9522);
#7012=LINE('',#52815,#9523);
#7013=LINE('',#52820,#9524);
#7014=LINE('',#52823,#9525);
#7015=LINE('',#52828,#9526);
#7016=LINE('',#52831,#9527);
#7017=LINE('',#52836,#9528);
#7018=LINE('',#52839,#9529);
#7019=LINE('',#52844,#9530);
#7020=LINE('',#52847,#9531);
#7021=LINE('',#52852,#9532);
#7022=LINE('',#52855,#9533);
#7023=LINE('',#52860,#9534);
#7024=LINE('',#52863,#9535);
#7025=LINE('',#52868,#9536);
#7026=LINE('',#52871,#9537);
#7027=LINE('',#52876,#9538);
#7028=LINE('',#52877,#9539);
#7029=LINE('',#52878,#9540);
#7030=LINE('',#52881,#9541);
#7031=LINE('',#52882,#9542);
#7032=LINE('',#52885,#9543);
#7033=LINE('',#52886,#9544);
#7034=LINE('',#52889,#9545);
#7035=LINE('',#52890,#9546);
#7036=LINE('',#52893,#9547);
#7037=LINE('',#52894,#9548);
#7038=LINE('',#52896,#9549);
#7039=LINE('',#52900,#9550);
#7040=LINE('',#52901,#9551);
#7041=LINE('',#52902,#9552);
#7042=LINE('',#52905,#9553);
#7043=LINE('',#52906,#9554);
#7044=LINE('',#52909,#9555);
#7045=LINE('',#52910,#9556);
#7046=LINE('',#52913,#9557);
#7047=LINE('',#52914,#9558);
#7048=LINE('',#52917,#9559);
#7049=LINE('',#52918,#9560);
#7050=LINE('',#52920,#9561);
#7051=LINE('',#52923,#9562);
#7052=LINE('',#52925,#9563);
#7053=LINE('',#52926,#9564);
#7054=LINE('',#52929,#9565);
#7055=LINE('',#52930,#9566);
#7056=LINE('',#52933,#9567);
#7057=LINE('',#52934,#9568);
#7058=LINE('',#52937,#9569);
#7059=LINE('',#52938,#9570);
#7060=LINE('',#52941,#9571);
#7061=LINE('',#52942,#9572);
#7062=LINE('',#52945,#9573);
#7063=LINE('',#52946,#9574);
#7064=LINE('',#52949,#9575);
#7065=LINE('',#52950,#9576);
#7066=LINE('',#52952,#9577);
#7067=LINE('',#52955,#9578);
#7068=LINE('',#52957,#9579);
#7069=LINE('',#52958,#9580);
#7070=LINE('',#52961,#9581);
#7071=LINE('',#52962,#9582);
#7072=LINE('',#52965,#9583);
#7073=LINE('',#52966,#9584);
#7074=LINE('',#52969,#9585);
#7075=LINE('',#52970,#9586);
#7076=LINE('',#52973,#9587);
#7077=LINE('',#52974,#9588);
#7078=LINE('',#52977,#9589);
#7079=LINE('',#52978,#9590);
#7080=LINE('',#52981,#9591);
#7081=LINE('',#52982,#9592);
#7082=LINE('',#52984,#9593);
#7083=LINE('',#52991,#9594);
#7084=LINE('',#52997,#9595);
#7085=LINE('',#53003,#9596);
#7086=LINE('',#53007,#9597);
#7087=LINE('',#53020,#9598);
#7088=LINE('',#53022,#9599);
#7089=LINE('',#53024,#9600);
#7090=LINE('',#53025,#9601);
#7091=LINE('',#53030,#9602);
#7092=LINE('',#53034,#9603);
#7093=LINE('',#53047,#9604);
#7094=LINE('',#53049,#9605);
#7095=LINE('',#53051,#9606);
#7096=LINE('',#53052,#9607);
#7097=LINE('',#53072,#9608);
#7098=LINE('',#53095,#9609);
#7099=LINE('',#53101,#9610);
#7100=LINE('',#53106,#9611);
#7101=LINE('',#53108,#9612);
#7102=LINE('',#53110,#9613);
#7103=LINE('',#53111,#9614);
#7104=LINE('',#53112,#9615);
#7105=LINE('',#53115,#9616);
#7106=LINE('',#53118,#9617);
#7107=LINE('',#53123,#9618);
#7108=LINE('',#53124,#9619);
#7109=LINE('',#53126,#9620);
#7110=LINE('',#53128,#9621);
#7111=LINE('',#53129,#9622);
#7112=LINE('',#53132,#9623);
#7113=LINE('',#53134,#9624);
#7114=LINE('',#53135,#9625);
#7115=LINE('',#53137,#9626);
#7116=LINE('',#53139,#9627);
#7117=LINE('',#53142,#9628);
#7118=LINE('',#53144,#9629);
#7119=LINE('',#53145,#9630);
#7120=LINE('',#53148,#9631);
#7121=LINE('',#53150,#9632);
#7122=LINE('',#53151,#9633);
#7123=LINE('',#53153,#9634);
#7124=LINE('',#53154,#9635);
#7125=LINE('',#53161,#9636);
#7126=LINE('',#53348,#9637);
#7127=LINE('',#53646,#9638);
#7128=LINE('',#53946,#9639);
#7129=LINE('',#54236,#9640);
#7130=LINE('',#54534,#9641);
#7131=LINE('',#54826,#9642);
#7132=LINE('',#58528,#9643);
#7133=LINE('',#58534,#9644);
#7134=LINE('',#58536,#9645);
#7135=LINE('',#58538,#9646);
#7136=LINE('',#58545,#9647);
#7137=LINE('',#58549,#9648);
#7138=LINE('',#58905,#9649);
#7139=LINE('',#58909,#9650);
#7140=LINE('',#58911,#9651);
#7141=LINE('',#58912,#9652);
#7142=LINE('',#58915,#9653);
#7143=LINE('',#58916,#9654);
#7144=LINE('',#58921,#9655);
#7145=LINE('',#58923,#9656);
#7146=LINE('',#58924,#9657);
#7147=LINE('',#58927,#9658);
#7148=LINE('',#58928,#9659);
#7149=LINE('',#58933,#9660);
#7150=LINE('',#58935,#9661);
#7151=LINE('',#58936,#9662);
#7152=LINE('',#58939,#9663);
#7153=LINE('',#58940,#9664);
#7154=LINE('',#58945,#9665);
#7155=LINE('',#58947,#9666);
#7156=LINE('',#58948,#9667);
#7157=LINE('',#58951,#9668);
#7158=LINE('',#58952,#9669);
#7159=LINE('',#58957,#9670);
#7160=LINE('',#58959,#9671);
#7161=LINE('',#58960,#9672);
#7162=LINE('',#58963,#9673);
#7163=LINE('',#58964,#9674);
#7164=LINE('',#58969,#9675);
#7165=LINE('',#58971,#9676);
#7166=LINE('',#58972,#9677);
#7167=LINE('',#58975,#9678);
#7168=LINE('',#58976,#9679);
#7169=LINE('',#58981,#9680);
#7170=LINE('',#58983,#9681);
#7171=LINE('',#58984,#9682);
#7172=LINE('',#58987,#9683);
#7173=LINE('',#58988,#9684);
#7174=LINE('',#58993,#9685);
#7175=LINE('',#58995,#9686);
#7176=LINE('',#58996,#9687);
#7177=LINE('',#58999,#9688);
#7178=LINE('',#59000,#9689);
#7179=LINE('',#59007,#9690);
#7180=LINE('',#59009,#9691);
#7181=LINE('',#59010,#9692);
#7182=LINE('',#59013,#9693);
#7183=LINE('',#59014,#9694);
#7184=LINE('',#59019,#9695);
#7185=LINE('',#59021,#9696);
#7186=LINE('',#59022,#9697);
#7187=LINE('',#59025,#9698);
#7188=LINE('',#59026,#9699);
#7189=LINE('',#59031,#9700);
#7190=LINE('',#59033,#9701);
#7191=LINE('',#59034,#9702);
#7192=LINE('',#59037,#9703);
#7193=LINE('',#59038,#9704);
#7194=LINE('',#59043,#9705);
#7195=LINE('',#59045,#9706);
#7196=LINE('',#59046,#9707);
#7197=LINE('',#59049,#9708);
#7198=LINE('',#59050,#9709);
#7199=LINE('',#59055,#9710);
#7200=LINE('',#59057,#9711);
#7201=LINE('',#59058,#9712);
#7202=LINE('',#59061,#9713);
#7203=LINE('',#59062,#9714);
#7204=LINE('',#59067,#9715);
#7205=LINE('',#59069,#9716);
#7206=LINE('',#59070,#9717);
#7207=LINE('',#59073,#9718);
#7208=LINE('',#59074,#9719);
#7209=LINE('',#59079,#9720);
#7210=LINE('',#59081,#9721);
#7211=LINE('',#59082,#9722);
#7212=LINE('',#59085,#9723);
#7213=LINE('',#59086,#9724);
#7214=LINE('',#59091,#9725);
#7215=LINE('',#59093,#9726);
#7216=LINE('',#59094,#9727);
#7217=LINE('',#59097,#9728);
#7218=LINE('',#59098,#9729);
#7219=LINE('',#59103,#9730);
#7220=LINE('',#59105,#9731);
#7221=LINE('',#59106,#9732);
#7222=LINE('',#59109,#9733);
#7223=LINE('',#59110,#9734);
#7224=LINE('',#59115,#9735);
#7225=LINE('',#59117,#9736);
#7226=LINE('',#59118,#9737);
#7227=LINE('',#59121,#9738);
#7228=LINE('',#59122,#9739);
#7229=LINE('',#59127,#9740);
#7230=LINE('',#59129,#9741);
#7231=LINE('',#59130,#9742);
#7232=LINE('',#59133,#9743);
#7233=LINE('',#59134,#9744);
#7234=LINE('',#59139,#9745);
#7235=LINE('',#59141,#9746);
#7236=LINE('',#59142,#9747);
#7237=LINE('',#59145,#9748);
#7238=LINE('',#59146,#9749);
#7239=LINE('',#59151,#9750);
#7240=LINE('',#59153,#9751);
#7241=LINE('',#59154,#9752);
#7242=LINE('',#59157,#9753);
#7243=LINE('',#59158,#9754);
#7244=LINE('',#59163,#9755);
#7245=LINE('',#59165,#9756);
#7246=LINE('',#59166,#9757);
#7247=LINE('',#59169,#9758);
#7248=LINE('',#59170,#9759);
#7249=LINE('',#59175,#9760);
#7250=LINE('',#59177,#9761);
#7251=LINE('',#59178,#9762);
#7252=LINE('',#59181,#9763);
#7253=LINE('',#59182,#9764);
#7254=LINE('',#59187,#9765);
#7255=LINE('',#59189,#9766);
#7256=LINE('',#59190,#9767);
#7257=LINE('',#59193,#9768);
#7258=LINE('',#59194,#9769);
#7259=LINE('',#59199,#9770);
#7260=LINE('',#59201,#9771);
#7261=LINE('',#59202,#9772);
#7262=LINE('',#59205,#9773);
#7263=LINE('',#59206,#9774);
#7264=LINE('',#59211,#9775);
#7265=LINE('',#59213,#9776);
#7266=LINE('',#59214,#9777);
#7267=LINE('',#59217,#9778);
#7268=LINE('',#59218,#9779);
#7269=LINE('',#59223,#9780);
#7270=LINE('',#59225,#9781);
#7271=LINE('',#59226,#9782);
#7272=LINE('',#59229,#9783);
#7273=LINE('',#59230,#9784);
#7274=LINE('',#59235,#9785);
#7275=LINE('',#59237,#9786);
#7276=LINE('',#59238,#9787);
#7277=LINE('',#59241,#9788);
#7278=LINE('',#59242,#9789);
#7279=LINE('',#59247,#9790);
#7280=LINE('',#59249,#9791);
#7281=LINE('',#59250,#9792);
#7282=LINE('',#59253,#9793);
#7283=LINE('',#59254,#9794);
#7284=LINE('',#59259,#9795);
#7285=LINE('',#59261,#9796);
#7286=LINE('',#59262,#9797);
#7287=LINE('',#59265,#9798);
#7288=LINE('',#59266,#9799);
#7289=LINE('',#59271,#9800);
#7290=LINE('',#59273,#9801);
#7291=LINE('',#59274,#9802);
#7292=LINE('',#59277,#9803);
#7293=LINE('',#59278,#9804);
#7294=LINE('',#59283,#9805);
#7295=LINE('',#59285,#9806);
#7296=LINE('',#59286,#9807);
#7297=LINE('',#59289,#9808);
#7298=LINE('',#59290,#9809);
#7299=LINE('',#59295,#9810);
#7300=LINE('',#59297,#9811);
#7301=LINE('',#59298,#9812);
#7302=LINE('',#59301,#9813);
#7303=LINE('',#59302,#9814);
#7304=LINE('',#59307,#9815);
#7305=LINE('',#59309,#9816);
#7306=LINE('',#59310,#9817);
#7307=LINE('',#59313,#9818);
#7308=LINE('',#59314,#9819);
#7309=LINE('',#59319,#9820);
#7310=LINE('',#59321,#9821);
#7311=LINE('',#59322,#9822);
#7312=LINE('',#59325,#9823);
#7313=LINE('',#59326,#9824);
#7314=LINE('',#59330,#9825);
#7315=LINE('',#59334,#9826);
#7316=LINE('',#59336,#9827);
#7317=LINE('',#59338,#9828);
#7318=LINE('',#59340,#9829);
#7319=LINE('',#59342,#9830);
#7320=LINE('',#59343,#9831);
#7321=LINE('',#59347,#9832);
#7322=LINE('',#59351,#9833);
#7323=LINE('',#59355,#9834);
#7324=LINE('',#59359,#9835);
#7325=LINE('',#59363,#9836);
#7326=LINE('',#59366,#9837);
#7327=LINE('',#59370,#9838);
#7328=LINE('',#59372,#9839);
#7329=LINE('',#59373,#9840);
#7330=LINE('',#59375,#9841);
#7331=LINE('',#59377,#9842);
#7332=LINE('',#59379,#9843);
#7333=LINE('',#59381,#9844);
#7334=LINE('',#59387,#9845);
#7335=LINE('',#59609,#9846);
#7336=LINE('',#59942,#9847);
#7337=LINE('',#60138,#9848);
#7338=LINE('',#60335,#9849);
#7339=LINE('',#60514,#9850);
#7340=LINE('',#60814,#9851);
#7341=LINE('',#61133,#9852);
#7342=LINE('',#61454,#9853);
#7343=LINE('',#65981,#9854);
#7344=LINE('',#65987,#9855);
#7345=LINE('',#65989,#9856);
#7346=LINE('',#65991,#9857);
#7347=LINE('',#65998,#9858);
#7348=LINE('',#66002,#9859);
#7349=LINE('',#66358,#9860);
#7350=LINE('',#66362,#9861);
#7351=LINE('',#66364,#9862);
#7352=LINE('',#66365,#9863);
#7353=LINE('',#66368,#9864);
#7354=LINE('',#66369,#9865);
#7355=LINE('',#66374,#9866);
#7356=LINE('',#66376,#9867);
#7357=LINE('',#66377,#9868);
#7358=LINE('',#66380,#9869);
#7359=LINE('',#66381,#9870);
#7360=LINE('',#66386,#9871);
#7361=LINE('',#66388,#9872);
#7362=LINE('',#66389,#9873);
#7363=LINE('',#66392,#9874);
#7364=LINE('',#66393,#9875);
#7365=LINE('',#66398,#9876);
#7366=LINE('',#66400,#9877);
#7367=LINE('',#66401,#9878);
#7368=LINE('',#66404,#9879);
#7369=LINE('',#66405,#9880);
#7370=LINE('',#66410,#9881);
#7371=LINE('',#66412,#9882);
#7372=LINE('',#66413,#9883);
#7373=LINE('',#66416,#9884);
#7374=LINE('',#66417,#9885);
#7375=LINE('',#66422,#9886);
#7376=LINE('',#66424,#9887);
#7377=LINE('',#66425,#9888);
#7378=LINE('',#66428,#9889);
#7379=LINE('',#66429,#9890);
#7380=LINE('',#66434,#9891);
#7381=LINE('',#66436,#9892);
#7382=LINE('',#66437,#9893);
#7383=LINE('',#66440,#9894);
#7384=LINE('',#66441,#9895);
#7385=LINE('',#66446,#9896);
#7386=LINE('',#66448,#9897);
#7387=LINE('',#66449,#9898);
#7388=LINE('',#66452,#9899);
#7389=LINE('',#66453,#9900);
#7390=LINE('',#66458,#9901);
#7391=LINE('',#66460,#9902);
#7392=LINE('',#66461,#9903);
#7393=LINE('',#66464,#9904);
#7394=LINE('',#66465,#9905);
#7395=LINE('',#66470,#9906);
#7396=LINE('',#66472,#9907);
#7397=LINE('',#66473,#9908);
#7398=LINE('',#66476,#9909);
#7399=LINE('',#66477,#9910);
#7400=LINE('',#66482,#9911);
#7401=LINE('',#66484,#9912);
#7402=LINE('',#66485,#9913);
#7403=LINE('',#66488,#9914);
#7404=LINE('',#66489,#9915);
#7405=LINE('',#66494,#9916);
#7406=LINE('',#66496,#9917);
#7407=LINE('',#66497,#9918);
#7408=LINE('',#66500,#9919);
#7409=LINE('',#66501,#9920);
#7410=LINE('',#66506,#9921);
#7411=LINE('',#66508,#9922);
#7412=LINE('',#66509,#9923);
#7413=LINE('',#66512,#9924);
#7414=LINE('',#66513,#9925);
#7415=LINE('',#66518,#9926);
#7416=LINE('',#66520,#9927);
#7417=LINE('',#66521,#9928);
#7418=LINE('',#66524,#9929);
#7419=LINE('',#66525,#9930);
#7420=LINE('',#66530,#9931);
#7421=LINE('',#66532,#9932);
#7422=LINE('',#66533,#9933);
#7423=LINE('',#66536,#9934);
#7424=LINE('',#66537,#9935);
#7425=LINE('',#66542,#9936);
#7426=LINE('',#66544,#9937);
#7427=LINE('',#66545,#9938);
#7428=LINE('',#66548,#9939);
#7429=LINE('',#66549,#9940);
#7430=LINE('',#66554,#9941);
#7431=LINE('',#66556,#9942);
#7432=LINE('',#66557,#9943);
#7433=LINE('',#66560,#9944);
#7434=LINE('',#66561,#9945);
#7435=LINE('',#66568,#9946);
#7436=LINE('',#66570,#9947);
#7437=LINE('',#66571,#9948);
#7438=LINE('',#66574,#9949);
#7439=LINE('',#66575,#9950);
#7440=LINE('',#66580,#9951);
#7441=LINE('',#66582,#9952);
#7442=LINE('',#66583,#9953);
#7443=LINE('',#66586,#9954);
#7444=LINE('',#66587,#9955);
#7445=LINE('',#66592,#9956);
#7446=LINE('',#66594,#9957);
#7447=LINE('',#66595,#9958);
#7448=LINE('',#66598,#9959);
#7449=LINE('',#66599,#9960);
#7450=LINE('',#66604,#9961);
#7451=LINE('',#66606,#9962);
#7452=LINE('',#66607,#9963);
#7453=LINE('',#66610,#9964);
#7454=LINE('',#66611,#9965);
#7455=LINE('',#66616,#9966);
#7456=LINE('',#66618,#9967);
#7457=LINE('',#66619,#9968);
#7458=LINE('',#66622,#9969);
#7459=LINE('',#66623,#9970);
#7460=LINE('',#66628,#9971);
#7461=LINE('',#66630,#9972);
#7462=LINE('',#66631,#9973);
#7463=LINE('',#66634,#9974);
#7464=LINE('',#66635,#9975);
#7465=LINE('',#66640,#9976);
#7466=LINE('',#66642,#9977);
#7467=LINE('',#66643,#9978);
#7468=LINE('',#66646,#9979);
#7469=LINE('',#66647,#9980);
#7470=LINE('',#66652,#9981);
#7471=LINE('',#66654,#9982);
#7472=LINE('',#66655,#9983);
#7473=LINE('',#66658,#9984);
#7474=LINE('',#66659,#9985);
#7475=LINE('',#66664,#9986);
#7476=LINE('',#66666,#9987);
#7477=LINE('',#66667,#9988);
#7478=LINE('',#66670,#9989);
#7479=LINE('',#66671,#9990);
#7480=LINE('',#66676,#9991);
#7481=LINE('',#66678,#9992);
#7482=LINE('',#66679,#9993);
#7483=LINE('',#66682,#9994);
#7484=LINE('',#66683,#9995);
#7485=LINE('',#66688,#9996);
#7486=LINE('',#66690,#9997);
#7487=LINE('',#66691,#9998);
#7488=LINE('',#66694,#9999);
#7489=LINE('',#66695,#10000);
#7490=LINE('',#66700,#10001);
#7491=LINE('',#66702,#10002);
#7492=LINE('',#66703,#10003);
#7493=LINE('',#66706,#10004);
#7494=LINE('',#66707,#10005);
#7495=LINE('',#66712,#10006);
#7496=LINE('',#66714,#10007);
#7497=LINE('',#66715,#10008);
#7498=LINE('',#66718,#10009);
#7499=LINE('',#66719,#10010);
#7500=LINE('',#66724,#10011);
#7501=LINE('',#66726,#10012);
#7502=LINE('',#66727,#10013);
#7503=LINE('',#66730,#10014);
#7504=LINE('',#66731,#10015);
#7505=LINE('',#66736,#10016);
#7506=LINE('',#66738,#10017);
#7507=LINE('',#66739,#10018);
#7508=LINE('',#66742,#10019);
#7509=LINE('',#66743,#10020);
#7510=LINE('',#66748,#10021);
#7511=LINE('',#66750,#10022);
#7512=LINE('',#66751,#10023);
#7513=LINE('',#66754,#10024);
#7514=LINE('',#66755,#10025);
#7515=LINE('',#66760,#10026);
#7516=LINE('',#66762,#10027);
#7517=LINE('',#66763,#10028);
#7518=LINE('',#66766,#10029);
#7519=LINE('',#66767,#10030);
#7520=LINE('',#66772,#10031);
#7521=LINE('',#66774,#10032);
#7522=LINE('',#66775,#10033);
#7523=LINE('',#66778,#10034);
#7524=LINE('',#66779,#10035);
#7525=LINE('',#66783,#10036);
#7526=LINE('',#66787,#10037);
#7527=LINE('',#66789,#10038);
#7528=LINE('',#66791,#10039);
#7529=LINE('',#66793,#10040);
#7530=LINE('',#66795,#10041);
#7531=LINE('',#66796,#10042);
#7532=LINE('',#66800,#10043);
#7533=LINE('',#66804,#10044);
#7534=LINE('',#66808,#10045);
#7535=LINE('',#66812,#10046);
#7536=LINE('',#66816,#10047);
#7537=LINE('',#66819,#10048);
#7538=LINE('',#66823,#10049);
#7539=LINE('',#66825,#10050);
#7540=LINE('',#66826,#10051);
#7541=LINE('',#66828,#10052);
#7542=LINE('',#66830,#10053);
#7543=LINE('',#66832,#10054);
#7544=LINE('',#66834,#10055);
#7545=LINE('',#66840,#10056);
#7546=LINE('',#67099,#10057);
#7547=LINE('',#67517,#10058);
#7548=LINE('',#67785,#10059);
#7549=LINE('',#68181,#10060);
#7550=LINE('',#68617,#10061);
#7551=LINE('',#69039,#10062);
#7552=LINE('',#69473,#10063);
#7553=LINE('',#69905,#10064);
#7554=LINE('',#70148,#10065);
#7555=LINE('',#70520,#10066);
#7556=LINE('',#70787,#10067);
#7557=LINE('',#71233,#10068);
#7558=LINE('',#71652,#10069);
#7559=LINE('',#72067,#10070);
#7560=LINE('',#72504,#10071);
#7561=LINE('',#72914,#10072);
#7562=LINE('',#73169,#10073);
#7563=LINE('',#73537,#10074);
#7564=LINE('',#82182,#10075);
#7565=LINE('',#82188,#10076);
#7566=LINE('',#82190,#10077);
#7567=LINE('',#82192,#10078);
#7568=LINE('',#82199,#10079);
#7569=LINE('',#82203,#10080);
#7570=LINE('',#82559,#10081);
#7571=LINE('',#82563,#10082);
#7572=LINE('',#82565,#10083);
#7573=LINE('',#82566,#10084);
#7574=LINE('',#82569,#10085);
#7575=LINE('',#82570,#10086);
#7576=LINE('',#82575,#10087);
#7577=LINE('',#82577,#10088);
#7578=LINE('',#82578,#10089);
#7579=LINE('',#82581,#10090);
#7580=LINE('',#82582,#10091);
#7581=LINE('',#82587,#10092);
#7582=LINE('',#82589,#10093);
#7583=LINE('',#82590,#10094);
#7584=LINE('',#82593,#10095);
#7585=LINE('',#82594,#10096);
#7586=LINE('',#82599,#10097);
#7587=LINE('',#82601,#10098);
#7588=LINE('',#82602,#10099);
#7589=LINE('',#82605,#10100);
#7590=LINE('',#82606,#10101);
#7591=LINE('',#82611,#10102);
#7592=LINE('',#82613,#10103);
#7593=LINE('',#82614,#10104);
#7594=LINE('',#82617,#10105);
#7595=LINE('',#82618,#10106);
#7596=LINE('',#82623,#10107);
#7597=LINE('',#82625,#10108);
#7598=LINE('',#82626,#10109);
#7599=LINE('',#82629,#10110);
#7600=LINE('',#82630,#10111);
#7601=LINE('',#82635,#10112);
#7602=LINE('',#82637,#10113);
#7603=LINE('',#82638,#10114);
#7604=LINE('',#82641,#10115);
#7605=LINE('',#82642,#10116);
#7606=LINE('',#82647,#10117);
#7607=LINE('',#82649,#10118);
#7608=LINE('',#82650,#10119);
#7609=LINE('',#82653,#10120);
#7610=LINE('',#82654,#10121);
#7611=LINE('',#82659,#10122);
#7612=LINE('',#82661,#10123);
#7613=LINE('',#82662,#10124);
#7614=LINE('',#82665,#10125);
#7615=LINE('',#82666,#10126);
#7616=LINE('',#82671,#10127);
#7617=LINE('',#82673,#10128);
#7618=LINE('',#82674,#10129);
#7619=LINE('',#82677,#10130);
#7620=LINE('',#82678,#10131);
#7621=LINE('',#82683,#10132);
#7622=LINE('',#82685,#10133);
#7623=LINE('',#82686,#10134);
#7624=LINE('',#82689,#10135);
#7625=LINE('',#82690,#10136);
#7626=LINE('',#82695,#10137);
#7627=LINE('',#82697,#10138);
#7628=LINE('',#82698,#10139);
#7629=LINE('',#82701,#10140);
#7630=LINE('',#82702,#10141);
#7631=LINE('',#82707,#10142);
#7632=LINE('',#82709,#10143);
#7633=LINE('',#82710,#10144);
#7634=LINE('',#82713,#10145);
#7635=LINE('',#82714,#10146);
#7636=LINE('',#82719,#10147);
#7637=LINE('',#82721,#10148);
#7638=LINE('',#82722,#10149);
#7639=LINE('',#82725,#10150);
#7640=LINE('',#82726,#10151);
#7641=LINE('',#82731,#10152);
#7642=LINE('',#82733,#10153);
#7643=LINE('',#82734,#10154);
#7644=LINE('',#82737,#10155);
#7645=LINE('',#82738,#10156);
#7646=LINE('',#82743,#10157);
#7647=LINE('',#82745,#10158);
#7648=LINE('',#82746,#10159);
#7649=LINE('',#82749,#10160);
#7650=LINE('',#82750,#10161);
#7651=LINE('',#82755,#10162);
#7652=LINE('',#82757,#10163);
#7653=LINE('',#82758,#10164);
#7654=LINE('',#82761,#10165);
#7655=LINE('',#82762,#10166);
#7656=LINE('',#82769,#10167);
#7657=LINE('',#82771,#10168);
#7658=LINE('',#82772,#10169);
#7659=LINE('',#82775,#10170);
#7660=LINE('',#82776,#10171);
#7661=LINE('',#82781,#10172);
#7662=LINE('',#82783,#10173);
#7663=LINE('',#82784,#10174);
#7664=LINE('',#82787,#10175);
#7665=LINE('',#82788,#10176);
#7666=LINE('',#82793,#10177);
#7667=LINE('',#82795,#10178);
#7668=LINE('',#82796,#10179);
#7669=LINE('',#82799,#10180);
#7670=LINE('',#82800,#10181);
#7671=LINE('',#82805,#10182);
#7672=LINE('',#82807,#10183);
#7673=LINE('',#82808,#10184);
#7674=LINE('',#82811,#10185);
#7675=LINE('',#82812,#10186);
#7676=LINE('',#82817,#10187);
#7677=LINE('',#82819,#10188);
#7678=LINE('',#82820,#10189);
#7679=LINE('',#82823,#10190);
#7680=LINE('',#82824,#10191);
#7681=LINE('',#82829,#10192);
#7682=LINE('',#82831,#10193);
#7683=LINE('',#82832,#10194);
#7684=LINE('',#82835,#10195);
#7685=LINE('',#82836,#10196);
#7686=LINE('',#82841,#10197);
#7687=LINE('',#82843,#10198);
#7688=LINE('',#82844,#10199);
#7689=LINE('',#82847,#10200);
#7690=LINE('',#82848,#10201);
#7691=LINE('',#82853,#10202);
#7692=LINE('',#82855,#10203);
#7693=LINE('',#82856,#10204);
#7694=LINE('',#82859,#10205);
#7695=LINE('',#82860,#10206);
#7696=LINE('',#82865,#10207);
#7697=LINE('',#82867,#10208);
#7698=LINE('',#82868,#10209);
#7699=LINE('',#82871,#10210);
#7700=LINE('',#82872,#10211);
#7701=LINE('',#82877,#10212);
#7702=LINE('',#82879,#10213);
#7703=LINE('',#82880,#10214);
#7704=LINE('',#82883,#10215);
#7705=LINE('',#82884,#10216);
#7706=LINE('',#82889,#10217);
#7707=LINE('',#82891,#10218);
#7708=LINE('',#82892,#10219);
#7709=LINE('',#82895,#10220);
#7710=LINE('',#82896,#10221);
#7711=LINE('',#82901,#10222);
#7712=LINE('',#82903,#10223);
#7713=LINE('',#82904,#10224);
#7714=LINE('',#82907,#10225);
#7715=LINE('',#82908,#10226);
#7716=LINE('',#82913,#10227);
#7717=LINE('',#82915,#10228);
#7718=LINE('',#82916,#10229);
#7719=LINE('',#82919,#10230);
#7720=LINE('',#82920,#10231);
#7721=LINE('',#82925,#10232);
#7722=LINE('',#82927,#10233);
#7723=LINE('',#82928,#10234);
#7724=LINE('',#82931,#10235);
#7725=LINE('',#82932,#10236);
#7726=LINE('',#82937,#10237);
#7727=LINE('',#82939,#10238);
#7728=LINE('',#82940,#10239);
#7729=LINE('',#82943,#10240);
#7730=LINE('',#82944,#10241);
#7731=LINE('',#82949,#10242);
#7732=LINE('',#82951,#10243);
#7733=LINE('',#82952,#10244);
#7734=LINE('',#82955,#10245);
#7735=LINE('',#82956,#10246);
#7736=LINE('',#82961,#10247);
#7737=LINE('',#82963,#10248);
#7738=LINE('',#82964,#10249);
#7739=LINE('',#82967,#10250);
#7740=LINE('',#82968,#10251);
#7741=LINE('',#82973,#10252);
#7742=LINE('',#82975,#10253);
#7743=LINE('',#82976,#10254);
#7744=LINE('',#82979,#10255);
#7745=LINE('',#82980,#10256);
#7746=LINE('',#82984,#10257);
#7747=LINE('',#82988,#10258);
#7748=LINE('',#82990,#10259);
#7749=LINE('',#82992,#10260);
#7750=LINE('',#82994,#10261);
#7751=LINE('',#82996,#10262);
#7752=LINE('',#82997,#10263);
#7753=LINE('',#83001,#10264);
#7754=LINE('',#83005,#10265);
#7755=LINE('',#83009,#10266);
#7756=LINE('',#83013,#10267);
#7757=LINE('',#83017,#10268);
#7758=LINE('',#83020,#10269);
#7759=LINE('',#83024,#10270);
#7760=LINE('',#83026,#10271);
#7761=LINE('',#83027,#10272);
#7762=LINE('',#83029,#10273);
#7763=LINE('',#83031,#10274);
#7764=LINE('',#83033,#10275);
#7765=LINE('',#83035,#10276);
#7766=LINE('',#83042,#10277);
#7767=LINE('',#83050,#10278);
#7768=LINE('',#83053,#10279);
#7769=LINE('',#83059,#10280);
#7770=LINE('',#83065,#10281);
#7771=LINE('',#83069,#10282);
#7772=LINE('',#83078,#10283);
#7773=LINE('',#83082,#10284);
#7774=LINE('',#83090,#10285);
#7775=LINE('',#83117,#10286);
#7776=LINE('',#83120,#10287);
#7777=LINE('',#83122,#10288);
#7778=LINE('',#83123,#10289);
#7779=LINE('',#83126,#10290);
#7780=LINE('',#83127,#10291);
#7781=LINE('',#83130,#10292);
#7782=LINE('',#83131,#10293);
#7783=LINE('',#83134,#10294);
#7784=LINE('',#83135,#10295);
#7785=LINE('',#83138,#10296);
#7786=LINE('',#83139,#10297);
#7787=LINE('',#83141,#10298);
#7788=VECTOR('',#29263,1.9525);
#7789=VECTOR('',#29268,1.8025);
#7790=VECTOR('',#29275,10.);
#7791=VECTOR('',#29276,10.);
#7792=VECTOR('',#29277,10.);
#7793=VECTOR('',#29278,10.);
#7794=VECTOR('',#29283,1.9525);
#7795=VECTOR('',#29288,1.8025);
#7796=VECTOR('',#29295,10.);
#7797=VECTOR('',#29296,10.);
#7798=VECTOR('',#29297,10.);
#7799=VECTOR('',#29298,10.);
#7800=VECTOR('',#29301,1.80249999999999);
#7801=VECTOR('',#29304,1.80249999999999);
#7802=VECTOR('',#29309,1.9525);
#7803=VECTOR('',#29314,1.8025);
#7804=VECTOR('',#29321,10.);
#7805=VECTOR('',#29322,10.);
#7806=VECTOR('',#29323,10.);
#7807=VECTOR('',#29324,10.);
#7808=VECTOR('',#29329,1.9525);
#7809=VECTOR('',#29334,1.8025);
#7810=VECTOR('',#29341,10.);
#7811=VECTOR('',#29342,10.);
#7812=VECTOR('',#29343,10.);
#7813=VECTOR('',#29344,10.);
#7814=VECTOR('',#29347,0.901249999999996);
#7815=VECTOR('',#29350,0.901249999999996);
#7816=VECTOR('',#29355,1.778);
#7817=VECTOR('',#29362,1.778);
#7818=VECTOR('',#29369,1.778);
#7819=VECTOR('',#29376,1.778);
#7820=VECTOR('',#29383,1.9525);
#7821=VECTOR('',#29388,10.);
#7822=VECTOR('',#29389,10.);
#7823=VECTOR('',#29390,10.);
#7824=VECTOR('',#29391,10.);
#7825=VECTOR('',#29392,10.);
#7826=VECTOR('',#29393,10.);
#7827=VECTOR('',#29394,10.);
#7828=VECTOR('',#29395,10.);
#7829=VECTOR('',#29396,10.);
#7830=VECTOR('',#29397,10.);
#7831=VECTOR('',#29398,10.);
#7832=VECTOR('',#29399,10.);
#7833=VECTOR('',#29400,10.);
#7834=VECTOR('',#29401,10.);
#7835=VECTOR('',#29402,10.);
#7836=VECTOR('',#29403,10.);
#7837=VECTOR('',#29404,10.);
#7838=VECTOR('',#29405,10.);
#7839=VECTOR('',#29406,10.);
#7840=VECTOR('',#29407,10.);
#7841=VECTOR('',#29418,1.8025);
#7842=VECTOR('',#29425,1.9525);
#7843=VECTOR('',#29428,1.8025);
#7844=VECTOR('',#29435,1.9525);
#7845=VECTOR('',#29438,1.8025);
#7846=VECTOR('',#29445,1.9525);
#7847=VECTOR('',#29448,1.8025);
#7848=VECTOR('',#29455,6.563);
#7849=VECTOR('',#29458,6.363);
#7850=VECTOR('',#29463,10.);
#7851=VECTOR('',#29464,10.);
#7852=VECTOR('',#29465,10.);
#7853=VECTOR('',#29468,9.99999999999999);
#7854=VECTOR('',#29469,10.);
#7855=VECTOR('',#29472,10.);
#7856=VECTOR('',#29475,10.);
#7857=VECTOR('',#29476,10.);
#7858=VECTOR('',#29477,10.);
#7859=VECTOR('',#29480,10.);
#7860=VECTOR('',#29481,10.);
#7861=VECTOR('',#29484,10.);
#7862=VECTOR('',#29485,10.);
#7863=VECTOR('',#29486,10.);
#7864=VECTOR('',#29489,10.);
#7865=VECTOR('',#29492,10.);
#7866=VECTOR('',#29493,10.);
#7867=VECTOR('',#29494,10.);
#7868=VECTOR('',#29497,10.);
#7869=VECTOR('',#29498,10.);
#7870=VECTOR('',#29501,10.);
#7871=VECTOR('',#29502,10.);
#7872=VECTOR('',#29505,10.);
#7873=VECTOR('',#29508,10.);
#7874=VECTOR('',#29509,9.99999999999999);
#7875=VECTOR('',#29512,10.);
#7876=VECTOR('',#29515,10.);
#7877=VECTOR('',#29518,10.);
#7878=VECTOR('',#29521,10.);
#7879=VECTOR('',#29522,10.);
#7880=VECTOR('',#29525,10.);
#7881=VECTOR('',#29528,10.);
#7882=VECTOR('',#29529,10.);
#7883=VECTOR('',#29532,10.);
#7884=VECTOR('',#29533,10.);
#7885=VECTOR('',#29536,10.);
#7886=VECTOR('',#29539,10.);
#7887=VECTOR('',#29540,10.);
#7888=VECTOR('',#29543,10.);
#7889=VECTOR('',#29544,10.);
#7890=VECTOR('',#29547,10.);
#7891=VECTOR('',#29548,10.);
#7892=VECTOR('',#29551,10.);
#7893=VECTOR('',#29554,10.);
#7894=VECTOR('',#29555,10.);
#7895=VECTOR('',#29558,10.);
#7896=VECTOR('',#29559,10.);
#7897=VECTOR('',#29562,10.);
#7898=VECTOR('',#29563,10.);
#7899=VECTOR('',#29566,10.);
#7900=VECTOR('',#29567,10.);
#7901=VECTOR('',#29570,10.);
#7902=VECTOR('',#29571,10.);
#7903=VECTOR('',#29572,10.);
#7904=VECTOR('',#29575,10.);
#7905=VECTOR('',#29576,10.);
#7906=VECTOR('',#29579,10.);
#7907=VECTOR('',#29582,10.);
#7908=VECTOR('',#29585,10.);
#7909=VECTOR('',#29588,10.);
#7910=VECTOR('',#29589,10.);
#7911=VECTOR('',#29590,10.);
#7912=VECTOR('',#29593,10.);
#7913=VECTOR('',#29594,10.);
#7914=VECTOR('',#29605,1.903);
#7915=VECTOR('',#29610,10.);
#7916=VECTOR('',#29613,10.);
#7917=VECTOR('',#29616,10.);
#7918=VECTOR('',#29617,10.);
#7919=VECTOR('',#29618,10.);
#7920=VECTOR('',#29619,10.);
#7921=VECTOR('',#29620,10.);
#7922=VECTOR('',#29621,10.);
#7923=VECTOR('',#29622,10.);
#7924=VECTOR('',#29623,10.);
#7925=VECTOR('',#29624,10.);
#7926=VECTOR('',#29627,10.);
#7927=VECTOR('',#29630,10.);
#7928=VECTOR('',#29631,10.);
#7929=VECTOR('',#29632,10.);
#7930=VECTOR('',#29633,10.);
#7931=VECTOR('',#29634,10.);
#7932=VECTOR('',#29635,10.);
#7933=VECTOR('',#29636,10.);
#7934=VECTOR('',#29637,10.);
#7935=VECTOR('',#29650,10.);
#7936=VECTOR('',#29651,10.);
#7937=VECTOR('',#29654,10.);
#7938=VECTOR('',#29657,10.);
#7939=VECTOR('',#29658,10.);
#7940=VECTOR('',#29661,10.);
#7941=VECTOR('',#29662,10.);
#7942=VECTOR('',#29665,10.);
#7943=VECTOR('',#29668,10.);
#7944=VECTOR('',#29669,10.);
#7945=VECTOR('',#29678,1.778);
#7946=VECTOR('',#29683,1.903);
#7947=VECTOR('',#29688,1.778);
#7948=VECTOR('',#29693,1.903);
#7949=VECTOR('',#29698,1.778);
#7950=VECTOR('',#29703,1.903);
#7951=VECTOR('',#29708,1.778);
#7952=VECTOR('',#29713,1.9525);
#7953=VECTOR('',#29718,10.);
#7954=VECTOR('',#29721,10.);
#7955=VECTOR('',#29724,10.);
#7956=VECTOR('',#29725,10.);
#7957=VECTOR('',#29726,10.);
#7958=VECTOR('',#29727,10.);
#7959=VECTOR('',#29728,10.);
#7960=VECTOR('',#29729,10.);
#7961=VECTOR('',#29730,10.);
#7962=VECTOR('',#29731,10.);
#7963=VECTOR('',#29732,10.);
#7964=VECTOR('',#29735,10.);
#7965=VECTOR('',#29738,10.);
#7966=VECTOR('',#29739,10.);
#7967=VECTOR('',#29740,10.);
#7968=VECTOR('',#29741,10.);
#7969=VECTOR('',#29742,10.);
#7970=VECTOR('',#29743,10.);
#7971=VECTOR('',#29744,10.);
#7972=VECTOR('',#29745,10.);
#7973=VECTOR('',#29748,10.);
#7974=VECTOR('',#29751,10.);
#7975=VECTOR('',#29754,10.);
#7976=VECTOR('',#29755,10.);
#7977=VECTOR('',#29758,10.);
#7978=VECTOR('',#29759,10.);
#7979=VECTOR('',#29762,10.);
#7980=VECTOR('',#29765,10.);
#7981=VECTOR('',#29766,10.);
#7982=VECTOR('',#29769,10.);
#7983=VECTOR('',#29776,1.8025);
#7984=VECTOR('',#29781,1.9525);
#7985=VECTOR('',#29784,1.8025);
#7986=VECTOR('',#29789,1.9525);
#7987=VECTOR('',#29792,1.8025);
#7988=VECTOR('',#29797,1.9525);
#7989=VECTOR('',#29800,1.8025);
#7990=VECTOR('',#29803,10.);
#7991=VECTOR('',#29804,10.);
#7992=VECTOR('',#29805,10.);
#7993=VECTOR('',#29808,10.);
#7994=VECTOR('',#29809,10.);
#7995=VECTOR('',#29812,10.);
#7996=VECTOR('',#29813,10.);
#7997=VECTOR('',#29816,10.);
#7998=VECTOR('',#29817,10.);
#7999=VECTOR('',#29820,10.);
#8000=VECTOR('',#29821,10.);
#8001=VECTOR('',#29822,10.);
#8002=VECTOR('',#29825,10.);
#8003=VECTOR('',#29826,10.);
#8004=VECTOR('',#29829,10.);
#8005=VECTOR('',#29830,10.);
#8006=VECTOR('',#29833,10.);
#8007=VECTOR('',#29834,10.);
#8008=VECTOR('',#29837,10.);
#8009=VECTOR('',#29838,10.);
#8010=VECTOR('',#29841,10.);
#8011=VECTOR('',#29842,10.);
#8012=VECTOR('',#29845,10.);
#8013=VECTOR('',#29846,10.);
#8014=VECTOR('',#29849,10.);
#8015=VECTOR('',#29850,10.);
#8016=VECTOR('',#29853,10.);
#8017=VECTOR('',#29854,10.);
#8018=VECTOR('',#29855,10.);
#8019=VECTOR('',#29858,10.);
#8020=VECTOR('',#29863,10.);
#8021=VECTOR('',#29864,10.);
#8022=VECTOR('',#29867,10.);
#8023=VECTOR('',#29872,10.);
#8024=VECTOR('',#29875,9.99999999999999);
#8025=VECTOR('',#29880,9.99999999999999);
#8026=VECTOR('',#29881,10.);
#8027=VECTOR('',#29884,9.99999999999999);
#8028=VECTOR('',#29889,10.);
#8029=VECTOR('',#29892,10.);
#8030=VECTOR('',#29893,10.);
#8031=VECTOR('',#29896,10.);
#8032=VECTOR('',#29897,10.);
#8033=VECTOR('',#29900,10.);
#8034=VECTOR('',#29903,10.);
#8035=VECTOR('',#29904,10.);
#8036=VECTOR('',#29907,10.);
#8037=VECTOR('',#29910,10.);
#8038=VECTOR('',#29913,10.);
#8039=VECTOR('',#29916,10.);
#8040=VECTOR('',#29919,10.);
#8041=VECTOR('',#29922,10.);
#8042=VECTOR('',#29925,10.);
#8043=VECTOR('',#29928,10.);
#8044=VECTOR('',#29931,10.);
#8045=VECTOR('',#29934,10.);
#8046=VECTOR('',#29937,10.);
#8047=VECTOR('',#29940,10.);
#8048=VECTOR('',#29941,10.);
#8049=VECTOR('',#29942,10.);
#8050=VECTOR('',#29945,10.);
#8051=VECTOR('',#29946,10.);
#8052=VECTOR('',#29947,10.);
#8053=VECTOR('',#29950,10.);
#8054=VECTOR('',#29951,10.);
#8055=VECTOR('',#29952,10.);
#8056=VECTOR('',#29955,10.);
#8057=VECTOR('',#29960,10.);
#8058=VECTOR('',#29963,10.);
#8059=VECTOR('',#29964,10.);
#8060=VECTOR('',#29965,10.);
#8061=VECTOR('',#29968,10.);
#8062=VECTOR('',#29973,10.);
#8063=VECTOR('',#29974,10.);
#8064=VECTOR('',#29977,10.);
#8065=VECTOR('',#29982,10.);
#8066=VECTOR('',#29985,10.);
#8067=VECTOR('',#29990,10.);
#8068=VECTOR('',#29991,10.);
#8069=VECTOR('',#29994,10.);
#8070=VECTOR('',#29999,10.);
#8071=VECTOR('',#30002,9.99999999999999);
#8072=VECTOR('',#30007,10.);
#8073=VECTOR('',#30010,10.);
#8074=VECTOR('',#30011,10.);
#8075=VECTOR('',#30014,10.);
#8076=VECTOR('',#30017,10.);
#8077=VECTOR('',#30020,10.);
#8078=VECTOR('',#30023,10.);
#8079=VECTOR('',#30026,10.);
#8080=VECTOR('',#30029,10.);
#8081=VECTOR('',#30032,10.);
#8082=VECTOR('',#30035,10.);
#8083=VECTOR('',#30038,10.);
#8084=VECTOR('',#30039,10.);
#8085=VECTOR('',#30044,10.);
#8086=VECTOR('',#30047,10.);
#8087=VECTOR('',#30050,10.);
#8088=VECTOR('',#30053,10.);
#8089=VECTOR('',#30058,10.);
#8090=VECTOR('',#30061,10.);
#8091=VECTOR('',#30062,10.);
#8092=VECTOR('',#30067,10.);
#8093=VECTOR('',#30070,10.);
#8094=VECTOR('',#30071,10.);
#8095=VECTOR('',#30074,10.);
#8096=VECTOR('',#30079,10.);
#8097=VECTOR('',#30082,10.);
#8098=VECTOR('',#30085,10.);
#8099=VECTOR('',#30088,10.);
#8100=VECTOR('',#30097,2.5);
#8101=VECTOR('',#30106,2.);
#8102=VECTOR('',#30113,2.);
#8103=VECTOR('',#30120,2.);
#8104=VECTOR('',#30127,2.);
#8105=VECTOR('',#30134,1.65);
#8106=VECTOR('',#30139,1.55);
#8107=VECTOR('',#30148,1.55);
#8108=VECTOR('',#30153,3.255);
#8109=VECTOR('',#30158,3.105);
#8110=VECTOR('',#30163,5.5);
#8111=VECTOR('',#30172,5.35);
#8112=VECTOR('',#30175,10.);
#8113=VECTOR('',#30176,10.);
#8114=VECTOR('',#30177,10.);
#8115=VECTOR('',#30178,10.);
#8116=VECTOR('',#30185,10.);
#8117=VECTOR('',#30190,10.);
#8118=VECTOR('',#30193,10.);
#8119=VECTOR('',#30196,10.);
#8120=VECTOR('',#30197,10.);
#8121=VECTOR('',#30198,10.);
#8122=VECTOR('',#30205,10.);
#8123=VECTOR('',#30210,10.);
#8124=VECTOR('',#30215,10.);
#8125=VECTOR('',#30216,10.);
#8126=VECTOR('',#30219,10.);
#8127=VECTOR('',#30222,10.);
#8128=VECTOR('',#30225,10.);
#8129=VECTOR('',#30228,10.);
#8130=VECTOR('',#30231,10.);
#8131=VECTOR('',#30234,10.);
#8132=VECTOR('',#30239,10.);
#8133=VECTOR('',#30242,10.);
#8134=VECTOR('',#30245,10.);
#8135=VECTOR('',#30248,10.);
#8136=VECTOR('',#30251,10.);
#8137=VECTOR('',#30252,10.);
#8138=VECTOR('',#30255,10.);
#8139=VECTOR('',#30258,10.);
#8140=VECTOR('',#30259,10.);
#8141=VECTOR('',#30260,10.);
#8142=VECTOR('',#30265,10.);
#8143=VECTOR('',#30268,10.);
#8144=VECTOR('',#30269,10.);
#8145=VECTOR('',#30274,10.);
#8146=VECTOR('',#30277,10.);
#8147=VECTOR('',#30278,10.);
#8148=VECTOR('',#30279,10.);
#8149=VECTOR('',#30288,10.);
#8150=VECTOR('',#30293,10.);
#8151=VECTOR('',#30298,10.);
#8152=VECTOR('',#30299,10.);
#8153=VECTOR('',#30300,10.);
#8154=VECTOR('',#30307,10.);
#8155=VECTOR('',#30310,10.);
#8156=VECTOR('',#30311,10.);
#8157=VECTOR('',#30312,10.);
#8158=VECTOR('',#30319,10.);
#8159=VECTOR('',#30322,10.);
#8160=VECTOR('',#30323,10.);
#8161=VECTOR('',#30328,10.);
#8162=VECTOR('',#30331,10.);
#8163=VECTOR('',#30332,10.);
#8164=VECTOR('',#30345,10.);
#8165=VECTOR('',#30346,10.);
#8166=VECTOR('',#30347,10.);
#8167=VECTOR('',#30348,10.);
#8168=VECTOR('',#30353,10.);
#8169=VECTOR('',#30356,10.);
#8170=VECTOR('',#30357,10.);
#8171=VECTOR('',#30360,10.);
#8172=VECTOR('',#30361,10.);
#8173=VECTOR('',#30362,10.);
#8174=VECTOR('',#30367,10.);
#8175=VECTOR('',#30370,10.);
#8176=VECTOR('',#30373,9.99999999999999);
#8177=VECTOR('',#30376,10.);
#8178=VECTOR('',#30379,10.);
#8179=VECTOR('',#30382,10.);
#8180=VECTOR('',#30385,10.);
#8181=VECTOR('',#30388,10.);
#8182=VECTOR('',#30391,10.);
#8183=VECTOR('',#30394,10.);
#8184=VECTOR('',#30397,10.);
#8185=VECTOR('',#30400,10.);
#8186=VECTOR('',#30403,10.);
#8187=VECTOR('',#30406,10.);
#8188=VECTOR('',#30409,10.);
#8189=VECTOR('',#30412,10.);
#8190=VECTOR('',#30415,10.);
#8191=VECTOR('',#30418,10.);
#8192=VECTOR('',#30421,10.);
#8193=VECTOR('',#30424,10.);
#8194=VECTOR('',#30427,10.);
#8195=VECTOR('',#30430,10.);
#8196=VECTOR('',#30433,10.);
#8197=VECTOR('',#30436,10.);
#8198=VECTOR('',#30439,10.);
#8199=VECTOR('',#30442,10.);
#8200=VECTOR('',#30445,10.);
#8201=VECTOR('',#30448,10.);
#8202=VECTOR('',#30451,10.);
#8203=VECTOR('',#30454,10.);
#8204=VECTOR('',#30463,10.);
#8205=VECTOR('',#30466,10.);
#8206=VECTOR('',#30467,10.);
#8207=VECTOR('',#30470,10.);
#8208=VECTOR('',#30473,10.);
#8209=VECTOR('',#30474,10.);
#8210=VECTOR('',#30477,10.);
#8211=VECTOR('',#30478,10.);
#8212=VECTOR('',#30483,10.);
#8213=VECTOR('',#30486,9.99999999999999);
#8214=VECTOR('',#30487,10.);
#8215=VECTOR('',#30490,10.);
#8216=VECTOR('',#30493,10.);
#8217=VECTOR('',#30494,10.);
#8218=VECTOR('',#30497,10.);
#8219=VECTOR('',#30498,10.);
#8220=VECTOR('',#30503,10.);
#8221=VECTOR('',#30506,10.);
#8222=VECTOR('',#30507,10.);
#8223=VECTOR('',#30510,10.);
#8224=VECTOR('',#30513,10.);
#8225=VECTOR('',#30514,10.);
#8226=VECTOR('',#30517,10.);
#8227=VECTOR('',#30518,10.);
#8228=VECTOR('',#30523,10.);
#8229=VECTOR('',#30526,10.);
#8230=VECTOR('',#30527,10.);
#8231=VECTOR('',#30530,10.);
#8232=VECTOR('',#30533,10.);
#8233=VECTOR('',#30534,10.);
#8234=VECTOR('',#30537,10.);
#8235=VECTOR('',#30538,10.);
#8236=VECTOR('',#30543,10.);
#8237=VECTOR('',#30546,10.);
#8238=VECTOR('',#30547,10.);
#8239=VECTOR('',#30550,10.);
#8240=VECTOR('',#30553,10.);
#8241=VECTOR('',#30554,10.);
#8242=VECTOR('',#30557,10.);
#8243=VECTOR('',#30558,10.);
#8244=VECTOR('',#30563,10.);
#8245=VECTOR('',#30566,10.);
#8246=VECTOR('',#30567,10.);
#8247=VECTOR('',#30570,10.);
#8248=VECTOR('',#30573,10.);
#8249=VECTOR('',#30574,10.);
#8250=VECTOR('',#30577,10.);
#8251=VECTOR('',#30578,10.);
#8252=VECTOR('',#30583,10.);
#8253=VECTOR('',#30586,10.);
#8254=VECTOR('',#30587,10.);
#8255=VECTOR('',#30590,10.);
#8256=VECTOR('',#30593,10.);
#8257=VECTOR('',#30594,10.);
#8258=VECTOR('',#30597,10.);
#8259=VECTOR('',#30598,10.);
#8260=VECTOR('',#30603,10.);
#8261=VECTOR('',#30606,10.);
#8262=VECTOR('',#30607,10.);
#8263=VECTOR('',#30610,10.);
#8264=VECTOR('',#30613,10.);
#8265=VECTOR('',#30614,10.);
#8266=VECTOR('',#30617,10.);
#8267=VECTOR('',#30618,10.);
#8268=VECTOR('',#30623,10.);
#8269=VECTOR('',#30626,10.);
#8270=VECTOR('',#30627,10.);
#8271=VECTOR('',#30630,10.);
#8272=VECTOR('',#30633,10.);
#8273=VECTOR('',#30634,10.);
#8274=VECTOR('',#30637,10.);
#8275=VECTOR('',#30638,10.);
#8276=VECTOR('',#30643,10.);
#8277=VECTOR('',#30646,10.);
#8278=VECTOR('',#30647,10.);
#8279=VECTOR('',#30650,10.);
#8280=VECTOR('',#30653,10.);
#8281=VECTOR('',#30654,10.);
#8282=VECTOR('',#30657,10.);
#8283=VECTOR('',#30658,10.);
#8284=VECTOR('',#30663,10.);
#8285=VECTOR('',#30666,10.);
#8286=VECTOR('',#30667,10.);
#8287=VECTOR('',#30670,10.);
#8288=VECTOR('',#30673,10.);
#8289=VECTOR('',#30674,10.);
#8290=VECTOR('',#30677,10.);
#8291=VECTOR('',#30678,10.);
#8292=VECTOR('',#30683,10.);
#8293=VECTOR('',#30686,10.);
#8294=VECTOR('',#30687,10.);
#8295=VECTOR('',#30690,10.);
#8296=VECTOR('',#30693,10.);
#8297=VECTOR('',#30694,10.);
#8298=VECTOR('',#30697,10.);
#8299=VECTOR('',#30698,10.);
#8300=VECTOR('',#30703,10.);
#8301=VECTOR('',#30706,10.);
#8302=VECTOR('',#30707,10.);
#8303=VECTOR('',#30710,10.);
#8304=VECTOR('',#30713,10.);
#8305=VECTOR('',#30714,10.);
#8306=VECTOR('',#30717,10.);
#8307=VECTOR('',#30718,10.);
#8308=VECTOR('',#30723,10.);
#8309=VECTOR('',#30726,10.);
#8310=VECTOR('',#30727,10.);
#8311=VECTOR('',#30728,10.);
#8312=VECTOR('',#30731,10.);
#8313=VECTOR('',#30732,10.);
#8314=VECTOR('',#30735,10.);
#8315=VECTOR('',#30738,10.);
#8316=VECTOR('',#30743,10.);
#8317=VECTOR('',#30746,10.);
#8318=VECTOR('',#30753,10.);
#8319=VECTOR('',#30756,10.);
#8320=VECTOR('',#30759,10.);
#8321=VECTOR('',#30760,10.);
#8322=VECTOR('',#30763,10.);
#8323=VECTOR('',#30764,10.);
#8324=VECTOR('',#30777,1.6);
#8325=VECTOR('',#30784,4.477);
#8326=VECTOR('',#30787,3.261);
#8327=VECTOR('',#30792,1.17775);
#8328=VECTOR('',#30797,1.17775);
#8329=VECTOR('',#30800,1.17775);
#8330=VECTOR('',#30803,1.17775);
#8331=VECTOR('',#30806,1.17775);
#8332=VECTOR('',#30809,1.17775);
#8333=VECTOR('',#30812,1.17775);
#8334=VECTOR('',#30815,1.17775);
#8335=VECTOR('',#30818,1.17775);
#8336=VECTOR('',#30821,1.17775);
#8337=VECTOR('',#30824,1.17775);
#8338=VECTOR('',#30827,1.4635);
#8339=VECTOR('',#30832,1.4635);
#8340=VECTOR('',#30835,1.4635);
#8341=VECTOR('',#30838,1.4635);
#8342=VECTOR('',#30841,1.4635);
#8343=VECTOR('',#30844,1.4635);
#8344=VECTOR('',#30847,1.4635);
#8345=VECTOR('',#30850,1.4635);
#8346=VECTOR('',#30853,1.4635);
#8347=VECTOR('',#30856,1.4635);
#8348=VECTOR('',#30859,1.4635);
#8349=VECTOR('',#30892,1.2885);
#8350=VECTOR('',#30899,10.);
#8351=VECTOR('',#30900,10.);
#8352=VECTOR('',#30901,10.);
#8353=VECTOR('',#30906,10.);
#8354=VECTOR('',#30909,10.);
#8355=VECTOR('',#30914,2.75);
#8356=VECTOR('',#30921,10.);
#8357=VECTOR('',#30924,10.);
#8358=VECTOR('',#30927,10.);
#8359=VECTOR('',#30930,10.);
#8360=VECTOR('',#30933,10.);
#8361=VECTOR('',#30936,10.);
#8362=VECTOR('',#30939,10.);
#8363=VECTOR('',#30942,10.);
#8364=VECTOR('',#30945,10.);
#8365=VECTOR('',#30948,10.);
#8366=VECTOR('',#30951,10.);
#8367=VECTOR('',#30954,10.);
#8368=VECTOR('',#30957,10.);
#8369=VECTOR('',#30960,10.);
#8370=VECTOR('',#30963,10.);
#8371=VECTOR('',#30966,10.);
#8372=VECTOR('',#30969,10.);
#8373=VECTOR('',#30972,10.);
#8374=VECTOR('',#30975,10.);
#8375=VECTOR('',#30978,10.);
#8376=VECTOR('',#30981,10.);
#8377=VECTOR('',#30984,10.);
#8378=VECTOR('',#30987,10.);
#8379=VECTOR('',#30990,10.);
#8380=VECTOR('',#30993,10.);
#8381=VECTOR('',#30996,10.);
#8382=VECTOR('',#30999,10.);
#8383=VECTOR('',#31002,10.);
#8384=VECTOR('',#31005,10.);
#8385=VECTOR('',#31008,10.);
#8386=VECTOR('',#31011,10.);
#8387=VECTOR('',#31014,10.);
#8388=VECTOR('',#31017,10.);
#8389=VECTOR('',#31022,10.);
#8390=VECTOR('',#31025,10.);
#8391=VECTOR('',#31028,10.);
#8392=VECTOR('',#31031,10.);
#8393=VECTOR('',#31034,10.);
#8394=VECTOR('',#31037,10.);
#8395=VECTOR('',#31040,10.);
#8396=VECTOR('',#31043,10.);
#8397=VECTOR('',#31046,10.);
#8398=VECTOR('',#31049,10.);
#8399=VECTOR('',#31052,10.);
#8400=VECTOR('',#31055,10.);
#8401=VECTOR('',#31058,10.);
#8402=VECTOR('',#31061,10.);
#8403=VECTOR('',#31064,10.);
#8404=VECTOR('',#31067,10.);
#8405=VECTOR('',#31070,10.);
#8406=VECTOR('',#31073,10.);
#8407=VECTOR('',#31076,10.);
#8408=VECTOR('',#31079,10.);
#8409=VECTOR('',#31082,10.);
#8410=VECTOR('',#31085,10.);
#8411=VECTOR('',#31088,10.);
#8412=VECTOR('',#31091,10.);
#8413=VECTOR('',#31094,10.);
#8414=VECTOR('',#31097,10.);
#8415=VECTOR('',#31100,10.);
#8416=VECTOR('',#31103,10.);
#8417=VECTOR('',#31106,10.);
#8418=VECTOR('',#31109,10.);
#8419=VECTOR('',#31112,10.);
#8420=VECTOR('',#31115,10.);
#8421=VECTOR('',#31118,10.);
#8422=VECTOR('',#31121,10.);
#8423=VECTOR('',#31124,10.);
#8424=VECTOR('',#31127,10.);
#8425=VECTOR('',#31130,10.);
#8426=VECTOR('',#31133,10.);
#8427=VECTOR('',#31134,10.);
#8428=VECTOR('',#31137,10.);
#8429=VECTOR('',#31142,10.);
#8430=VECTOR('',#31143,10.);
#8431=VECTOR('',#31146,10.);
#8432=VECTOR('',#31151,10.);
#8433=VECTOR('',#31152,10.);
#8434=VECTOR('',#31155,10.);
#8435=VECTOR('',#31160,10.);
#8436=VECTOR('',#31161,10.);
#8437=VECTOR('',#31164,10.);
#8438=VECTOR('',#31169,10.);
#8439=VECTOR('',#31170,10.);
#8440=VECTOR('',#31173,10.);
#8441=VECTOR('',#31178,10.);
#8442=VECTOR('',#31179,10.);
#8443=VECTOR('',#31182,10.);
#8444=VECTOR('',#31187,10.);
#8445=VECTOR('',#31188,10.);
#8446=VECTOR('',#31191,10.);
#8447=VECTOR('',#31196,10.);
#8448=VECTOR('',#31197,10.);
#8449=VECTOR('',#31200,10.);
#8450=VECTOR('',#31205,10.);
#8451=VECTOR('',#31206,10.);
#8452=VECTOR('',#31209,10.);
#8453=VECTOR('',#31214,10.);
#8454=VECTOR('',#31215,10.);
#8455=VECTOR('',#31218,10.);
#8456=VECTOR('',#31223,10.);
#8457=VECTOR('',#31224,10.);
#8458=VECTOR('',#31227,10.);
#8459=VECTOR('',#31232,10.);
#8460=VECTOR('',#31233,10.);
#8461=VECTOR('',#31236,10.);
#8462=VECTOR('',#31241,10.);
#8463=VECTOR('',#31242,10.);
#8464=VECTOR('',#31245,10.);
#8465=VECTOR('',#31250,10.);
#8466=VECTOR('',#31251,10.);
#8467=VECTOR('',#31254,10.);
#8468=VECTOR('',#31259,10.);
#8469=VECTOR('',#31260,10.);
#8470=VECTOR('',#31263,10.);
#8471=VECTOR('',#31268,10.);
#8472=VECTOR('',#31269,10.);
#8473=VECTOR('',#31272,10.);
#8474=VECTOR('',#31277,10.);
#8475=VECTOR('',#31278,10.);
#8476=VECTOR('',#31281,10.);
#8477=VECTOR('',#31286,10.);
#8478=VECTOR('',#31287,10.);
#8479=VECTOR('',#31290,10.);
#8480=VECTOR('',#31295,10.);
#8481=VECTOR('',#31296,10.);
#8482=VECTOR('',#31299,10.);
#8483=VECTOR('',#31304,10.);
#8484=VECTOR('',#31305,10.);
#8485=VECTOR('',#31308,10.);
#8486=VECTOR('',#31313,10.);
#8487=VECTOR('',#31314,10.);
#8488=VECTOR('',#31317,10.);
#8489=VECTOR('',#31322,10.);
#8490=VECTOR('',#31323,10.);
#8491=VECTOR('',#31326,10.);
#8492=VECTOR('',#31331,10.);
#8493=VECTOR('',#31332,10.);
#8494=VECTOR('',#31335,10.);
#8495=VECTOR('',#31340,10.);
#8496=VECTOR('',#31341,10.);
#8497=VECTOR('',#31344,10.);
#8498=VECTOR('',#31349,10.);
#8499=VECTOR('',#31350,10.);
#8500=VECTOR('',#31353,10.);
#8501=VECTOR('',#31358,10.);
#8502=VECTOR('',#31359,10.);
#8503=VECTOR('',#31362,10.);
#8504=VECTOR('',#31367,10.);
#8505=VECTOR('',#31368,10.);
#8506=VECTOR('',#31371,10.);
#8507=VECTOR('',#31376,10.);
#8508=VECTOR('',#31377,10.);
#8509=VECTOR('',#31380,10.);
#8510=VECTOR('',#31385,10.);
#8511=VECTOR('',#31386,10.);
#8512=VECTOR('',#31389,10.);
#8513=VECTOR('',#31394,10.);
#8514=VECTOR('',#31395,10.);
#8515=VECTOR('',#31398,10.);
#8516=VECTOR('',#31403,10.);
#8517=VECTOR('',#31404,10.);
#8518=VECTOR('',#31407,10.);
#8519=VECTOR('',#31412,10.);
#8520=VECTOR('',#31413,10.);
#8521=VECTOR('',#31416,10.);
#8522=VECTOR('',#31421,10.);
#8523=VECTOR('',#31422,10.);
#8524=VECTOR('',#31425,10.);
#8525=VECTOR('',#31430,10.);
#8526=VECTOR('',#31431,10.);
#8527=VECTOR('',#31434,10.);
#8528=VECTOR('',#31439,10.);
#8529=VECTOR('',#31440,10.);
#8530=VECTOR('',#31443,10.);
#8531=VECTOR('',#31452,2.6);
#8532=VECTOR('',#31473,1.49337567297406);
#8533=VECTOR('',#31476,10.);
#8534=VECTOR('',#31477,10.);
#8535=VECTOR('',#31482,10.);
#8536=VECTOR('',#31483,10.);
#8537=VECTOR('',#31488,10.);
#8538=VECTOR('',#31491,10.);
#8539=VECTOR('',#31494,10.);
#8540=VECTOR('',#31495,10.);
#8541=VECTOR('',#31500,10.);
#8542=VECTOR('',#31503,10.);
#8543=VECTOR('',#31506,10.);
#8544=VECTOR('',#31509,10.);
#8545=VECTOR('',#31512,10.);
#8546=VECTOR('',#31513,10.);
#8547=VECTOR('',#31514,10.);
#8548=VECTOR('',#31515,10.);
#8549=VECTOR('',#31518,10.);
#8550=VECTOR('',#31519,10.);
#8551=VECTOR('',#31520,10.);
#8552=VECTOR('',#31523,10.);
#8553=VECTOR('',#31524,10.);
#8554=VECTOR('',#31525,10.);
#8555=VECTOR('',#31532,10.);
#8556=VECTOR('',#31537,9.99999999999999);
#8557=VECTOR('',#31540,10.);
#8558=VECTOR('',#31543,10.);
#8559=VECTOR('',#31560,10.);
#8560=VECTOR('',#31565,9.99999999999999);
#8561=VECTOR('',#31570,1.44337567297406);
#8562=VECTOR('',#31573,10.);
#8563=VECTOR('',#31576,10.);
#8564=VECTOR('',#31585,1.87799999999999);
#8565=VECTOR('',#31590,10.);
#8566=VECTOR('',#31593,10.);
#8567=VECTOR('',#31638,1.778);
#8568=VECTOR('',#31645,1.87799999999999);
#8569=VECTOR('',#31648,1.778);
#8570=VECTOR('',#31655,1.878);
#8571=VECTOR('',#31658,1.778);
#8572=VECTOR('',#31665,1.878);
#8573=VECTOR('',#31668,1.778);
#8574=VECTOR('',#31675,1.878);
#8575=VECTOR('',#31678,1.778);
#8576=VECTOR('',#31685,1.87799999999999);
#8577=VECTOR('',#31688,1.778);
#8578=VECTOR('',#31695,1.878);
#8579=VECTOR('',#31698,1.778);
#8580=VECTOR('',#31705,1.878);
#8581=VECTOR('',#31708,1.778);
#8582=VECTOR('',#31715,1.878);
#8583=VECTOR('',#31718,1.778);
#8584=VECTOR('',#31725,1.878);
#8585=VECTOR('',#31728,1.778);
#8586=VECTOR('',#31735,1.87799999999999);
#8587=VECTOR('',#31738,1.778);
#8588=VECTOR('',#31745,1.878);
#8589=VECTOR('',#31748,1.778);
#8590=VECTOR('',#31755,1.878);
#8591=VECTOR('',#31758,1.778);
#8592=VECTOR('',#31765,1.878);
#8593=VECTOR('',#31768,1.778);
#8594=VECTOR('',#31775,1.878);
#8595=VECTOR('',#31778,1.778);
#8596=VECTOR('',#31785,1.878);
#8597=VECTOR('',#31788,1.778);
#8598=VECTOR('',#31795,1.878);
#8599=VECTOR('',#31798,1.778);
#8600=VECTOR('',#31805,1.878);
#8601=VECTOR('',#31808,1.778);
#8602=VECTOR('',#31815,1.878);
#8603=VECTOR('',#31818,1.778);
#8604=VECTOR('',#31825,1.878);
#8605=VECTOR('',#31828,1.778);
#8606=VECTOR('',#31835,1.87799999999999);
#8607=VECTOR('',#31838,1.778);
#8608=VECTOR('',#31843,10.);
#8609=VECTOR('',#31844,10.);
#8610=VECTOR('',#31845,10.);
#8611=VECTOR('',#31848,9.99999999999999);
#8612=VECTOR('',#31853,10.);
#8613=VECTOR('',#31854,10.);
#8614=VECTOR('',#31861,10.);
#8615=VECTOR('',#31864,10.);
#8616=VECTOR('',#31867,10.);
#8617=VECTOR('',#31868,10.);
#8618=VECTOR('',#31871,10.);
#8619=VECTOR('',#31872,10.);
#8620=VECTOR('',#31873,10.);
#8621=VECTOR('',#31878,9.99999999999999);
#8622=VECTOR('',#31883,10.);
#8623=VECTOR('',#31884,10.);
#8624=VECTOR('',#31885,10.);
#8625=VECTOR('',#31892,10.);
#8626=VECTOR('',#31901,10.);
#8627=VECTOR('',#31902,10.);
#8628=VECTOR('',#31903,10.);
#8629=VECTOR('',#31904,10.);
#8630=VECTOR('',#31907,10.);
#8631=VECTOR('',#31914,10.);
#8632=VECTOR('',#31915,10.);
#8633=VECTOR('',#31916,10.);
#8634=VECTOR('',#31919,10.);
#8635=VECTOR('',#31926,10.);
#8636=VECTOR('',#31927,10.);
#8637=VECTOR('',#31928,10.);
#8638=VECTOR('',#31931,10.);
#8639=VECTOR('',#31932,10.);
#8640=VECTOR('',#31933,10.);
#8641=VECTOR('',#31936,10.);
#8642=VECTOR('',#31941,10.);
#8643=VECTOR('',#31942,10.);
#8644=VECTOR('',#31945,10.);
#8645=VECTOR('',#31950,10.);
#8646=VECTOR('',#31951,10.);
#8647=VECTOR('',#31954,10.);
#8648=VECTOR('',#31955,10.);
#8649=VECTOR('',#31956,10.);
#8650=VECTOR('',#31959,10.);
#8651=VECTOR('',#31964,10.);
#8652=VECTOR('',#31965,10.);
#8653=VECTOR('',#31968,10.);
#8654=VECTOR('',#31973,10.);
#8655=VECTOR('',#31974,10.);
#8656=VECTOR('',#31979,1.778);
#8657=VECTOR('',#31986,1.778);
#8658=VECTOR('',#31993,1.778);
#8659=VECTOR('',#32000,1.778);
#8660=VECTOR('',#32007,1.778);
#8661=VECTOR('',#32014,1.778);
#8662=VECTOR('',#32021,1.778);
#8663=VECTOR('',#32028,1.778);
#8664=VECTOR('',#32035,1.778);
#8665=VECTOR('',#32042,1.778);
#8666=VECTOR('',#32047,10.);
#8667=VECTOR('',#32048,10.);
#8668=VECTOR('',#32049,10.);
#8669=VECTOR('',#32052,10.);
#8670=VECTOR('',#32053,10.);
#8671=VECTOR('',#32054,10.);
#8672=VECTOR('',#32057,10.);
#8673=VECTOR('',#32058,10.);
#8674=VECTOR('',#32059,10.);
#8675=VECTOR('',#32062,10.);
#8676=VECTOR('',#32063,10.);
#8677=VECTOR('',#32064,10.);
#8678=VECTOR('',#32067,10.);
#8679=VECTOR('',#32068,10.);
#8680=VECTOR('',#32069,10.);
#8681=VECTOR('',#32072,10.);
#8682=VECTOR('',#32073,10.);
#8683=VECTOR('',#32074,10.);
#8684=VECTOR('',#32077,10.);
#8685=VECTOR('',#32078,10.);
#8686=VECTOR('',#32079,10.);
#8687=VECTOR('',#32082,10.);
#8688=VECTOR('',#32083,10.);
#8689=VECTOR('',#32084,10.);
#8690=VECTOR('',#32087,10.);
#8691=VECTOR('',#32088,10.);
#8692=VECTOR('',#32089,10.);
#8693=VECTOR('',#32092,10.);
#8694=VECTOR('',#32093,10.);
#8695=VECTOR('',#32094,10.);
#8696=VECTOR('',#32097,10.);
#8697=VECTOR('',#32098,10.);
#8698=VECTOR('',#32099,10.);
#8699=VECTOR('',#32102,10.);
#8700=VECTOR('',#32103,10.);
#8701=VECTOR('',#32104,10.);
#8702=VECTOR('',#32107,10.);
#8703=VECTOR('',#32108,10.);
#8704=VECTOR('',#32109,10.);
#8705=VECTOR('',#32112,10.);
#8706=VECTOR('',#32113,10.);
#8707=VECTOR('',#32114,10.);
#8708=VECTOR('',#32117,10.);
#8709=VECTOR('',#32118,10.);
#8710=VECTOR('',#32119,10.);
#8711=VECTOR('',#32122,10.);
#8712=VECTOR('',#32123,10.);
#8713=VECTOR('',#32124,10.);
#8714=VECTOR('',#32127,10.);
#8715=VECTOR('',#32128,10.);
#8716=VECTOR('',#32129,10.);
#8717=VECTOR('',#32132,10.);
#8718=VECTOR('',#32133,10.);
#8719=VECTOR('',#32134,10.);
#8720=VECTOR('',#32137,10.);
#8721=VECTOR('',#32138,10.);
#8722=VECTOR('',#32139,10.);
#8723=VECTOR('',#32142,10.);
#8724=VECTOR('',#32143,10.);
#8725=VECTOR('',#32144,10.);
#8726=VECTOR('',#32147,10.);
#8727=VECTOR('',#32148,10.);
#8728=VECTOR('',#32149,10.);
#8729=VECTOR('',#32152,10.);
#8730=VECTOR('',#32153,10.);
#8731=VECTOR('',#32154,10.);
#8732=VECTOR('',#32157,10.);
#8733=VECTOR('',#32158,10.);
#8734=VECTOR('',#32159,10.);
#8735=VECTOR('',#32162,10.);
#8736=VECTOR('',#32163,10.);
#8737=VECTOR('',#32164,10.);
#8738=VECTOR('',#32167,10.);
#8739=VECTOR('',#32168,10.);
#8740=VECTOR('',#32169,10.);
#8741=VECTOR('',#32172,10.);
#8742=VECTOR('',#32173,10.);
#8743=VECTOR('',#32174,10.);
#8744=VECTOR('',#32177,10.);
#8745=VECTOR('',#32178,10.);
#8746=VECTOR('',#32179,10.);
#8747=VECTOR('',#32182,10.);
#8748=VECTOR('',#32183,10.);
#8749=VECTOR('',#32184,10.);
#8750=VECTOR('',#32187,10.);
#8751=VECTOR('',#32188,10.);
#8752=VECTOR('',#32189,10.);
#8753=VECTOR('',#32192,10.);
#8754=VECTOR('',#32193,10.);
#8755=VECTOR('',#32194,10.);
#8756=VECTOR('',#32197,10.);
#8757=VECTOR('',#32198,10.);
#8758=VECTOR('',#32199,10.);
#8759=VECTOR('',#32202,10.);
#8760=VECTOR('',#32203,10.);
#8761=VECTOR('',#32204,10.);
#8762=VECTOR('',#32207,10.);
#8763=VECTOR('',#32208,10.);
#8764=VECTOR('',#32209,10.);
#8765=VECTOR('',#32212,10.);
#8766=VECTOR('',#32213,10.);
#8767=VECTOR('',#32214,10.);
#8768=VECTOR('',#32217,10.);
#8769=VECTOR('',#32218,10.);
#8770=VECTOR('',#32219,10.);
#8771=VECTOR('',#32222,10.);
#8772=VECTOR('',#32223,10.);
#8773=VECTOR('',#32224,10.);
#8774=VECTOR('',#32227,9.99999999999999);
#8775=VECTOR('',#32228,9.99999999999999);
#8776=VECTOR('',#32229,10.);
#8777=VECTOR('',#32232,10.);
#8778=VECTOR('',#32233,10.);
#8779=VECTOR('',#32234,10.);
#8780=VECTOR('',#32237,9.99999999999999);
#8781=VECTOR('',#32238,9.99999999999999);
#8782=VECTOR('',#32239,10.);
#8783=VECTOR('',#32242,10.);
#8784=VECTOR('',#32243,10.);
#8785=VECTOR('',#32244,10.);
#8786=VECTOR('',#32247,9.99999999999999);
#8787=VECTOR('',#32248,9.99999999999999);
#8788=VECTOR('',#32249,10.);
#8789=VECTOR('',#32252,10.);
#8790=VECTOR('',#32253,10.);
#8791=VECTOR('',#32254,10.);
#8792=VECTOR('',#32257,10.);
#8793=VECTOR('',#32258,10.);
#8794=VECTOR('',#32259,10.);
#8795=VECTOR('',#32262,10.);
#8796=VECTOR('',#32263,10.);
#8797=VECTOR('',#32264,10.);
#8798=VECTOR('',#32267,10.);
#8799=VECTOR('',#32268,10.);
#8800=VECTOR('',#32269,10.);
#8801=VECTOR('',#32272,10.);
#8802=VECTOR('',#32273,10.);
#8803=VECTOR('',#32274,10.);
#8804=VECTOR('',#32277,10.);
#8805=VECTOR('',#32278,10.);
#8806=VECTOR('',#32279,10.);
#8807=VECTOR('',#32282,10.);
#8808=VECTOR('',#32283,10.);
#8809=VECTOR('',#32284,10.);
#8810=VECTOR('',#32287,10.);
#8811=VECTOR('',#32288,10.);
#8812=VECTOR('',#32289,10.);
#8813=VECTOR('',#32292,10.);
#8814=VECTOR('',#32293,10.);
#8815=VECTOR('',#32294,10.);
#8816=VECTOR('',#32297,10.);
#8817=VECTOR('',#32298,10.);
#8818=VECTOR('',#32299,10.);
#8819=VECTOR('',#32302,10.);
#8820=VECTOR('',#32303,10.);
#8821=VECTOR('',#32304,10.);
#8822=VECTOR('',#32307,10.);
#8823=VECTOR('',#32308,10.);
#8824=VECTOR('',#32309,10.);
#8825=VECTOR('',#32312,10.);
#8826=VECTOR('',#32313,10.);
#8827=VECTOR('',#32314,10.);
#8828=VECTOR('',#32317,9.99999999999999);
#8829=VECTOR('',#32318,9.99999999999999);
#8830=VECTOR('',#32319,10.);
#8831=VECTOR('',#32322,10.);
#8832=VECTOR('',#32323,10.);
#8833=VECTOR('',#32324,10.);
#8834=VECTOR('',#32327,9.99999999999999);
#8835=VECTOR('',#32328,9.99999999999999);
#8836=VECTOR('',#32329,10.);
#8837=VECTOR('',#32332,10.);
#8838=VECTOR('',#32333,10.);
#8839=VECTOR('',#32334,10.);
#8840=VECTOR('',#32337,9.99999999999999);
#8841=VECTOR('',#32338,9.99999999999999);
#8842=VECTOR('',#32339,10.);
#8843=VECTOR('',#32342,10.);
#8844=VECTOR('',#32343,10.);
#8845=VECTOR('',#32344,10.);
#8846=VECTOR('',#32347,9.99999999999999);
#8847=VECTOR('',#32348,9.99999999999999);
#8848=VECTOR('',#32349,10.);
#8849=VECTOR('',#32352,10.);
#8850=VECTOR('',#32353,10.);
#8851=VECTOR('',#32354,10.);
#8852=VECTOR('',#32357,9.99999999999999);
#8853=VECTOR('',#32358,9.99999999999999);
#8854=VECTOR('',#32359,10.);
#8855=VECTOR('',#32362,10.);
#8856=VECTOR('',#32363,10.);
#8857=VECTOR('',#32364,10.);
#8858=VECTOR('',#32367,9.99999999999999);
#8859=VECTOR('',#32368,9.99999999999999);
#8860=VECTOR('',#32369,10.);
#8861=VECTOR('',#32372,10.);
#8862=VECTOR('',#32373,10.);
#8863=VECTOR('',#32374,10.);
#8864=VECTOR('',#32377,10.);
#8865=VECTOR('',#32378,10.);
#8866=VECTOR('',#32379,10.);
#8867=VECTOR('',#32382,10.);
#8868=VECTOR('',#32383,10.);
#8869=VECTOR('',#32384,10.);
#8870=VECTOR('',#32387,10.);
#8871=VECTOR('',#32388,10.);
#8872=VECTOR('',#32389,10.);
#8873=VECTOR('',#32392,10.);
#8874=VECTOR('',#32393,10.);
#8875=VECTOR('',#32394,10.);
#8876=VECTOR('',#32397,10.);
#8877=VECTOR('',#32398,10.);
#8878=VECTOR('',#32399,10.);
#8879=VECTOR('',#32402,10.);
#8880=VECTOR('',#32403,10.);
#8881=VECTOR('',#32404,10.);
#8882=VECTOR('',#32407,10.);
#8883=VECTOR('',#32408,10.);
#8884=VECTOR('',#32409,10.);
#8885=VECTOR('',#32412,10.);
#8886=VECTOR('',#32413,10.);
#8887=VECTOR('',#32414,10.);
#8888=VECTOR('',#32417,10.);
#8889=VECTOR('',#32418,10.);
#8890=VECTOR('',#32419,10.);
#8891=VECTOR('',#32422,10.);
#8892=VECTOR('',#32423,10.);
#8893=VECTOR('',#32424,10.);
#8894=VECTOR('',#32427,10.);
#8895=VECTOR('',#32428,10.);
#8896=VECTOR('',#32429,10.);
#8897=VECTOR('',#32432,10.);
#8898=VECTOR('',#32433,10.);
#8899=VECTOR('',#32434,10.);
#8900=VECTOR('',#32437,10.);
#8901=VECTOR('',#32438,10.);
#8902=VECTOR('',#32439,10.);
#8903=VECTOR('',#32442,10.);
#8904=VECTOR('',#32443,10.);
#8905=VECTOR('',#32444,10.);
#8906=VECTOR('',#32447,10.);
#8907=VECTOR('',#32448,10.);
#8908=VECTOR('',#32449,10.);
#8909=VECTOR('',#32452,10.);
#8910=VECTOR('',#32453,10.);
#8911=VECTOR('',#32454,10.);
#8912=VECTOR('',#32457,10.);
#8913=VECTOR('',#32458,10.);
#8914=VECTOR('',#32459,10.);
#8915=VECTOR('',#32462,10.);
#8916=VECTOR('',#32463,10.);
#8917=VECTOR('',#32464,10.);
#8918=VECTOR('',#32467,10.);
#8919=VECTOR('',#32468,10.);
#8920=VECTOR('',#32469,10.);
#8921=VECTOR('',#32472,10.);
#8922=VECTOR('',#32473,10.);
#8923=VECTOR('',#32474,10.);
#8924=VECTOR('',#32477,10.);
#8925=VECTOR('',#32478,10.);
#8926=VECTOR('',#32479,10.);
#8927=VECTOR('',#32482,10.);
#8928=VECTOR('',#32483,10.);
#8929=VECTOR('',#32484,10.);
#8930=VECTOR('',#32487,10.);
#8931=VECTOR('',#32488,10.);
#8932=VECTOR('',#32489,10.);
#8933=VECTOR('',#32492,10.);
#8934=VECTOR('',#32493,10.);
#8935=VECTOR('',#32494,10.);
#8936=VECTOR('',#32497,10.);
#8937=VECTOR('',#32498,10.);
#8938=VECTOR('',#32499,10.);
#8939=VECTOR('',#32502,10.);
#8940=VECTOR('',#32503,10.);
#8941=VECTOR('',#32504,10.);
#8942=VECTOR('',#32507,10.);
#8943=VECTOR('',#32508,10.);
#8944=VECTOR('',#32509,10.);
#8945=VECTOR('',#32512,10.);
#8946=VECTOR('',#32513,10.);
#8947=VECTOR('',#32514,10.);
#8948=VECTOR('',#32517,10.);
#8949=VECTOR('',#32518,10.);
#8950=VECTOR('',#32519,10.);
#8951=VECTOR('',#32522,10.);
#8952=VECTOR('',#32523,10.);
#8953=VECTOR('',#32524,10.);
#8954=VECTOR('',#32527,10.);
#8955=VECTOR('',#32528,10.);
#8956=VECTOR('',#32529,10.);
#8957=VECTOR('',#32532,10.);
#8958=VECTOR('',#32533,10.);
#8959=VECTOR('',#32534,10.);
#8960=VECTOR('',#32537,10.);
#8961=VECTOR('',#32538,10.);
#8962=VECTOR('',#32539,10.);
#8963=VECTOR('',#32542,10.);
#8964=VECTOR('',#32543,10.);
#8965=VECTOR('',#32544,10.);
#8966=VECTOR('',#32547,10.);
#8967=VECTOR('',#32548,10.);
#8968=VECTOR('',#32549,10.);
#8969=VECTOR('',#32552,10.);
#8970=VECTOR('',#32553,10.);
#8971=VECTOR('',#32554,10.);
#8972=VECTOR('',#32557,10.);
#8973=VECTOR('',#32558,10.);
#8974=VECTOR('',#32559,10.);
#8975=VECTOR('',#32562,10.);
#8976=VECTOR('',#32563,10.);
#8977=VECTOR('',#32564,10.);
#8978=VECTOR('',#32567,10.);
#8979=VECTOR('',#32568,10.);
#8980=VECTOR('',#32569,10.);
#8981=VECTOR('',#32572,10.);
#8982=VECTOR('',#32573,10.);
#8983=VECTOR('',#32574,10.);
#8984=VECTOR('',#32577,10.);
#8985=VECTOR('',#32578,10.);
#8986=VECTOR('',#32579,10.);
#8987=VECTOR('',#32582,10.);
#8988=VECTOR('',#32583,10.);
#8989=VECTOR('',#32584,10.);
#8990=VECTOR('',#32587,10.);
#8991=VECTOR('',#32588,10.);
#8992=VECTOR('',#32589,10.);
#8993=VECTOR('',#32592,10.);
#8994=VECTOR('',#32593,10.);
#8995=VECTOR('',#32594,10.);
#8996=VECTOR('',#32597,10.);
#8997=VECTOR('',#32598,10.);
#8998=VECTOR('',#32599,10.);
#8999=VECTOR('',#32602,10.);
#9000=VECTOR('',#32603,10.);
#9001=VECTOR('',#32604,10.);
#9002=VECTOR('',#32607,10.);
#9003=VECTOR('',#32608,10.);
#9004=VECTOR('',#32609,10.);
#9005=VECTOR('',#32612,10.);
#9006=VECTOR('',#32613,10.);
#9007=VECTOR('',#32614,10.);
#9008=VECTOR('',#32617,10.);
#9009=VECTOR('',#32618,10.);
#9010=VECTOR('',#32619,10.);
#9011=VECTOR('',#32622,10.);
#9012=VECTOR('',#32623,10.);
#9013=VECTOR('',#32624,10.);
#9014=VECTOR('',#32627,10.);
#9015=VECTOR('',#32628,10.);
#9016=VECTOR('',#32629,10.);
#9017=VECTOR('',#32632,10.);
#9018=VECTOR('',#32633,10.);
#9019=VECTOR('',#32634,10.);
#9020=VECTOR('',#32637,10.);
#9021=VECTOR('',#32638,10.);
#9022=VECTOR('',#32639,10.);
#9023=VECTOR('',#32642,10.);
#9024=VECTOR('',#32643,10.);
#9025=VECTOR('',#32644,10.);
#9026=VECTOR('',#32647,10.);
#9027=VECTOR('',#32648,10.);
#9028=VECTOR('',#32649,10.);
#9029=VECTOR('',#32652,10.);
#9030=VECTOR('',#32653,10.);
#9031=VECTOR('',#32654,10.);
#9032=VECTOR('',#32657,10.);
#9033=VECTOR('',#32658,10.);
#9034=VECTOR('',#32659,10.);
#9035=VECTOR('',#32662,10.);
#9036=VECTOR('',#32663,10.);
#9037=VECTOR('',#32664,10.);
#9038=VECTOR('',#32667,10.);
#9039=VECTOR('',#32668,10.);
#9040=VECTOR('',#32669,10.);
#9041=VECTOR('',#32672,10.);
#9042=VECTOR('',#32673,10.);
#9043=VECTOR('',#32674,10.);
#9044=VECTOR('',#32677,10.);
#9045=VECTOR('',#32678,10.);
#9046=VECTOR('',#32679,10.);
#9047=VECTOR('',#32682,10.);
#9048=VECTOR('',#32683,10.);
#9049=VECTOR('',#32684,10.);
#9050=VECTOR('',#32687,10.);
#9051=VECTOR('',#32688,10.);
#9052=VECTOR('',#32689,10.);
#9053=VECTOR('',#32692,10.);
#9054=VECTOR('',#32693,10.);
#9055=VECTOR('',#32694,10.);
#9056=VECTOR('',#32697,10.);
#9057=VECTOR('',#32698,10.);
#9058=VECTOR('',#32699,10.);
#9059=VECTOR('',#32702,10.);
#9060=VECTOR('',#32703,10.);
#9061=VECTOR('',#32704,10.);
#9062=VECTOR('',#32707,10.);
#9063=VECTOR('',#32708,10.);
#9064=VECTOR('',#32709,10.);
#9065=VECTOR('',#32712,10.);
#9066=VECTOR('',#32713,10.);
#9067=VECTOR('',#32714,10.);
#9068=VECTOR('',#32717,10.);
#9069=VECTOR('',#32718,10.);
#9070=VECTOR('',#32719,10.);
#9071=VECTOR('',#32722,10.);
#9072=VECTOR('',#32723,10.);
#9073=VECTOR('',#32724,10.);
#9074=VECTOR('',#32727,10.);
#9075=VECTOR('',#32728,10.);
#9076=VECTOR('',#32729,10.);
#9077=VECTOR('',#32732,10.);
#9078=VECTOR('',#32733,10.);
#9079=VECTOR('',#32734,10.);
#9080=VECTOR('',#32737,10.);
#9081=VECTOR('',#32738,10.);
#9082=VECTOR('',#32739,10.);
#9083=VECTOR('',#32742,10.);
#9084=VECTOR('',#32743,10.);
#9085=VECTOR('',#32744,10.);
#9086=VECTOR('',#32747,10.);
#9087=VECTOR('',#32748,10.);
#9088=VECTOR('',#32749,10.);
#9089=VECTOR('',#32752,10.);
#9090=VECTOR('',#32753,10.);
#9091=VECTOR('',#32754,10.);
#9092=VECTOR('',#32757,10.);
#9093=VECTOR('',#32758,10.);
#9094=VECTOR('',#32759,10.);
#9095=VECTOR('',#32762,10.);
#9096=VECTOR('',#32763,10.);
#9097=VECTOR('',#32764,10.);
#9098=VECTOR('',#32767,10.);
#9099=VECTOR('',#32768,10.);
#9100=VECTOR('',#32769,10.);
#9101=VECTOR('',#32772,10.);
#9102=VECTOR('',#32773,10.);
#9103=VECTOR('',#32774,10.);
#9104=VECTOR('',#32777,10.);
#9105=VECTOR('',#32778,10.);
#9106=VECTOR('',#32779,10.);
#9107=VECTOR('',#32782,10.);
#9108=VECTOR('',#32783,10.);
#9109=VECTOR('',#32784,10.);
#9110=VECTOR('',#32787,10.);
#9111=VECTOR('',#32788,10.);
#9112=VECTOR('',#32789,10.);
#9113=VECTOR('',#32792,10.);
#9114=VECTOR('',#32793,10.);
#9115=VECTOR('',#32794,10.);
#9116=VECTOR('',#32797,10.);
#9117=VECTOR('',#32798,10.);
#9118=VECTOR('',#32799,10.);
#9119=VECTOR('',#32802,10.);
#9120=VECTOR('',#32803,10.);
#9121=VECTOR('',#32804,10.);
#9122=VECTOR('',#32807,10.);
#9123=VECTOR('',#32808,10.);
#9124=VECTOR('',#32809,10.);
#9125=VECTOR('',#32812,10.);
#9126=VECTOR('',#32813,10.);
#9127=VECTOR('',#32814,10.);
#9128=VECTOR('',#32817,10.);
#9129=VECTOR('',#32818,10.);
#9130=VECTOR('',#32819,10.);
#9131=VECTOR('',#32822,10.);
#9132=VECTOR('',#32823,10.);
#9133=VECTOR('',#32824,10.);
#9134=VECTOR('',#32827,10.);
#9135=VECTOR('',#32828,10.);
#9136=VECTOR('',#32829,10.);
#9137=VECTOR('',#32832,10.);
#9138=VECTOR('',#32833,10.);
#9139=VECTOR('',#32834,10.);
#9140=VECTOR('',#32837,10.);
#9141=VECTOR('',#32838,10.);
#9142=VECTOR('',#32839,10.);
#9143=VECTOR('',#32842,10.);
#9144=VECTOR('',#32843,10.);
#9145=VECTOR('',#32844,10.);
#9146=VECTOR('',#32847,10.);
#9147=VECTOR('',#32848,10.);
#9148=VECTOR('',#32849,10.);
#9149=VECTOR('',#32852,10.);
#9150=VECTOR('',#32853,10.);
#9151=VECTOR('',#32854,10.);
#9152=VECTOR('',#32857,10.);
#9153=VECTOR('',#32858,10.);
#9154=VECTOR('',#32859,10.);
#9155=VECTOR('',#32862,10.);
#9156=VECTOR('',#32863,10.);
#9157=VECTOR('',#32864,10.);
#9158=VECTOR('',#32867,10.);
#9159=VECTOR('',#32868,10.);
#9160=VECTOR('',#32869,10.);
#9161=VECTOR('',#32872,10.);
#9162=VECTOR('',#32873,10.);
#9163=VECTOR('',#32874,10.);
#9164=VECTOR('',#32877,10.);
#9165=VECTOR('',#32878,10.);
#9166=VECTOR('',#32879,10.);
#9167=VECTOR('',#32882,10.);
#9168=VECTOR('',#32883,10.);
#9169=VECTOR('',#32884,10.);
#9170=VECTOR('',#32887,10.);
#9171=VECTOR('',#32888,10.);
#9172=VECTOR('',#32889,10.);
#9173=VECTOR('',#32892,10.);
#9174=VECTOR('',#32893,10.);
#9175=VECTOR('',#32894,10.);
#9176=VECTOR('',#32897,10.);
#9177=VECTOR('',#32898,10.);
#9178=VECTOR('',#32899,10.);
#9179=VECTOR('',#32902,10.);
#9180=VECTOR('',#32903,10.);
#9181=VECTOR('',#32904,10.);
#9182=VECTOR('',#32907,10.);
#9183=VECTOR('',#32908,10.);
#9184=VECTOR('',#32909,10.);
#9185=VECTOR('',#32912,10.);
#9186=VECTOR('',#32913,10.);
#9187=VECTOR('',#32914,10.);
#9188=VECTOR('',#32917,10.);
#9189=VECTOR('',#32918,10.);
#9190=VECTOR('',#32919,10.);
#9191=VECTOR('',#32922,10.);
#9192=VECTOR('',#32923,10.);
#9193=VECTOR('',#32924,10.);
#9194=VECTOR('',#32927,10.);
#9195=VECTOR('',#32928,10.);
#9196=VECTOR('',#32929,10.);
#9197=VECTOR('',#32932,10.);
#9198=VECTOR('',#32933,10.);
#9199=VECTOR('',#32934,10.);
#9200=VECTOR('',#32937,10.);
#9201=VECTOR('',#32938,10.);
#9202=VECTOR('',#32939,10.);
#9203=VECTOR('',#32942,10.);
#9204=VECTOR('',#32943,10.);
#9205=VECTOR('',#32944,10.);
#9206=VECTOR('',#32947,10.);
#9207=VECTOR('',#32948,10.);
#9208=VECTOR('',#32949,10.);
#9209=VECTOR('',#32952,10.);
#9210=VECTOR('',#32953,10.);
#9211=VECTOR('',#32954,10.);
#9212=VECTOR('',#32957,10.);
#9213=VECTOR('',#32958,10.);
#9214=VECTOR('',#32959,10.);
#9215=VECTOR('',#32962,10.);
#9216=VECTOR('',#32963,10.);
#9217=VECTOR('',#32964,10.);
#9218=VECTOR('',#32967,10.);
#9219=VECTOR('',#32968,10.);
#9220=VECTOR('',#32969,10.);
#9221=VECTOR('',#32972,10.);
#9222=VECTOR('',#32973,10.);
#9223=VECTOR('',#32974,10.);
#9224=VECTOR('',#32977,10.);
#9225=VECTOR('',#32978,10.);
#9226=VECTOR('',#32979,10.);
#9227=VECTOR('',#32982,10.);
#9228=VECTOR('',#32983,10.);
#9229=VECTOR('',#32984,10.);
#9230=VECTOR('',#32987,10.);
#9231=VECTOR('',#32988,10.);
#9232=VECTOR('',#32989,10.);
#9233=VECTOR('',#32992,10.);
#9234=VECTOR('',#32993,10.);
#9235=VECTOR('',#32994,10.);
#9236=VECTOR('',#32997,10.);
#9237=VECTOR('',#32998,10.);
#9238=VECTOR('',#32999,10.);
#9239=VECTOR('',#33002,10.);
#9240=VECTOR('',#33003,10.);
#9241=VECTOR('',#33004,10.);
#9242=VECTOR('',#33007,10.);
#9243=VECTOR('',#33008,10.);
#9244=VECTOR('',#33009,10.);
#9245=VECTOR('',#33012,10.);
#9246=VECTOR('',#33013,10.);
#9247=VECTOR('',#33014,10.);
#9248=VECTOR('',#33017,10.);
#9249=VECTOR('',#33018,10.);
#9250=VECTOR('',#33019,10.);
#9251=VECTOR('',#33022,10.);
#9252=VECTOR('',#33023,10.);
#9253=VECTOR('',#33024,10.);
#9254=VECTOR('',#33027,10.);
#9255=VECTOR('',#33028,10.);
#9256=VECTOR('',#33029,10.);
#9257=VECTOR('',#33032,10.);
#9258=VECTOR('',#33033,10.);
#9259=VECTOR('',#33034,10.);
#9260=VECTOR('',#33037,10.);
#9261=VECTOR('',#33038,10.);
#9262=VECTOR('',#33039,10.);
#9263=VECTOR('',#33042,10.);
#9264=VECTOR('',#33043,10.);
#9265=VECTOR('',#33044,10.);
#9266=VECTOR('',#33047,10.);
#9267=VECTOR('',#33048,10.);
#9268=VECTOR('',#33049,10.);
#9269=VECTOR('',#33052,10.);
#9270=VECTOR('',#33053,10.);
#9271=VECTOR('',#33054,10.);
#9272=VECTOR('',#33057,10.);
#9273=VECTOR('',#33058,10.);
#9274=VECTOR('',#33059,10.);
#9275=VECTOR('',#33062,10.);
#9276=VECTOR('',#33063,10.);
#9277=VECTOR('',#33064,10.);
#9278=VECTOR('',#33067,10.);
#9279=VECTOR('',#33068,10.);
#9280=VECTOR('',#33069,10.);
#9281=VECTOR('',#33072,10.);
#9282=VECTOR('',#33073,10.);
#9283=VECTOR('',#33074,10.);
#9284=VECTOR('',#33077,10.);
#9285=VECTOR('',#33078,10.);
#9286=VECTOR('',#33079,10.);
#9287=VECTOR('',#33082,10.);
#9288=VECTOR('',#33083,10.);
#9289=VECTOR('',#33084,10.);
#9290=VECTOR('',#33087,10.);
#9291=VECTOR('',#33088,10.);
#9292=VECTOR('',#33089,10.);
#9293=VECTOR('',#33092,10.);
#9294=VECTOR('',#33093,10.);
#9295=VECTOR('',#33094,10.);
#9296=VECTOR('',#33097,10.);
#9297=VECTOR('',#33098,10.);
#9298=VECTOR('',#33099,10.);
#9299=VECTOR('',#33102,10.);
#9300=VECTOR('',#33103,10.);
#9301=VECTOR('',#33104,10.);
#9302=VECTOR('',#33107,10.);
#9303=VECTOR('',#33108,10.);
#9304=VECTOR('',#33109,10.);
#9305=VECTOR('',#33112,10.);
#9306=VECTOR('',#33113,10.);
#9307=VECTOR('',#33114,10.);
#9308=VECTOR('',#33117,9.99999999999999);
#9309=VECTOR('',#33118,9.99999999999999);
#9310=VECTOR('',#33119,10.);
#9311=VECTOR('',#33122,10.);
#9312=VECTOR('',#33123,10.);
#9313=VECTOR('',#33124,10.);
#9314=VECTOR('',#33127,9.99999999999999);
#9315=VECTOR('',#33128,9.99999999999999);
#9316=VECTOR('',#33129,10.);
#9317=VECTOR('',#33132,10.);
#9318=VECTOR('',#33133,10.);
#9319=VECTOR('',#33134,10.);
#9320=VECTOR('',#33137,9.99999999999999);
#9321=VECTOR('',#33138,9.99999999999999);
#9322=VECTOR('',#33139,10.);
#9323=VECTOR('',#33142,10.);
#9324=VECTOR('',#33143,10.);
#9325=VECTOR('',#33144,10.);
#9326=VECTOR('',#33147,9.99999999999999);
#9327=VECTOR('',#33148,9.99999999999999);
#9328=VECTOR('',#33149,10.);
#9329=VECTOR('',#33152,10.);
#9330=VECTOR('',#33153,10.);
#9331=VECTOR('',#33154,10.);
#9332=VECTOR('',#33157,9.99999999999999);
#9333=VECTOR('',#33158,9.99999999999999);
#9334=VECTOR('',#33159,10.);
#9335=VECTOR('',#33162,10.);
#9336=VECTOR('',#33163,10.);
#9337=VECTOR('',#33164,10.);
#9338=VECTOR('',#33167,9.99999999999999);
#9339=VECTOR('',#33168,9.99999999999999);
#9340=VECTOR('',#33169,10.);
#9341=VECTOR('',#33172,10.);
#9342=VECTOR('',#33173,10.);
#9343=VECTOR('',#33174,10.);
#9344=VECTOR('',#33177,10.);
#9345=VECTOR('',#33178,10.);
#9346=VECTOR('',#33179,10.);
#9347=VECTOR('',#33182,10.);
#9348=VECTOR('',#33183,10.);
#9349=VECTOR('',#33184,10.);
#9350=VECTOR('',#33187,10.);
#9351=VECTOR('',#33188,10.);
#9352=VECTOR('',#33189,10.);
#9353=VECTOR('',#33192,10.);
#9354=VECTOR('',#33193,10.);
#9355=VECTOR('',#33194,10.);
#9356=VECTOR('',#33197,10.);
#9357=VECTOR('',#33198,10.);
#9358=VECTOR('',#33199,10.);
#9359=VECTOR('',#33202,10.);
#9360=VECTOR('',#33203,10.);
#9361=VECTOR('',#33204,10.);
#9362=VECTOR('',#33207,10.);
#9363=VECTOR('',#33208,10.);
#9364=VECTOR('',#33209,10.);
#9365=VECTOR('',#33212,10.);
#9366=VECTOR('',#33213,10.);
#9367=VECTOR('',#33214,10.);
#9368=VECTOR('',#33217,10.);
#9369=VECTOR('',#33218,10.);
#9370=VECTOR('',#33219,10.);
#9371=VECTOR('',#33222,10.);
#9372=VECTOR('',#33223,10.);
#9373=VECTOR('',#33224,10.);
#9374=VECTOR('',#33227,10.);
#9375=VECTOR('',#33228,10.);
#9376=VECTOR('',#33229,10.);
#9377=VECTOR('',#33232,10.);
#9378=VECTOR('',#33233,10.);
#9379=VECTOR('',#33234,10.);
#9380=VECTOR('',#33237,9.99999999999999);
#9381=VECTOR('',#33238,9.99999999999999);
#9382=VECTOR('',#33239,10.);
#9383=VECTOR('',#33242,10.);
#9384=VECTOR('',#33243,10.);
#9385=VECTOR('',#33244,10.);
#9386=VECTOR('',#33247,9.99999999999999);
#9387=VECTOR('',#33248,9.99999999999999);
#9388=VECTOR('',#33249,10.);
#9389=VECTOR('',#33252,10.);
#9390=VECTOR('',#33253,10.);
#9391=VECTOR('',#33254,10.);
#9392=VECTOR('',#33257,9.99999999999999);
#9393=VECTOR('',#33258,9.99999999999999);
#9394=VECTOR('',#33259,10.);
#9395=VECTOR('',#33262,10.);
#9396=VECTOR('',#33263,10.);
#9397=VECTOR('',#33264,10.);
#9398=VECTOR('',#33267,10.);
#9399=VECTOR('',#33268,10.);
#9400=VECTOR('',#33269,10.);
#9401=VECTOR('',#33272,10.);
#9402=VECTOR('',#33273,10.);
#9403=VECTOR('',#33274,10.);
#9404=VECTOR('',#33277,10.);
#9405=VECTOR('',#33278,10.);
#9406=VECTOR('',#33279,10.);
#9407=VECTOR('',#33282,10.);
#9408=VECTOR('',#33283,10.);
#9409=VECTOR('',#33284,10.);
#9410=VECTOR('',#33287,10.);
#9411=VECTOR('',#33288,10.);
#9412=VECTOR('',#33289,10.);
#9413=VECTOR('',#33292,10.);
#9414=VECTOR('',#33293,10.);
#9415=VECTOR('',#33294,10.);
#9416=VECTOR('',#33297,10.);
#9417=VECTOR('',#33298,10.);
#9418=VECTOR('',#33299,10.);
#9419=VECTOR('',#33302,10.);
#9420=VECTOR('',#33303,10.);
#9421=VECTOR('',#33304,10.);
#9422=VECTOR('',#33307,10.);
#9423=VECTOR('',#33308,10.);
#9424=VECTOR('',#33309,10.);
#9425=VECTOR('',#33312,10.);
#9426=VECTOR('',#33313,10.);
#9427=VECTOR('',#33314,10.);
#9428=VECTOR('',#33317,10.);
#9429=VECTOR('',#33318,10.);
#9430=VECTOR('',#33319,10.);
#9431=VECTOR('',#33322,10.);
#9432=VECTOR('',#33323,10.);
#9433=VECTOR('',#33324,10.);
#9434=VECTOR('',#33327,10.);
#9435=VECTOR('',#33328,10.);
#9436=VECTOR('',#33329,10.);
#9437=VECTOR('',#33332,10.);
#9438=VECTOR('',#33333,10.);
#9439=VECTOR('',#33334,10.);
#9440=VECTOR('',#33337,10.);
#9441=VECTOR('',#33338,10.);
#9442=VECTOR('',#33339,10.);
#9443=VECTOR('',#33342,10.);
#9444=VECTOR('',#33343,10.);
#9445=VECTOR('',#33344,10.);
#9446=VECTOR('',#33347,10.);
#9447=VECTOR('',#33348,10.);
#9448=VECTOR('',#33349,10.);
#9449=VECTOR('',#33352,10.);
#9450=VECTOR('',#33353,10.);
#9451=VECTOR('',#33354,10.);
#9452=VECTOR('',#33357,10.);
#9453=VECTOR('',#33358,10.);
#9454=VECTOR('',#33359,10.);
#9455=VECTOR('',#33362,10.);
#9456=VECTOR('',#33363,10.);
#9457=VECTOR('',#33364,10.);
#9458=VECTOR('',#33367,10.);
#9459=VECTOR('',#33368,10.);
#9460=VECTOR('',#33369,10.);
#9461=VECTOR('',#33372,10.);
#9462=VECTOR('',#33373,10.);
#9463=VECTOR('',#33374,10.);
#9464=VECTOR('',#33377,10.);
#9465=VECTOR('',#33378,10.);
#9466=VECTOR('',#33379,10.);
#9467=VECTOR('',#33382,10.);
#9468=VECTOR('',#33383,10.);
#9469=VECTOR('',#33384,10.);
#9470=VECTOR('',#33387,10.);
#9471=VECTOR('',#33388,10.);
#9472=VECTOR('',#33389,10.);
#9473=VECTOR('',#33392,10.);
#9474=VECTOR('',#33393,10.);
#9475=VECTOR('',#33394,10.);
#9476=VECTOR('',#33397,10.);
#9477=VECTOR('',#33398,10.);
#9478=VECTOR('',#33399,10.);
#9479=VECTOR('',#33402,10.);
#9480=VECTOR('',#33403,10.);
#9481=VECTOR('',#33404,10.);
#9482=VECTOR('',#33407,10.);
#9483=VECTOR('',#33408,10.);
#9484=VECTOR('',#33409,10.);
#9485=VECTOR('',#33412,10.);
#9486=VECTOR('',#33413,10.);
#9487=VECTOR('',#33414,10.);
#9488=VECTOR('',#33417,10.);
#9489=VECTOR('',#33418,10.);
#9490=VECTOR('',#33419,10.);
#9491=VECTOR('',#33422,10.);
#9492=VECTOR('',#33423,10.);
#9493=VECTOR('',#33424,10.);
#9494=VECTOR('',#33427,10.);
#9495=VECTOR('',#33428,10.);
#9496=VECTOR('',#33429,10.);
#9497=VECTOR('',#33432,10.);
#9498=VECTOR('',#33433,10.);
#9499=VECTOR('',#33434,10.);
#9500=VECTOR('',#33437,10.);
#9501=VECTOR('',#33438,10.);
#9502=VECTOR('',#33449,1.903);
#9503=VECTOR('',#33454,10.);
#9504=VECTOR('',#33455,10.);
#9505=VECTOR('',#33456,10.);
#9506=VECTOR('',#33457,10.);
#9507=VECTOR('',#33458,10.);
#9508=VECTOR('',#33459,10.);
#9509=VECTOR('',#33460,10.);
#9510=VECTOR('',#33461,10.);
#9511=VECTOR('',#33470,10.);
#9512=VECTOR('',#33471,10.);
#9513=VECTOR('',#33472,10.);
#9514=VECTOR('',#33473,10.);
#9515=VECTOR('',#33474,10.);
#9516=VECTOR('',#33475,10.);
#9517=VECTOR('',#33476,10.);
#9518=VECTOR('',#33477,10.);
#9519=VECTOR('',#33478,10.);
#9520=VECTOR('',#33479,10.);
#9521=VECTOR('',#33480,10.);
#9522=VECTOR('',#33481,10.);
#9523=VECTOR('',#33490,1.778);
#9524=VECTOR('',#33497,1.903);
#9525=VECTOR('',#33500,1.778);
#9526=VECTOR('',#33507,1.903);
#9527=VECTOR('',#33510,1.778);
#9528=VECTOR('',#33517,1.903);
#9529=VECTOR('',#33520,1.778);
#9530=VECTOR('',#33527,1.903);
#9531=VECTOR('',#33530,1.778);
#9532=VECTOR('',#33537,1.903);
#9533=VECTOR('',#33540,1.778);
#9534=VECTOR('',#33547,1.903);
#9535=VECTOR('',#33550,1.778);
#9536=VECTOR('',#33557,1.903);
#9537=VECTOR('',#33560,1.778);
#9538=VECTOR('',#33565,10.);
#9539=VECTOR('',#33566,10.);
#9540=VECTOR('',#33567,10.);
#9541=VECTOR('',#33570,10.);
#9542=VECTOR('',#33571,10.);
#9543=VECTOR('',#33574,10.);
#9544=VECTOR('',#33575,10.);
#9545=VECTOR('',#33578,10.);
#9546=VECTOR('',#33579,10.);
#9547=VECTOR('',#33582,10.);
#9548=VECTOR('',#33583,10.);
#9549=VECTOR('',#33586,10.);
#9550=VECTOR('',#33589,10.);
#9551=VECTOR('',#33590,10.);
#9552=VECTOR('',#33591,10.);
#9553=VECTOR('',#33594,10.);
#9554=VECTOR('',#33595,10.);
#9555=VECTOR('',#33598,10.);
#9556=VECTOR('',#33599,10.);
#9557=VECTOR('',#33602,10.);
#9558=VECTOR('',#33603,10.);
#9559=VECTOR('',#33606,10.);
#9560=VECTOR('',#33607,10.);
#9561=VECTOR('',#33610,10.);
#9562=VECTOR('',#33613,10.);
#9563=VECTOR('',#33614,10.);
#9564=VECTOR('',#33615,10.);
#9565=VECTOR('',#33618,10.);
#9566=VECTOR('',#33619,10.);
#9567=VECTOR('',#33622,10.);
#9568=VECTOR('',#33623,10.);
#9569=VECTOR('',#33626,10.);
#9570=VECTOR('',#33627,10.);
#9571=VECTOR('',#33630,10.);
#9572=VECTOR('',#33631,10.);
#9573=VECTOR('',#33634,10.);
#9574=VECTOR('',#33635,10.);
#9575=VECTOR('',#33638,10.);
#9576=VECTOR('',#33639,10.);
#9577=VECTOR('',#33642,10.);
#9578=VECTOR('',#33645,10.);
#9579=VECTOR('',#33646,10.);
#9580=VECTOR('',#33647,10.);
#9581=VECTOR('',#33650,10.);
#9582=VECTOR('',#33651,10.);
#9583=VECTOR('',#33654,10.);
#9584=VECTOR('',#33655,10.);
#9585=VECTOR('',#33658,10.);
#9586=VECTOR('',#33659,10.);
#9587=VECTOR('',#33662,10.);
#9588=VECTOR('',#33663,10.);
#9589=VECTOR('',#33666,10.);
#9590=VECTOR('',#33667,10.);
#9591=VECTOR('',#33670,10.);
#9592=VECTOR('',#33671,10.);
#9593=VECTOR('',#33674,10.);
#9594=VECTOR('',#33683,1.778);
#9595=VECTOR('',#33690,1.778);
#9596=VECTOR('',#33697,1.9525);
#9597=VECTOR('',#33702,1.8025);
#9598=VECTOR('',#33715,10.);
#9599=VECTOR('',#33716,10.);
#9600=VECTOR('',#33717,10.);
#9601=VECTOR('',#33718,10.);
#9602=VECTOR('',#33723,1.9525);
#9603=VECTOR('',#33728,1.8025);
#9604=VECTOR('',#33741,10.);
#9605=VECTOR('',#33742,10.);
#9606=VECTOR('',#33743,10.);
#9607=VECTOR('',#33744,10.);
#9608=VECTOR('',#33753,1.8025);
#9609=VECTOR('',#33766,1.8025);
#9610=VECTOR('',#33773,1.9525);
#9611=VECTOR('',#33778,10.);
#9612=VECTOR('',#33779,10.);
#9613=VECTOR('',#33780,10.);
#9614=VECTOR('',#33781,10.);
#9615=VECTOR('',#33782,10.);
#9616=VECTOR('',#33785,1.8025);
#9617=VECTOR('',#33788,1.9525);
#9618=VECTOR('',#33793,10.);
#9619=VECTOR('',#33794,10.);
#9620=VECTOR('',#33795,10.);
#9621=VECTOR('',#33796,10.);
#9622=VECTOR('',#33797,10.);
#9623=VECTOR('',#33800,0.901250000000005);
#9624=VECTOR('',#33803,10.);
#9625=VECTOR('',#33804,10.);
#9626=VECTOR('',#33807,10.);
#9627=VECTOR('',#33810,10.);
#9628=VECTOR('',#33813,10.);
#9629=VECTOR('',#33814,10.);
#9630=VECTOR('',#33815,10.);
#9631=VECTOR('',#33818,10.);
#9632=VECTOR('',#33819,10.);
#9633=VECTOR('',#33820,10.);
#9634=VECTOR('',#33823,10.);
#9635=VECTOR('',#33824,10.);
#9636=VECTOR('',#33833,1.27);
#9637=VECTOR('',#33838,1.27);
#9638=VECTOR('',#33841,1.27);
#9639=VECTOR('',#33844,1.27);
#9640=VECTOR('',#33847,1.27);
#9641=VECTOR('',#33850,1.27);
#9642=VECTOR('',#33853,1.27);
#9643=VECTOR('',#33888,1.52934);
#9644=VECTOR('',#33895,10.);
#9645=VECTOR('',#33896,9.99999999999999);
#9646=VECTOR('',#33897,10.);
#9647=VECTOR('',#33900,10.);
#9648=VECTOR('',#33901,10.);
#9649=VECTOR('',#33980,2.7202);
#9650=VECTOR('',#33985,10.);
#9651=VECTOR('',#33986,10.);
#9652=VECTOR('',#33987,10.);
#9653=VECTOR('',#33990,10.);
#9654=VECTOR('',#33991,10.);
#9655=VECTOR('',#33998,10.);
#9656=VECTOR('',#33999,10.);
#9657=VECTOR('',#34000,10.);
#9658=VECTOR('',#34003,10.);
#9659=VECTOR('',#34004,10.);
#9660=VECTOR('',#34011,10.);
#9661=VECTOR('',#34012,10.);
#9662=VECTOR('',#34013,10.);
#9663=VECTOR('',#34016,10.);
#9664=VECTOR('',#34017,10.);
#9665=VECTOR('',#34024,10.);
#9666=VECTOR('',#34025,10.);
#9667=VECTOR('',#34026,10.);
#9668=VECTOR('',#34029,10.);
#9669=VECTOR('',#34030,10.);
#9670=VECTOR('',#34037,10.);
#9671=VECTOR('',#34038,9.99999999999999);
#9672=VECTOR('',#34039,10.);
#9673=VECTOR('',#34042,10.);
#9674=VECTOR('',#34043,10.);
#9675=VECTOR('',#34050,10.);
#9676=VECTOR('',#34051,10.);
#9677=VECTOR('',#34052,10.);
#9678=VECTOR('',#34055,10.);
#9679=VECTOR('',#34056,10.);
#9680=VECTOR('',#34063,10.);
#9681=VECTOR('',#34064,10.);
#9682=VECTOR('',#34065,10.);
#9683=VECTOR('',#34068,10.);
#9684=VECTOR('',#34069,9.99999999999999);
#9685=VECTOR('',#34076,10.);
#9686=VECTOR('',#34077,10.);
#9687=VECTOR('',#34078,10.);
#9688=VECTOR('',#34081,10.);
#9689=VECTOR('',#34082,10.);
#9690=VECTOR('',#34091,10.);
#9691=VECTOR('',#34092,10.);
#9692=VECTOR('',#34093,10.);
#9693=VECTOR('',#34096,10.);
#9694=VECTOR('',#34097,10.);
#9695=VECTOR('',#34104,10.);
#9696=VECTOR('',#34105,10.);
#9697=VECTOR('',#34106,10.);
#9698=VECTOR('',#34109,10.);
#9699=VECTOR('',#34110,10.);
#9700=VECTOR('',#34117,10.);
#9701=VECTOR('',#34118,10.);
#9702=VECTOR('',#34119,10.);
#9703=VECTOR('',#34122,10.);
#9704=VECTOR('',#34123,10.);
#9705=VECTOR('',#34130,10.);
#9706=VECTOR('',#34131,10.);
#9707=VECTOR('',#34132,10.);
#9708=VECTOR('',#34135,10.);
#9709=VECTOR('',#34136,10.);
#9710=VECTOR('',#34143,10.);
#9711=VECTOR('',#34144,10.);
#9712=VECTOR('',#34145,10.);
#9713=VECTOR('',#34148,10.);
#9714=VECTOR('',#34149,10.);
#9715=VECTOR('',#34156,10.);
#9716=VECTOR('',#34157,9.99999999999999);
#9717=VECTOR('',#34158,10.);
#9718=VECTOR('',#34161,10.);
#9719=VECTOR('',#34162,10.);
#9720=VECTOR('',#34169,10.);
#9721=VECTOR('',#34170,10.);
#9722=VECTOR('',#34171,10.);
#9723=VECTOR('',#34174,10.);
#9724=VECTOR('',#34175,10.);
#9725=VECTOR('',#34182,10.);
#9726=VECTOR('',#34183,10.);
#9727=VECTOR('',#34184,10.);
#9728=VECTOR('',#34187,10.);
#9729=VECTOR('',#34188,10.);
#9730=VECTOR('',#34195,10.);
#9731=VECTOR('',#34196,10.);
#9732=VECTOR('',#34197,10.);
#9733=VECTOR('',#34200,10.);
#9734=VECTOR('',#34201,10.);
#9735=VECTOR('',#34208,10.);
#9736=VECTOR('',#34209,10.);
#9737=VECTOR('',#34210,10.);
#9738=VECTOR('',#34213,10.);
#9739=VECTOR('',#34214,10.);
#9740=VECTOR('',#34221,10.);
#9741=VECTOR('',#34222,10.);
#9742=VECTOR('',#34223,10.);
#9743=VECTOR('',#34226,10.);
#9744=VECTOR('',#34227,10.);
#9745=VECTOR('',#34234,10.);
#9746=VECTOR('',#34235,10.);
#9747=VECTOR('',#34236,10.);
#9748=VECTOR('',#34239,10.);
#9749=VECTOR('',#34240,9.99999999999999);
#9750=VECTOR('',#34247,10.);
#9751=VECTOR('',#34248,10.);
#9752=VECTOR('',#34249,10.);
#9753=VECTOR('',#34252,10.);
#9754=VECTOR('',#34253,10.);
#9755=VECTOR('',#34260,10.);
#9756=VECTOR('',#34261,10.);
#9757=VECTOR('',#34262,10.);
#9758=VECTOR('',#34265,10.);
#9759=VECTOR('',#34266,10.);
#9760=VECTOR('',#34273,10.);
#9761=VECTOR('',#34274,9.99999999999999);
#9762=VECTOR('',#34275,10.);
#9763=VECTOR('',#34278,10.);
#9764=VECTOR('',#34279,10.);
#9765=VECTOR('',#34286,10.);
#9766=VECTOR('',#34287,10.);
#9767=VECTOR('',#34288,10.);
#9768=VECTOR('',#34291,10.);
#9769=VECTOR('',#34292,10.);
#9770=VECTOR('',#34299,10.);
#9771=VECTOR('',#34300,10.);
#9772=VECTOR('',#34301,10.);
#9773=VECTOR('',#34304,10.);
#9774=VECTOR('',#34305,10.);
#9775=VECTOR('',#34312,10.);
#9776=VECTOR('',#34313,10.);
#9777=VECTOR('',#34314,10.);
#9778=VECTOR('',#34317,10.);
#9779=VECTOR('',#34318,10.);
#9780=VECTOR('',#34325,10.);
#9781=VECTOR('',#34326,10.);
#9782=VECTOR('',#34327,10.);
#9783=VECTOR('',#34330,10.);
#9784=VECTOR('',#34331,10.);
#9785=VECTOR('',#34338,10.);
#9786=VECTOR('',#34339,10.);
#9787=VECTOR('',#34340,10.);
#9788=VECTOR('',#34343,10.);
#9789=VECTOR('',#34344,10.);
#9790=VECTOR('',#34351,10.);
#9791=VECTOR('',#34352,10.);
#9792=VECTOR('',#34353,10.);
#9793=VECTOR('',#34356,10.);
#9794=VECTOR('',#34357,9.99999999999999);
#9795=VECTOR('',#34364,10.);
#9796=VECTOR('',#34365,10.);
#9797=VECTOR('',#34366,10.);
#9798=VECTOR('',#34369,10.);
#9799=VECTOR('',#34370,10.);
#9800=VECTOR('',#34377,10.);
#9801=VECTOR('',#34378,10.);
#9802=VECTOR('',#34379,10.);
#9803=VECTOR('',#34382,10.);
#9804=VECTOR('',#34383,10.);
#9805=VECTOR('',#34390,10.);
#9806=VECTOR('',#34391,9.99999999999999);
#9807=VECTOR('',#34392,10.);
#9808=VECTOR('',#34395,10.);
#9809=VECTOR('',#34396,10.);
#9810=VECTOR('',#34403,10.);
#9811=VECTOR('',#34404,10.);
#9812=VECTOR('',#34405,10.);
#9813=VECTOR('',#34408,10.);
#9814=VECTOR('',#34409,10.);
#9815=VECTOR('',#34416,10.);
#9816=VECTOR('',#34417,10.);
#9817=VECTOR('',#34418,10.);
#9818=VECTOR('',#34421,10.);
#9819=VECTOR('',#34422,10.);
#9820=VECTOR('',#34429,10.);
#9821=VECTOR('',#34430,10.);
#9822=VECTOR('',#34431,10.);
#9823=VECTOR('',#34434,10.);
#9824=VECTOR('',#34435,10.);
#9825=VECTOR('',#34442,2.8702);
#9826=VECTOR('',#34445,10.);
#9827=VECTOR('',#34446,10.);
#9828=VECTOR('',#34447,10.);
#9829=VECTOR('',#34448,10.);
#9830=VECTOR('',#34449,10.);
#9831=VECTOR('',#34450,10.);
#9832=VECTOR('',#34453,10.);
#9833=VECTOR('',#34458,10.);
#9834=VECTOR('',#34463,10.);
#9835=VECTOR('',#34468,10.);
#9836=VECTOR('',#34473,10.);
#9837=VECTOR('',#34478,10.);
#9838=VECTOR('',#34483,0.801975608296219);
#9839=VECTOR('',#34486,10.);
#9840=VECTOR('',#34487,10.);
#9841=VECTOR('',#34490,10.);
#9842=VECTOR('',#34493,10.);
#9843=VECTOR('',#34496,10.);
#9844=VECTOR('',#34499,10.);
#9845=VECTOR('',#34506,1.27);
#9846=VECTOR('',#34511,1.27);
#9847=VECTOR('',#34514,1.27);
#9848=VECTOR('',#34517,1.27);
#9849=VECTOR('',#34520,1.27);
#9850=VECTOR('',#34523,1.27);
#9851=VECTOR('',#34526,1.27);
#9852=VECTOR('',#34529,1.27);
#9853=VECTOR('',#34532,1.27);
#9854=VECTOR('',#34567,1.52934);
#9855=VECTOR('',#34574,10.);
#9856=VECTOR('',#34575,10.);
#9857=VECTOR('',#34576,10.);
#9858=VECTOR('',#34579,10.);
#9859=VECTOR('',#34580,10.);
#9860=VECTOR('',#34659,2.7202);
#9861=VECTOR('',#34664,10.);
#9862=VECTOR('',#34665,10.);
#9863=VECTOR('',#34666,10.);
#9864=VECTOR('',#34669,10.);
#9865=VECTOR('',#34670,10.);
#9866=VECTOR('',#34677,10.);
#9867=VECTOR('',#34678,10.);
#9868=VECTOR('',#34679,10.);
#9869=VECTOR('',#34682,10.);
#9870=VECTOR('',#34683,10.);
#9871=VECTOR('',#34690,10.);
#9872=VECTOR('',#34691,10.);
#9873=VECTOR('',#34692,10.);
#9874=VECTOR('',#34695,10.);
#9875=VECTOR('',#34696,10.);
#9876=VECTOR('',#34703,10.);
#9877=VECTOR('',#34704,10.);
#9878=VECTOR('',#34705,10.);
#9879=VECTOR('',#34708,10.);
#9880=VECTOR('',#34709,10.);
#9881=VECTOR('',#34716,10.);
#9882=VECTOR('',#34717,10.);
#9883=VECTOR('',#34718,10.);
#9884=VECTOR('',#34721,10.);
#9885=VECTOR('',#34722,10.);
#9886=VECTOR('',#34729,10.);
#9887=VECTOR('',#34730,10.);
#9888=VECTOR('',#34731,10.);
#9889=VECTOR('',#34734,10.);
#9890=VECTOR('',#34735,10.);
#9891=VECTOR('',#34742,10.);
#9892=VECTOR('',#34743,10.);
#9893=VECTOR('',#34744,10.);
#9894=VECTOR('',#34747,10.);
#9895=VECTOR('',#34748,10.);
#9896=VECTOR('',#34755,10.);
#9897=VECTOR('',#34756,10.);
#9898=VECTOR('',#34757,10.);
#9899=VECTOR('',#34760,10.);
#9900=VECTOR('',#34761,10.);
#9901=VECTOR('',#34768,10.);
#9902=VECTOR('',#34769,10.);
#9903=VECTOR('',#34770,10.);
#9904=VECTOR('',#34773,10.);
#9905=VECTOR('',#34774,10.);
#9906=VECTOR('',#34781,10.);
#9907=VECTOR('',#34782,9.99999999999999);
#9908=VECTOR('',#34783,10.);
#9909=VECTOR('',#34786,10.);
#9910=VECTOR('',#34787,10.);
#9911=VECTOR('',#34794,10.);
#9912=VECTOR('',#34795,10.);
#9913=VECTOR('',#34796,10.);
#9914=VECTOR('',#34799,10.);
#9915=VECTOR('',#34800,10.);
#9916=VECTOR('',#34807,10.);
#9917=VECTOR('',#34808,10.);
#9918=VECTOR('',#34809,10.);
#9919=VECTOR('',#34812,10.);
#9920=VECTOR('',#34813,10.);
#9921=VECTOR('',#34820,10.);
#9922=VECTOR('',#34821,10.);
#9923=VECTOR('',#34822,10.);
#9924=VECTOR('',#34825,10.);
#9925=VECTOR('',#34826,10.);
#9926=VECTOR('',#34833,10.);
#9927=VECTOR('',#34834,10.);
#9928=VECTOR('',#34835,10.);
#9929=VECTOR('',#34838,10.);
#9930=VECTOR('',#34839,10.);
#9931=VECTOR('',#34846,10.);
#9932=VECTOR('',#34847,10.);
#9933=VECTOR('',#34848,10.);
#9934=VECTOR('',#34851,10.);
#9935=VECTOR('',#34852,10.);
#9936=VECTOR('',#34859,10.);
#9937=VECTOR('',#34860,10.);
#9938=VECTOR('',#34861,10.);
#9939=VECTOR('',#34864,10.);
#9940=VECTOR('',#34865,10.);
#9941=VECTOR('',#34872,10.);
#9942=VECTOR('',#34873,10.);
#9943=VECTOR('',#34874,10.);
#9944=VECTOR('',#34877,10.);
#9945=VECTOR('',#34878,10.);
#9946=VECTOR('',#34887,10.);
#9947=VECTOR('',#34888,10.);
#9948=VECTOR('',#34889,10.);
#9949=VECTOR('',#34892,10.);
#9950=VECTOR('',#34893,10.);
#9951=VECTOR('',#34900,10.);
#9952=VECTOR('',#34901,10.);
#9953=VECTOR('',#34902,10.);
#9954=VECTOR('',#34905,10.);
#9955=VECTOR('',#34906,10.);
#9956=VECTOR('',#34913,10.);
#9957=VECTOR('',#34914,10.);
#9958=VECTOR('',#34915,10.);
#9959=VECTOR('',#34918,10.);
#9960=VECTOR('',#34919,10.);
#9961=VECTOR('',#34926,10.);
#9962=VECTOR('',#34927,10.);
#9963=VECTOR('',#34928,10.);
#9964=VECTOR('',#34931,10.);
#9965=VECTOR('',#34932,10.);
#9966=VECTOR('',#34939,10.);
#9967=VECTOR('',#34940,10.);
#9968=VECTOR('',#34941,10.);
#9969=VECTOR('',#34944,10.);
#9970=VECTOR('',#34945,10.);
#9971=VECTOR('',#34952,10.);
#9972=VECTOR('',#34953,10.);
#9973=VECTOR('',#34954,10.);
#9974=VECTOR('',#34957,10.);
#9975=VECTOR('',#34958,10.);
#9976=VECTOR('',#34965,10.);
#9977=VECTOR('',#34966,10.);
#9978=VECTOR('',#34967,10.);
#9979=VECTOR('',#34970,10.);
#9980=VECTOR('',#34971,10.);
#9981=VECTOR('',#34978,10.);
#9982=VECTOR('',#34979,10.);
#9983=VECTOR('',#34980,10.);
#9984=VECTOR('',#34983,10.);
#9985=VECTOR('',#34984,10.);
#9986=VECTOR('',#34991,10.);
#9987=VECTOR('',#34992,10.);
#9988=VECTOR('',#34993,10.);
#9989=VECTOR('',#34996,10.);
#9990=VECTOR('',#34997,10.);
#9991=VECTOR('',#35004,10.);
#9992=VECTOR('',#35005,10.);
#9993=VECTOR('',#35006,10.);
#9994=VECTOR('',#35009,10.);
#9995=VECTOR('',#35010,10.);
#9996=VECTOR('',#35017,10.);
#9997=VECTOR('',#35018,9.99999999999999);
#9998=VECTOR('',#35019,10.);
#9999=VECTOR('',#35022,10.);
#10000=VECTOR('',#35023,10.);
#10001=VECTOR('',#35030,10.);
#10002=VECTOR('',#35031,10.);
#10003=VECTOR('',#35032,10.);
#10004=VECTOR('',#35035,10.);
#10005=VECTOR('',#35036,10.);
#10006=VECTOR('',#35043,10.);
#10007=VECTOR('',#35044,10.);
#10008=VECTOR('',#35045,10.);
#10009=VECTOR('',#35048,10.);
#10010=VECTOR('',#35049,10.);
#10011=VECTOR('',#35056,10.);
#10012=VECTOR('',#35057,10.);
#10013=VECTOR('',#35058,10.);
#10014=VECTOR('',#35061,10.);
#10015=VECTOR('',#35062,10.);
#10016=VECTOR('',#35069,10.);
#10017=VECTOR('',#35070,10.);
#10018=VECTOR('',#35071,10.);
#10019=VECTOR('',#35074,10.);
#10020=VECTOR('',#35075,10.);
#10021=VECTOR('',#35082,10.);
#10022=VECTOR('',#35083,10.);
#10023=VECTOR('',#35084,10.);
#10024=VECTOR('',#35087,10.);
#10025=VECTOR('',#35088,10.);
#10026=VECTOR('',#35095,10.);
#10027=VECTOR('',#35096,9.99999999999999);
#10028=VECTOR('',#35097,10.);
#10029=VECTOR('',#35100,10.);
#10030=VECTOR('',#35101,10.);
#10031=VECTOR('',#35108,10.);
#10032=VECTOR('',#35109,10.);
#10033=VECTOR('',#35110,10.);
#10034=VECTOR('',#35113,10.);
#10035=VECTOR('',#35114,10.);
#10036=VECTOR('',#35121,2.8702);
#10037=VECTOR('',#35124,10.);
#10038=VECTOR('',#35125,10.);
#10039=VECTOR('',#35126,10.);
#10040=VECTOR('',#35127,10.);
#10041=VECTOR('',#35128,10.);
#10042=VECTOR('',#35129,10.);
#10043=VECTOR('',#35132,10.);
#10044=VECTOR('',#35137,10.);
#10045=VECTOR('',#35142,10.);
#10046=VECTOR('',#35147,10.);
#10047=VECTOR('',#35152,10.);
#10048=VECTOR('',#35157,10.);
#10049=VECTOR('',#35162,1.60395121659243);
#10050=VECTOR('',#35165,10.);
#10051=VECTOR('',#35166,10.);
#10052=VECTOR('',#35169,10.);
#10053=VECTOR('',#35172,10.);
#10054=VECTOR('',#35175,10.);
#10055=VECTOR('',#35178,10.);
#10056=VECTOR('',#35185,1.26999999999999);
#10057=VECTOR('',#35190,1.26999999999999);
#10058=VECTOR('',#35193,1.26999999999999);
#10059=VECTOR('',#35196,1.26999999999999);
#10060=VECTOR('',#35199,1.26999999999999);
#10061=VECTOR('',#35202,1.26999999999999);
#10062=VECTOR('',#35205,1.26999999999999);
#10063=VECTOR('',#35208,1.26999999999999);
#10064=VECTOR('',#35211,1.26999999999999);
#10065=VECTOR('',#35214,1.26999999999999);
#10066=VECTOR('',#35217,1.26999999999999);
#10067=VECTOR('',#35220,1.26999999999999);
#10068=VECTOR('',#35223,1.26999999999999);
#10069=VECTOR('',#35226,1.26999999999999);
#10070=VECTOR('',#35229,1.26999999999999);
#10071=VECTOR('',#35232,1.26999999999999);
#10072=VECTOR('',#35235,1.26999999999999);
#10073=VECTOR('',#35238,1.26999999999999);
#10074=VECTOR('',#35241,1.26999999999999);
#10075=VECTOR('',#35276,1.52934);
#10076=VECTOR('',#35283,10.);
#10077=VECTOR('',#35284,10.);
#10078=VECTOR('',#35285,10.);
#10079=VECTOR('',#35288,10.);
#10080=VECTOR('',#35289,10.);
#10081=VECTOR('',#35368,2.7202);
#10082=VECTOR('',#35373,10.);
#10083=VECTOR('',#35374,10.);
#10084=VECTOR('',#35375,10.);
#10085=VECTOR('',#35378,10.);
#10086=VECTOR('',#35379,10.);
#10087=VECTOR('',#35386,10.);
#10088=VECTOR('',#35387,10.);
#10089=VECTOR('',#35388,10.);
#10090=VECTOR('',#35391,10.);
#10091=VECTOR('',#35392,10.);
#10092=VECTOR('',#35399,10.);
#10093=VECTOR('',#35400,10.);
#10094=VECTOR('',#35401,10.);
#10095=VECTOR('',#35404,10.);
#10096=VECTOR('',#35405,10.);
#10097=VECTOR('',#35412,10.);
#10098=VECTOR('',#35413,10.);
#10099=VECTOR('',#35414,10.);
#10100=VECTOR('',#35417,10.);
#10101=VECTOR('',#35418,10.);
#10102=VECTOR('',#35425,10.);
#10103=VECTOR('',#35426,10.);
#10104=VECTOR('',#35427,10.);
#10105=VECTOR('',#35430,10.);
#10106=VECTOR('',#35431,10.);
#10107=VECTOR('',#35438,10.);
#10108=VECTOR('',#35439,10.);
#10109=VECTOR('',#35440,10.);
#10110=VECTOR('',#35443,10.);
#10111=VECTOR('',#35444,9.99999999999999);
#10112=VECTOR('',#35451,10.);
#10113=VECTOR('',#35452,10.);
#10114=VECTOR('',#35453,10.);
#10115=VECTOR('',#35456,10.);
#10116=VECTOR('',#35457,10.);
#10117=VECTOR('',#35464,10.);
#10118=VECTOR('',#35465,10.);
#10119=VECTOR('',#35466,10.);
#10120=VECTOR('',#35469,10.);
#10121=VECTOR('',#35470,10.);
#10122=VECTOR('',#35477,10.);
#10123=VECTOR('',#35478,10.);
#10124=VECTOR('',#35479,10.);
#10125=VECTOR('',#35482,10.);
#10126=VECTOR('',#35483,10.);
#10127=VECTOR('',#35490,10.);
#10128=VECTOR('',#35491,10.);
#10129=VECTOR('',#35492,10.);
#10130=VECTOR('',#35495,10.);
#10131=VECTOR('',#35496,10.);
#10132=VECTOR('',#35503,10.);
#10133=VECTOR('',#35504,10.);
#10134=VECTOR('',#35505,10.);
#10135=VECTOR('',#35508,10.);
#10136=VECTOR('',#35509,10.);
#10137=VECTOR('',#35516,10.);
#10138=VECTOR('',#35517,10.);
#10139=VECTOR('',#35518,10.);
#10140=VECTOR('',#35521,10.);
#10141=VECTOR('',#35522,10.);
#10142=VECTOR('',#35529,10.);
#10143=VECTOR('',#35530,10.);
#10144=VECTOR('',#35531,10.);
#10145=VECTOR('',#35534,10.);
#10146=VECTOR('',#35535,10.);
#10147=VECTOR('',#35542,10.);
#10148=VECTOR('',#35543,10.);
#10149=VECTOR('',#35544,10.);
#10150=VECTOR('',#35547,10.);
#10151=VECTOR('',#35548,10.);
#10152=VECTOR('',#35555,10.);
#10153=VECTOR('',#35556,10.);
#10154=VECTOR('',#35557,10.);
#10155=VECTOR('',#35560,10.);
#10156=VECTOR('',#35561,10.);
#10157=VECTOR('',#35568,10.);
#10158=VECTOR('',#35569,10.);
#10159=VECTOR('',#35570,10.);
#10160=VECTOR('',#35573,10.);
#10161=VECTOR('',#35574,10.);
#10162=VECTOR('',#35581,10.);
#10163=VECTOR('',#35582,10.);
#10164=VECTOR('',#35583,10.);
#10165=VECTOR('',#35586,10.);
#10166=VECTOR('',#35587,10.);
#10167=VECTOR('',#35596,10.);
#10168=VECTOR('',#35597,10.);
#10169=VECTOR('',#35598,10.);
#10170=VECTOR('',#35601,10.);
#10171=VECTOR('',#35602,10.);
#10172=VECTOR('',#35609,10.);
#10173=VECTOR('',#35610,10.);
#10174=VECTOR('',#35611,10.);
#10175=VECTOR('',#35614,10.);
#10176=VECTOR('',#35615,10.);
#10177=VECTOR('',#35622,10.);
#10178=VECTOR('',#35623,10.);
#10179=VECTOR('',#35624,10.);
#10180=VECTOR('',#35627,10.);
#10181=VECTOR('',#35628,10.);
#10182=VECTOR('',#35635,10.);
#10183=VECTOR('',#35636,10.);
#10184=VECTOR('',#35637,10.);
#10185=VECTOR('',#35640,10.);
#10186=VECTOR('',#35641,10.);
#10187=VECTOR('',#35648,10.);
#10188=VECTOR('',#35649,10.);
#10189=VECTOR('',#35650,10.);
#10190=VECTOR('',#35653,10.);
#10191=VECTOR('',#35654,10.);
#10192=VECTOR('',#35661,10.);
#10193=VECTOR('',#35662,10.);
#10194=VECTOR('',#35663,10.);
#10195=VECTOR('',#35666,10.);
#10196=VECTOR('',#35667,10.);
#10197=VECTOR('',#35674,10.);
#10198=VECTOR('',#35675,10.);
#10199=VECTOR('',#35676,10.);
#10200=VECTOR('',#35679,10.);
#10201=VECTOR('',#35680,10.);
#10202=VECTOR('',#35687,10.);
#10203=VECTOR('',#35688,10.);
#10204=VECTOR('',#35689,10.);
#10205=VECTOR('',#35692,10.);
#10206=VECTOR('',#35693,10.);
#10207=VECTOR('',#35700,10.);
#10208=VECTOR('',#35701,10.);
#10209=VECTOR('',#35702,10.);
#10210=VECTOR('',#35705,10.);
#10211=VECTOR('',#35706,10.);
#10212=VECTOR('',#35713,10.);
#10213=VECTOR('',#35714,10.);
#10214=VECTOR('',#35715,10.);
#10215=VECTOR('',#35718,10.);
#10216=VECTOR('',#35719,10.);
#10217=VECTOR('',#35726,10.);
#10218=VECTOR('',#35727,10.);
#10219=VECTOR('',#35728,10.);
#10220=VECTOR('',#35731,10.);
#10221=VECTOR('',#35732,10.);
#10222=VECTOR('',#35739,10.);
#10223=VECTOR('',#35740,10.);
#10224=VECTOR('',#35741,10.);
#10225=VECTOR('',#35744,10.);
#10226=VECTOR('',#35745,10.);
#10227=VECTOR('',#35752,10.);
#10228=VECTOR('',#35753,10.);
#10229=VECTOR('',#35754,10.);
#10230=VECTOR('',#35757,10.);
#10231=VECTOR('',#35758,10.);
#10232=VECTOR('',#35765,10.);
#10233=VECTOR('',#35766,10.);
#10234=VECTOR('',#35767,10.);
#10235=VECTOR('',#35770,10.);
#10236=VECTOR('',#35771,10.);
#10237=VECTOR('',#35778,10.);
#10238=VECTOR('',#35779,10.);
#10239=VECTOR('',#35780,10.);
#10240=VECTOR('',#35783,10.);
#10241=VECTOR('',#35784,10.);
#10242=VECTOR('',#35791,10.);
#10243=VECTOR('',#35792,10.);
#10244=VECTOR('',#35793,10.);
#10245=VECTOR('',#35796,10.);
#10246=VECTOR('',#35797,10.);
#10247=VECTOR('',#35804,10.);
#10248=VECTOR('',#35805,10.);
#10249=VECTOR('',#35806,10.);
#10250=VECTOR('',#35809,10.);
#10251=VECTOR('',#35810,10.);
#10252=VECTOR('',#35817,10.);
#10253=VECTOR('',#35818,10.);
#10254=VECTOR('',#35819,10.);
#10255=VECTOR('',#35822,10.);
#10256=VECTOR('',#35823,10.);
#10257=VECTOR('',#35830,2.8702);
#10258=VECTOR('',#35833,10.);
#10259=VECTOR('',#35834,10.);
#10260=VECTOR('',#35835,10.);
#10261=VECTOR('',#35836,10.);
#10262=VECTOR('',#35837,10.);
#10263=VECTOR('',#35838,10.);
#10264=VECTOR('',#35841,10.);
#10265=VECTOR('',#35846,10.);
#10266=VECTOR('',#35851,10.);
#10267=VECTOR('',#35856,10.);
#10268=VECTOR('',#35861,10.);
#10269=VECTOR('',#35866,10.);
#10270=VECTOR('',#35871,1.60395121659244);
#10271=VECTOR('',#35874,10.);
#10272=VECTOR('',#35875,10.);
#10273=VECTOR('',#35878,10.);
#10274=VECTOR('',#35881,10.);
#10275=VECTOR('',#35884,10.);
#10276=VECTOR('',#35887,10.);
#10277=VECTOR('',#35896,2.0312);
#10278=VECTOR('',#35907,4.7625);
#10279=VECTOR('',#35910,4.6875);
#10280=VECTOR('',#35919,1.98119999999999);
#10281=VECTOR('',#35926,1.92749999999999);
#10282=VECTOR('',#35931,1.80249999999999);
#10283=VECTOR('',#35942,3.59999999999999);
#10284=VECTOR('',#35947,3.5);
#10285=VECTOR('',#35958,1.9);
#10286=VECTOR('',#35963,4.42651513084632);
#10287=VECTOR('',#35966,10.);
#10288=VECTOR('',#35967,10.);
#10289=VECTOR('',#35968,10.);
#10290=VECTOR('',#35971,10.);
#10291=VECTOR('',#35972,10.);
#10292=VECTOR('',#35975,10.);
#10293=VECTOR('',#35976,10.);
#10294=VECTOR('',#35979,10.);
#10295=VECTOR('',#35980,10.);
#10296=VECTOR('',#35983,10.);
#10297=VECTOR('',#35984,10.);
#10298=VECTOR('',#35987,10.);
#10299=CIRCLE('',#27101,1.8025);
#10300=CIRCLE('',#27102,2.1025);
#10301=CIRCLE('',#27104,1.8025);
#10302=CIRCLE('',#27105,1.8025);
#10303=CIRCLE('',#27108,1.8025);
#10304=CIRCLE('',#27109,2.1025);
#10305=CIRCLE('',#27111,1.8025);
#10306=CIRCLE('',#27112,1.8025);
#10307=CIRCLE('',#27117,1.8025);
#10308=CIRCLE('',#27118,2.1025);
#10309=CIRCLE('',#27120,1.8025);
#10310=CIRCLE('',#27121,1.8025);
#10311=CIRCLE('',#27124,1.8025);
#10312=CIRCLE('',#27125,2.1025);
#10313=CIRCLE('',#27127,1.8025);
#10314=CIRCLE('',#27128,1.8025);
#10315=CIRCLE('',#27133,1.778);
#10316=CIRCLE('',#27134,1.778);
#10317=CIRCLE('',#27136,1.778);
#10318=CIRCLE('',#27137,1.778);
#10319=CIRCLE('',#27139,1.778);
#10320=CIRCLE('',#27140,1.778);
#10321=CIRCLE('',#27142,1.778);
#10322=CIRCLE('',#27143,1.778);
#10323=CIRCLE('',#27145,1.8025);
#10324=CIRCLE('',#27146,2.1025);
#10325=CIRCLE('',#27148,2.1025);
#10326=CIRCLE('',#27149,6.763);
#10327=CIRCLE('',#27150,2.1025);
#10328=CIRCLE('',#27151,2.1025);
#10329=CIRCLE('',#27153,1.8025);
#10330=CIRCLE('',#27155,1.8025);
#10331=CIRCLE('',#27157,1.8025);
#10332=CIRCLE('',#27159,1.8025);
#10333=CIRCLE('',#27161,1.8025);
#10334=CIRCLE('',#27163,1.8025);
#10335=CIRCLE('',#27165,1.8025);
#10336=CIRCLE('',#27167,6.363);
#10337=CIRCLE('',#27169,6.363);
#10338=CIRCLE('',#27209,1.778);
#10339=CIRCLE('',#27210,2.028);
#10340=CIRCLE('',#27212,3.19);
#10341=CIRCLE('',#27213,3.19);
#10342=CIRCLE('',#27214,3.19);
#10343=CIRCLE('',#27215,3.19);
#10344=CIRCLE('',#27216,2.028);
#10345=CIRCLE('',#27217,2.028);
#10346=CIRCLE('',#27218,1.8025);
#10347=CIRCLE('',#27219,1.8025);
#10348=CIRCLE('',#27220,1.8025);
#10349=CIRCLE('',#27221,1.8025);
#10350=CIRCLE('',#27222,0.799999999999992);
#10351=CIRCLE('',#27223,0.799999999999994);
#10352=CIRCLE('',#27224,2.475);
#10353=CIRCLE('',#27225,0.799999999999994);
#10354=CIRCLE('',#27226,0.799999999999994);
#10355=CIRCLE('',#27227,2.475);
#10356=CIRCLE('',#27228,2.028);
#10357=CIRCLE('',#27230,1.778);
#10358=CIRCLE('',#27232,1.778);
#10359=CIRCLE('',#27234,1.778);
#10360=CIRCLE('',#27236,1.778);
#10361=CIRCLE('',#27238,1.778);
#10362=CIRCLE('',#27240,1.778);
#10363=CIRCLE('',#27242,1.778);
#10364=CIRCLE('',#27244,1.8025);
#10365=CIRCLE('',#27245,2.1025);
#10366=CIRCLE('',#27247,2.89);
#10367=CIRCLE('',#27248,2.88999999999999);
#10368=CIRCLE('',#27249,2.89000000000001);
#10369=CIRCLE('',#27250,2.89);
#10370=CIRCLE('',#27251,2.1025);
#10371=CIRCLE('',#27252,1.09999999999999);
#10372=CIRCLE('',#27253,1.1);
#10373=CIRCLE('',#27254,2.775);
#10374=CIRCLE('',#27255,1.1);
#10375=CIRCLE('',#27256,1.09999999999999);
#10376=CIRCLE('',#27257,2.775);
#10377=CIRCLE('',#27258,2.1025);
#10378=CIRCLE('',#27259,2.1025);
#10379=CIRCLE('',#27262,1.8025);
#10380=CIRCLE('',#27265,1.8025);
#10381=CIRCLE('',#27268,1.8025);
#10382=CIRCLE('',#27284,3.19);
#10383=CIRCLE('',#27287,3.19);
#10384=CIRCLE('',#27290,3.19);
#10385=CIRCLE('',#27293,3.19);
#10386=CIRCLE('',#27314,2.475);
#10387=CIRCLE('',#27318,0.799999999999994);
#10388=CIRCLE('',#27321,0.799999999999992);
#10389=CIRCLE('',#27324,0.799999999999994);
#10390=CIRCLE('',#27327,0.799999999999994);
#10391=CIRCLE('',#27330,2.475);
#10392=CIRCLE('',#27362,2.5);
#10393=CIRCLE('',#27363,2.5);
#10394=CIRCLE('',#27366,2.);
#10395=CIRCLE('',#27367,2.);
#10396=CIRCLE('',#27369,2.);
#10397=CIRCLE('',#27370,2.);
#10398=CIRCLE('',#27372,2.);
#10399=CIRCLE('',#27373,2.);
#10400=CIRCLE('',#27375,2.);
#10401=CIRCLE('',#27376,2.);
#10402=CIRCLE('',#27378,1.55);
#10403=CIRCLE('',#27379,1.75);
#10404=CIRCLE('',#27381,1.55);
#10405=CIRCLE('',#27383,2.955);
#10406=CIRCLE('',#27386,3.255);
#10407=CIRCLE('',#27387,3.255);
#10408=CIRCLE('',#27390,5.5);
#10409=CIRCLE('',#27391,5.5);
#10410=CIRCLE('',#27393,5.2);
#10411=CIRCLE('',#27397,1.5);
#10412=CIRCLE('',#27398,1.5);
#10413=CIRCLE('',#27400,1.5);
#10414=CIRCLE('',#27401,1.5);
#10415=CIRCLE('',#27404,1.5);
#10416=CIRCLE('',#27405,1.5);
#10417=CIRCLE('',#27407,1.49999999999999);
#10418=CIRCLE('',#27408,1.49999999999999);
#10419=CIRCLE('',#27411,0.999999999999992);
#10420=CIRCLE('',#27412,0.999999999999996);
#10421=CIRCLE('',#27414,0.999999999999999);
#10422=CIRCLE('',#27415,1.);
#10423=CIRCLE('',#27417,1.5);
#10424=CIRCLE('',#27418,1.49999999999999);
#10425=CIRCLE('',#27419,0.999999999999996);
#10426=CIRCLE('',#27420,0.999999999999992);
#10427=CIRCLE('',#27425,1.);
#10428=CIRCLE('',#27428,0.999999999999999);
#10429=CIRCLE('',#27432,1.5);
#10430=CIRCLE('',#27433,1.5);
#10431=CIRCLE('',#27435,1.49999999999999);
#10432=CIRCLE('',#27436,1.5);
#10433=CIRCLE('',#27439,1.5);
#10434=CIRCLE('',#27440,1.5);
#10435=CIRCLE('',#27443,1.5);
#10436=CIRCLE('',#27444,1.5);
#10437=CIRCLE('',#27447,1.5);
#10438=CIRCLE('',#27450,1.49999999999999);
#10439=CIRCLE('',#27456,7.14399999999837);
#10440=CIRCLE('',#27457,7.14399999999837);
#10441=CIRCLE('',#27460,5.358);
#10442=CIRCLE('',#27461,7.14399999999837);
#10443=CIRCLE('',#27462,5.358);
#10444=CIRCLE('',#27463,7.14399999999837);
#10445=CIRCLE('',#27464,5.358);
#10446=CIRCLE('',#27465,7.14399999999837);
#10447=CIRCLE('',#27466,5.358);
#10448=CIRCLE('',#27467,7.14399999999837);
#10449=CIRCLE('',#27468,5.358);
#10450=CIRCLE('',#27469,7.14399999999837);
#10451=CIRCLE('',#27470,5.358);
#10452=CIRCLE('',#27471,7.14399999999837);
#10453=CIRCLE('',#27472,5.358);
#10454=CIRCLE('',#27473,7.14399999999837);
#10455=CIRCLE('',#27474,5.358);
#10456=CIRCLE('',#27475,7.14399999999837);
#10457=CIRCLE('',#27476,5.358);
#10458=CIRCLE('',#27477,7.14399999999837);
#10459=CIRCLE('',#27478,5.358);
#10460=CIRCLE('',#27479,7.14399999999837);
#10461=CIRCLE('',#27480,5.358);
#10462=CIRCLE('',#27481,7.14399999999837);
#10463=CIRCLE('',#27482,5.358);
#10464=CIRCLE('',#27483,7.14399999999837);
#10465=CIRCLE('',#27484,5.358);
#10466=CIRCLE('',#27485,7.14399999999837);
#10467=CIRCLE('',#27486,5.358);
#10468=CIRCLE('',#27487,7.14399999999837);
#10469=CIRCLE('',#27488,5.358);
#10470=CIRCLE('',#27489,7.14399999999837);
#10471=CIRCLE('',#27490,5.358);
#10472=CIRCLE('',#27491,4.477);
#10473=CIRCLE('',#27493,5.358);
#10474=CIRCLE('',#27496,7.14399999999837);
#10475=CIRCLE('',#27499,5.358);
#10476=CIRCLE('',#27502,7.14399999999837);
#10477=CIRCLE('',#27505,5.358);
#10478=CIRCLE('',#27508,7.14399999999837);
#10479=CIRCLE('',#27511,5.358);
#10480=CIRCLE('',#27514,7.14399999999837);
#10481=CIRCLE('',#27517,5.358);
#10482=CIRCLE('',#27520,7.14399999999837);
#10483=CIRCLE('',#27523,5.358);
#10484=CIRCLE('',#27526,7.14399999999837);
#10485=CIRCLE('',#27529,5.358);
#10486=CIRCLE('',#27532,7.14399999999837);
#10487=CIRCLE('',#27535,5.358);
#10488=CIRCLE('',#27538,7.14399999999837);
#10489=CIRCLE('',#27541,5.358);
#10490=CIRCLE('',#27544,7.14399999999837);
#10491=CIRCLE('',#27547,5.358);
#10492=CIRCLE('',#27550,7.14399999999837);
#10493=CIRCLE('',#27553,5.358);
#10494=CIRCLE('',#27556,7.14399999999837);
#10495=CIRCLE('',#27559,5.358);
#10496=CIRCLE('',#27562,7.14399999999837);
#10497=CIRCLE('',#27565,5.358);
#10498=CIRCLE('',#27568,7.14399999999837);
#10499=CIRCLE('',#27571,5.358);
#10500=CIRCLE('',#27575,7.14399999999837);
#10501=CIRCLE('',#27577,5.358);
#10502=CIRCLE('',#27578,7.14399999999837);
#10503=CIRCLE('',#27579,5.358);
#10504=CIRCLE('',#27580,3.261);
#10505=CIRCLE('',#27587,3.261);
#10506=CIRCLE('',#27588,1.6);
#10507=CIRCLE('',#27590,1.6);
#10508=CIRCLE('',#27592,4.477);
#10509=CIRCLE('',#27597,1.17775);
#10510=CIRCLE('',#27609,1.4635);
#10511=CIRCLE('',#27621,1.4635);
#10512=CIRCLE('',#27623,1.17775);
#10513=CIRCLE('',#27625,1.4635);
#10514=CIRCLE('',#27626,1.4635);
#10515=CIRCLE('',#27628,1.4635);
#10516=CIRCLE('',#27629,1.4635);
#10517=CIRCLE('',#27631,1.5635);
#10518=CIRCLE('',#27632,0.1);
#10519=CIRCLE('',#27634,2.55);
#10520=CIRCLE('',#27636,1.1135);
#10521=CIRCLE('',#27640,2.75);
#10522=CIRCLE('',#27643,2.75);
#10523=CIRCLE('',#27644,2.75);
#10524=CIRCLE('',#27645,2.75);
#10525=CIRCLE('',#27646,2.75);
#10526=CIRCLE('',#27647,2.75);
#10527=CIRCLE('',#27648,2.75);
#10528=CIRCLE('',#27649,2.75);
#10529=CIRCLE('',#27650,2.75);
#10530=CIRCLE('',#27651,2.75);
#10531=CIRCLE('',#27652,2.75);
#10532=CIRCLE('',#27653,2.75);
#10533=CIRCLE('',#27654,2.75);
#10534=CIRCLE('',#27655,2.75);
#10535=CIRCLE('',#27656,2.75);
#10536=CIRCLE('',#27657,2.75);
#10537=CIRCLE('',#27658,2.75);
#10538=CIRCLE('',#27659,2.75);
#10539=CIRCLE('',#27660,2.75);
#10540=CIRCLE('',#27661,2.75);
#10541=CIRCLE('',#27662,2.75);
#10542=CIRCLE('',#27663,2.75);
#10543=CIRCLE('',#27664,2.75);
#10544=CIRCLE('',#27665,2.75);
#10545=CIRCLE('',#27666,2.75);
#10546=CIRCLE('',#27667,2.75);
#10547=CIRCLE('',#27668,2.75);
#10548=CIRCLE('',#27669,2.75);
#10549=CIRCLE('',#27670,2.75);
#10550=CIRCLE('',#27671,2.75);
#10551=CIRCLE('',#27672,2.75);
#10552=CIRCLE('',#27673,2.75);
#10553=CIRCLE('',#27674,2.75);
#10554=CIRCLE('',#27675,2.75);
#10555=CIRCLE('',#27676,2.75);
#10556=CIRCLE('',#27677,2.75);
#10557=CIRCLE('',#27678,2.75);
#10558=CIRCLE('',#27679,2.75);
#10559=CIRCLE('',#27680,2.75);
#10560=CIRCLE('',#27681,2.75);
#10561=CIRCLE('',#27682,2.75);
#10562=CIRCLE('',#27683,2.75);
#10563=CIRCLE('',#27684,2.75);
#10564=CIRCLE('',#27685,2.75);
#10565=CIRCLE('',#27686,2.75);
#10566=CIRCLE('',#27687,2.75);
#10567=CIRCLE('',#27688,2.75);
#10568=CIRCLE('',#27689,2.75);
#10569=CIRCLE('',#27690,2.75);
#10570=CIRCLE('',#27691,2.75);
#10571=CIRCLE('',#27692,2.75);
#10572=CIRCLE('',#27693,2.75);
#10573=CIRCLE('',#27694,2.75);
#10574=CIRCLE('',#27695,2.75);
#10575=CIRCLE('',#27696,2.75);
#10576=CIRCLE('',#27697,2.75);
#10577=CIRCLE('',#27698,2.75);
#10578=CIRCLE('',#27699,2.75);
#10579=CIRCLE('',#27700,2.75);
#10580=CIRCLE('',#27701,2.75);
#10581=CIRCLE('',#27702,2.75);
#10582=CIRCLE('',#27703,2.75);
#10583=CIRCLE('',#27704,2.75);
#10584=CIRCLE('',#27705,2.75);
#10585=CIRCLE('',#27706,2.75);
#10586=CIRCLE('',#27707,2.75);
#10587=CIRCLE('',#27708,2.75);
#10588=CIRCLE('',#27709,2.75);
#10589=CIRCLE('',#27710,2.75);
#10590=CIRCLE('',#27711,2.75);
#10591=CIRCLE('',#27712,2.75);
#10592=CIRCLE('',#27713,2.75);
#10593=CIRCLE('',#27714,2.75);
#10594=CIRCLE('',#27715,2.75);
#10595=CIRCLE('',#27716,2.75);
#10596=CIRCLE('',#27823,0.2);
#10597=CIRCLE('',#27825,2.45);
#10598=CIRCLE('',#27827,1.59337567297407);
#10599=CIRCLE('',#27829,1.39337567297406);
#10600=CIRCLE('',#27830,1.39337567297406);
#10601=CIRCLE('',#27831,1.39337567297406);
#10602=CIRCLE('',#27832,1.39337567297406);
#10603=CIRCLE('',#27833,1.39337567297406);
#10604=CIRCLE('',#27834,1.39337567297406);
#10605=CIRCLE('',#27836,1.39337567297406);
#10606=CIRCLE('',#27838,1.39337567297406);
#10607=CIRCLE('',#27840,1.39337567297406);
#10608=CIRCLE('',#27842,1.39337567297406);
#10609=CIRCLE('',#27844,1.39337567297406);
#10610=CIRCLE('',#27846,1.39337567297406);
#10611=CIRCLE('',#27857,1.44337567297406);
#10612=CIRCLE('',#27859,1.44337567297406);
#10613=CIRCLE('',#27861,1.44337567297406);
#10614=CIRCLE('',#27863,1.44337567297406);
#10615=CIRCLE('',#27865,1.44337567297406);
#10616=CIRCLE('',#27867,1.44337567297406);
#10617=CIRCLE('',#27874,1.778);
#10618=CIRCLE('',#27875,1.97799999999999);
#10619=CIRCLE('',#27877,4.51249999999999);
#10620=CIRCLE('',#27878,4.5125);
#10621=CIRCLE('',#27879,1.97799999999999);
#10622=CIRCLE('',#27880,1.978);
#10623=CIRCLE('',#27881,1.97799999999999);
#10624=CIRCLE('',#27882,1.978);
#10625=CIRCLE('',#27883,1.978);
#10626=CIRCLE('',#27884,1.978);
#10627=CIRCLE('',#27885,1.978);
#10628=CIRCLE('',#27886,1.978);
#10629=CIRCLE('',#27887,1.978);
#10630=CIRCLE('',#27888,1.978);
#10631=CIRCLE('',#27889,1.97799999999999);
#10632=CIRCLE('',#27890,1.978);
#10633=CIRCLE('',#27891,1.978);
#10634=CIRCLE('',#27892,1.978);
#10635=CIRCLE('',#27893,1.978);
#10636=CIRCLE('',#27894,1.97799999999999);
#10637=CIRCLE('',#27895,1.978);
#10638=CIRCLE('',#27896,1.978);
#10639=CIRCLE('',#27897,1.978);
#10640=CIRCLE('',#27898,1.978);
#10641=CIRCLE('',#27900,1.778);
#10642=CIRCLE('',#27902,1.778);
#10643=CIRCLE('',#27904,1.778);
#10644=CIRCLE('',#27906,1.778);
#10645=CIRCLE('',#27908,1.778);
#10646=CIRCLE('',#27910,1.778);
#10647=CIRCLE('',#27912,1.778);
#10648=CIRCLE('',#27914,1.778);
#10649=CIRCLE('',#27916,1.778);
#10650=CIRCLE('',#27918,1.778);
#10651=CIRCLE('',#27920,1.778);
#10652=CIRCLE('',#27922,1.778);
#10653=CIRCLE('',#27924,1.778);
#10654=CIRCLE('',#27926,1.778);
#10655=CIRCLE('',#27928,1.778);
#10656=CIRCLE('',#27930,1.778);
#10657=CIRCLE('',#27932,1.778);
#10658=CIRCLE('',#27934,1.778);
#10659=CIRCLE('',#27936,1.778);
#10660=CIRCLE('',#27938,1.778);
#10661=CIRCLE('',#27940,1.778);
#10662=CIRCLE('',#27942,1.778);
#10663=CIRCLE('',#27944,1.778);
#10664=CIRCLE('',#27946,1.778);
#10665=CIRCLE('',#27948,1.778);
#10666=CIRCLE('',#27950,1.778);
#10667=CIRCLE('',#27952,1.778);
#10668=CIRCLE('',#27954,1.778);
#10669=CIRCLE('',#27956,1.778);
#10670=CIRCLE('',#27958,1.778);
#10671=CIRCLE('',#27960,1.778);
#10672=CIRCLE('',#27962,1.778);
#10673=CIRCLE('',#27964,1.778);
#10674=CIRCLE('',#27966,1.778);
#10675=CIRCLE('',#27968,1.778);
#10676=CIRCLE('',#27970,1.778);
#10677=CIRCLE('',#27972,1.778);
#10678=CIRCLE('',#27974,1.778);
#10679=CIRCLE('',#27976,1.778);
#10680=CIRCLE('',#27978,1.778);
#10681=CIRCLE('',#27980,1.778);
#10682=CIRCLE('',#27983,4.7625);
#10683=CIRCLE('',#27986,4.7625);
#10684=CIRCLE('',#27988,4.7625);
#10685=CIRCLE('',#27992,4.7625);
#10686=CIRCLE('',#27993,4.5125);
#10687=CIRCLE('',#27996,4.51249999999999);
#10688=CIRCLE('',#28003,4.5625);
#10689=CIRCLE('',#28004,4.7625);
#10690=CIRCLE('',#28007,4.5625);
#10691=CIRCLE('',#28008,4.7625);
#10692=CIRCLE('',#28012,4.7625);
#10693=CIRCLE('',#28015,4.7625);
#10694=CIRCLE('',#28019,4.5625);
#10695=CIRCLE('',#28022,4.5625);
#10696=CIRCLE('',#28025,1.778);
#10697=CIRCLE('',#28026,1.778);
#10698=CIRCLE('',#28028,1.778);
#10699=CIRCLE('',#28029,1.778);
#10700=CIRCLE('',#28031,1.778);
#10701=CIRCLE('',#28032,1.778);
#10702=CIRCLE('',#28034,1.778);
#10703=CIRCLE('',#28035,1.778);
#10704=CIRCLE('',#28037,1.778);
#10705=CIRCLE('',#28038,1.778);
#10706=CIRCLE('',#28040,1.778);
#10707=CIRCLE('',#28041,1.778);
#10708=CIRCLE('',#28043,1.778);
#10709=CIRCLE('',#28044,1.778);
#10710=CIRCLE('',#28046,1.778);
#10711=CIRCLE('',#28047,1.778);
#10712=CIRCLE('',#28049,1.778);
#10713=CIRCLE('',#28050,1.778);
#10714=CIRCLE('',#28052,1.778);
#10715=CIRCLE('',#28053,1.778);
#10716=CIRCLE('',#28337,1.778);
#10717=CIRCLE('',#28338,2.028);
#10718=CIRCLE('',#28340,2.028);
#10719=CIRCLE('',#28341,2.028);
#10720=CIRCLE('',#28342,2.028);
#10721=CIRCLE('',#28343,2.028);
#10722=CIRCLE('',#28344,2.028);
#10723=CIRCLE('',#28345,2.028);
#10724=CIRCLE('',#28346,2.028);
#10725=CIRCLE('',#28348,1.778);
#10726=CIRCLE('',#28350,1.778);
#10727=CIRCLE('',#28352,1.778);
#10728=CIRCLE('',#28354,1.778);
#10729=CIRCLE('',#28356,1.778);
#10730=CIRCLE('',#28358,1.778);
#10731=CIRCLE('',#28360,1.778);
#10732=CIRCLE('',#28362,1.778);
#10733=CIRCLE('',#28364,1.778);
#10734=CIRCLE('',#28366,1.778);
#10735=CIRCLE('',#28368,1.778);
#10736=CIRCLE('',#28370,1.778);
#10737=CIRCLE('',#28372,1.778);
#10738=CIRCLE('',#28374,1.778);
#10739=CIRCLE('',#28376,1.778);
#10740=CIRCLE('',#28408,1.778);
#10741=CIRCLE('',#28409,1.778);
#10742=CIRCLE('',#28411,1.778);
#10743=CIRCLE('',#28412,1.778);
#10744=CIRCLE('',#28414,1.8025);
#10745=CIRCLE('',#28415,2.1025);
#10746=CIRCLE('',#28418,1.8025);
#10747=CIRCLE('',#28420,1.8025);
#10748=CIRCLE('',#28424,1.8025);
#10749=CIRCLE('',#28425,2.1025);
#10750=CIRCLE('',#28428,1.8025);
#10751=CIRCLE('',#28430,1.8025);
#10752=CIRCLE('',#28436,1.8025);
#10753=CIRCLE('',#28437,1.8025);
#10754=CIRCLE('',#28438,1.8025);
#10755=CIRCLE('',#28442,1.8025);
#10756=CIRCLE('',#28443,1.8025);
#10757=CIRCLE('',#28444,1.8025);
#10758=CIRCLE('',#28446,2.1025);
#10759=CIRCLE('',#28450,2.1025);
#10760=CIRCLE('',#28463,1.27);
#10761=CIRCLE('',#28471,1.70434);
#10762=CIRCLE('',#28472,1.70434);
#10763=CIRCLE('',#28474,1.27);
#10764=CIRCLE('',#28476,1.70434);
#10765=CIRCLE('',#28477,1.70434);
#10766=CIRCLE('',#28479,1.70434);
#10767=CIRCLE('',#28480,1.70434);
#10768=CIRCLE('',#28482,1.85434);
#10769=CIRCLE('',#28483,0.15);
#10770=CIRCLE('',#28485,2.8702);
#10771=CIRCLE('',#28487,1.35434);
#10772=CIRCLE('',#28492,2.8702);
#10773=CIRCLE('',#28494,2.8702);
#10774=CIRCLE('',#28495,2.8702);
#10775=CIRCLE('',#28496,2.8702);
#10776=CIRCLE('',#28497,2.8702);
#10777=CIRCLE('',#28498,2.8702);
#10778=CIRCLE('',#28499,2.8702);
#10779=CIRCLE('',#28500,2.8702);
#10780=CIRCLE('',#28501,2.8702);
#10781=CIRCLE('',#28502,2.8702);
#10782=CIRCLE('',#28503,2.8702);
#10783=CIRCLE('',#28504,2.8702);
#10784=CIRCLE('',#28505,2.8702);
#10785=CIRCLE('',#28506,2.8702);
#10786=CIRCLE('',#28507,2.8702);
#10787=CIRCLE('',#28508,2.8702);
#10788=CIRCLE('',#28509,2.8702);
#10789=CIRCLE('',#28510,2.8702);
#10790=CIRCLE('',#28511,2.8702);
#10791=CIRCLE('',#28512,2.8702);
#10792=CIRCLE('',#28513,2.8702);
#10793=CIRCLE('',#28514,2.8702);
#10794=CIRCLE('',#28515,2.8702);
#10795=CIRCLE('',#28516,2.8702);
#10796=CIRCLE('',#28517,2.8702);
#10797=CIRCLE('',#28518,2.8702);
#10798=CIRCLE('',#28519,2.8702);
#10799=CIRCLE('',#28520,2.8702);
#10800=CIRCLE('',#28521,2.8702);
#10801=CIRCLE('',#28522,2.8702);
#10802=CIRCLE('',#28523,2.8702);
#10803=CIRCLE('',#28524,2.8702);
#10804=CIRCLE('',#28525,2.8702);
#10805=CIRCLE('',#28526,2.8702);
#10806=CIRCLE('',#28527,2.8702);
#10807=CIRCLE('',#28528,2.8702);
#10808=CIRCLE('',#28529,2.8702);
#10809=CIRCLE('',#28530,2.5702);
#10810=CIRCLE('',#28534,2.8702);
#10811=CIRCLE('',#28538,2.8702);
#10812=CIRCLE('',#28542,2.8702);
#10813=CIRCLE('',#28546,2.8702);
#10814=CIRCLE('',#28550,2.8702);
#10815=CIRCLE('',#28554,2.8702);
#10816=CIRCLE('',#28558,2.8702);
#10817=CIRCLE('',#28562,2.8702);
#10818=CIRCLE('',#28563,2.8702);
#10819=CIRCLE('',#28567,2.8702);
#10820=CIRCLE('',#28571,2.8702);
#10821=CIRCLE('',#28575,2.8702);
#10822=CIRCLE('',#28579,2.8702);
#10823=CIRCLE('',#28583,2.8702);
#10824=CIRCLE('',#28587,2.8702);
#10825=CIRCLE('',#28591,2.8702);
#10826=CIRCLE('',#28595,2.8702);
#10827=CIRCLE('',#28599,2.8702);
#10828=CIRCLE('',#28603,2.8702);
#10829=CIRCLE('',#28607,2.8702);
#10830=CIRCLE('',#28611,2.8702);
#10831=CIRCLE('',#28615,2.8702);
#10832=CIRCLE('',#28619,2.8702);
#10833=CIRCLE('',#28623,2.8702);
#10834=CIRCLE('',#28627,2.8702);
#10835=CIRCLE('',#28631,2.8702);
#10836=CIRCLE('',#28635,2.8702);
#10837=CIRCLE('',#28639,2.8702);
#10838=CIRCLE('',#28643,2.8702);
#10839=CIRCLE('',#28647,2.8702);
#10840=CIRCLE('',#28651,2.8702);
#10841=CIRCLE('',#28655,2.8702);
#10842=CIRCLE('',#28659,2.8702);
#10843=CIRCLE('',#28663,2.8702);
#10844=CIRCLE('',#28667,2.8702);
#10845=CIRCLE('',#28671,2.8702);
#10846=CIRCLE('',#28675,1.60395121659243);
#10847=CIRCLE('',#28677,1.60395121659243);
#10848=CIRCLE('',#28679,1.60395121659243);
#10849=CIRCLE('',#28681,1.60395121659243);
#10850=CIRCLE('',#28683,1.60395121659243);
#10851=CIRCLE('',#28685,1.60395121659243);
#10852=CIRCLE('',#28695,1.27);
#10853=CIRCLE('',#28705,1.70434);
#10854=CIRCLE('',#28706,1.70434);
#10855=CIRCLE('',#28708,1.27);
#10856=CIRCLE('',#28710,1.70434);
#10857=CIRCLE('',#28711,1.70434);
#10858=CIRCLE('',#28713,1.70434);
#10859=CIRCLE('',#28714,1.70434);
#10860=CIRCLE('',#28716,1.85434);
#10861=CIRCLE('',#28717,0.15);
#10862=CIRCLE('',#28719,2.8702);
#10863=CIRCLE('',#28721,1.35434);
#10864=CIRCLE('',#28726,2.8702);
#10865=CIRCLE('',#28728,2.8702);
#10866=CIRCLE('',#28729,2.8702);
#10867=CIRCLE('',#28730,2.8702);
#10868=CIRCLE('',#28731,2.8702);
#10869=CIRCLE('',#28732,2.8702);
#10870=CIRCLE('',#28733,2.8702);
#10871=CIRCLE('',#28734,2.8702);
#10872=CIRCLE('',#28735,2.8702);
#10873=CIRCLE('',#28736,2.8702);
#10874=CIRCLE('',#28737,2.8702);
#10875=CIRCLE('',#28738,2.8702);
#10876=CIRCLE('',#28739,2.8702);
#10877=CIRCLE('',#28740,2.8702);
#10878=CIRCLE('',#28741,2.8702);
#10879=CIRCLE('',#28742,2.8702);
#10880=CIRCLE('',#28743,2.8702);
#10881=CIRCLE('',#28744,2.8702);
#10882=CIRCLE('',#28745,2.8702);
#10883=CIRCLE('',#28746,2.8702);
#10884=CIRCLE('',#28747,2.8702);
#10885=CIRCLE('',#28748,2.8702);
#10886=CIRCLE('',#28749,2.8702);
#10887=CIRCLE('',#28750,2.8702);
#10888=CIRCLE('',#28751,2.8702);
#10889=CIRCLE('',#28752,2.8702);
#10890=CIRCLE('',#28753,2.8702);
#10891=CIRCLE('',#28754,2.8702);
#10892=CIRCLE('',#28755,2.8702);
#10893=CIRCLE('',#28756,2.8702);
#10894=CIRCLE('',#28757,2.8702);
#10895=CIRCLE('',#28758,2.8702);
#10896=CIRCLE('',#28759,2.8702);
#10897=CIRCLE('',#28760,2.8702);
#10898=CIRCLE('',#28761,2.8702);
#10899=CIRCLE('',#28762,2.8702);
#10900=CIRCLE('',#28763,2.8702);
#10901=CIRCLE('',#28764,2.5702);
#10902=CIRCLE('',#28768,2.8702);
#10903=CIRCLE('',#28772,2.8702);
#10904=CIRCLE('',#28776,2.8702);
#10905=CIRCLE('',#28780,2.8702);
#10906=CIRCLE('',#28784,2.8702);
#10907=CIRCLE('',#28788,2.8702);
#10908=CIRCLE('',#28792,2.8702);
#10909=CIRCLE('',#28796,2.8702);
#10910=CIRCLE('',#28800,2.8702);
#10911=CIRCLE('',#28804,2.8702);
#10912=CIRCLE('',#28808,2.8702);
#10913=CIRCLE('',#28812,2.8702);
#10914=CIRCLE('',#28816,2.8702);
#10915=CIRCLE('',#28820,2.8702);
#10916=CIRCLE('',#28824,2.8702);
#10917=CIRCLE('',#28828,2.8702);
#10918=CIRCLE('',#28832,2.8702);
#10919=CIRCLE('',#28833,2.8702);
#10920=CIRCLE('',#28837,2.8702);
#10921=CIRCLE('',#28841,2.8702);
#10922=CIRCLE('',#28845,2.8702);
#10923=CIRCLE('',#28849,2.8702);
#10924=CIRCLE('',#28853,2.8702);
#10925=CIRCLE('',#28857,2.8702);
#10926=CIRCLE('',#28861,2.8702);
#10927=CIRCLE('',#28865,2.8702);
#10928=CIRCLE('',#28869,2.8702);
#10929=CIRCLE('',#28873,2.8702);
#10930=CIRCLE('',#28877,2.8702);
#10931=CIRCLE('',#28881,2.8702);
#10932=CIRCLE('',#28885,2.8702);
#10933=CIRCLE('',#28889,2.8702);
#10934=CIRCLE('',#28893,2.8702);
#10935=CIRCLE('',#28897,2.8702);
#10936=CIRCLE('',#28901,2.8702);
#10937=CIRCLE('',#28905,2.8702);
#10938=CIRCLE('',#28909,1.60395121659243);
#10939=CIRCLE('',#28911,1.60395121659243);
#10940=CIRCLE('',#28913,1.60395121659243);
#10941=CIRCLE('',#28915,1.60395121659243);
#10942=CIRCLE('',#28917,1.60395121659243);
#10943=CIRCLE('',#28919,1.60395121659243);
#10944=CIRCLE('',#28929,1.26999999999999);
#10945=CIRCLE('',#28949,1.70434);
#10946=CIRCLE('',#28950,1.70434);
#10947=CIRCLE('',#28952,1.26999999999999);
#10948=CIRCLE('',#28954,1.70434);
#10949=CIRCLE('',#28955,1.70434);
#10950=CIRCLE('',#28957,1.70434);
#10951=CIRCLE('',#28958,1.70434);
#10952=CIRCLE('',#28960,1.85434);
#10953=CIRCLE('',#28961,0.15);
#10954=CIRCLE('',#28963,2.8702);
#10955=CIRCLE('',#28965,1.35434);
#10956=CIRCLE('',#28970,2.8702);
#10957=CIRCLE('',#28972,2.8702);
#10958=CIRCLE('',#28973,2.8702);
#10959=CIRCLE('',#28974,2.8702);
#10960=CIRCLE('',#28975,2.8702);
#10961=CIRCLE('',#28976,2.8702);
#10962=CIRCLE('',#28977,2.8702);
#10963=CIRCLE('',#28978,2.8702);
#10964=CIRCLE('',#28979,2.8702);
#10965=CIRCLE('',#28980,2.8702);
#10966=CIRCLE('',#28981,2.8702);
#10967=CIRCLE('',#28982,2.8702);
#10968=CIRCLE('',#28983,2.8702);
#10969=CIRCLE('',#28984,2.8702);
#10970=CIRCLE('',#28985,2.8702);
#10971=CIRCLE('',#28986,2.8702);
#10972=CIRCLE('',#28987,2.8702);
#10973=CIRCLE('',#28988,2.8702);
#10974=CIRCLE('',#28989,2.8702);
#10975=CIRCLE('',#28990,2.8702);
#10976=CIRCLE('',#28991,2.8702);
#10977=CIRCLE('',#28992,2.8702);
#10978=CIRCLE('',#28993,2.8702);
#10979=CIRCLE('',#28994,2.8702);
#10980=CIRCLE('',#28995,2.8702);
#10981=CIRCLE('',#28996,2.8702);
#10982=CIRCLE('',#28997,2.8702);
#10983=CIRCLE('',#28998,2.8702);
#10984=CIRCLE('',#28999,2.8702);
#10985=CIRCLE('',#29000,2.8702);
#10986=CIRCLE('',#29001,2.8702);
#10987=CIRCLE('',#29002,2.8702);
#10988=CIRCLE('',#29003,2.8702);
#10989=CIRCLE('',#29004,2.8702);
#10990=CIRCLE('',#29005,2.8702);
#10991=CIRCLE('',#29006,2.8702);
#10992=CIRCLE('',#29007,2.8702);
#10993=CIRCLE('',#29008,2.57020000000001);
#10994=CIRCLE('',#29012,2.8702);
#10995=CIRCLE('',#29016,2.8702);
#10996=CIRCLE('',#29020,2.8702);
#10997=CIRCLE('',#29024,2.8702);
#10998=CIRCLE('',#29028,2.8702);
#10999=CIRCLE('',#29032,2.8702);
#11000=CIRCLE('',#29036,2.8702);
#11001=CIRCLE('',#29040,2.8702);
#11002=CIRCLE('',#29044,2.8702);
#11003=CIRCLE('',#29048,2.8702);
#11004=CIRCLE('',#29052,2.8702);
#11005=CIRCLE('',#29056,2.8702);
#11006=CIRCLE('',#29060,2.8702);
#11007=CIRCLE('',#29064,2.8702);
#11008=CIRCLE('',#29068,2.8702);
#11009=CIRCLE('',#29072,2.8702);
#11010=CIRCLE('',#29076,2.8702);
#11011=CIRCLE('',#29077,2.8702);
#11012=CIRCLE('',#29081,2.8702);
#11013=CIRCLE('',#29085,2.8702);
#11014=CIRCLE('',#29089,2.8702);
#11015=CIRCLE('',#29093,2.8702);
#11016=CIRCLE('',#29097,2.8702);
#11017=CIRCLE('',#29101,2.8702);
#11018=CIRCLE('',#29105,2.8702);
#11019=CIRCLE('',#29109,2.8702);
#11020=CIRCLE('',#29113,2.8702);
#11021=CIRCLE('',#29117,2.8702);
#11022=CIRCLE('',#29121,2.8702);
#11023=CIRCLE('',#29125,2.8702);
#11024=CIRCLE('',#29129,2.8702);
#11025=CIRCLE('',#29133,2.8702);
#11026=CIRCLE('',#29137,2.8702);
#11027=CIRCLE('',#29141,2.8702);
#11028=CIRCLE('',#29145,2.8702);
#11029=CIRCLE('',#29149,2.8702);
#11030=CIRCLE('',#29153,1.60395121659244);
#11031=CIRCLE('',#29155,1.60395121659244);
#11032=CIRCLE('',#29157,1.60395121659244);
#11033=CIRCLE('',#29159,1.60395121659244);
#11034=CIRCLE('',#29161,1.60395121659244);
#11035=CIRCLE('',#29163,1.60395121659244);
#11036=CIRCLE('',#29173,1.98119999999999);
#11037=CIRCLE('',#29174,2.08119999999999);
#11038=CIRCLE('',#29176,4.7625);
#11039=CIRCLE('',#29178,4.7625);
#11040=CIRCLE('',#29180,4.6125);
#11041=CIRCLE('',#29182,1.98119999999999);
#11042=CIRCLE('',#29186,1.80249999999999);
#11043=CIRCLE('',#29187,2.05249999999999);
#11044=CIRCLE('',#29189,1.80249999999999);
#11045=CIRCLE('',#29191,3.77031249999999);
#11046=CIRCLE('',#29193,3.59999999999999);
#11047=CIRCLE('',#29194,3.59999999999999);
#11048=CIRCLE('',#29196,3.4);
#11049=CIRCLE('',#29198,1.9);
#11050=CIRCLE('',#29200,1.9);
#11051=VERTEX_POINT('',#36083);
#11052=VERTEX_POINT('',#36085);
#11053=VERTEX_POINT('',#36089);
#11054=VERTEX_POINT('',#36091);
#11055=VERTEX_POINT('',#36095);
#11056=VERTEX_POINT('',#36096);
#11057=VERTEX_POINT('',#36098);
#11058=VERTEX_POINT('',#36100);
#11059=VERTEX_POINT('',#36104);
#11060=VERTEX_POINT('',#36106);
#11061=VERTEX_POINT('',#36110);
#11062=VERTEX_POINT('',#36112);
#11063=VERTEX_POINT('',#36116);
#11064=VERTEX_POINT('',#36117);
#11065=VERTEX_POINT('',#36119);
#11066=VERTEX_POINT('',#36121);
#11067=VERTEX_POINT('',#36125);
#11068=VERTEX_POINT('',#36128);
#11069=VERTEX_POINT('',#36131);
#11070=VERTEX_POINT('',#36133);
#11071=VERTEX_POINT('',#36137);
#11072=VERTEX_POINT('',#36139);
#11073=VERTEX_POINT('',#36143);
#11074=VERTEX_POINT('',#36144);
#11075=VERTEX_POINT('',#36146);
#11076=VERTEX_POINT('',#36148);
#11077=VERTEX_POINT('',#36152);
#11078=VERTEX_POINT('',#36154);
#11079=VERTEX_POINT('',#36158);
#11080=VERTEX_POINT('',#36160);
#11081=VERTEX_POINT('',#36164);
#11082=VERTEX_POINT('',#36165);
#11083=VERTEX_POINT('',#36167);
#11084=VERTEX_POINT('',#36169);
#11085=VERTEX_POINT('',#36173);
#11086=VERTEX_POINT('',#36176);
#11087=VERTEX_POINT('',#36179);
#11088=VERTEX_POINT('',#36181);
#11089=VERTEX_POINT('',#36185);
#11090=VERTEX_POINT('',#36187);
#11091=VERTEX_POINT('',#36191);
#11092=VERTEX_POINT('',#36193);
#11093=VERTEX_POINT('',#36197);
#11094=VERTEX_POINT('',#36199);
#11095=VERTEX_POINT('',#36203);
#11096=VERTEX_POINT('',#36205);
#11097=VERTEX_POINT('',#36209);
#11098=VERTEX_POINT('',#36210);
#11099=VERTEX_POINT('',#36212);
#11100=VERTEX_POINT('',#36214);
#11101=VERTEX_POINT('',#36216);
#11102=VERTEX_POINT('',#36218);
#11103=VERTEX_POINT('',#36220);
#11104=VERTEX_POINT('',#36222);
#11105=VERTEX_POINT('',#36224);
#11106=VERTEX_POINT('',#36226);
#11107=VERTEX_POINT('',#36228);
#11108=VERTEX_POINT('',#36230);
#11109=VERTEX_POINT('',#36232);
#11110=VERTEX_POINT('',#36234);
#11111=VERTEX_POINT('',#36236);
#11112=VERTEX_POINT('',#36238);
#11113=VERTEX_POINT('',#36240);
#11114=VERTEX_POINT('',#36242);
#11115=VERTEX_POINT('',#36244);
#11116=VERTEX_POINT('',#36246);
#11117=VERTEX_POINT('',#36249);
#11118=VERTEX_POINT('',#36251);
#11119=VERTEX_POINT('',#36253);
#11120=VERTEX_POINT('',#36255);
#11121=VERTEX_POINT('',#36258);
#11122=VERTEX_POINT('',#36262);
#11123=VERTEX_POINT('',#36266);
#11124=VERTEX_POINT('',#36270);
#11125=VERTEX_POINT('',#36274);
#11126=VERTEX_POINT('',#36278);
#11127=VERTEX_POINT('',#36282);
#11128=VERTEX_POINT('',#36286);
#11129=VERTEX_POINT('',#36290);
#11130=VERTEX_POINT('',#36294);
#11131=VERTEX_POINT('',#36296);
#11132=VERTEX_POINT('',#36305);
#11133=VERTEX_POINT('',#36306);
#11134=VERTEX_POINT('',#36311);
#11135=VERTEX_POINT('',#36316);
#11136=VERTEX_POINT('',#36322);
#11137=VERTEX_POINT('',#36323);
#11138=VERTEX_POINT('',#36328);
#11139=VERTEX_POINT('',#36332);
#11140=VERTEX_POINT('',#36352);
#11141=VERTEX_POINT('',#36356);
#11142=VERTEX_POINT('',#36362);
#11143=VERTEX_POINT('',#36366);
#11144=VERTEX_POINT('',#36370);
#11145=VERTEX_POINT('',#36376);
#11146=VERTEX_POINT('',#36380);
#11147=VERTEX_POINT('',#36384);
#11148=VERTEX_POINT('',#36388);
#11149=VERTEX_POINT('',#36392);
#11150=VERTEX_POINT('',#36394);
#11151=VERTEX_POINT('',#36398);
#11152=VERTEX_POINT('',#36408);
#11153=VERTEX_POINT('',#36410);
#11154=VERTEX_POINT('',#36420);
#11155=VERTEX_POINT('',#36422);
#11156=VERTEX_POINT('',#36426);
#11157=VERTEX_POINT('',#36427);
#11158=VERTEX_POINT('',#36429);
#11159=VERTEX_POINT('',#36431);
#11160=VERTEX_POINT('',#36433);
#11161=VERTEX_POINT('',#36435);
#11162=VERTEX_POINT('',#36437);
#11163=VERTEX_POINT('',#36439);
#11164=VERTEX_POINT('',#36441);
#11165=VERTEX_POINT('',#36443);
#11166=VERTEX_POINT('',#36445);
#11167=VERTEX_POINT('',#36447);
#11168=VERTEX_POINT('',#36449);
#11169=VERTEX_POINT('',#36451);
#11170=VERTEX_POINT('',#36453);
#11171=VERTEX_POINT('',#36455);
#11172=VERTEX_POINT('',#36457);
#11173=VERTEX_POINT('',#36459);
#11174=VERTEX_POINT('',#36461);
#11175=VERTEX_POINT('',#36463);
#11176=VERTEX_POINT('',#36465);
#11177=VERTEX_POINT('',#36467);
#11178=VERTEX_POINT('',#36469);
#11179=VERTEX_POINT('',#36471);
#11180=VERTEX_POINT('',#36474);
#11181=VERTEX_POINT('',#36476);
#11182=VERTEX_POINT('',#36478);
#11183=VERTEX_POINT('',#36480);
#11184=VERTEX_POINT('',#36482);
#11185=VERTEX_POINT('',#36484);
#11186=VERTEX_POINT('',#36486);
#11187=VERTEX_POINT('',#36487);
#11188=VERTEX_POINT('',#36489);
#11189=VERTEX_POINT('',#36491);
#11190=VERTEX_POINT('',#36493);
#11191=VERTEX_POINT('',#36495);
#11192=VERTEX_POINT('',#36497);
#11193=VERTEX_POINT('',#36499);
#11194=VERTEX_POINT('',#36501);
#11195=VERTEX_POINT('',#36503);
#11196=VERTEX_POINT('',#36505);
#11197=VERTEX_POINT('',#36507);
#11198=VERTEX_POINT('',#36509);
#11199=VERTEX_POINT('',#36511);
#11200=VERTEX_POINT('',#36513);
#11201=VERTEX_POINT('',#36515);
#11202=VERTEX_POINT('',#36518);
#11203=VERTEX_POINT('',#36521);
#11204=VERTEX_POINT('',#36525);
#11205=VERTEX_POINT('',#36529);
#11206=VERTEX_POINT('',#36533);
#11207=VERTEX_POINT('',#36537);
#11208=VERTEX_POINT('',#36541);
#11209=VERTEX_POINT('',#36545);
#11210=VERTEX_POINT('',#36549);
#11211=VERTEX_POINT('',#36551);
#11212=VERTEX_POINT('',#36555);
#11213=VERTEX_POINT('',#36556);
#11214=VERTEX_POINT('',#36558);
#11215=VERTEX_POINT('',#36560);
#11216=VERTEX_POINT('',#36562);
#11217=VERTEX_POINT('',#36564);
#11218=VERTEX_POINT('',#36566);
#11219=VERTEX_POINT('',#36568);
#11220=VERTEX_POINT('',#36570);
#11221=VERTEX_POINT('',#36572);
#11222=VERTEX_POINT('',#36574);
#11223=VERTEX_POINT('',#36576);
#11224=VERTEX_POINT('',#36578);
#11225=VERTEX_POINT('',#36580);
#11226=VERTEX_POINT('',#36582);
#11227=VERTEX_POINT('',#36584);
#11228=VERTEX_POINT('',#36586);
#11229=VERTEX_POINT('',#36588);
#11230=VERTEX_POINT('',#36590);
#11231=VERTEX_POINT('',#36592);
#11232=VERTEX_POINT('',#36594);
#11233=VERTEX_POINT('',#36596);
#11234=VERTEX_POINT('',#36598);
#11235=VERTEX_POINT('',#36600);
#11236=VERTEX_POINT('',#36603);
#11237=VERTEX_POINT('',#36605);
#11238=VERTEX_POINT('',#36606);
#11239=VERTEX_POINT('',#36608);
#11240=VERTEX_POINT('',#36610);
#11241=VERTEX_POINT('',#36612);
#11242=VERTEX_POINT('',#36614);
#11243=VERTEX_POINT('',#36616);
#11244=VERTEX_POINT('',#36618);
#11245=VERTEX_POINT('',#36620);
#11246=VERTEX_POINT('',#36622);
#11247=VERTEX_POINT('',#36624);
#11248=VERTEX_POINT('',#36626);
#11249=VERTEX_POINT('',#36628);
#11250=VERTEX_POINT('',#36630);
#11251=VERTEX_POINT('',#36632);
#11252=VERTEX_POINT('',#36634);
#11253=VERTEX_POINT('',#36637);
#11254=VERTEX_POINT('',#36639);
#11255=VERTEX_POINT('',#36644);
#11256=VERTEX_POINT('',#36650);
#11257=VERTEX_POINT('',#36656);
#11258=VERTEX_POINT('',#36662);
#11259=VERTEX_POINT('',#36664);
#11260=VERTEX_POINT('',#36668);
#11261=VERTEX_POINT('',#36672);
#11262=VERTEX_POINT('',#36676);
#11263=VERTEX_POINT('',#36680);
#11264=VERTEX_POINT('',#36681);
#11265=VERTEX_POINT('',#36686);
#11266=VERTEX_POINT('',#36690);
#11267=VERTEX_POINT('',#36694);
#11268=VERTEX_POINT('',#36698);
#11269=VERTEX_POINT('',#36702);
#11270=VERTEX_POINT('',#36706);
#11271=VERTEX_POINT('',#36710);
#11272=VERTEX_POINT('',#36714);
#11273=VERTEX_POINT('',#36715);
#11274=VERTEX_POINT('',#36720);
#11275=VERTEX_POINT('',#36724);
#11276=VERTEX_POINT('',#36728);
#11277=VERTEX_POINT('',#36734);
#11278=VERTEX_POINT('',#36738);
#11279=VERTEX_POINT('',#36742);
#11280=VERTEX_POINT('',#36748);
#11281=VERTEX_POINT('',#36752);
#11282=VERTEX_POINT('',#36783);
#11283=VERTEX_POINT('',#36784);
#11284=VERTEX_POINT('',#36789);
#11285=VERTEX_POINT('',#36790);
#11286=VERTEX_POINT('',#36795);
#11287=VERTEX_POINT('',#36796);
#11288=VERTEX_POINT('',#36801);
#11289=VERTEX_POINT('',#36807);
#11290=VERTEX_POINT('',#36808);
#11291=VERTEX_POINT('',#36813);
#11292=VERTEX_POINT('',#36817);
#11293=VERTEX_POINT('',#36821);
#11294=VERTEX_POINT('',#36827);
#11295=VERTEX_POINT('',#36831);
#11296=VERTEX_POINT('',#36835);
#11297=VERTEX_POINT('',#36841);
#11298=VERTEX_POINT('',#36903);
#11299=VERTEX_POINT('',#36905);
#11300=VERTEX_POINT('',#36910);
#11301=VERTEX_POINT('',#36912);
#11302=VERTEX_POINT('',#36916);
#11303=VERTEX_POINT('',#36918);
#11304=VERTEX_POINT('',#36922);
#11305=VERTEX_POINT('',#36924);
#11306=VERTEX_POINT('',#36928);
#11307=VERTEX_POINT('',#36930);
#11308=VERTEX_POINT('',#36934);
#11309=VERTEX_POINT('',#36936);
#11310=VERTEX_POINT('',#36940);
#11311=VERTEX_POINT('',#36944);
#11312=VERTEX_POINT('',#36947);
#11313=VERTEX_POINT('',#36950);
#11314=VERTEX_POINT('',#36952);
#11315=VERTEX_POINT('',#36958);
#11316=VERTEX_POINT('',#36960);
#11317=VERTEX_POINT('',#36964);
#11318=VERTEX_POINT('',#36969);
#11319=VERTEX_POINT('',#36970);
#11320=VERTEX_POINT('',#36972);
#11321=VERTEX_POINT('',#36974);
#11322=VERTEX_POINT('',#36978);
#11323=VERTEX_POINT('',#36980);
#11324=VERTEX_POINT('',#36984);
#11325=VERTEX_POINT('',#36985);
#11326=VERTEX_POINT('',#36987);
#11327=VERTEX_POINT('',#36989);
#11328=VERTEX_POINT('',#36993);
#11329=VERTEX_POINT('',#36995);
#11330=VERTEX_POINT('',#36999);
#11331=VERTEX_POINT('',#37001);
#11332=VERTEX_POINT('',#37005);
#11333=VERTEX_POINT('',#37007);
#11334=VERTEX_POINT('',#37014);
#11335=VERTEX_POINT('',#37016);
#11336=VERTEX_POINT('',#37018);
#11337=VERTEX_POINT('',#37020);
#11338=VERTEX_POINT('',#37024);
#11339=VERTEX_POINT('',#37026);
#11340=VERTEX_POINT('',#37028);
#11341=VERTEX_POINT('',#37030);
#11342=VERTEX_POINT('',#37034);
#11343=VERTEX_POINT('',#37035);
#11344=VERTEX_POINT('',#37037);
#11345=VERTEX_POINT('',#37039);
#11346=VERTEX_POINT('',#37041);
#11347=VERTEX_POINT('',#37043);
#11348=VERTEX_POINT('',#37045);
#11349=VERTEX_POINT('',#37047);
#11350=VERTEX_POINT('',#37056);
#11351=VERTEX_POINT('',#37058);
#11352=VERTEX_POINT('',#37062);
#11353=VERTEX_POINT('',#37066);
#11354=VERTEX_POINT('',#37070);
#11355=VERTEX_POINT('',#37074);
#11356=VERTEX_POINT('',#37080);
#11357=VERTEX_POINT('',#37082);
#11358=VERTEX_POINT('',#37086);
#11359=VERTEX_POINT('',#37088);
#11360=VERTEX_POINT('',#37092);
#11361=VERTEX_POINT('',#37093);
#11362=VERTEX_POINT('',#37098);
#11363=VERTEX_POINT('',#37100);
#11364=VERTEX_POINT('',#37104);
#11365=VERTEX_POINT('',#37106);
#11366=VERTEX_POINT('',#37110);
#11367=VERTEX_POINT('',#37115);
#11368=VERTEX_POINT('',#37119);
#11369=VERTEX_POINT('',#37123);
#11370=VERTEX_POINT('',#37132);
#11371=VERTEX_POINT('',#37133);
#11372=VERTEX_POINT('',#37135);
#11373=VERTEX_POINT('',#37137);
#11374=VERTEX_POINT('',#37141);
#11375=VERTEX_POINT('',#37142);
#11376=VERTEX_POINT('',#37144);
#11377=VERTEX_POINT('',#37146);
#11378=VERTEX_POINT('',#37219);
#11379=VERTEX_POINT('',#37255);
#11380=VERTEX_POINT('',#37293);
#11381=VERTEX_POINT('',#37294);
#11382=VERTEX_POINT('',#37439);
#11383=VERTEX_POINT('',#37441);
#11384=VERTEX_POINT('',#37443);
#11385=VERTEX_POINT('',#37479);
#11386=VERTEX_POINT('',#37481);
#11387=VERTEX_POINT('',#37517);
#11388=VERTEX_POINT('',#37519);
#11389=VERTEX_POINT('',#37521);
#11390=VERTEX_POINT('',#37523);
#11391=VERTEX_POINT('',#37559);
#11392=VERTEX_POINT('',#37561);
#11393=VERTEX_POINT('',#37597);
#11394=VERTEX_POINT('',#37599);
#11395=VERTEX_POINT('',#37601);
#11396=VERTEX_POINT('',#37603);
#11397=VERTEX_POINT('',#37639);
#11398=VERTEX_POINT('',#37641);
#11399=VERTEX_POINT('',#37677);
#11400=VERTEX_POINT('',#37679);
#11401=VERTEX_POINT('',#37681);
#11402=VERTEX_POINT('',#37683);
#11403=VERTEX_POINT('',#37719);
#11404=VERTEX_POINT('',#37721);
#11405=VERTEX_POINT('',#37757);
#11406=VERTEX_POINT('',#37759);
#11407=VERTEX_POINT('',#37761);
#11408=VERTEX_POINT('',#37763);
#11409=VERTEX_POINT('',#37799);
#11410=VERTEX_POINT('',#37801);
#11411=VERTEX_POINT('',#37837);
#11412=VERTEX_POINT('',#37839);
#11413=VERTEX_POINT('',#37841);
#11414=VERTEX_POINT('',#37843);
#11415=VERTEX_POINT('',#37879);
#11416=VERTEX_POINT('',#37881);
#11417=VERTEX_POINT('',#37917);
#11418=VERTEX_POINT('',#37919);
#11419=VERTEX_POINT('',#37921);
#11420=VERTEX_POINT('',#37923);
#11421=VERTEX_POINT('',#37959);
#11422=VERTEX_POINT('',#37961);
#11423=VERTEX_POINT('',#37997);
#11424=VERTEX_POINT('',#37999);
#11425=VERTEX_POINT('',#38001);
#11426=VERTEX_POINT('',#38003);
#11427=VERTEX_POINT('',#38039);
#11428=VERTEX_POINT('',#38041);
#11429=VERTEX_POINT('',#38077);
#11430=VERTEX_POINT('',#38079);
#11431=VERTEX_POINT('',#38081);
#11432=VERTEX_POINT('',#38083);
#11433=VERTEX_POINT('',#38119);
#11434=VERTEX_POINT('',#38121);
#11435=VERTEX_POINT('',#38157);
#11436=VERTEX_POINT('',#38159);
#11437=VERTEX_POINT('',#38161);
#11438=VERTEX_POINT('',#38163);
#11439=VERTEX_POINT('',#38199);
#11440=VERTEX_POINT('',#38201);
#11441=VERTEX_POINT('',#38237);
#11442=VERTEX_POINT('',#38239);
#11443=VERTEX_POINT('',#38241);
#11444=VERTEX_POINT('',#38243);
#11445=VERTEX_POINT('',#38279);
#11446=VERTEX_POINT('',#38281);
#11447=VERTEX_POINT('',#38317);
#11448=VERTEX_POINT('',#38319);
#11449=VERTEX_POINT('',#38321);
#11450=VERTEX_POINT('',#38323);
#11451=VERTEX_POINT('',#38359);
#11452=VERTEX_POINT('',#38361);
#11453=VERTEX_POINT('',#38397);
#11454=VERTEX_POINT('',#38399);
#11455=VERTEX_POINT('',#38401);
#11456=VERTEX_POINT('',#38403);
#11457=VERTEX_POINT('',#38439);
#11458=VERTEX_POINT('',#38441);
#11459=VERTEX_POINT('',#38477);
#11460=VERTEX_POINT('',#38479);
#11461=VERTEX_POINT('',#38481);
#11462=VERTEX_POINT('',#38483);
#11463=VERTEX_POINT('',#38519);
#11464=VERTEX_POINT('',#38521);
#11465=VERTEX_POINT('',#38557);
#11466=VERTEX_POINT('',#38559);
#11467=VERTEX_POINT('',#38561);
#11468=VERTEX_POINT('',#38563);
#11469=VERTEX_POINT('',#38599);
#11470=VERTEX_POINT('',#38601);
#11471=VERTEX_POINT('',#38637);
#11472=VERTEX_POINT('',#38640);
#11473=VERTEX_POINT('',#38643);
#11474=VERTEX_POINT('',#38647);
#11475=VERTEX_POINT('',#38651);
#11476=VERTEX_POINT('',#38653);
#11477=VERTEX_POINT('',#38726);
#11478=VERTEX_POINT('',#38764);
#11479=VERTEX_POINT('',#38873);
#11480=VERTEX_POINT('',#38877);
#11481=VERTEX_POINT('',#38881);
#11482=VERTEX_POINT('',#38883);
#11483=VERTEX_POINT('',#38956);
#11484=VERTEX_POINT('',#38994);
#11485=VERTEX_POINT('',#39103);
#11486=VERTEX_POINT('',#39107);
#11487=VERTEX_POINT('',#39111);
#11488=VERTEX_POINT('',#39113);
#11489=VERTEX_POINT('',#39186);
#11490=VERTEX_POINT('',#39224);
#11491=VERTEX_POINT('',#39333);
#11492=VERTEX_POINT('',#39337);
#11493=VERTEX_POINT('',#39341);
#11494=VERTEX_POINT('',#39343);
#11495=VERTEX_POINT('',#39416);
#11496=VERTEX_POINT('',#39454);
#11497=VERTEX_POINT('',#39563);
#11498=VERTEX_POINT('',#39567);
#11499=VERTEX_POINT('',#39571);
#11500=VERTEX_POINT('',#39573);
#11501=VERTEX_POINT('',#39646);
#11502=VERTEX_POINT('',#39684);
#11503=VERTEX_POINT('',#39793);
#11504=VERTEX_POINT('',#39797);
#11505=VERTEX_POINT('',#39801);
#11506=VERTEX_POINT('',#39803);
#11507=VERTEX_POINT('',#39876);
#11508=VERTEX_POINT('',#39914);
#11509=VERTEX_POINT('',#40023);
#11510=VERTEX_POINT('',#40027);
#11511=VERTEX_POINT('',#40031);
#11512=VERTEX_POINT('',#40033);
#11513=VERTEX_POINT('',#40106);
#11514=VERTEX_POINT('',#40144);
#11515=VERTEX_POINT('',#40253);
#11516=VERTEX_POINT('',#40257);
#11517=VERTEX_POINT('',#40261);
#11518=VERTEX_POINT('',#40263);
#11519=VERTEX_POINT('',#40336);
#11520=VERTEX_POINT('',#40374);
#11521=VERTEX_POINT('',#40483);
#11522=VERTEX_POINT('',#40487);
#11523=VERTEX_POINT('',#40491);
#11524=VERTEX_POINT('',#40493);
#11525=VERTEX_POINT('',#40566);
#11526=VERTEX_POINT('',#40604);
#11527=VERTEX_POINT('',#40713);
#11528=VERTEX_POINT('',#40717);
#11529=VERTEX_POINT('',#40721);
#11530=VERTEX_POINT('',#40723);
#11531=VERTEX_POINT('',#40796);
#11532=VERTEX_POINT('',#40834);
#11533=VERTEX_POINT('',#40943);
#11534=VERTEX_POINT('',#40947);
#11535=VERTEX_POINT('',#40951);
#11536=VERTEX_POINT('',#40953);
#11537=VERTEX_POINT('',#41026);
#11538=VERTEX_POINT('',#41064);
#11539=VERTEX_POINT('',#41173);
#11540=VERTEX_POINT('',#41177);
#11541=VERTEX_POINT('',#41181);
#11542=VERTEX_POINT('',#41183);
#11543=VERTEX_POINT('',#41256);
#11544=VERTEX_POINT('',#41294);
#11545=VERTEX_POINT('',#41403);
#11546=VERTEX_POINT('',#41407);
#11547=VERTEX_POINT('',#41411);
#11548=VERTEX_POINT('',#41413);
#11549=VERTEX_POINT('',#41486);
#11550=VERTEX_POINT('',#41524);
#11551=VERTEX_POINT('',#41633);
#11552=VERTEX_POINT('',#41637);
#11553=VERTEX_POINT('',#41639);
#11554=VERTEX_POINT('',#41643);
#11555=VERTEX_POINT('',#41647);
#11556=VERTEX_POINT('',#41649);
#11557=VERTEX_POINT('',#41863);
#11558=VERTEX_POINT('',#41865);
#11559=VERTEX_POINT('',#41867);
#11560=VERTEX_POINT('',#41903);
#11561=VERTEX_POINT('',#41905);
#11562=VERTEX_POINT('',#41941);
#11563=VERTEX_POINT('',#41944);
#11564=VERTEX_POINT('',#42098);
#11565=VERTEX_POINT('',#42100);
#11566=VERTEX_POINT('',#42103);
#11567=VERTEX_POINT('',#42107);
#11568=VERTEX_POINT('',#42115);
#11569=VERTEX_POINT('',#42116);
#11570=VERTEX_POINT('',#42118);
#11571=VERTEX_POINT('',#42216);
#11572=VERTEX_POINT('',#42280);
#11573=VERTEX_POINT('',#42281);
#11574=VERTEX_POINT('',#42283);
#11575=VERTEX_POINT('',#42341);
#11576=VERTEX_POINT('',#42524);
#11577=VERTEX_POINT('',#42525);
#11578=VERTEX_POINT('',#42527);
#11579=VERTEX_POINT('',#42837);
#11580=VERTEX_POINT('',#42838);
#11581=VERTEX_POINT('',#42840);
#11582=VERTEX_POINT('',#43026);
#11583=VERTEX_POINT('',#43220);
#11584=VERTEX_POINT('',#43221);
#11585=VERTEX_POINT('',#43576);
#11586=VERTEX_POINT('',#43577);
#11587=VERTEX_POINT('',#43579);
#11588=VERTEX_POINT('',#43770);
#11589=VERTEX_POINT('',#43952);
#11590=VERTEX_POINT('',#43953);
#11591=VERTEX_POINT('',#44324);
#11592=VERTEX_POINT('',#44325);
#11593=VERTEX_POINT('',#44327);
#11594=VERTEX_POINT('',#44390);
#11595=VERTEX_POINT('',#44572);
#11596=VERTEX_POINT('',#44573);
#11597=VERTEX_POINT('',#44575);
#11598=VERTEX_POINT('',#44901);
#11599=VERTEX_POINT('',#44902);
#11600=VERTEX_POINT('',#45082);
#11601=VERTEX_POINT('',#45262);
#11602=VERTEX_POINT('',#45263);
#11603=VERTEX_POINT('',#45265);
#11604=VERTEX_POINT('',#45448);
#11605=VERTEX_POINT('',#45505);
#11606=VERTEX_POINT('',#45506);
#11607=VERTEX_POINT('',#45508);
#11608=VERTEX_POINT('',#45567);
#11609=VERTEX_POINT('',#45575);
#11610=VERTEX_POINT('',#45576);
#11611=VERTEX_POINT('',#45923);
#11612=VERTEX_POINT('',#45924);
#11613=VERTEX_POINT('',#46109);
#11614=VERTEX_POINT('',#46110);
#11615=VERTEX_POINT('',#46457);
#11616=VERTEX_POINT('',#46458);
#11617=VERTEX_POINT('',#46805);
#11618=VERTEX_POINT('',#46806);
#11619=VERTEX_POINT('',#46991);
#11620=VERTEX_POINT('',#46992);
#11621=VERTEX_POINT('',#47177);
#11622=VERTEX_POINT('',#47178);
#11623=VERTEX_POINT('',#47525);
#11624=VERTEX_POINT('',#47526);
#11625=VERTEX_POINT('',#47711);
#11626=VERTEX_POINT('',#47712);
#11627=VERTEX_POINT('',#48059);
#11628=VERTEX_POINT('',#48060);
#11629=VERTEX_POINT('',#48407);
#11630=VERTEX_POINT('',#48568);
#11631=VERTEX_POINT('',#48579);
#11632=VERTEX_POINT('',#48586);
#11633=VERTEX_POINT('',#48663);
#11634=VERTEX_POINT('',#48665);
#11635=VERTEX_POINT('',#48756);
#11636=VERTEX_POINT('',#48757);
#11637=VERTEX_POINT('',#49311);
#11638=VERTEX_POINT('',#49312);
#11639=VERTEX_POINT('',#49702);
#11640=VERTEX_POINT('',#49706);
#11641=VERTEX_POINT('',#49709);
#11642=VERTEX_POINT('',#49714);
#11643=VERTEX_POINT('',#49715);
#11644=VERTEX_POINT('',#49719);
#11645=VERTEX_POINT('',#49721);
#11646=VERTEX_POINT('',#49725);
#11647=VERTEX_POINT('',#49729);
#11648=VERTEX_POINT('',#49735);
#11649=VERTEX_POINT('',#49736);
#11650=VERTEX_POINT('',#49738);
#11651=VERTEX_POINT('',#49740);
#11652=VERTEX_POINT('',#49743);
#11653=VERTEX_POINT('',#49745);
#11654=VERTEX_POINT('',#49747);
#11655=VERTEX_POINT('',#49749);
#11656=VERTEX_POINT('',#49751);
#11657=VERTEX_POINT('',#49753);
#11658=VERTEX_POINT('',#49755);
#11659=VERTEX_POINT('',#49757);
#11660=VERTEX_POINT('',#49759);
#11661=VERTEX_POINT('',#49761);
#11662=VERTEX_POINT('',#49763);
#11663=VERTEX_POINT('',#49765);
#11664=VERTEX_POINT('',#49767);
#11665=VERTEX_POINT('',#49769);
#11666=VERTEX_POINT('',#49771);
#11667=VERTEX_POINT('',#49773);
#11668=VERTEX_POINT('',#49775);
#11669=VERTEX_POINT('',#49777);
#11670=VERTEX_POINT('',#49779);
#11671=VERTEX_POINT('',#49781);
#11672=VERTEX_POINT('',#49783);
#11673=VERTEX_POINT('',#49785);
#11674=VERTEX_POINT('',#49787);
#11675=VERTEX_POINT('',#49789);
#11676=VERTEX_POINT('',#49791);
#11677=VERTEX_POINT('',#49793);
#11678=VERTEX_POINT('',#49795);
#11679=VERTEX_POINT('',#49797);
#11680=VERTEX_POINT('',#49799);
#11681=VERTEX_POINT('',#49801);
#11682=VERTEX_POINT('',#49803);
#11683=VERTEX_POINT('',#49805);
#11684=VERTEX_POINT('',#49807);
#11685=VERTEX_POINT('',#49809);
#11686=VERTEX_POINT('',#49811);
#11687=VERTEX_POINT('',#49813);
#11688=VERTEX_POINT('',#49815);
#11689=VERTEX_POINT('',#49817);
#11690=VERTEX_POINT('',#49819);
#11691=VERTEX_POINT('',#49821);
#11692=VERTEX_POINT('',#49823);
#11693=VERTEX_POINT('',#49825);
#11694=VERTEX_POINT('',#49827);
#11695=VERTEX_POINT('',#49829);
#11696=VERTEX_POINT('',#49831);
#11697=VERTEX_POINT('',#49833);
#11698=VERTEX_POINT('',#49835);
#11699=VERTEX_POINT('',#49837);
#11700=VERTEX_POINT('',#49839);
#11701=VERTEX_POINT('',#49841);
#11702=VERTEX_POINT('',#49843);
#11703=VERTEX_POINT('',#49845);
#11704=VERTEX_POINT('',#49847);
#11705=VERTEX_POINT('',#49849);
#11706=VERTEX_POINT('',#49851);
#11707=VERTEX_POINT('',#49853);
#11708=VERTEX_POINT('',#49855);
#11709=VERTEX_POINT('',#49857);
#11710=VERTEX_POINT('',#49859);
#11711=VERTEX_POINT('',#49861);
#11712=VERTEX_POINT('',#49863);
#11713=VERTEX_POINT('',#49865);
#11714=VERTEX_POINT('',#49867);
#11715=VERTEX_POINT('',#49869);
#11716=VERTEX_POINT('',#49871);
#11717=VERTEX_POINT('',#49873);
#11718=VERTEX_POINT('',#49876);
#11719=VERTEX_POINT('',#49878);
#11720=VERTEX_POINT('',#49880);
#11721=VERTEX_POINT('',#49882);
#11722=VERTEX_POINT('',#49884);
#11723=VERTEX_POINT('',#49886);
#11724=VERTEX_POINT('',#49888);
#11725=VERTEX_POINT('',#49890);
#11726=VERTEX_POINT('',#49892);
#11727=VERTEX_POINT('',#49894);
#11728=VERTEX_POINT('',#49896);
#11729=VERTEX_POINT('',#49898);
#11730=VERTEX_POINT('',#49900);
#11731=VERTEX_POINT('',#49902);
#11732=VERTEX_POINT('',#49904);
#11733=VERTEX_POINT('',#49906);
#11734=VERTEX_POINT('',#49908);
#11735=VERTEX_POINT('',#49910);
#11736=VERTEX_POINT('',#49912);
#11737=VERTEX_POINT('',#49914);
#11738=VERTEX_POINT('',#49916);
#11739=VERTEX_POINT('',#49918);
#11740=VERTEX_POINT('',#49920);
#11741=VERTEX_POINT('',#49922);
#11742=VERTEX_POINT('',#49924);
#11743=VERTEX_POINT('',#49926);
#11744=VERTEX_POINT('',#49928);
#11745=VERTEX_POINT('',#49930);
#11746=VERTEX_POINT('',#49932);
#11747=VERTEX_POINT('',#49934);
#11748=VERTEX_POINT('',#49936);
#11749=VERTEX_POINT('',#49938);
#11750=VERTEX_POINT('',#49940);
#11751=VERTEX_POINT('',#49942);
#11752=VERTEX_POINT('',#49944);
#11753=VERTEX_POINT('',#49946);
#11754=VERTEX_POINT('',#49948);
#11755=VERTEX_POINT('',#49950);
#11756=VERTEX_POINT('',#49952);
#11757=VERTEX_POINT('',#49954);
#11758=VERTEX_POINT('',#49956);
#11759=VERTEX_POINT('',#49958);
#11760=VERTEX_POINT('',#49960);
#11761=VERTEX_POINT('',#49962);
#11762=VERTEX_POINT('',#49964);
#11763=VERTEX_POINT('',#49966);
#11764=VERTEX_POINT('',#49968);
#11765=VERTEX_POINT('',#49970);
#11766=VERTEX_POINT('',#49972);
#11767=VERTEX_POINT('',#49974);
#11768=VERTEX_POINT('',#49976);
#11769=VERTEX_POINT('',#49978);
#11770=VERTEX_POINT('',#49980);
#11771=VERTEX_POINT('',#49982);
#11772=VERTEX_POINT('',#49984);
#11773=VERTEX_POINT('',#49986);
#11774=VERTEX_POINT('',#49988);
#11775=VERTEX_POINT('',#49990);
#11776=VERTEX_POINT('',#49992);
#11777=VERTEX_POINT('',#49994);
#11778=VERTEX_POINT('',#49996);
#11779=VERTEX_POINT('',#49998);
#11780=VERTEX_POINT('',#50000);
#11781=VERTEX_POINT('',#50002);
#11782=VERTEX_POINT('',#50004);
#11783=VERTEX_POINT('',#50006);
#11784=VERTEX_POINT('',#50008);
#11785=VERTEX_POINT('',#50010);
#11786=VERTEX_POINT('',#50012);
#11787=VERTEX_POINT('',#50014);
#11788=VERTEX_POINT('',#50016);
#11789=VERTEX_POINT('',#50018);
#11790=VERTEX_POINT('',#50020);
#11791=VERTEX_POINT('',#50024);
#11792=VERTEX_POINT('',#50028);
#11793=VERTEX_POINT('',#50038);
#11794=VERTEX_POINT('',#50042);
#11795=VERTEX_POINT('',#50052);
#11796=VERTEX_POINT('',#50056);
#11797=VERTEX_POINT('',#50066);
#11798=VERTEX_POINT('',#50070);
#11799=VERTEX_POINT('',#50080);
#11800=VERTEX_POINT('',#50084);
#11801=VERTEX_POINT('',#50094);
#11802=VERTEX_POINT('',#50098);
#11803=VERTEX_POINT('',#50108);
#11804=VERTEX_POINT('',#50112);
#11805=VERTEX_POINT('',#50122);
#11806=VERTEX_POINT('',#50126);
#11807=VERTEX_POINT('',#50136);
#11808=VERTEX_POINT('',#50140);
#11809=VERTEX_POINT('',#50150);
#11810=VERTEX_POINT('',#50154);
#11811=VERTEX_POINT('',#50164);
#11812=VERTEX_POINT('',#50168);
#11813=VERTEX_POINT('',#50178);
#11814=VERTEX_POINT('',#50182);
#11815=VERTEX_POINT('',#50192);
#11816=VERTEX_POINT('',#50196);
#11817=VERTEX_POINT('',#50206);
#11818=VERTEX_POINT('',#50210);
#11819=VERTEX_POINT('',#50220);
#11820=VERTEX_POINT('',#50224);
#11821=VERTEX_POINT('',#50234);
#11822=VERTEX_POINT('',#50238);
#11823=VERTEX_POINT('',#50248);
#11824=VERTEX_POINT('',#50252);
#11825=VERTEX_POINT('',#50262);
#11826=VERTEX_POINT('',#50266);
#11827=VERTEX_POINT('',#50276);
#11828=VERTEX_POINT('',#50280);
#11829=VERTEX_POINT('',#50290);
#11830=VERTEX_POINT('',#50294);
#11831=VERTEX_POINT('',#50304);
#11832=VERTEX_POINT('',#50308);
#11833=VERTEX_POINT('',#50318);
#11834=VERTEX_POINT('',#50322);
#11835=VERTEX_POINT('',#50332);
#11836=VERTEX_POINT('',#50336);
#11837=VERTEX_POINT('',#50346);
#11838=VERTEX_POINT('',#50350);
#11839=VERTEX_POINT('',#50360);
#11840=VERTEX_POINT('',#50364);
#11841=VERTEX_POINT('',#50374);
#11842=VERTEX_POINT('',#50378);
#11843=VERTEX_POINT('',#50388);
#11844=VERTEX_POINT('',#50392);
#11845=VERTEX_POINT('',#50402);
#11846=VERTEX_POINT('',#50406);
#11847=VERTEX_POINT('',#50416);
#11848=VERTEX_POINT('',#50420);
#11849=VERTEX_POINT('',#50430);
#11850=VERTEX_POINT('',#50434);
#11851=VERTEX_POINT('',#50444);
#11852=VERTEX_POINT('',#50448);
#11853=VERTEX_POINT('',#50458);
#11854=VERTEX_POINT('',#50462);
#11855=VERTEX_POINT('',#50472);
#11856=VERTEX_POINT('',#50476);
#11857=VERTEX_POINT('',#50486);
#11858=VERTEX_POINT('',#50490);
#11859=VERTEX_POINT('',#50500);
#11860=VERTEX_POINT('',#50504);
#11861=VERTEX_POINT('',#50516);
#11862=VERTEX_POINT('',#50520);
#11863=VERTEX_POINT('',#50523);
#11864=VERTEX_POINT('',#50524);
#11865=VERTEX_POINT('',#50528);
#11866=VERTEX_POINT('',#50530);
#11867=VERTEX_POINT('',#50534);
#11868=VERTEX_POINT('',#50538);
#11869=VERTEX_POINT('',#50540);
#11870=VERTEX_POINT('',#50544);
#11871=VERTEX_POINT('',#50548);
#11872=VERTEX_POINT('',#50550);
#11873=VERTEX_POINT('',#50554);
#11874=VERTEX_POINT('',#50558);
#11875=VERTEX_POINT('',#50560);
#11876=VERTEX_POINT('',#50564);
#11877=VERTEX_POINT('',#50568);
#11878=VERTEX_POINT('',#50570);
#11879=VERTEX_POINT('',#50574);
#11880=VERTEX_POINT('',#50578);
#11881=VERTEX_POINT('',#50585);
#11882=VERTEX_POINT('',#50587);
#11883=VERTEX_POINT('',#50591);
#11884=VERTEX_POINT('',#50593);
#11885=VERTEX_POINT('',#50597);
#11886=VERTEX_POINT('',#50599);
#11887=VERTEX_POINT('',#50603);
#11888=VERTEX_POINT('',#50605);
#11889=VERTEX_POINT('',#50609);
#11890=VERTEX_POINT('',#50611);
#11891=VERTEX_POINT('',#50615);
#11892=VERTEX_POINT('',#50617);
#11893=VERTEX_POINT('',#50622);
#11894=VERTEX_POINT('',#50624);
#11895=VERTEX_POINT('',#50629);
#11896=VERTEX_POINT('',#50634);
#11897=VERTEX_POINT('',#50647);
#11898=VERTEX_POINT('',#50657);
#11899=VERTEX_POINT('',#50664);
#11900=VERTEX_POINT('',#50673);
#11901=VERTEX_POINT('',#50675);
#11902=VERTEX_POINT('',#50679);
#11903=VERTEX_POINT('',#50680);
#11904=VERTEX_POINT('',#50682);
#11905=VERTEX_POINT('',#50684);
#11906=VERTEX_POINT('',#50687);
#11907=VERTEX_POINT('',#50689);
#11908=VERTEX_POINT('',#50691);
#11909=VERTEX_POINT('',#50693);
#11910=VERTEX_POINT('',#50695);
#11911=VERTEX_POINT('',#50697);
#11912=VERTEX_POINT('',#50699);
#11913=VERTEX_POINT('',#50701);
#11914=VERTEX_POINT('',#50703);
#11915=VERTEX_POINT('',#50705);
#11916=VERTEX_POINT('',#50707);
#11917=VERTEX_POINT('',#50709);
#11918=VERTEX_POINT('',#50711);
#11919=VERTEX_POINT('',#50713);
#11920=VERTEX_POINT('',#50715);
#11921=VERTEX_POINT('',#50717);
#11922=VERTEX_POINT('',#50719);
#11923=VERTEX_POINT('',#50721);
#11924=VERTEX_POINT('',#50723);
#11925=VERTEX_POINT('',#50725);
#11926=VERTEX_POINT('',#50728);
#11927=VERTEX_POINT('',#50732);
#11928=VERTEX_POINT('',#50736);
#11929=VERTEX_POINT('',#50740);
#11930=VERTEX_POINT('',#50744);
#11931=VERTEX_POINT('',#50748);
#11932=VERTEX_POINT('',#50752);
#11933=VERTEX_POINT('',#50756);
#11934=VERTEX_POINT('',#50760);
#11935=VERTEX_POINT('',#50764);
#11936=VERTEX_POINT('',#50768);
#11937=VERTEX_POINT('',#50772);
#11938=VERTEX_POINT('',#50776);
#11939=VERTEX_POINT('',#50780);
#11940=VERTEX_POINT('',#50784);
#11941=VERTEX_POINT('',#50788);
#11942=VERTEX_POINT('',#50792);
#11943=VERTEX_POINT('',#50796);
#11944=VERTEX_POINT('',#50800);
#11945=VERTEX_POINT('',#50804);
#11946=VERTEX_POINT('',#50808);
#11947=VERTEX_POINT('',#50812);
#11948=VERTEX_POINT('',#50816);
#11949=VERTEX_POINT('',#50820);
#11950=VERTEX_POINT('',#50824);
#11951=VERTEX_POINT('',#50828);
#11952=VERTEX_POINT('',#50832);
#11953=VERTEX_POINT('',#50836);
#11954=VERTEX_POINT('',#50840);
#11955=VERTEX_POINT('',#50844);
#11956=VERTEX_POINT('',#50848);
#11957=VERTEX_POINT('',#50852);
#11958=VERTEX_POINT('',#50856);
#11959=VERTEX_POINT('',#50860);
#11960=VERTEX_POINT('',#50864);
#11961=VERTEX_POINT('',#50868);
#11962=VERTEX_POINT('',#50872);
#11963=VERTEX_POINT('',#50876);
#11964=VERTEX_POINT('',#50880);
#11965=VERTEX_POINT('',#50884);
#11966=VERTEX_POINT('',#50888);
#11967=VERTEX_POINT('',#50892);
#11968=VERTEX_POINT('',#50894);
#11969=VERTEX_POINT('',#50898);
#11970=VERTEX_POINT('',#50902);
#11971=VERTEX_POINT('',#50908);
#11972=VERTEX_POINT('',#50910);
#11973=VERTEX_POINT('',#50914);
#11974=VERTEX_POINT('',#50918);
#11975=VERTEX_POINT('',#50920);
#11976=VERTEX_POINT('',#50924);
#11977=VERTEX_POINT('',#50926);
#11978=VERTEX_POINT('',#50930);
#11979=VERTEX_POINT('',#50942);
#11980=VERTEX_POINT('',#50943);
#11981=VERTEX_POINT('',#50945);
#11982=VERTEX_POINT('',#50947);
#11983=VERTEX_POINT('',#50951);
#11984=VERTEX_POINT('',#50952);
#11985=VERTEX_POINT('',#50957);
#11986=VERTEX_POINT('',#50958);
#11987=VERTEX_POINT('',#50963);
#11988=VERTEX_POINT('',#50964);
#11989=VERTEX_POINT('',#50969);
#11990=VERTEX_POINT('',#50970);
#11991=VERTEX_POINT('',#50975);
#11992=VERTEX_POINT('',#50977);
#11993=VERTEX_POINT('',#50981);
#11994=VERTEX_POINT('',#50985);
#11995=VERTEX_POINT('',#50989);
#11996=VERTEX_POINT('',#50993);
#11997=VERTEX_POINT('',#50997);
#11998=VERTEX_POINT('',#50999);
#11999=VERTEX_POINT('',#51003);
#12000=VERTEX_POINT('',#51007);
#12001=VERTEX_POINT('',#51011);
#12002=VERTEX_POINT('',#51015);
#12003=VERTEX_POINT('',#51019);
#12004=VERTEX_POINT('',#51021);
#12005=VERTEX_POINT('',#51025);
#12006=VERTEX_POINT('',#51027);
#12007=VERTEX_POINT('',#51031);
#12008=VERTEX_POINT('',#51033);
#12009=VERTEX_POINT('',#51037);
#12010=VERTEX_POINT('',#51039);
#12011=VERTEX_POINT('',#51043);
#12012=VERTEX_POINT('',#51045);
#12013=VERTEX_POINT('',#51049);
#12014=VERTEX_POINT('',#51051);
#12015=VERTEX_POINT('',#51055);
#12016=VERTEX_POINT('',#51057);
#12017=VERTEX_POINT('',#51061);
#12018=VERTEX_POINT('',#51063);
#12019=VERTEX_POINT('',#51067);
#12020=VERTEX_POINT('',#51069);
#12021=VERTEX_POINT('',#51073);
#12022=VERTEX_POINT('',#51075);
#12023=VERTEX_POINT('',#51079);
#12024=VERTEX_POINT('',#51081);
#12025=VERTEX_POINT('',#51085);
#12026=VERTEX_POINT('',#51087);
#12027=VERTEX_POINT('',#51091);
#12028=VERTEX_POINT('',#51093);
#12029=VERTEX_POINT('',#51097);
#12030=VERTEX_POINT('',#51099);
#12031=VERTEX_POINT('',#51103);
#12032=VERTEX_POINT('',#51105);
#12033=VERTEX_POINT('',#51109);
#12034=VERTEX_POINT('',#51111);
#12035=VERTEX_POINT('',#51115);
#12036=VERTEX_POINT('',#51117);
#12037=VERTEX_POINT('',#51121);
#12038=VERTEX_POINT('',#51123);
#12039=VERTEX_POINT('',#51127);
#12040=VERTEX_POINT('',#51129);
#12041=VERTEX_POINT('',#51133);
#12042=VERTEX_POINT('',#51135);
#12043=VERTEX_POINT('',#51139);
#12044=VERTEX_POINT('',#51141);
#12045=VERTEX_POINT('',#51145);
#12046=VERTEX_POINT('',#51147);
#12047=VERTEX_POINT('',#51151);
#12048=VERTEX_POINT('',#51153);
#12049=VERTEX_POINT('',#51157);
#12050=VERTEX_POINT('',#51159);
#12051=VERTEX_POINT('',#51163);
#12052=VERTEX_POINT('',#51165);
#12053=VERTEX_POINT('',#51169);
#12054=VERTEX_POINT('',#51171);
#12055=VERTEX_POINT('',#51175);
#12056=VERTEX_POINT('',#51177);
#12057=VERTEX_POINT('',#51181);
#12058=VERTEX_POINT('',#51183);
#12059=VERTEX_POINT('',#51187);
#12060=VERTEX_POINT('',#51189);
#12061=VERTEX_POINT('',#51193);
#12062=VERTEX_POINT('',#51195);
#12063=VERTEX_POINT('',#51199);
#12064=VERTEX_POINT('',#51201);
#12065=VERTEX_POINT('',#51205);
#12066=VERTEX_POINT('',#51207);
#12067=VERTEX_POINT('',#51211);
#12068=VERTEX_POINT('',#51213);
#12069=VERTEX_POINT('',#51217);
#12070=VERTEX_POINT('',#51219);
#12071=VERTEX_POINT('',#51223);
#12072=VERTEX_POINT('',#51225);
#12073=VERTEX_POINT('',#51229);
#12074=VERTEX_POINT('',#51231);
#12075=VERTEX_POINT('',#51235);
#12076=VERTEX_POINT('',#51237);
#12077=VERTEX_POINT('',#51241);
#12078=VERTEX_POINT('',#51243);
#12079=VERTEX_POINT('',#51247);
#12080=VERTEX_POINT('',#51249);
#12081=VERTEX_POINT('',#51253);
#12082=VERTEX_POINT('',#51255);
#12083=VERTEX_POINT('',#51259);
#12084=VERTEX_POINT('',#51261);
#12085=VERTEX_POINT('',#51265);
#12086=VERTEX_POINT('',#51267);
#12087=VERTEX_POINT('',#51271);
#12088=VERTEX_POINT('',#51273);
#12089=VERTEX_POINT('',#51277);
#12090=VERTEX_POINT('',#51279);
#12091=VERTEX_POINT('',#51283);
#12092=VERTEX_POINT('',#51285);
#12093=VERTEX_POINT('',#51289);
#12094=VERTEX_POINT('',#51291);
#12095=VERTEX_POINT('',#51295);
#12096=VERTEX_POINT('',#51297);
#12097=VERTEX_POINT('',#51301);
#12098=VERTEX_POINT('',#51303);
#12099=VERTEX_POINT('',#51307);
#12100=VERTEX_POINT('',#51309);
#12101=VERTEX_POINT('',#51313);
#12102=VERTEX_POINT('',#51315);
#12103=VERTEX_POINT('',#51319);
#12104=VERTEX_POINT('',#51321);
#12105=VERTEX_POINT('',#51325);
#12106=VERTEX_POINT('',#51327);
#12107=VERTEX_POINT('',#51331);
#12108=VERTEX_POINT('',#51333);
#12109=VERTEX_POINT('',#51337);
#12110=VERTEX_POINT('',#51339);
#12111=VERTEX_POINT('',#51343);
#12112=VERTEX_POINT('',#51345);
#12113=VERTEX_POINT('',#51349);
#12114=VERTEX_POINT('',#51351);
#12115=VERTEX_POINT('',#51355);
#12116=VERTEX_POINT('',#51357);
#12117=VERTEX_POINT('',#51361);
#12118=VERTEX_POINT('',#51363);
#12119=VERTEX_POINT('',#51367);
#12120=VERTEX_POINT('',#51369);
#12121=VERTEX_POINT('',#51373);
#12122=VERTEX_POINT('',#51375);
#12123=VERTEX_POINT('',#51379);
#12124=VERTEX_POINT('',#51381);
#12125=VERTEX_POINT('',#51385);
#12126=VERTEX_POINT('',#51387);
#12127=VERTEX_POINT('',#51391);
#12128=VERTEX_POINT('',#51393);
#12129=VERTEX_POINT('',#51397);
#12130=VERTEX_POINT('',#51399);
#12131=VERTEX_POINT('',#51403);
#12132=VERTEX_POINT('',#51405);
#12133=VERTEX_POINT('',#51409);
#12134=VERTEX_POINT('',#51411);
#12135=VERTEX_POINT('',#51415);
#12136=VERTEX_POINT('',#51417);
#12137=VERTEX_POINT('',#51421);
#12138=VERTEX_POINT('',#51423);
#12139=VERTEX_POINT('',#51427);
#12140=VERTEX_POINT('',#51429);
#12141=VERTEX_POINT('',#51433);
#12142=VERTEX_POINT('',#51435);
#12143=VERTEX_POINT('',#51439);
#12144=VERTEX_POINT('',#51441);
#12145=VERTEX_POINT('',#51445);
#12146=VERTEX_POINT('',#51447);
#12147=VERTEX_POINT('',#51451);
#12148=VERTEX_POINT('',#51453);
#12149=VERTEX_POINT('',#51457);
#12150=VERTEX_POINT('',#51459);
#12151=VERTEX_POINT('',#51463);
#12152=VERTEX_POINT('',#51465);
#12153=VERTEX_POINT('',#51469);
#12154=VERTEX_POINT('',#51471);
#12155=VERTEX_POINT('',#51475);
#12156=VERTEX_POINT('',#51477);
#12157=VERTEX_POINT('',#51481);
#12158=VERTEX_POINT('',#51483);
#12159=VERTEX_POINT('',#51487);
#12160=VERTEX_POINT('',#51489);
#12161=VERTEX_POINT('',#51493);
#12162=VERTEX_POINT('',#51495);
#12163=VERTEX_POINT('',#51499);
#12164=VERTEX_POINT('',#51501);
#12165=VERTEX_POINT('',#51505);
#12166=VERTEX_POINT('',#51507);
#12167=VERTEX_POINT('',#51511);
#12168=VERTEX_POINT('',#51513);
#12169=VERTEX_POINT('',#51517);
#12170=VERTEX_POINT('',#51519);
#12171=VERTEX_POINT('',#51523);
#12172=VERTEX_POINT('',#51525);
#12173=VERTEX_POINT('',#51529);
#12174=VERTEX_POINT('',#51531);
#12175=VERTEX_POINT('',#51535);
#12176=VERTEX_POINT('',#51537);
#12177=VERTEX_POINT('',#51541);
#12178=VERTEX_POINT('',#51543);
#12179=VERTEX_POINT('',#51547);
#12180=VERTEX_POINT('',#51549);
#12181=VERTEX_POINT('',#51553);
#12182=VERTEX_POINT('',#51555);
#12183=VERTEX_POINT('',#51559);
#12184=VERTEX_POINT('',#51561);
#12185=VERTEX_POINT('',#51565);
#12186=VERTEX_POINT('',#51567);
#12187=VERTEX_POINT('',#51571);
#12188=VERTEX_POINT('',#51573);
#12189=VERTEX_POINT('',#51577);
#12190=VERTEX_POINT('',#51579);
#12191=VERTEX_POINT('',#51583);
#12192=VERTEX_POINT('',#51585);
#12193=VERTEX_POINT('',#51589);
#12194=VERTEX_POINT('',#51591);
#12195=VERTEX_POINT('',#51595);
#12196=VERTEX_POINT('',#51597);
#12197=VERTEX_POINT('',#51601);
#12198=VERTEX_POINT('',#51603);
#12199=VERTEX_POINT('',#51607);
#12200=VERTEX_POINT('',#51609);
#12201=VERTEX_POINT('',#51613);
#12202=VERTEX_POINT('',#51615);
#12203=VERTEX_POINT('',#51619);
#12204=VERTEX_POINT('',#51621);
#12205=VERTEX_POINT('',#51625);
#12206=VERTEX_POINT('',#51627);
#12207=VERTEX_POINT('',#51631);
#12208=VERTEX_POINT('',#51633);
#12209=VERTEX_POINT('',#51637);
#12210=VERTEX_POINT('',#51639);
#12211=VERTEX_POINT('',#51643);
#12212=VERTEX_POINT('',#51645);
#12213=VERTEX_POINT('',#51649);
#12214=VERTEX_POINT('',#51651);
#12215=VERTEX_POINT('',#51655);
#12216=VERTEX_POINT('',#51657);
#12217=VERTEX_POINT('',#51661);
#12218=VERTEX_POINT('',#51663);
#12219=VERTEX_POINT('',#51667);
#12220=VERTEX_POINT('',#51669);
#12221=VERTEX_POINT('',#51673);
#12222=VERTEX_POINT('',#51675);
#12223=VERTEX_POINT('',#51679);
#12224=VERTEX_POINT('',#51681);
#12225=VERTEX_POINT('',#51685);
#12226=VERTEX_POINT('',#51687);
#12227=VERTEX_POINT('',#51691);
#12228=VERTEX_POINT('',#51693);
#12229=VERTEX_POINT('',#51697);
#12230=VERTEX_POINT('',#51699);
#12231=VERTEX_POINT('',#51703);
#12232=VERTEX_POINT('',#51705);
#12233=VERTEX_POINT('',#51709);
#12234=VERTEX_POINT('',#51711);
#12235=VERTEX_POINT('',#51715);
#12236=VERTEX_POINT('',#51717);
#12237=VERTEX_POINT('',#51721);
#12238=VERTEX_POINT('',#51723);
#12239=VERTEX_POINT('',#51727);
#12240=VERTEX_POINT('',#51729);
#12241=VERTEX_POINT('',#51733);
#12242=VERTEX_POINT('',#51735);
#12243=VERTEX_POINT('',#51739);
#12244=VERTEX_POINT('',#51741);
#12245=VERTEX_POINT('',#51745);
#12246=VERTEX_POINT('',#51747);
#12247=VERTEX_POINT('',#51751);
#12248=VERTEX_POINT('',#51753);
#12249=VERTEX_POINT('',#51757);
#12250=VERTEX_POINT('',#51759);
#12251=VERTEX_POINT('',#51763);
#12252=VERTEX_POINT('',#51765);
#12253=VERTEX_POINT('',#51769);
#12254=VERTEX_POINT('',#51771);
#12255=VERTEX_POINT('',#51775);
#12256=VERTEX_POINT('',#51777);
#12257=VERTEX_POINT('',#51781);
#12258=VERTEX_POINT('',#51783);
#12259=VERTEX_POINT('',#51787);
#12260=VERTEX_POINT('',#51789);
#12261=VERTEX_POINT('',#51793);
#12262=VERTEX_POINT('',#51795);
#12263=VERTEX_POINT('',#51799);
#12264=VERTEX_POINT('',#51801);
#12265=VERTEX_POINT('',#51805);
#12266=VERTEX_POINT('',#51807);
#12267=VERTEX_POINT('',#51811);
#12268=VERTEX_POINT('',#51813);
#12269=VERTEX_POINT('',#51817);
#12270=VERTEX_POINT('',#51819);
#12271=VERTEX_POINT('',#51823);
#12272=VERTEX_POINT('',#51825);
#12273=VERTEX_POINT('',#51829);
#12274=VERTEX_POINT('',#51831);
#12275=VERTEX_POINT('',#51835);
#12276=VERTEX_POINT('',#51837);
#12277=VERTEX_POINT('',#51841);
#12278=VERTEX_POINT('',#51843);
#12279=VERTEX_POINT('',#51847);
#12280=VERTEX_POINT('',#51849);
#12281=VERTEX_POINT('',#51853);
#12282=VERTEX_POINT('',#51855);
#12283=VERTEX_POINT('',#51859);
#12284=VERTEX_POINT('',#51861);
#12285=VERTEX_POINT('',#51865);
#12286=VERTEX_POINT('',#51867);
#12287=VERTEX_POINT('',#51871);
#12288=VERTEX_POINT('',#51873);
#12289=VERTEX_POINT('',#51877);
#12290=VERTEX_POINT('',#51879);
#12291=VERTEX_POINT('',#51883);
#12292=VERTEX_POINT('',#51885);
#12293=VERTEX_POINT('',#51889);
#12294=VERTEX_POINT('',#51891);
#12295=VERTEX_POINT('',#51895);
#12296=VERTEX_POINT('',#51897);
#12297=VERTEX_POINT('',#51901);
#12298=VERTEX_POINT('',#51903);
#12299=VERTEX_POINT('',#51907);
#12300=VERTEX_POINT('',#51909);
#12301=VERTEX_POINT('',#51913);
#12302=VERTEX_POINT('',#51915);
#12303=VERTEX_POINT('',#51919);
#12304=VERTEX_POINT('',#51921);
#12305=VERTEX_POINT('',#51925);
#12306=VERTEX_POINT('',#51927);
#12307=VERTEX_POINT('',#51931);
#12308=VERTEX_POINT('',#51933);
#12309=VERTEX_POINT('',#51937);
#12310=VERTEX_POINT('',#51939);
#12311=VERTEX_POINT('',#51943);
#12312=VERTEX_POINT('',#51945);
#12313=VERTEX_POINT('',#51949);
#12314=VERTEX_POINT('',#51951);
#12315=VERTEX_POINT('',#51955);
#12316=VERTEX_POINT('',#51957);
#12317=VERTEX_POINT('',#51961);
#12318=VERTEX_POINT('',#51963);
#12319=VERTEX_POINT('',#51967);
#12320=VERTEX_POINT('',#51969);
#12321=VERTEX_POINT('',#51973);
#12322=VERTEX_POINT('',#51975);
#12323=VERTEX_POINT('',#51979);
#12324=VERTEX_POINT('',#51981);
#12325=VERTEX_POINT('',#51985);
#12326=VERTEX_POINT('',#51987);
#12327=VERTEX_POINT('',#51991);
#12328=VERTEX_POINT('',#51993);
#12329=VERTEX_POINT('',#51997);
#12330=VERTEX_POINT('',#51999);
#12331=VERTEX_POINT('',#52003);
#12332=VERTEX_POINT('',#52005);
#12333=VERTEX_POINT('',#52009);
#12334=VERTEX_POINT('',#52011);
#12335=VERTEX_POINT('',#52015);
#12336=VERTEX_POINT('',#52017);
#12337=VERTEX_POINT('',#52021);
#12338=VERTEX_POINT('',#52023);
#12339=VERTEX_POINT('',#52027);
#12340=VERTEX_POINT('',#52029);
#12341=VERTEX_POINT('',#52033);
#12342=VERTEX_POINT('',#52035);
#12343=VERTEX_POINT('',#52039);
#12344=VERTEX_POINT('',#52041);
#12345=VERTEX_POINT('',#52045);
#12346=VERTEX_POINT('',#52047);
#12347=VERTEX_POINT('',#52051);
#12348=VERTEX_POINT('',#52053);
#12349=VERTEX_POINT('',#52057);
#12350=VERTEX_POINT('',#52059);
#12351=VERTEX_POINT('',#52063);
#12352=VERTEX_POINT('',#52065);
#12353=VERTEX_POINT('',#52069);
#12354=VERTEX_POINT('',#52071);
#12355=VERTEX_POINT('',#52075);
#12356=VERTEX_POINT('',#52077);
#12357=VERTEX_POINT('',#52081);
#12358=VERTEX_POINT('',#52083);
#12359=VERTEX_POINT('',#52087);
#12360=VERTEX_POINT('',#52089);
#12361=VERTEX_POINT('',#52093);
#12362=VERTEX_POINT('',#52095);
#12363=VERTEX_POINT('',#52099);
#12364=VERTEX_POINT('',#52101);
#12365=VERTEX_POINT('',#52105);
#12366=VERTEX_POINT('',#52107);
#12367=VERTEX_POINT('',#52111);
#12368=VERTEX_POINT('',#52113);
#12369=VERTEX_POINT('',#52117);
#12370=VERTEX_POINT('',#52119);
#12371=VERTEX_POINT('',#52123);
#12372=VERTEX_POINT('',#52125);
#12373=VERTEX_POINT('',#52129);
#12374=VERTEX_POINT('',#52131);
#12375=VERTEX_POINT('',#52135);
#12376=VERTEX_POINT('',#52137);
#12377=VERTEX_POINT('',#52141);
#12378=VERTEX_POINT('',#52143);
#12379=VERTEX_POINT('',#52147);
#12380=VERTEX_POINT('',#52149);
#12381=VERTEX_POINT('',#52153);
#12382=VERTEX_POINT('',#52155);
#12383=VERTEX_POINT('',#52159);
#12384=VERTEX_POINT('',#52161);
#12385=VERTEX_POINT('',#52165);
#12386=VERTEX_POINT('',#52167);
#12387=VERTEX_POINT('',#52171);
#12388=VERTEX_POINT('',#52173);
#12389=VERTEX_POINT('',#52177);
#12390=VERTEX_POINT('',#52179);
#12391=VERTEX_POINT('',#52183);
#12392=VERTEX_POINT('',#52185);
#12393=VERTEX_POINT('',#52189);
#12394=VERTEX_POINT('',#52191);
#12395=VERTEX_POINT('',#52195);
#12396=VERTEX_POINT('',#52197);
#12397=VERTEX_POINT('',#52201);
#12398=VERTEX_POINT('',#52203);
#12399=VERTEX_POINT('',#52207);
#12400=VERTEX_POINT('',#52209);
#12401=VERTEX_POINT('',#52213);
#12402=VERTEX_POINT('',#52215);
#12403=VERTEX_POINT('',#52219);
#12404=VERTEX_POINT('',#52221);
#12405=VERTEX_POINT('',#52225);
#12406=VERTEX_POINT('',#52227);
#12407=VERTEX_POINT('',#52231);
#12408=VERTEX_POINT('',#52233);
#12409=VERTEX_POINT('',#52237);
#12410=VERTEX_POINT('',#52239);
#12411=VERTEX_POINT('',#52243);
#12412=VERTEX_POINT('',#52245);
#12413=VERTEX_POINT('',#52249);
#12414=VERTEX_POINT('',#52251);
#12415=VERTEX_POINT('',#52255);
#12416=VERTEX_POINT('',#52257);
#12417=VERTEX_POINT('',#52261);
#12418=VERTEX_POINT('',#52263);
#12419=VERTEX_POINT('',#52267);
#12420=VERTEX_POINT('',#52269);
#12421=VERTEX_POINT('',#52273);
#12422=VERTEX_POINT('',#52275);
#12423=VERTEX_POINT('',#52279);
#12424=VERTEX_POINT('',#52281);
#12425=VERTEX_POINT('',#52285);
#12426=VERTEX_POINT('',#52287);
#12427=VERTEX_POINT('',#52291);
#12428=VERTEX_POINT('',#52293);
#12429=VERTEX_POINT('',#52297);
#12430=VERTEX_POINT('',#52299);
#12431=VERTEX_POINT('',#52303);
#12432=VERTEX_POINT('',#52305);
#12433=VERTEX_POINT('',#52309);
#12434=VERTEX_POINT('',#52311);
#12435=VERTEX_POINT('',#52315);
#12436=VERTEX_POINT('',#52317);
#12437=VERTEX_POINT('',#52321);
#12438=VERTEX_POINT('',#52323);
#12439=VERTEX_POINT('',#52327);
#12440=VERTEX_POINT('',#52329);
#12441=VERTEX_POINT('',#52333);
#12442=VERTEX_POINT('',#52335);
#12443=VERTEX_POINT('',#52339);
#12444=VERTEX_POINT('',#52341);
#12445=VERTEX_POINT('',#52345);
#12446=VERTEX_POINT('',#52347);
#12447=VERTEX_POINT('',#52351);
#12448=VERTEX_POINT('',#52353);
#12449=VERTEX_POINT('',#52357);
#12450=VERTEX_POINT('',#52359);
#12451=VERTEX_POINT('',#52363);
#12452=VERTEX_POINT('',#52365);
#12453=VERTEX_POINT('',#52369);
#12454=VERTEX_POINT('',#52371);
#12455=VERTEX_POINT('',#52375);
#12456=VERTEX_POINT('',#52377);
#12457=VERTEX_POINT('',#52381);
#12458=VERTEX_POINT('',#52383);
#12459=VERTEX_POINT('',#52387);
#12460=VERTEX_POINT('',#52389);
#12461=VERTEX_POINT('',#52393);
#12462=VERTEX_POINT('',#52395);
#12463=VERTEX_POINT('',#52399);
#12464=VERTEX_POINT('',#52401);
#12465=VERTEX_POINT('',#52405);
#12466=VERTEX_POINT('',#52407);
#12467=VERTEX_POINT('',#52411);
#12468=VERTEX_POINT('',#52413);
#12469=VERTEX_POINT('',#52417);
#12470=VERTEX_POINT('',#52419);
#12471=VERTEX_POINT('',#52423);
#12472=VERTEX_POINT('',#52425);
#12473=VERTEX_POINT('',#52429);
#12474=VERTEX_POINT('',#52431);
#12475=VERTEX_POINT('',#52435);
#12476=VERTEX_POINT('',#52437);
#12477=VERTEX_POINT('',#52441);
#12478=VERTEX_POINT('',#52443);
#12479=VERTEX_POINT('',#52447);
#12480=VERTEX_POINT('',#52449);
#12481=VERTEX_POINT('',#52453);
#12482=VERTEX_POINT('',#52455);
#12483=VERTEX_POINT('',#52459);
#12484=VERTEX_POINT('',#52461);
#12485=VERTEX_POINT('',#52465);
#12486=VERTEX_POINT('',#52467);
#12487=VERTEX_POINT('',#52471);
#12488=VERTEX_POINT('',#52473);
#12489=VERTEX_POINT('',#52477);
#12490=VERTEX_POINT('',#52479);
#12491=VERTEX_POINT('',#52483);
#12492=VERTEX_POINT('',#52485);
#12493=VERTEX_POINT('',#52489);
#12494=VERTEX_POINT('',#52491);
#12495=VERTEX_POINT('',#52495);
#12496=VERTEX_POINT('',#52497);
#12497=VERTEX_POINT('',#52501);
#12498=VERTEX_POINT('',#52503);
#12499=VERTEX_POINT('',#52507);
#12500=VERTEX_POINT('',#52509);
#12501=VERTEX_POINT('',#52513);
#12502=VERTEX_POINT('',#52515);
#12503=VERTEX_POINT('',#52519);
#12504=VERTEX_POINT('',#52521);
#12505=VERTEX_POINT('',#52525);
#12506=VERTEX_POINT('',#52527);
#12507=VERTEX_POINT('',#52531);
#12508=VERTEX_POINT('',#52533);
#12509=VERTEX_POINT('',#52537);
#12510=VERTEX_POINT('',#52539);
#12511=VERTEX_POINT('',#52543);
#12512=VERTEX_POINT('',#52545);
#12513=VERTEX_POINT('',#52549);
#12514=VERTEX_POINT('',#52551);
#12515=VERTEX_POINT('',#52555);
#12516=VERTEX_POINT('',#52557);
#12517=VERTEX_POINT('',#52561);
#12518=VERTEX_POINT('',#52563);
#12519=VERTEX_POINT('',#52567);
#12520=VERTEX_POINT('',#52569);
#12521=VERTEX_POINT('',#52573);
#12522=VERTEX_POINT('',#52575);
#12523=VERTEX_POINT('',#52579);
#12524=VERTEX_POINT('',#52581);
#12525=VERTEX_POINT('',#52585);
#12526=VERTEX_POINT('',#52587);
#12527=VERTEX_POINT('',#52591);
#12528=VERTEX_POINT('',#52593);
#12529=VERTEX_POINT('',#52597);
#12530=VERTEX_POINT('',#52599);
#12531=VERTEX_POINT('',#52603);
#12532=VERTEX_POINT('',#52605);
#12533=VERTEX_POINT('',#52609);
#12534=VERTEX_POINT('',#52611);
#12535=VERTEX_POINT('',#52615);
#12536=VERTEX_POINT('',#52617);
#12537=VERTEX_POINT('',#52621);
#12538=VERTEX_POINT('',#52623);
#12539=VERTEX_POINT('',#52627);
#12540=VERTEX_POINT('',#52629);
#12541=VERTEX_POINT('',#52633);
#12542=VERTEX_POINT('',#52635);
#12543=VERTEX_POINT('',#52639);
#12544=VERTEX_POINT('',#52641);
#12545=VERTEX_POINT('',#52645);
#12546=VERTEX_POINT('',#52647);
#12547=VERTEX_POINT('',#52651);
#12548=VERTEX_POINT('',#52653);
#12549=VERTEX_POINT('',#52657);
#12550=VERTEX_POINT('',#52659);
#12551=VERTEX_POINT('',#52663);
#12552=VERTEX_POINT('',#52665);
#12553=VERTEX_POINT('',#52669);
#12554=VERTEX_POINT('',#52671);
#12555=VERTEX_POINT('',#52675);
#12556=VERTEX_POINT('',#52677);
#12557=VERTEX_POINT('',#52681);
#12558=VERTEX_POINT('',#52683);
#12559=VERTEX_POINT('',#52687);
#12560=VERTEX_POINT('',#52689);
#12561=VERTEX_POINT('',#52693);
#12562=VERTEX_POINT('',#52695);
#12563=VERTEX_POINT('',#52699);
#12564=VERTEX_POINT('',#52701);
#12565=VERTEX_POINT('',#52705);
#12566=VERTEX_POINT('',#52707);
#12567=VERTEX_POINT('',#52711);
#12568=VERTEX_POINT('',#52713);
#12569=VERTEX_POINT('',#52717);
#12570=VERTEX_POINT('',#52719);
#12571=VERTEX_POINT('',#52723);
#12572=VERTEX_POINT('',#52725);
#12573=VERTEX_POINT('',#52729);
#12574=VERTEX_POINT('',#52731);
#12575=VERTEX_POINT('',#52735);
#12576=VERTEX_POINT('',#52737);
#12577=VERTEX_POINT('',#52741);
#12578=VERTEX_POINT('',#52743);
#12579=VERTEX_POINT('',#52753);
#12580=VERTEX_POINT('',#52755);
#12581=VERTEX_POINT('',#52759);
#12582=VERTEX_POINT('',#52760);
#12583=VERTEX_POINT('',#52762);
#12584=VERTEX_POINT('',#52764);
#12585=VERTEX_POINT('',#52766);
#12586=VERTEX_POINT('',#52768);
#12587=VERTEX_POINT('',#52770);
#12588=VERTEX_POINT('',#52772);
#12589=VERTEX_POINT('',#52775);
#12590=VERTEX_POINT('',#52777);
#12591=VERTEX_POINT('',#52779);
#12592=VERTEX_POINT('',#52781);
#12593=VERTEX_POINT('',#52783);
#12594=VERTEX_POINT('',#52784);
#12595=VERTEX_POINT('',#52786);
#12596=VERTEX_POINT('',#52788);
#12597=VERTEX_POINT('',#52790);
#12598=VERTEX_POINT('',#52792);
#12599=VERTEX_POINT('',#52795);
#12600=VERTEX_POINT('',#52796);
#12601=VERTEX_POINT('',#52798);
#12602=VERTEX_POINT('',#52800);
#12603=VERTEX_POINT('',#52802);
#12604=VERTEX_POINT('',#52804);
#12605=VERTEX_POINT('',#52807);
#12606=VERTEX_POINT('',#52809);
#12607=VERTEX_POINT('',#52811);
#12608=VERTEX_POINT('',#52814);
#12609=VERTEX_POINT('',#52818);
#12610=VERTEX_POINT('',#52822);
#12611=VERTEX_POINT('',#52826);
#12612=VERTEX_POINT('',#52830);
#12613=VERTEX_POINT('',#52834);
#12614=VERTEX_POINT('',#52838);
#12615=VERTEX_POINT('',#52842);
#12616=VERTEX_POINT('',#52846);
#12617=VERTEX_POINT('',#52850);
#12618=VERTEX_POINT('',#52854);
#12619=VERTEX_POINT('',#52858);
#12620=VERTEX_POINT('',#52862);
#12621=VERTEX_POINT('',#52866);
#12622=VERTEX_POINT('',#52870);
#12623=VERTEX_POINT('',#52874);
#12624=VERTEX_POINT('',#52875);
#12625=VERTEX_POINT('',#52880);
#12626=VERTEX_POINT('',#52884);
#12627=VERTEX_POINT('',#52888);
#12628=VERTEX_POINT('',#52892);
#12629=VERTEX_POINT('',#52898);
#12630=VERTEX_POINT('',#52899);
#12631=VERTEX_POINT('',#52904);
#12632=VERTEX_POINT('',#52908);
#12633=VERTEX_POINT('',#52912);
#12634=VERTEX_POINT('',#52916);
#12635=VERTEX_POINT('',#52922);
#12636=VERTEX_POINT('',#52924);
#12637=VERTEX_POINT('',#52928);
#12638=VERTEX_POINT('',#52932);
#12639=VERTEX_POINT('',#52936);
#12640=VERTEX_POINT('',#52940);
#12641=VERTEX_POINT('',#52944);
#12642=VERTEX_POINT('',#52948);
#12643=VERTEX_POINT('',#52954);
#12644=VERTEX_POINT('',#52956);
#12645=VERTEX_POINT('',#52960);
#12646=VERTEX_POINT('',#52964);
#12647=VERTEX_POINT('',#52968);
#12648=VERTEX_POINT('',#52972);
#12649=VERTEX_POINT('',#52976);
#12650=VERTEX_POINT('',#52980);
#12651=VERTEX_POINT('',#52988);
#12652=VERTEX_POINT('',#52990);
#12653=VERTEX_POINT('',#52994);
#12654=VERTEX_POINT('',#52996);
#12655=VERTEX_POINT('',#53000);
#12656=VERTEX_POINT('',#53002);
#12657=VERTEX_POINT('',#53006);
#12658=VERTEX_POINT('',#53008);
#12659=VERTEX_POINT('',#53010);
#12660=VERTEX_POINT('',#53012);
#12661=VERTEX_POINT('',#53014);
#12662=VERTEX_POINT('',#53018);
#12663=VERTEX_POINT('',#53019);
#12664=VERTEX_POINT('',#53021);
#12665=VERTEX_POINT('',#53023);
#12666=VERTEX_POINT('',#53027);
#12667=VERTEX_POINT('',#53029);
#12668=VERTEX_POINT('',#53033);
#12669=VERTEX_POINT('',#53035);
#12670=VERTEX_POINT('',#53037);
#12671=VERTEX_POINT('',#53039);
#12672=VERTEX_POINT('',#53041);
#12673=VERTEX_POINT('',#53045);
#12674=VERTEX_POINT('',#53046);
#12675=VERTEX_POINT('',#53048);
#12676=VERTEX_POINT('',#53050);
#12677=VERTEX_POINT('',#53069);
#12678=VERTEX_POINT('',#53071);
#12679=VERTEX_POINT('',#53073);
#12680=VERTEX_POINT('',#53092);
#12681=VERTEX_POINT('',#53094);
#12682=VERTEX_POINT('',#53096);
#12683=VERTEX_POINT('',#53100);
#12684=VERTEX_POINT('',#53104);
#12685=VERTEX_POINT('',#53105);
#12686=VERTEX_POINT('',#53107);
#12687=VERTEX_POINT('',#53109);
#12688=VERTEX_POINT('',#53114);
#12689=VERTEX_POINT('',#53117);
#12690=VERTEX_POINT('',#53121);
#12691=VERTEX_POINT('',#53122);
#12692=VERTEX_POINT('',#53125);
#12693=VERTEX_POINT('',#53127);
#12694=VERTEX_POINT('',#53131);
#12695=VERTEX_POINT('',#53141);
#12696=VERTEX_POINT('',#53143);
#12697=VERTEX_POINT('',#53147);
#12698=VERTEX_POINT('',#53149);
#12699=VERTEX_POINT('',#53159);
#12700=VERTEX_POINT('',#53160);
#12701=VERTEX_POINT('',#53162);
#12702=VERTEX_POINT('',#53269);
#12703=VERTEX_POINT('',#53346);
#12704=VERTEX_POINT('',#53347);
#12705=VERTEX_POINT('',#53644);
#12706=VERTEX_POINT('',#53645);
#12707=VERTEX_POINT('',#53647);
#12708=VERTEX_POINT('',#53796);
#12709=VERTEX_POINT('',#53944);
#12710=VERTEX_POINT('',#53945);
#12711=VERTEX_POINT('',#54234);
#12712=VERTEX_POINT('',#54235);
#12713=VERTEX_POINT('',#54237);
#12714=VERTEX_POINT('',#54382);
#12715=VERTEX_POINT('',#54532);
#12716=VERTEX_POINT('',#54533);
#12717=VERTEX_POINT('',#54824);
#12718=VERTEX_POINT('',#54825);
#12719=VERTEX_POINT('',#54827);
#12720=VERTEX_POINT('',#54970);
#12721=VERTEX_POINT('',#55114);
#12722=VERTEX_POINT('',#55115);
#12723=VERTEX_POINT('',#55174);
#12724=VERTEX_POINT('',#55176);
#12725=VERTEX_POINT('',#55182);
#12726=VERTEX_POINT('',#55358);
#12727=VERTEX_POINT('',#55534);
#12728=VERTEX_POINT('',#55707);
#12729=VERTEX_POINT('',#55883);
#12730=VERTEX_POINT('',#56059);
#12731=VERTEX_POINT('',#56235);
#12732=VERTEX_POINT('',#56411);
#12733=VERTEX_POINT('',#56446);
#12734=VERTEX_POINT('',#56448);
#12735=VERTEX_POINT('',#56456);
#12736=VERTEX_POINT('',#56467);
#12737=VERTEX_POINT('',#56643);
#12738=VERTEX_POINT('',#56819);
#12739=VERTEX_POINT('',#56995);
#12740=VERTEX_POINT('',#57168);
#12741=VERTEX_POINT('',#57520);
#12742=VERTEX_POINT('',#57649);
#12743=VERTEX_POINT('',#57748);
#12744=VERTEX_POINT('',#57749);
#12745=VERTEX_POINT('',#57830);
#12746=VERTEX_POINT('',#58133);
#12747=VERTEX_POINT('',#58224);
#12748=VERTEX_POINT('',#58225);
#12749=VERTEX_POINT('',#58520);
#12750=VERTEX_POINT('',#58524);
#12751=VERTEX_POINT('',#58527);
#12752=VERTEX_POINT('',#58532);
#12753=VERTEX_POINT('',#58533);
#12754=VERTEX_POINT('',#58535);
#12755=VERTEX_POINT('',#58537);
#12756=VERTEX_POINT('',#58543);
#12757=VERTEX_POINT('',#58544);
#12758=VERTEX_POINT('',#58553);
#12759=VERTEX_POINT('',#58554);
#12760=VERTEX_POINT('',#58558);
#12761=VERTEX_POINT('',#58560);
#12762=VERTEX_POINT('',#58564);
#12763=VERTEX_POINT('',#58568);
#12764=VERTEX_POINT('',#58570);
#12765=VERTEX_POINT('',#58574);
#12766=VERTEX_POINT('',#58578);
#12767=VERTEX_POINT('',#58580);
#12768=VERTEX_POINT('',#58584);
#12769=VERTEX_POINT('',#58588);
#12770=VERTEX_POINT('',#58590);
#12771=VERTEX_POINT('',#58594);
#12772=VERTEX_POINT('',#58598);
#12773=VERTEX_POINT('',#58600);
#12774=VERTEX_POINT('',#58604);
#12775=VERTEX_POINT('',#58608);
#12776=VERTEX_POINT('',#58610);
#12777=VERTEX_POINT('',#58614);
#12778=VERTEX_POINT('',#58618);
#12779=VERTEX_POINT('',#58620);
#12780=VERTEX_POINT('',#58624);
#12781=VERTEX_POINT('',#58628);
#12782=VERTEX_POINT('',#58630);
#12783=VERTEX_POINT('',#58634);
#12784=VERTEX_POINT('',#58638);
#12785=VERTEX_POINT('',#58640);
#12786=VERTEX_POINT('',#58644);
#12787=VERTEX_POINT('',#58648);
#12788=VERTEX_POINT('',#58650);
#12789=VERTEX_POINT('',#58654);
#12790=VERTEX_POINT('',#58658);
#12791=VERTEX_POINT('',#58660);
#12792=VERTEX_POINT('',#58664);
#12793=VERTEX_POINT('',#58668);
#12794=VERTEX_POINT('',#58670);
#12795=VERTEX_POINT('',#58674);
#12796=VERTEX_POINT('',#58678);
#12797=VERTEX_POINT('',#58680);
#12798=VERTEX_POINT('',#58684);
#12799=VERTEX_POINT('',#58688);
#12800=VERTEX_POINT('',#58690);
#12801=VERTEX_POINT('',#58694);
#12802=VERTEX_POINT('',#58698);
#12803=VERTEX_POINT('',#58700);
#12804=VERTEX_POINT('',#58704);
#12805=VERTEX_POINT('',#58708);
#12806=VERTEX_POINT('',#58710);
#12807=VERTEX_POINT('',#58714);
#12808=VERTEX_POINT('',#58718);
#12809=VERTEX_POINT('',#58720);
#12810=VERTEX_POINT('',#58724);
#12811=VERTEX_POINT('',#58728);
#12812=VERTEX_POINT('',#58730);
#12813=VERTEX_POINT('',#58734);
#12814=VERTEX_POINT('',#58738);
#12815=VERTEX_POINT('',#58740);
#12816=VERTEX_POINT('',#58744);
#12817=VERTEX_POINT('',#58748);
#12818=VERTEX_POINT('',#58750);
#12819=VERTEX_POINT('',#58754);
#12820=VERTEX_POINT('',#58758);
#12821=VERTEX_POINT('',#58760);
#12822=VERTEX_POINT('',#58764);
#12823=VERTEX_POINT('',#58768);
#12824=VERTEX_POINT('',#58770);
#12825=VERTEX_POINT('',#58774);
#12826=VERTEX_POINT('',#58778);
#12827=VERTEX_POINT('',#58780);
#12828=VERTEX_POINT('',#58784);
#12829=VERTEX_POINT('',#58788);
#12830=VERTEX_POINT('',#58790);
#12831=VERTEX_POINT('',#58794);
#12832=VERTEX_POINT('',#58798);
#12833=VERTEX_POINT('',#58800);
#12834=VERTEX_POINT('',#58804);
#12835=VERTEX_POINT('',#58808);
#12836=VERTEX_POINT('',#58810);
#12837=VERTEX_POINT('',#58814);
#12838=VERTEX_POINT('',#58818);
#12839=VERTEX_POINT('',#58820);
#12840=VERTEX_POINT('',#58824);
#12841=VERTEX_POINT('',#58829);
#12842=VERTEX_POINT('',#58831);
#12843=VERTEX_POINT('',#58835);
#12844=VERTEX_POINT('',#58839);
#12845=VERTEX_POINT('',#58841);
#12846=VERTEX_POINT('',#58845);
#12847=VERTEX_POINT('',#58849);
#12848=VERTEX_POINT('',#58851);
#12849=VERTEX_POINT('',#58855);
#12850=VERTEX_POINT('',#58859);
#12851=VERTEX_POINT('',#58861);
#12852=VERTEX_POINT('',#58865);
#12853=VERTEX_POINT('',#58869);
#12854=VERTEX_POINT('',#58871);
#12855=VERTEX_POINT('',#58875);
#12856=VERTEX_POINT('',#58879);
#12857=VERTEX_POINT('',#58881);
#12858=VERTEX_POINT('',#58885);
#12859=VERTEX_POINT('',#58889);
#12860=VERTEX_POINT('',#58891);
#12861=VERTEX_POINT('',#58895);
#12862=VERTEX_POINT('',#58899);
#12863=VERTEX_POINT('',#58904);
#12864=VERTEX_POINT('',#58908);
#12865=VERTEX_POINT('',#58910);
#12866=VERTEX_POINT('',#58914);
#12867=VERTEX_POINT('',#58920);
#12868=VERTEX_POINT('',#58922);
#12869=VERTEX_POINT('',#58926);
#12870=VERTEX_POINT('',#58932);
#12871=VERTEX_POINT('',#58934);
#12872=VERTEX_POINT('',#58938);
#12873=VERTEX_POINT('',#58944);
#12874=VERTEX_POINT('',#58946);
#12875=VERTEX_POINT('',#58950);
#12876=VERTEX_POINT('',#58956);
#12877=VERTEX_POINT('',#58958);
#12878=VERTEX_POINT('',#58962);
#12879=VERTEX_POINT('',#58968);
#12880=VERTEX_POINT('',#58970);
#12881=VERTEX_POINT('',#58974);
#12882=VERTEX_POINT('',#58980);
#12883=VERTEX_POINT('',#58982);
#12884=VERTEX_POINT('',#58986);
#12885=VERTEX_POINT('',#58992);
#12886=VERTEX_POINT('',#58994);
#12887=VERTEX_POINT('',#58998);
#12888=VERTEX_POINT('',#59002);
#12889=VERTEX_POINT('',#59006);
#12890=VERTEX_POINT('',#59008);
#12891=VERTEX_POINT('',#59012);
#12892=VERTEX_POINT('',#59018);
#12893=VERTEX_POINT('',#59020);
#12894=VERTEX_POINT('',#59024);
#12895=VERTEX_POINT('',#59030);
#12896=VERTEX_POINT('',#59032);
#12897=VERTEX_POINT('',#59036);
#12898=VERTEX_POINT('',#59042);
#12899=VERTEX_POINT('',#59044);
#12900=VERTEX_POINT('',#59048);
#12901=VERTEX_POINT('',#59054);
#12902=VERTEX_POINT('',#59056);
#12903=VERTEX_POINT('',#59060);
#12904=VERTEX_POINT('',#59066);
#12905=VERTEX_POINT('',#59068);
#12906=VERTEX_POINT('',#59072);
#12907=VERTEX_POINT('',#59078);
#12908=VERTEX_POINT('',#59080);
#12909=VERTEX_POINT('',#59084);
#12910=VERTEX_POINT('',#59090);
#12911=VERTEX_POINT('',#59092);
#12912=VERTEX_POINT('',#59096);
#12913=VERTEX_POINT('',#59102);
#12914=VERTEX_POINT('',#59104);
#12915=VERTEX_POINT('',#59108);
#12916=VERTEX_POINT('',#59114);
#12917=VERTEX_POINT('',#59116);
#12918=VERTEX_POINT('',#59120);
#12919=VERTEX_POINT('',#59126);
#12920=VERTEX_POINT('',#59128);
#12921=VERTEX_POINT('',#59132);
#12922=VERTEX_POINT('',#59138);
#12923=VERTEX_POINT('',#59140);
#12924=VERTEX_POINT('',#59144);
#12925=VERTEX_POINT('',#59150);
#12926=VERTEX_POINT('',#59152);
#12927=VERTEX_POINT('',#59156);
#12928=VERTEX_POINT('',#59162);
#12929=VERTEX_POINT('',#59164);
#12930=VERTEX_POINT('',#59168);
#12931=VERTEX_POINT('',#59174);
#12932=VERTEX_POINT('',#59176);
#12933=VERTEX_POINT('',#59180);
#12934=VERTEX_POINT('',#59186);
#12935=VERTEX_POINT('',#59188);
#12936=VERTEX_POINT('',#59192);
#12937=VERTEX_POINT('',#59198);
#12938=VERTEX_POINT('',#59200);
#12939=VERTEX_POINT('',#59204);
#12940=VERTEX_POINT('',#59210);
#12941=VERTEX_POINT('',#59212);
#12942=VERTEX_POINT('',#59216);
#12943=VERTEX_POINT('',#59222);
#12944=VERTEX_POINT('',#59224);
#12945=VERTEX_POINT('',#59228);
#12946=VERTEX_POINT('',#59234);
#12947=VERTEX_POINT('',#59236);
#12948=VERTEX_POINT('',#59240);
#12949=VERTEX_POINT('',#59246);
#12950=VERTEX_POINT('',#59248);
#12951=VERTEX_POINT('',#59252);
#12952=VERTEX_POINT('',#59258);
#12953=VERTEX_POINT('',#59260);
#12954=VERTEX_POINT('',#59264);
#12955=VERTEX_POINT('',#59270);
#12956=VERTEX_POINT('',#59272);
#12957=VERTEX_POINT('',#59276);
#12958=VERTEX_POINT('',#59282);
#12959=VERTEX_POINT('',#59284);
#12960=VERTEX_POINT('',#59288);
#12961=VERTEX_POINT('',#59294);
#12962=VERTEX_POINT('',#59296);
#12963=VERTEX_POINT('',#59300);
#12964=VERTEX_POINT('',#59306);
#12965=VERTEX_POINT('',#59308);
#12966=VERTEX_POINT('',#59312);
#12967=VERTEX_POINT('',#59318);
#12968=VERTEX_POINT('',#59320);
#12969=VERTEX_POINT('',#59324);
#12970=VERTEX_POINT('',#59332);
#12971=VERTEX_POINT('',#59333);
#12972=VERTEX_POINT('',#59335);
#12973=VERTEX_POINT('',#59337);
#12974=VERTEX_POINT('',#59339);
#12975=VERTEX_POINT('',#59341);
#12976=VERTEX_POINT('',#59345);
#12977=VERTEX_POINT('',#59346);
#12978=VERTEX_POINT('',#59350);
#12979=VERTEX_POINT('',#59354);
#12980=VERTEX_POINT('',#59358);
#12981=VERTEX_POINT('',#59362);
#12982=VERTEX_POINT('',#59369);
#12983=VERTEX_POINT('',#59385);
#12984=VERTEX_POINT('',#59386);
#12985=VERTEX_POINT('',#59388);
#12986=VERTEX_POINT('',#59516);
#12987=VERTEX_POINT('',#59607);
#12988=VERTEX_POINT('',#59608);
#12989=VERTEX_POINT('',#59610);
#12990=VERTEX_POINT('',#59781);
#12991=VERTEX_POINT('',#59940);
#12992=VERTEX_POINT('',#59941);
#12993=VERTEX_POINT('',#59943);
#12994=VERTEX_POINT('',#60136);
#12995=VERTEX_POINT('',#60137);
#12996=VERTEX_POINT('',#60139);
#12997=VERTEX_POINT('',#60295);
#12998=VERTEX_POINT('',#60333);
#12999=VERTEX_POINT('',#60334);
#13000=VERTEX_POINT('',#60336);
#13001=VERTEX_POINT('',#60368);
#13002=VERTEX_POINT('',#60512);
#13003=VERTEX_POINT('',#60513);
#13004=VERTEX_POINT('',#60515);
#13005=VERTEX_POINT('',#60812);
#13006=VERTEX_POINT('',#60813);
#13007=VERTEX_POINT('',#60971);
#13008=VERTEX_POINT('',#61131);
#13009=VERTEX_POINT('',#61132);
#13010=VERTEX_POINT('',#61134);
#13011=VERTEX_POINT('',#61452);
#13012=VERTEX_POINT('',#61453);
#13013=VERTEX_POINT('',#61605);
#13014=VERTEX_POINT('',#61781);
#13015=VERTEX_POINT('',#61782);
#13016=VERTEX_POINT('',#61844);
#13017=VERTEX_POINT('',#61846);
#13018=VERTEX_POINT('',#61852);
#13019=VERTEX_POINT('',#62031);
#13020=VERTEX_POINT('',#62207);
#13021=VERTEX_POINT('',#62380);
#13022=VERTEX_POINT('',#62553);
#13023=VERTEX_POINT('',#62729);
#13024=VERTEX_POINT('',#62902);
#13025=VERTEX_POINT('',#63072);
#13026=VERTEX_POINT('',#63245);
#13027=VERTEX_POINT('',#63421);
#13028=VERTEX_POINT('',#63459);
#13029=VERTEX_POINT('',#63461);
#13030=VERTEX_POINT('',#63469);
#13031=VERTEX_POINT('',#63480);
#13032=VERTEX_POINT('',#63653);
#13033=VERTEX_POINT('',#63823);
#13034=VERTEX_POINT('',#63996);
#13035=VERTEX_POINT('',#64169);
#13036=VERTEX_POINT('',#64342);
#13037=VERTEX_POINT('',#64515);
#13038=VERTEX_POINT('',#64861);
#13039=VERTEX_POINT('',#64887);
#13040=VERTEX_POINT('',#65015);
#13041=VERTEX_POINT('',#65017);
#13042=VERTEX_POINT('',#65133);
#13043=VERTEX_POINT('',#65134);
#13044=VERTEX_POINT('',#65632);
#13045=VERTEX_POINT('',#65633);
#13046=VERTEX_POINT('',#65973);
#13047=VERTEX_POINT('',#65977);
#13048=VERTEX_POINT('',#65980);
#13049=VERTEX_POINT('',#65985);
#13050=VERTEX_POINT('',#65986);
#13051=VERTEX_POINT('',#65988);
#13052=VERTEX_POINT('',#65990);
#13053=VERTEX_POINT('',#65996);
#13054=VERTEX_POINT('',#65997);
#13055=VERTEX_POINT('',#66006);
#13056=VERTEX_POINT('',#66007);
#13057=VERTEX_POINT('',#66011);
#13058=VERTEX_POINT('',#66013);
#13059=VERTEX_POINT('',#66017);
#13060=VERTEX_POINT('',#66021);
#13061=VERTEX_POINT('',#66023);
#13062=VERTEX_POINT('',#66027);
#13063=VERTEX_POINT('',#66031);
#13064=VERTEX_POINT('',#66033);
#13065=VERTEX_POINT('',#66037);
#13066=VERTEX_POINT('',#66041);
#13067=VERTEX_POINT('',#66043);
#13068=VERTEX_POINT('',#66047);
#13069=VERTEX_POINT('',#66051);
#13070=VERTEX_POINT('',#66053);
#13071=VERTEX_POINT('',#66057);
#13072=VERTEX_POINT('',#66061);
#13073=VERTEX_POINT('',#66063);
#13074=VERTEX_POINT('',#66067);
#13075=VERTEX_POINT('',#66071);
#13076=VERTEX_POINT('',#66073);
#13077=VERTEX_POINT('',#66077);
#13078=VERTEX_POINT('',#66081);
#13079=VERTEX_POINT('',#66083);
#13080=VERTEX_POINT('',#66087);
#13081=VERTEX_POINT('',#66091);
#13082=VERTEX_POINT('',#66093);
#13083=VERTEX_POINT('',#66097);
#13084=VERTEX_POINT('',#66101);
#13085=VERTEX_POINT('',#66103);
#13086=VERTEX_POINT('',#66107);
#13087=VERTEX_POINT('',#66111);
#13088=VERTEX_POINT('',#66113);
#13089=VERTEX_POINT('',#66117);
#13090=VERTEX_POINT('',#66121);
#13091=VERTEX_POINT('',#66123);
#13092=VERTEX_POINT('',#66127);
#13093=VERTEX_POINT('',#66131);
#13094=VERTEX_POINT('',#66133);
#13095=VERTEX_POINT('',#66137);
#13096=VERTEX_POINT('',#66141);
#13097=VERTEX_POINT('',#66143);
#13098=VERTEX_POINT('',#66147);
#13099=VERTEX_POINT('',#66151);
#13100=VERTEX_POINT('',#66153);
#13101=VERTEX_POINT('',#66157);
#13102=VERTEX_POINT('',#66161);
#13103=VERTEX_POINT('',#66163);
#13104=VERTEX_POINT('',#66167);
#13105=VERTEX_POINT('',#66171);
#13106=VERTEX_POINT('',#66173);
#13107=VERTEX_POINT('',#66177);
#13108=VERTEX_POINT('',#66181);
#13109=VERTEX_POINT('',#66183);
#13110=VERTEX_POINT('',#66187);
#13111=VERTEX_POINT('',#66192);
#13112=VERTEX_POINT('',#66194);
#13113=VERTEX_POINT('',#66198);
#13114=VERTEX_POINT('',#66202);
#13115=VERTEX_POINT('',#66204);
#13116=VERTEX_POINT('',#66208);
#13117=VERTEX_POINT('',#66212);
#13118=VERTEX_POINT('',#66214);
#13119=VERTEX_POINT('',#66218);
#13120=VERTEX_POINT('',#66222);
#13121=VERTEX_POINT('',#66224);
#13122=VERTEX_POINT('',#66228);
#13123=VERTEX_POINT('',#66232);
#13124=VERTEX_POINT('',#66234);
#13125=VERTEX_POINT('',#66238);
#13126=VERTEX_POINT('',#66242);
#13127=VERTEX_POINT('',#66244);
#13128=VERTEX_POINT('',#66248);
#13129=VERTEX_POINT('',#66252);
#13130=VERTEX_POINT('',#66254);
#13131=VERTEX_POINT('',#66258);
#13132=VERTEX_POINT('',#66262);
#13133=VERTEX_POINT('',#66264);
#13134=VERTEX_POINT('',#66268);
#13135=VERTEX_POINT('',#66272);
#13136=VERTEX_POINT('',#66274);
#13137=VERTEX_POINT('',#66278);
#13138=VERTEX_POINT('',#66282);
#13139=VERTEX_POINT('',#66284);
#13140=VERTEX_POINT('',#66288);
#13141=VERTEX_POINT('',#66292);
#13142=VERTEX_POINT('',#66294);
#13143=VERTEX_POINT('',#66298);
#13144=VERTEX_POINT('',#66302);
#13145=VERTEX_POINT('',#66304);
#13146=VERTEX_POINT('',#66308);
#13147=VERTEX_POINT('',#66312);
#13148=VERTEX_POINT('',#66314);
#13149=VERTEX_POINT('',#66318);
#13150=VERTEX_POINT('',#66322);
#13151=VERTEX_POINT('',#66324);
#13152=VERTEX_POINT('',#66328);
#13153=VERTEX_POINT('',#66332);
#13154=VERTEX_POINT('',#66334);
#13155=VERTEX_POINT('',#66338);
#13156=VERTEX_POINT('',#66342);
#13157=VERTEX_POINT('',#66344);
#13158=VERTEX_POINT('',#66348);
#13159=VERTEX_POINT('',#66352);
#13160=VERTEX_POINT('',#66357);
#13161=VERTEX_POINT('',#66361);
#13162=VERTEX_POINT('',#66363);
#13163=VERTEX_POINT('',#66367);
#13164=VERTEX_POINT('',#66373);
#13165=VERTEX_POINT('',#66375);
#13166=VERTEX_POINT('',#66379);
#13167=VERTEX_POINT('',#66385);
#13168=VERTEX_POINT('',#66387);
#13169=VERTEX_POINT('',#66391);
#13170=VERTEX_POINT('',#66397);
#13171=VERTEX_POINT('',#66399);
#13172=VERTEX_POINT('',#66403);
#13173=VERTEX_POINT('',#66409);
#13174=VERTEX_POINT('',#66411);
#13175=VERTEX_POINT('',#66415);
#13176=VERTEX_POINT('',#66421);
#13177=VERTEX_POINT('',#66423);
#13178=VERTEX_POINT('',#66427);
#13179=VERTEX_POINT('',#66433);
#13180=VERTEX_POINT('',#66435);
#13181=VERTEX_POINT('',#66439);
#13182=VERTEX_POINT('',#66445);
#13183=VERTEX_POINT('',#66447);
#13184=VERTEX_POINT('',#66451);
#13185=VERTEX_POINT('',#66457);
#13186=VERTEX_POINT('',#66459);
#13187=VERTEX_POINT('',#66463);
#13188=VERTEX_POINT('',#66469);
#13189=VERTEX_POINT('',#66471);
#13190=VERTEX_POINT('',#66475);
#13191=VERTEX_POINT('',#66481);
#13192=VERTEX_POINT('',#66483);
#13193=VERTEX_POINT('',#66487);
#13194=VERTEX_POINT('',#66493);
#13195=VERTEX_POINT('',#66495);
#13196=VERTEX_POINT('',#66499);
#13197=VERTEX_POINT('',#66505);
#13198=VERTEX_POINT('',#66507);
#13199=VERTEX_POINT('',#66511);
#13200=VERTEX_POINT('',#66517);
#13201=VERTEX_POINT('',#66519);
#13202=VERTEX_POINT('',#66523);
#13203=VERTEX_POINT('',#66529);
#13204=VERTEX_POINT('',#66531);
#13205=VERTEX_POINT('',#66535);
#13206=VERTEX_POINT('',#66541);
#13207=VERTEX_POINT('',#66543);
#13208=VERTEX_POINT('',#66547);
#13209=VERTEX_POINT('',#66553);
#13210=VERTEX_POINT('',#66555);
#13211=VERTEX_POINT('',#66559);
#13212=VERTEX_POINT('',#66563);
#13213=VERTEX_POINT('',#66567);
#13214=VERTEX_POINT('',#66569);
#13215=VERTEX_POINT('',#66573);
#13216=VERTEX_POINT('',#66579);
#13217=VERTEX_POINT('',#66581);
#13218=VERTEX_POINT('',#66585);
#13219=VERTEX_POINT('',#66591);
#13220=VERTEX_POINT('',#66593);
#13221=VERTEX_POINT('',#66597);
#13222=VERTEX_POINT('',#66603);
#13223=VERTEX_POINT('',#66605);
#13224=VERTEX_POINT('',#66609);
#13225=VERTEX_POINT('',#66615);
#13226=VERTEX_POINT('',#66617);
#13227=VERTEX_POINT('',#66621);
#13228=VERTEX_POINT('',#66627);
#13229=VERTEX_POINT('',#66629);
#13230=VERTEX_POINT('',#66633);
#13231=VERTEX_POINT('',#66639);
#13232=VERTEX_POINT('',#66641);
#13233=VERTEX_POINT('',#66645);
#13234=VERTEX_POINT('',#66651);
#13235=VERTEX_POINT('',#66653);
#13236=VERTEX_POINT('',#66657);
#13237=VERTEX_POINT('',#66663);
#13238=VERTEX_POINT('',#66665);
#13239=VERTEX_POINT('',#66669);
#13240=VERTEX_POINT('',#66675);
#13241=VERTEX_POINT('',#66677);
#13242=VERTEX_POINT('',#66681);
#13243=VERTEX_POINT('',#66687);
#13244=VERTEX_POINT('',#66689);
#13245=VERTEX_POINT('',#66693);
#13246=VERTEX_POINT('',#66699);
#13247=VERTEX_POINT('',#66701);
#13248=VERTEX_POINT('',#66705);
#13249=VERTEX_POINT('',#66711);
#13250=VERTEX_POINT('',#66713);
#13251=VERTEX_POINT('',#66717);
#13252=VERTEX_POINT('',#66723);
#13253=VERTEX_POINT('',#66725);
#13254=VERTEX_POINT('',#66729);
#13255=VERTEX_POINT('',#66735);
#13256=VERTEX_POINT('',#66737);
#13257=VERTEX_POINT('',#66741);
#13258=VERTEX_POINT('',#66747);
#13259=VERTEX_POINT('',#66749);
#13260=VERTEX_POINT('',#66753);
#13261=VERTEX_POINT('',#66759);
#13262=VERTEX_POINT('',#66761);
#13263=VERTEX_POINT('',#66765);
#13264=VERTEX_POINT('',#66771);
#13265=VERTEX_POINT('',#66773);
#13266=VERTEX_POINT('',#66777);
#13267=VERTEX_POINT('',#66785);
#13268=VERTEX_POINT('',#66786);
#13269=VERTEX_POINT('',#66788);
#13270=VERTEX_POINT('',#66790);
#13271=VERTEX_POINT('',#66792);
#13272=VERTEX_POINT('',#66794);
#13273=VERTEX_POINT('',#66798);
#13274=VERTEX_POINT('',#66799);
#13275=VERTEX_POINT('',#66803);
#13276=VERTEX_POINT('',#66807);
#13277=VERTEX_POINT('',#66811);
#13278=VERTEX_POINT('',#66815);
#13279=VERTEX_POINT('',#66822);
#13280=VERTEX_POINT('',#66838);
#13281=VERTEX_POINT('',#66839);
#13282=VERTEX_POINT('',#66841);
#13283=VERTEX_POINT('',#66992);
#13284=VERTEX_POINT('',#67097);
#13285=VERTEX_POINT('',#67098);
#13286=VERTEX_POINT('',#67515);
#13287=VERTEX_POINT('',#67516);
#13288=VERTEX_POINT('',#67518);
#13289=VERTEX_POINT('',#67561);
#13290=VERTEX_POINT('',#67783);
#13291=VERTEX_POINT('',#67784);
#13292=VERTEX_POINT('',#67786);
#13293=VERTEX_POINT('',#68179);
#13294=VERTEX_POINT('',#68180);
#13295=VERTEX_POINT('',#68182);
#13296=VERTEX_POINT('',#68413);
#13297=VERTEX_POINT('',#68615);
#13298=VERTEX_POINT('',#68616);
#13299=VERTEX_POINT('',#69037);
#13300=VERTEX_POINT('',#69038);
#13301=VERTEX_POINT('',#69040);
#13302=VERTEX_POINT('',#69249);
#13303=VERTEX_POINT('',#69471);
#13304=VERTEX_POINT('',#69472);
#13305=VERTEX_POINT('',#69903);
#13306=VERTEX_POINT('',#69904);
#13307=VERTEX_POINT('',#69906);
#13308=VERTEX_POINT('',#69942);
#13309=VERTEX_POINT('',#70146);
#13310=VERTEX_POINT('',#70147);
#13311=VERTEX_POINT('',#70149);
#13312=VERTEX_POINT('',#70518);
#13313=VERTEX_POINT('',#70519);
#13314=VERTEX_POINT('',#70521);
#13315=VERTEX_POINT('',#70739);
#13316=VERTEX_POINT('',#70785);
#13317=VERTEX_POINT('',#70786);
#13318=VERTEX_POINT('',#70998);
#13319=VERTEX_POINT('',#71231);
#13320=VERTEX_POINT('',#71232);
#13321=VERTEX_POINT('',#71234);
#13322=VERTEX_POINT('',#71650);
#13323=VERTEX_POINT('',#71651);
#13324=VERTEX_POINT('',#71849);
#13325=VERTEX_POINT('',#72065);
#13326=VERTEX_POINT('',#72066);
#13327=VERTEX_POINT('',#72068);
#13328=VERTEX_POINT('',#72502);
#13329=VERTEX_POINT('',#72503);
#13330=VERTEX_POINT('',#72912);
#13331=VERTEX_POINT('',#72913);
#13332=VERTEX_POINT('',#72915);
#13333=VERTEX_POINT('',#73122);
#13334=VERTEX_POINT('',#73167);
#13335=VERTEX_POINT('',#73168);
#13336=VERTEX_POINT('',#73380);
#13337=VERTEX_POINT('',#73535);
#13338=VERTEX_POINT('',#73536);
#13339=VERTEX_POINT('',#73538);
#13340=VERTEX_POINT('',#73743);
#13341=VERTEX_POINT('',#73946);
#13342=VERTEX_POINT('',#73947);
#13343=VERTEX_POINT('',#74009);
#13344=VERTEX_POINT('',#74011);
#13345=VERTEX_POINT('',#74017);
#13346=VERTEX_POINT('',#74196);
#13347=VERTEX_POINT('',#74372);
#13348=VERTEX_POINT('',#74545);
#13349=VERTEX_POINT('',#74721);
#13350=VERTEX_POINT('',#74897);
#13351=VERTEX_POINT('',#75073);
#13352=VERTEX_POINT('',#75246);
#13353=VERTEX_POINT('',#75422);
#13354=VERTEX_POINT('',#75598);
#13355=VERTEX_POINT('',#75771);
#13356=VERTEX_POINT('',#75944);
#13357=VERTEX_POINT('',#76120);
#13358=VERTEX_POINT('',#76293);
#13359=VERTEX_POINT('',#76466);
#13360=VERTEX_POINT('',#76639);
#13361=VERTEX_POINT('',#76812);
#13362=VERTEX_POINT('',#76982);
#13363=VERTEX_POINT('',#77155);
#13364=VERTEX_POINT('',#77331);
#13365=VERTEX_POINT('',#77369);
#13366=VERTEX_POINT('',#77371);
#13367=VERTEX_POINT('',#77379);
#13368=VERTEX_POINT('',#77390);
#13369=VERTEX_POINT('',#77563);
#13370=VERTEX_POINT('',#77733);
#13371=VERTEX_POINT('',#77906);
#13372=VERTEX_POINT('',#78079);
#13373=VERTEX_POINT('',#78252);
#13374=VERTEX_POINT('',#78425);
#13375=VERTEX_POINT('',#78598);
#13376=VERTEX_POINT('',#78771);
#13377=VERTEX_POINT('',#78944);
#13378=VERTEX_POINT('',#79117);
#13379=VERTEX_POINT('',#79290);
#13380=VERTEX_POINT('',#79460);
#13381=VERTEX_POINT('',#79633);
#13382=VERTEX_POINT('',#79806);
#13383=VERTEX_POINT('',#79979);
#13384=VERTEX_POINT('',#80152);
#13385=VERTEX_POINT('',#80498);
#13386=VERTEX_POINT('',#80683);
#13387=VERTEX_POINT('',#80820);
#13388=VERTEX_POINT('',#80821);
#13389=VERTEX_POINT('',#80899);
#13390=VERTEX_POINT('',#81496);
#13391=VERTEX_POINT('',#81581);
#13392=VERTEX_POINT('',#81582);
#13393=VERTEX_POINT('',#82174);
#13394=VERTEX_POINT('',#82178);
#13395=VERTEX_POINT('',#82181);
#13396=VERTEX_POINT('',#82186);
#13397=VERTEX_POINT('',#82187);
#13398=VERTEX_POINT('',#82189);
#13399=VERTEX_POINT('',#82191);
#13400=VERTEX_POINT('',#82197);
#13401=VERTEX_POINT('',#82198);
#13402=VERTEX_POINT('',#82207);
#13403=VERTEX_POINT('',#82208);
#13404=VERTEX_POINT('',#82212);
#13405=VERTEX_POINT('',#82214);
#13406=VERTEX_POINT('',#82218);
#13407=VERTEX_POINT('',#82222);
#13408=VERTEX_POINT('',#82224);
#13409=VERTEX_POINT('',#82228);
#13410=VERTEX_POINT('',#82232);
#13411=VERTEX_POINT('',#82234);
#13412=VERTEX_POINT('',#82238);
#13413=VERTEX_POINT('',#82242);
#13414=VERTEX_POINT('',#82244);
#13415=VERTEX_POINT('',#82248);
#13416=VERTEX_POINT('',#82252);
#13417=VERTEX_POINT('',#82254);
#13418=VERTEX_POINT('',#82258);
#13419=VERTEX_POINT('',#82262);
#13420=VERTEX_POINT('',#82264);
#13421=VERTEX_POINT('',#82268);
#13422=VERTEX_POINT('',#82272);
#13423=VERTEX_POINT('',#82274);
#13424=VERTEX_POINT('',#82278);
#13425=VERTEX_POINT('',#82282);
#13426=VERTEX_POINT('',#82284);
#13427=VERTEX_POINT('',#82288);
#13428=VERTEX_POINT('',#82292);
#13429=VERTEX_POINT('',#82294);
#13430=VERTEX_POINT('',#82298);
#13431=VERTEX_POINT('',#82302);
#13432=VERTEX_POINT('',#82304);
#13433=VERTEX_POINT('',#82308);
#13434=VERTEX_POINT('',#82312);
#13435=VERTEX_POINT('',#82314);
#13436=VERTEX_POINT('',#82318);
#13437=VERTEX_POINT('',#82322);
#13438=VERTEX_POINT('',#82324);
#13439=VERTEX_POINT('',#82328);
#13440=VERTEX_POINT('',#82332);
#13441=VERTEX_POINT('',#82334);
#13442=VERTEX_POINT('',#82338);
#13443=VERTEX_POINT('',#82342);
#13444=VERTEX_POINT('',#82344);
#13445=VERTEX_POINT('',#82348);
#13446=VERTEX_POINT('',#82352);
#13447=VERTEX_POINT('',#82354);
#13448=VERTEX_POINT('',#82358);
#13449=VERTEX_POINT('',#82362);
#13450=VERTEX_POINT('',#82364);
#13451=VERTEX_POINT('',#82368);
#13452=VERTEX_POINT('',#82372);
#13453=VERTEX_POINT('',#82374);
#13454=VERTEX_POINT('',#82378);
#13455=VERTEX_POINT('',#82382);
#13456=VERTEX_POINT('',#82384);
#13457=VERTEX_POINT('',#82388);
#13458=VERTEX_POINT('',#82393);
#13459=VERTEX_POINT('',#82395);
#13460=VERTEX_POINT('',#82399);
#13461=VERTEX_POINT('',#82403);
#13462=VERTEX_POINT('',#82405);
#13463=VERTEX_POINT('',#82409);
#13464=VERTEX_POINT('',#82413);
#13465=VERTEX_POINT('',#82415);
#13466=VERTEX_POINT('',#82419);
#13467=VERTEX_POINT('',#82423);
#13468=VERTEX_POINT('',#82425);
#13469=VERTEX_POINT('',#82429);
#13470=VERTEX_POINT('',#82433);
#13471=VERTEX_POINT('',#82435);
#13472=VERTEX_POINT('',#82439);
#13473=VERTEX_POINT('',#82443);
#13474=VERTEX_POINT('',#82445);
#13475=VERTEX_POINT('',#82449);
#13476=VERTEX_POINT('',#82453);
#13477=VERTEX_POINT('',#82455);
#13478=VERTEX_POINT('',#82459);
#13479=VERTEX_POINT('',#82463);
#13480=VERTEX_POINT('',#82465);
#13481=VERTEX_POINT('',#82469);
#13482=VERTEX_POINT('',#82473);
#13483=VERTEX_POINT('',#82475);
#13484=VERTEX_POINT('',#82479);
#13485=VERTEX_POINT('',#82483);
#13486=VERTEX_POINT('',#82485);
#13487=VERTEX_POINT('',#82489);
#13488=VERTEX_POINT('',#82493);
#13489=VERTEX_POINT('',#82495);
#13490=VERTEX_POINT('',#82499);
#13491=VERTEX_POINT('',#82503);
#13492=VERTEX_POINT('',#82505);
#13493=VERTEX_POINT('',#82509);
#13494=VERTEX_POINT('',#82513);
#13495=VERTEX_POINT('',#82515);
#13496=VERTEX_POINT('',#82519);
#13497=VERTEX_POINT('',#82523);
#13498=VERTEX_POINT('',#82525);
#13499=VERTEX_POINT('',#82529);
#13500=VERTEX_POINT('',#82533);
#13501=VERTEX_POINT('',#82535);
#13502=VERTEX_POINT('',#82539);
#13503=VERTEX_POINT('',#82543);
#13504=VERTEX_POINT('',#82545);
#13505=VERTEX_POINT('',#82549);
#13506=VERTEX_POINT('',#82553);
#13507=VERTEX_POINT('',#82558);
#13508=VERTEX_POINT('',#82562);
#13509=VERTEX_POINT('',#82564);
#13510=VERTEX_POINT('',#82568);
#13511=VERTEX_POINT('',#82574);
#13512=VERTEX_POINT('',#82576);
#13513=VERTEX_POINT('',#82580);
#13514=VERTEX_POINT('',#82586);
#13515=VERTEX_POINT('',#82588);
#13516=VERTEX_POINT('',#82592);
#13517=VERTEX_POINT('',#82598);
#13518=VERTEX_POINT('',#82600);
#13519=VERTEX_POINT('',#82604);
#13520=VERTEX_POINT('',#82610);
#13521=VERTEX_POINT('',#82612);
#13522=VERTEX_POINT('',#82616);
#13523=VERTEX_POINT('',#82622);
#13524=VERTEX_POINT('',#82624);
#13525=VERTEX_POINT('',#82628);
#13526=VERTEX_POINT('',#82634);
#13527=VERTEX_POINT('',#82636);
#13528=VERTEX_POINT('',#82640);
#13529=VERTEX_POINT('',#82646);
#13530=VERTEX_POINT('',#82648);
#13531=VERTEX_POINT('',#82652);
#13532=VERTEX_POINT('',#82658);
#13533=VERTEX_POINT('',#82660);
#13534=VERTEX_POINT('',#82664);
#13535=VERTEX_POINT('',#82670);
#13536=VERTEX_POINT('',#82672);
#13537=VERTEX_POINT('',#82676);
#13538=VERTEX_POINT('',#82682);
#13539=VERTEX_POINT('',#82684);
#13540=VERTEX_POINT('',#82688);
#13541=VERTEX_POINT('',#82694);
#13542=VERTEX_POINT('',#82696);
#13543=VERTEX_POINT('',#82700);
#13544=VERTEX_POINT('',#82706);
#13545=VERTEX_POINT('',#82708);
#13546=VERTEX_POINT('',#82712);
#13547=VERTEX_POINT('',#82718);
#13548=VERTEX_POINT('',#82720);
#13549=VERTEX_POINT('',#82724);
#13550=VERTEX_POINT('',#82730);
#13551=VERTEX_POINT('',#82732);
#13552=VERTEX_POINT('',#82736);
#13553=VERTEX_POINT('',#82742);
#13554=VERTEX_POINT('',#82744);
#13555=VERTEX_POINT('',#82748);
#13556=VERTEX_POINT('',#82754);
#13557=VERTEX_POINT('',#82756);
#13558=VERTEX_POINT('',#82760);
#13559=VERTEX_POINT('',#82764);
#13560=VERTEX_POINT('',#82768);
#13561=VERTEX_POINT('',#82770);
#13562=VERTEX_POINT('',#82774);
#13563=VERTEX_POINT('',#82780);
#13564=VERTEX_POINT('',#82782);
#13565=VERTEX_POINT('',#82786);
#13566=VERTEX_POINT('',#82792);
#13567=VERTEX_POINT('',#82794);
#13568=VERTEX_POINT('',#82798);
#13569=VERTEX_POINT('',#82804);
#13570=VERTEX_POINT('',#82806);
#13571=VERTEX_POINT('',#82810);
#13572=VERTEX_POINT('',#82816);
#13573=VERTEX_POINT('',#82818);
#13574=VERTEX_POINT('',#82822);
#13575=VERTEX_POINT('',#82828);
#13576=VERTEX_POINT('',#82830);
#13577=VERTEX_POINT('',#82834);
#13578=VERTEX_POINT('',#82840);
#13579=VERTEX_POINT('',#82842);
#13580=VERTEX_POINT('',#82846);
#13581=VERTEX_POINT('',#82852);
#13582=VERTEX_POINT('',#82854);
#13583=VERTEX_POINT('',#82858);
#13584=VERTEX_POINT('',#82864);
#13585=VERTEX_POINT('',#82866);
#13586=VERTEX_POINT('',#82870);
#13587=VERTEX_POINT('',#82876);
#13588=VERTEX_POINT('',#82878);
#13589=VERTEX_POINT('',#82882);
#13590=VERTEX_POINT('',#82888);
#13591=VERTEX_POINT('',#82890);
#13592=VERTEX_POINT('',#82894);
#13593=VERTEX_POINT('',#82900);
#13594=VERTEX_POINT('',#82902);
#13595=VERTEX_POINT('',#82906);
#13596=VERTEX_POINT('',#82912);
#13597=VERTEX_POINT('',#82914);
#13598=VERTEX_POINT('',#82918);
#13599=VERTEX_POINT('',#82924);
#13600=VERTEX_POINT('',#82926);
#13601=VERTEX_POINT('',#82930);
#13602=VERTEX_POINT('',#82936);
#13603=VERTEX_POINT('',#82938);
#13604=VERTEX_POINT('',#82942);
#13605=VERTEX_POINT('',#82948);
#13606=VERTEX_POINT('',#82950);
#13607=VERTEX_POINT('',#82954);
#13608=VERTEX_POINT('',#82960);
#13609=VERTEX_POINT('',#82962);
#13610=VERTEX_POINT('',#82966);
#13611=VERTEX_POINT('',#82972);
#13612=VERTEX_POINT('',#82974);
#13613=VERTEX_POINT('',#82978);
#13614=VERTEX_POINT('',#82986);
#13615=VERTEX_POINT('',#82987);
#13616=VERTEX_POINT('',#82989);
#13617=VERTEX_POINT('',#82991);
#13618=VERTEX_POINT('',#82993);
#13619=VERTEX_POINT('',#82995);
#13620=VERTEX_POINT('',#82999);
#13621=VERTEX_POINT('',#83000);
#13622=VERTEX_POINT('',#83004);
#13623=VERTEX_POINT('',#83008);
#13624=VERTEX_POINT('',#83012);
#13625=VERTEX_POINT('',#83016);
#13626=VERTEX_POINT('',#83023);
#13627=VERTEX_POINT('',#83039);
#13628=VERTEX_POINT('',#83041);
#13629=VERTEX_POINT('',#83045);
#13630=VERTEX_POINT('',#83048);
#13631=VERTEX_POINT('',#83052);
#13632=VERTEX_POINT('',#83056);
#13633=VERTEX_POINT('',#83062);
#13634=VERTEX_POINT('',#83064);
#13635=VERTEX_POINT('',#83068);
#13636=VERTEX_POINT('',#83072);
#13637=VERTEX_POINT('',#83075);
#13638=VERTEX_POINT('',#83077);
#13639=VERTEX_POINT('',#83081);
#13640=VERTEX_POINT('',#83085);
#13641=VERTEX_POINT('',#83088);
#13642=VERTEX_POINT('',#83093);
#13643=VERTEX_POINT('',#83094);
#13644=VERTEX_POINT('',#83098);
#13645=VERTEX_POINT('',#83102);
#13646=VERTEX_POINT('',#83106);
#13647=VERTEX_POINT('',#83110);
#13648=VERTEX_POINT('',#83119);
#13649=VERTEX_POINT('',#83121);
#13650=VERTEX_POINT('',#83125);
#13651=VERTEX_POINT('',#83129);
#13652=VERTEX_POINT('',#83133);
#13653=VERTEX_POINT('',#83137);
#13654=EDGE_CURVE('',#11051,#11051,#10299,.T.);
#13655=EDGE_CURVE('',#11051,#11052,#5277,.T.);
#13656=EDGE_CURVE('',#11052,#11052,#10300,.T.);
#13657=EDGE_CURVE('',#11051,#11053,#5278,.T.);
#13658=EDGE_CURVE('',#11053,#11054,#10301,.T.);
#13659=EDGE_CURVE('',#11054,#11053,#10302,.T.);
#13660=EDGE_CURVE('',#11055,#11056,#5279,.T.);
#13661=EDGE_CURVE('',#11057,#11055,#5280,.T.);
#13662=EDGE_CURVE('',#11058,#11057,#5281,.T.);
#13663=EDGE_CURVE('',#11058,#11056,#5282,.T.);
#13664=EDGE_CURVE('',#11059,#11059,#10303,.T.);
#13665=EDGE_CURVE('',#11059,#11060,#5283,.T.);
#13666=EDGE_CURVE('',#11060,#11060,#10304,.T.);
#13667=EDGE_CURVE('',#11059,#11061,#5284,.T.);
#13668=EDGE_CURVE('',#11061,#11062,#10305,.T.);
#13669=EDGE_CURVE('',#11062,#11061,#10306,.T.);
#13670=EDGE_CURVE('',#11063,#11064,#5285,.T.);
#13671=EDGE_CURVE('',#11063,#11065,#5286,.T.);
#13672=EDGE_CURVE('',#11066,#11065,#5287,.T.);
#13673=EDGE_CURVE('',#11066,#11064,#5288,.T.);
#13674=EDGE_CURVE('',#11067,#11054,#5289,.T.);
#13675=EDGE_CURVE('',#11068,#11062,#5290,.T.);
#13676=EDGE_CURVE('',#11069,#11069,#10307,.T.);
#13677=EDGE_CURVE('',#11069,#11070,#5291,.T.);
#13678=EDGE_CURVE('',#11070,#11070,#10308,.T.);
#13679=EDGE_CURVE('',#11069,#11071,#5292,.T.);
#13680=EDGE_CURVE('',#11071,#11072,#10309,.T.);
#13681=EDGE_CURVE('',#11072,#11071,#10310,.T.);
#13682=EDGE_CURVE('',#11073,#11074,#5293,.T.);
#13683=EDGE_CURVE('',#11073,#11075,#5294,.T.);
#13684=EDGE_CURVE('',#11076,#11075,#5295,.T.);
#13685=EDGE_CURVE('',#11076,#11074,#5296,.T.);
#13686=EDGE_CURVE('',#11077,#11077,#10311,.T.);
#13687=EDGE_CURVE('',#11077,#11078,#5297,.T.);
#13688=EDGE_CURVE('',#11078,#11078,#10312,.T.);
#13689=EDGE_CURVE('',#11077,#11079,#5298,.T.);
#13690=EDGE_CURVE('',#11079,#11080,#10313,.T.);
#13691=EDGE_CURVE('',#11080,#11079,#10314,.T.);
#13692=EDGE_CURVE('',#11081,#11082,#5299,.T.);
#13693=EDGE_CURVE('',#11083,#11081,#5300,.T.);
#13694=EDGE_CURVE('',#11084,#11083,#5301,.T.);
#13695=EDGE_CURVE('',#11084,#11082,#5302,.T.);
#13696=EDGE_CURVE('',#11085,#11072,#5303,.T.);
#13697=EDGE_CURVE('',#11086,#11080,#5304,.T.);
#13698=EDGE_CURVE('',#11087,#11087,#10315,.T.);
#13699=EDGE_CURVE('',#11087,#11088,#5305,.T.);
#13700=EDGE_CURVE('',#11088,#11088,#10316,.T.);
#13701=EDGE_CURVE('',#11089,#11089,#10317,.T.);
#13702=EDGE_CURVE('',#11089,#11090,#5306,.T.);
#13703=EDGE_CURVE('',#11090,#11090,#10318,.T.);
#13704=EDGE_CURVE('',#11091,#11091,#10319,.T.);
#13705=EDGE_CURVE('',#11091,#11092,#5307,.T.);
#13706=EDGE_CURVE('',#11092,#11092,#10320,.T.);
#13707=EDGE_CURVE('',#11093,#11093,#10321,.T.);
#13708=EDGE_CURVE('',#11093,#11094,#5308,.T.);
#13709=EDGE_CURVE('',#11094,#11094,#10322,.T.);
#13710=EDGE_CURVE('',#11095,#11095,#10323,.T.);
#13711=EDGE_CURVE('',#11095,#11096,#5309,.T.);
#13712=EDGE_CURVE('',#11096,#11096,#10324,.T.);
#13713=EDGE_CURVE('',#11097,#11098,#5310,.T.);
#13714=EDGE_CURVE('',#11099,#11097,#5311,.T.);
#13715=EDGE_CURVE('',#11100,#11099,#5312,.T.);
#13716=EDGE_CURVE('',#11101,#11100,#5313,.T.);
#13717=EDGE_CURVE('',#11102,#11101,#5314,.T.);
#13718=EDGE_CURVE('',#11103,#11102,#5315,.T.);
#13719=EDGE_CURVE('',#11104,#11103,#5316,.T.);
#13720=EDGE_CURVE('',#11105,#11104,#5317,.T.);
#13721=EDGE_CURVE('',#11106,#11105,#5318,.T.);
#13722=EDGE_CURVE('',#11107,#11106,#5319,.T.);
#13723=EDGE_CURVE('',#11108,#11107,#5320,.T.);
#13724=EDGE_CURVE('',#11109,#11108,#5321,.T.);
#13725=EDGE_CURVE('',#11110,#11109,#5322,.T.);
#13726=EDGE_CURVE('',#11111,#11110,#5323,.T.);
#13727=EDGE_CURVE('',#11112,#11111,#5324,.T.);
#13728=EDGE_CURVE('',#11113,#11112,#5325,.T.);
#13729=EDGE_CURVE('',#11114,#11113,#5326,.T.);
#13730=EDGE_CURVE('',#11115,#11114,#5327,.T.);
#13731=EDGE_CURVE('',#11116,#11115,#5328,.T.);
#13732=EDGE_CURVE('',#11098,#11116,#5329,.T.);
#13733=EDGE_CURVE('',#11117,#11117,#10325,.T.);
#13734=EDGE_CURVE('',#11118,#11118,#10326,.T.);
#13735=EDGE_CURVE('',#11119,#11119,#10327,.T.);
#13736=EDGE_CURVE('',#11120,#11120,#10328,.T.);
#13737=EDGE_CURVE('',#11095,#11121,#5330,.T.);
#13738=EDGE_CURVE('',#11121,#11121,#10329,.T.);
#13739=EDGE_CURVE('',#11122,#11122,#10330,.T.);
#13740=EDGE_CURVE('',#11122,#11120,#5331,.T.);
#13741=EDGE_CURVE('',#11122,#11123,#5332,.T.);
#13742=EDGE_CURVE('',#11123,#11123,#10331,.T.);
#13743=EDGE_CURVE('',#11124,#11124,#10332,.T.);
#13744=EDGE_CURVE('',#11124,#11117,#5333,.T.);
#13745=EDGE_CURVE('',#11124,#11125,#5334,.T.);
#13746=EDGE_CURVE('',#11125,#11125,#10333,.T.);
#13747=EDGE_CURVE('',#11126,#11126,#10334,.T.);
#13748=EDGE_CURVE('',#11126,#11119,#5335,.T.);
#13749=EDGE_CURVE('',#11126,#11127,#5336,.T.);
#13750=EDGE_CURVE('',#11127,#11127,#10335,.T.);
#13751=EDGE_CURVE('',#11128,#11128,#10336,.T.);
#13752=EDGE_CURVE('',#11128,#11118,#5337,.T.);
#13753=EDGE_CURVE('',#11128,#11129,#5338,.T.);
#13754=EDGE_CURVE('',#11129,#11129,#10337,.T.);
#13755=EDGE_CURVE('',#11107,#11130,#5339,.T.);
#13756=EDGE_CURVE('',#11130,#11131,#5340,.T.);
#13757=EDGE_CURVE('',#11131,#11108,#5341,.T.);
#13758=EDGE_CURVE('',#11106,#11064,#5342,.T.);
#13759=EDGE_CURVE('',#11064,#11130,#5343,.T.);
#13760=EDGE_CURVE('',#11105,#11063,#5344,.T.);
#13761=EDGE_CURVE('',#11132,#11133,#5345,.T.);
#13762=EDGE_CURVE('',#11133,#11114,#5346,.T.);
#13763=EDGE_CURVE('',#11113,#11132,#5347,.T.);
#13764=EDGE_CURVE('',#11104,#11134,#5348,.T.);
#13765=EDGE_CURVE('',#11134,#11063,#5349,.T.);
#13766=EDGE_CURVE('',#11102,#11056,#5350,.T.);
#13767=EDGE_CURVE('',#11056,#11135,#5351,.T.);
#13768=EDGE_CURVE('',#11135,#11103,#5352,.T.);
#13769=EDGE_CURVE('',#11101,#11055,#5353,.T.);
#13770=EDGE_CURVE('',#11136,#11137,#5354,.T.);
#13771=EDGE_CURVE('',#11137,#11097,#5355,.T.);
#13772=EDGE_CURVE('',#11098,#11136,#5356,.T.);
#13773=EDGE_CURVE('',#11100,#11138,#5357,.T.);
#13774=EDGE_CURVE('',#11138,#11055,#5358,.T.);
#13775=EDGE_CURVE('',#11137,#11139,#5359,.T.);
#13776=EDGE_CURVE('',#11139,#11099,#5360,.T.);
#13777=EDGE_CURVE('',#11139,#11138,#5361,.T.);
#13778=EDGE_CURVE('',#11074,#11136,#5362,.T.);
#13779=EDGE_CURVE('',#11116,#11074,#5363,.T.);
#13780=EDGE_CURVE('',#11115,#11073,#5364,.T.);
#13781=EDGE_CURVE('',#11135,#11134,#5365,.T.);
#13782=EDGE_CURVE('',#11133,#11073,#5366,.T.);
#13783=EDGE_CURVE('',#11082,#11132,#5367,.T.);
#13784=EDGE_CURVE('',#11112,#11082,#5368,.T.);
#13785=EDGE_CURVE('',#11111,#11081,#5369,.T.);
#13786=EDGE_CURVE('',#11140,#11081,#5370,.T.);
#13787=EDGE_CURVE('',#11110,#11140,#5371,.T.);
#13788=EDGE_CURVE('',#11131,#11141,#5372,.T.);
#13789=EDGE_CURVE('',#11141,#11109,#5373,.T.);
#13790=EDGE_CURVE('',#11141,#11140,#5374,.T.);
#13791=EDGE_CURVE('',#11142,#11066,#5375,.T.);
#13792=EDGE_CURVE('',#11142,#11130,#5376,.T.);
#13793=EDGE_CURVE('',#11143,#11134,#5377,.T.);
#13794=EDGE_CURVE('',#11065,#11143,#5378,.T.);
#13795=EDGE_CURVE('',#11144,#11135,#5379,.T.);
#13796=EDGE_CURVE('',#11143,#11144,#5380,.T.);
#13797=EDGE_CURVE('',#11144,#11058,#5381,.T.);
#13798=EDGE_CURVE('',#11138,#11145,#5382,.T.);
#13799=EDGE_CURVE('',#11057,#11145,#5383,.T.);
#13800=EDGE_CURVE('',#11146,#11139,#5384,.T.);
#13801=EDGE_CURVE('',#11145,#11146,#5385,.T.);
#13802=EDGE_CURVE('',#11147,#11137,#5386,.T.);
#13803=EDGE_CURVE('',#11146,#11147,#5387,.T.);
#13804=EDGE_CURVE('',#11148,#11136,#5388,.T.);
#13805=EDGE_CURVE('',#11147,#11148,#5389,.T.);
#13806=EDGE_CURVE('',#11149,#11141,#5390,.T.);
#13807=EDGE_CURVE('',#11150,#11149,#5391,.T.);
#13808=EDGE_CURVE('',#11140,#11150,#5392,.T.);
#13809=EDGE_CURVE('',#11151,#11142,#5393,.T.);
#13810=EDGE_CURVE('',#11151,#11131,#5394,.T.);
#13811=EDGE_CURVE('',#11149,#11151,#5395,.T.);
#13812=EDGE_CURVE('',#11148,#11076,#5396,.T.);
#13813=EDGE_CURVE('',#11083,#11150,#5397,.T.);
#13814=EDGE_CURVE('',#11075,#11152,#5398,.T.);
#13815=EDGE_CURVE('',#11152,#11153,#5399,.T.);
#13816=EDGE_CURVE('',#11153,#11084,#5400,.T.);
#13817=EDGE_CURVE('',#11153,#11132,#5401,.T.);
#13818=EDGE_CURVE('',#11152,#11133,#5402,.T.);
#13819=EDGE_CURVE('',#11154,#11154,#10338,.T.);
#13820=EDGE_CURVE('',#11154,#11155,#5403,.T.);
#13821=EDGE_CURVE('',#11155,#11155,#10339,.T.);
#13822=EDGE_CURVE('',#11156,#11157,#5404,.T.);
#13823=EDGE_CURVE('',#11158,#11157,#10340,.T.);
#13824=EDGE_CURVE('',#11158,#11159,#5405,.T.);
#13825=EDGE_CURVE('',#11160,#11159,#10341,.T.);
#13826=EDGE_CURVE('',#11160,#11161,#5406,.T.);
#13827=EDGE_CURVE('',#11161,#11162,#5407,.T.);
#13828=EDGE_CURVE('',#11162,#11163,#5408,.T.);
#13829=EDGE_CURVE('',#11163,#11164,#5409,.T.);
#13830=EDGE_CURVE('',#11164,#11165,#5410,.T.);
#13831=EDGE_CURVE('',#11165,#11166,#5411,.T.);
#13832=EDGE_CURVE('',#11166,#11167,#5412,.T.);
#13833=EDGE_CURVE('',#11167,#11168,#5413,.T.);
#13834=EDGE_CURVE('',#11168,#11169,#5414,.T.);
#13835=EDGE_CURVE('',#11170,#11169,#10342,.T.);
#13836=EDGE_CURVE('',#11170,#11171,#5415,.T.);
#13837=EDGE_CURVE('',#11172,#11171,#10343,.T.);
#13838=EDGE_CURVE('',#11172,#11173,#5416,.T.);
#13839=EDGE_CURVE('',#11174,#11173,#5417,.T.);
#13840=EDGE_CURVE('',#11175,#11174,#5418,.T.);
#13841=EDGE_CURVE('',#11176,#11175,#5419,.T.);
#13842=EDGE_CURVE('',#11176,#11177,#5420,.T.);
#13843=EDGE_CURVE('',#11178,#11177,#5421,.T.);
#13844=EDGE_CURVE('',#11179,#11178,#5422,.T.);
#13845=EDGE_CURVE('',#11156,#11179,#5423,.T.);
#13846=EDGE_CURVE('',#11180,#11180,#10344,.T.);
#13847=EDGE_CURVE('',#11181,#11181,#10345,.T.);
#13848=EDGE_CURVE('',#11182,#11182,#10346,.T.);
#13849=EDGE_CURVE('',#11183,#11183,#10347,.T.);
#13850=EDGE_CURVE('',#11184,#11184,#10348,.T.);
#13851=EDGE_CURVE('',#11185,#11185,#10349,.T.);
#13852=EDGE_CURVE('',#11186,#11187,#5424,.T.);
#13853=EDGE_CURVE('',#11187,#11188,#5425,.T.);
#13854=EDGE_CURVE('',#11188,#11189,#10350,.T.);
#13855=EDGE_CURVE('',#11189,#11190,#5426,.T.);
#13856=EDGE_CURVE('',#11190,#11191,#10351,.T.);
#13857=EDGE_CURVE('',#11191,#11192,#5427,.T.);
#13858=EDGE_CURVE('',#11192,#11193,#5428,.T.);
#13859=EDGE_CURVE('',#11193,#11194,#10352,.T.);
#13860=EDGE_CURVE('',#11194,#11195,#5429,.T.);
#13861=EDGE_CURVE('',#11195,#11196,#5430,.T.);
#13862=EDGE_CURVE('',#11196,#11197,#10353,.T.);
#13863=EDGE_CURVE('',#11197,#11198,#5431,.T.);
#13864=EDGE_CURVE('',#11198,#11199,#10354,.T.);
#13865=EDGE_CURVE('',#11199,#11200,#5432,.T.);
#13866=EDGE_CURVE('',#11200,#11201,#5433,.T.);
#13867=EDGE_CURVE('',#11201,#11186,#10355,.T.);
#13868=EDGE_CURVE('',#11202,#11202,#10356,.T.);
#13869=EDGE_CURVE('',#11203,#11203,#10357,.T.);
#13870=EDGE_CURVE('',#11203,#11154,#5434,.T.);
#13871=EDGE_CURVE('',#11204,#11204,#10358,.T.);
#13872=EDGE_CURVE('',#11204,#11180,#5435,.T.);
#13873=EDGE_CURVE('',#11205,#11205,#10359,.T.);
#13874=EDGE_CURVE('',#11205,#11204,#5436,.T.);
#13875=EDGE_CURVE('',#11206,#11206,#10360,.T.);
#13876=EDGE_CURVE('',#11206,#11202,#5437,.T.);
#13877=EDGE_CURVE('',#11207,#11207,#10361,.T.);
#13878=EDGE_CURVE('',#11207,#11206,#5438,.T.);
#13879=EDGE_CURVE('',#11208,#11208,#10362,.T.);
#13880=EDGE_CURVE('',#11208,#11181,#5439,.T.);
#13881=EDGE_CURVE('',#11209,#11209,#10363,.T.);
#13882=EDGE_CURVE('',#11209,#11208,#5440,.T.);
#13883=EDGE_CURVE('',#11210,#11210,#10364,.T.);
#13884=EDGE_CURVE('',#11210,#11211,#5441,.T.);
#13885=EDGE_CURVE('',#11211,#11211,#10365,.T.);
#13886=EDGE_CURVE('',#11212,#11213,#5442,.T.);
#13887=EDGE_CURVE('',#11214,#11212,#10366,.T.);
#13888=EDGE_CURVE('',#11215,#11214,#5443,.T.);
#13889=EDGE_CURVE('',#11216,#11215,#10367,.T.);
#13890=EDGE_CURVE('',#11217,#11216,#5444,.T.);
#13891=EDGE_CURVE('',#11218,#11217,#5445,.T.);
#13892=EDGE_CURVE('',#11219,#11218,#5446,.T.);
#13893=EDGE_CURVE('',#11220,#11219,#5447,.T.);
#13894=EDGE_CURVE('',#11221,#11220,#5448,.T.);
#13895=EDGE_CURVE('',#11222,#11221,#5449,.T.);
#13896=EDGE_CURVE('',#11223,#11222,#5450,.T.);
#13897=EDGE_CURVE('',#11224,#11223,#5451,.T.);
#13898=EDGE_CURVE('',#11225,#11224,#5452,.T.);
#13899=EDGE_CURVE('',#11226,#11225,#10368,.T.);
#13900=EDGE_CURVE('',#11227,#11226,#5453,.T.);
#13901=EDGE_CURVE('',#11228,#11227,#10369,.T.);
#13902=EDGE_CURVE('',#11229,#11228,#5454,.T.);
#13903=EDGE_CURVE('',#11230,#11229,#5455,.T.);
#13904=EDGE_CURVE('',#11231,#11230,#5456,.T.);
#13905=EDGE_CURVE('',#11232,#11231,#5457,.T.);
#13906=EDGE_CURVE('',#11233,#11232,#5458,.T.);
#13907=EDGE_CURVE('',#11234,#11233,#5459,.T.);
#13908=EDGE_CURVE('',#11235,#11234,#5460,.T.);
#13909=EDGE_CURVE('',#11213,#11235,#5461,.T.);
#13910=EDGE_CURVE('',#11236,#11236,#10370,.T.);
#13911=EDGE_CURVE('',#11237,#11238,#5462,.T.);
#13912=EDGE_CURVE('',#11239,#11237,#10371,.T.);
#13913=EDGE_CURVE('',#11240,#11239,#5463,.T.);
#13914=EDGE_CURVE('',#11241,#11240,#10372,.T.);
#13915=EDGE_CURVE('',#11242,#11241,#5464,.T.);
#13916=EDGE_CURVE('',#11243,#11242,#5465,.T.);
#13917=EDGE_CURVE('',#11244,#11243,#10373,.T.);
#13918=EDGE_CURVE('',#11245,#11244,#5466,.T.);
#13919=EDGE_CURVE('',#11246,#11245,#5467,.T.);
#13920=EDGE_CURVE('',#11247,#11246,#10374,.T.);
#13921=EDGE_CURVE('',#11248,#11247,#5468,.T.);
#13922=EDGE_CURVE('',#11249,#11248,#10375,.T.);
#13923=EDGE_CURVE('',#11250,#11249,#5469,.T.);
#13924=EDGE_CURVE('',#11251,#11250,#5470,.T.);
#13925=EDGE_CURVE('',#11252,#11251,#10376,.T.);
#13926=EDGE_CURVE('',#11238,#11252,#5471,.T.);
#13927=EDGE_CURVE('',#11253,#11253,#10377,.T.);
#13928=EDGE_CURVE('',#11254,#11254,#10378,.T.);
#13929=EDGE_CURVE('',#11210,#11185,#5472,.T.);
#13930=EDGE_CURVE('',#11255,#11255,#10379,.T.);
#13931=EDGE_CURVE('',#11255,#11254,#5473,.T.);
#13932=EDGE_CURVE('',#11255,#11184,#5474,.T.);
#13933=EDGE_CURVE('',#11256,#11256,#10380,.T.);
#13934=EDGE_CURVE('',#11256,#11236,#5475,.T.);
#13935=EDGE_CURVE('',#11256,#11183,#5476,.T.);
#13936=EDGE_CURVE('',#11257,#11257,#10381,.T.);
#13937=EDGE_CURVE('',#11257,#11253,#5477,.T.);
#13938=EDGE_CURVE('',#11257,#11182,#5478,.T.);
#13939=EDGE_CURVE('',#11232,#11258,#5479,.T.);
#13940=EDGE_CURVE('',#11258,#11259,#5480,.T.);
#13941=EDGE_CURVE('',#11233,#11259,#5481,.T.);
#13942=EDGE_CURVE('',#11231,#11260,#5482,.T.);
#13943=EDGE_CURVE('',#11260,#11258,#5483,.T.);
#13944=EDGE_CURVE('',#11230,#11261,#5484,.T.);
#13945=EDGE_CURVE('',#11261,#11260,#5485,.T.);
#13946=EDGE_CURVE('',#11229,#11262,#5486,.T.);
#13947=EDGE_CURVE('',#11262,#11261,#5487,.T.);
#13948=EDGE_CURVE('',#11263,#11264,#5488,.T.);
#13949=EDGE_CURVE('',#11264,#11225,#5489,.T.);
#13950=EDGE_CURVE('',#11224,#11263,#5490,.T.);
#13951=EDGE_CURVE('',#11223,#11265,#5491,.T.);
#13952=EDGE_CURVE('',#11265,#11263,#5492,.T.);
#13953=EDGE_CURVE('',#11222,#11266,#5493,.T.);
#13954=EDGE_CURVE('',#11266,#11265,#5494,.T.);
#13955=EDGE_CURVE('',#11221,#11267,#5495,.T.);
#13956=EDGE_CURVE('',#11267,#11266,#5496,.T.);
#13957=EDGE_CURVE('',#11220,#11268,#5497,.T.);
#13958=EDGE_CURVE('',#11268,#11267,#5498,.T.);
#13959=EDGE_CURVE('',#11269,#11268,#5499,.T.);
#13960=EDGE_CURVE('',#11219,#11269,#5500,.T.);
#13961=EDGE_CURVE('',#11270,#11269,#5501,.T.);
#13962=EDGE_CURVE('',#11218,#11270,#5502,.T.);
#13963=EDGE_CURVE('',#11271,#11270,#5503,.T.);
#13964=EDGE_CURVE('',#11217,#11271,#5504,.T.);
#13965=EDGE_CURVE('',#11272,#11273,#5505,.T.);
#13966=EDGE_CURVE('',#11273,#11212,#5506,.T.);
#13967=EDGE_CURVE('',#11213,#11272,#5507,.T.);
#13968=EDGE_CURVE('',#11274,#11214,#5508,.T.);
#13969=EDGE_CURVE('',#11273,#11274,#10382,.T.);
#13970=EDGE_CURVE('',#11275,#11215,#5509,.T.);
#13971=EDGE_CURVE('',#11274,#11275,#5510,.T.);
#13972=EDGE_CURVE('',#11276,#11216,#5511,.T.);
#13973=EDGE_CURVE('',#11275,#11276,#10383,.T.);
#13974=EDGE_CURVE('',#11276,#11271,#5512,.T.);
#13975=EDGE_CURVE('',#11277,#11226,#5513,.T.);
#13976=EDGE_CURVE('',#11264,#11277,#10384,.T.);
#13977=EDGE_CURVE('',#11278,#11227,#5514,.T.);
#13978=EDGE_CURVE('',#11277,#11278,#5515,.T.);
#13979=EDGE_CURVE('',#11279,#11228,#5516,.T.);
#13980=EDGE_CURVE('',#11278,#11279,#10385,.T.);
#13981=EDGE_CURVE('',#11279,#11262,#5517,.T.);
#13982=EDGE_CURVE('',#11280,#11272,#5518,.T.);
#13983=EDGE_CURVE('',#11235,#11280,#5519,.T.);
#13984=EDGE_CURVE('',#11281,#11280,#5520,.T.);
#13985=EDGE_CURVE('',#11234,#11281,#5521,.T.);
#13986=EDGE_CURVE('',#11259,#11281,#5522,.T.);
#13987=EDGE_CURVE('',#11174,#11265,#5523,.T.);
#13988=EDGE_CURVE('',#11263,#11173,#5524,.T.);
#13989=EDGE_CURVE('',#11175,#11266,#5525,.T.);
#13990=EDGE_CURVE('',#11176,#11267,#5526,.T.);
#13991=EDGE_CURVE('',#11268,#11177,#5527,.T.);
#13992=EDGE_CURVE('',#11178,#11269,#5528,.T.);
#13993=EDGE_CURVE('',#11179,#11270,#5529,.T.);
#13994=EDGE_CURVE('',#11156,#11271,#5530,.T.);
#13995=EDGE_CURVE('',#11157,#11276,#5531,.T.);
#13996=EDGE_CURVE('',#11158,#11275,#5532,.T.);
#13997=EDGE_CURVE('',#11159,#11274,#5533,.T.);
#13998=EDGE_CURVE('',#11160,#11273,#5534,.T.);
#13999=EDGE_CURVE('',#11272,#11161,#5535,.T.);
#14000=EDGE_CURVE('',#11282,#11283,#5536,.T.);
#14001=EDGE_CURVE('',#11283,#11251,#5537,.T.);
#14002=EDGE_CURVE('',#11250,#11282,#5538,.T.);
#14003=EDGE_CURVE('',#11284,#11285,#5539,.T.);
#14004=EDGE_CURVE('',#11285,#11246,#5540,.T.);
#14005=EDGE_CURVE('',#11245,#11284,#5541,.T.);
#14006=EDGE_CURVE('',#11286,#11287,#5542,.T.);
#14007=EDGE_CURVE('',#11287,#11243,#5543,.T.);
#14008=EDGE_CURVE('',#11242,#11286,#5544,.T.);
#14009=EDGE_CURVE('',#11288,#11244,#5545,.T.);
#14010=EDGE_CURVE('',#11287,#11288,#10386,.T.);
#14011=EDGE_CURVE('',#11288,#11284,#5546,.T.);
#14012=EDGE_CURVE('',#11289,#11290,#5547,.T.);
#14013=EDGE_CURVE('',#11290,#11237,#5548,.T.);
#14014=EDGE_CURVE('',#11238,#11289,#5549,.T.);
#14015=EDGE_CURVE('',#11291,#11239,#5550,.T.);
#14016=EDGE_CURVE('',#11290,#11291,#10387,.T.);
#14017=EDGE_CURVE('',#11292,#11240,#5551,.T.);
#14018=EDGE_CURVE('',#11291,#11292,#5552,.T.);
#14019=EDGE_CURVE('',#11293,#11241,#5553,.T.);
#14020=EDGE_CURVE('',#11292,#11293,#10388,.T.);
#14021=EDGE_CURVE('',#11293,#11286,#5554,.T.);
#14022=EDGE_CURVE('',#11294,#11247,#5555,.T.);
#14023=EDGE_CURVE('',#11285,#11294,#10389,.T.);
#14024=EDGE_CURVE('',#11295,#11248,#5556,.T.);
#14025=EDGE_CURVE('',#11294,#11295,#5557,.T.);
#14026=EDGE_CURVE('',#11296,#11249,#5558,.T.);
#14027=EDGE_CURVE('',#11295,#11296,#10390,.T.);
#14028=EDGE_CURVE('',#11296,#11282,#5559,.T.);
#14029=EDGE_CURVE('',#11297,#11252,#5560,.T.);
#14030=EDGE_CURVE('',#11283,#11297,#10391,.T.);
#14031=EDGE_CURVE('',#11297,#11289,#5561,.T.);
#14032=EDGE_CURVE('',#11201,#11288,#5562,.T.);
#14033=EDGE_CURVE('',#11284,#11200,#5563,.T.);
#14034=EDGE_CURVE('',#11186,#11287,#5564,.T.);
#14035=EDGE_CURVE('',#11187,#11286,#5565,.T.);
#14036=EDGE_CURVE('',#11188,#11293,#5566,.T.);
#14037=EDGE_CURVE('',#11189,#11292,#5567,.T.);
#14038=EDGE_CURVE('',#11190,#11291,#5568,.T.);
#14039=EDGE_CURVE('',#11191,#11290,#5569,.T.);
#14040=EDGE_CURVE('',#11289,#11192,#5570,.T.);
#14041=EDGE_CURVE('',#11193,#11297,#5571,.T.);
#14042=EDGE_CURVE('',#11195,#11282,#5572,.T.);
#14043=EDGE_CURVE('',#11194,#11283,#5573,.T.);
#14044=EDGE_CURVE('',#11199,#11285,#5574,.T.);
#14045=EDGE_CURVE('',#11196,#11296,#5575,.T.);
#14046=EDGE_CURVE('',#11198,#11294,#5576,.T.);
#14047=EDGE_CURVE('',#11197,#11295,#5577,.T.);
#14048=EDGE_CURVE('',#11162,#11280,#5578,.T.);
#14049=EDGE_CURVE('',#11164,#11259,#5579,.T.);
#14050=EDGE_CURVE('',#11163,#11281,#5580,.T.);
#14051=EDGE_CURVE('',#11258,#11165,#5581,.T.);
#14052=EDGE_CURVE('',#11168,#11262,#5582,.T.);
#14053=EDGE_CURVE('',#11167,#11261,#5583,.T.);
#14054=EDGE_CURVE('',#11166,#11260,#5584,.T.);
#14055=EDGE_CURVE('',#11169,#11279,#5585,.T.);
#14056=EDGE_CURVE('',#11170,#11278,#5586,.T.);
#14057=EDGE_CURVE('',#11171,#11277,#5587,.T.);
#14058=EDGE_CURVE('',#11172,#11264,#5588,.T.);
#14059=EDGE_CURVE('',#11298,#11298,#10392,.T.);
#14060=EDGE_CURVE('',#11298,#11299,#5589,.T.);
#14061=EDGE_CURVE('',#11299,#11299,#10393,.T.);
#14062=EDGE_CURVE('',#11300,#11300,#10394,.T.);
#14063=EDGE_CURVE('',#11300,#11301,#5590,.T.);
#14064=EDGE_CURVE('',#11301,#11301,#10395,.T.);
#14065=EDGE_CURVE('',#11302,#11302,#10396,.T.);
#14066=EDGE_CURVE('',#11302,#11303,#5591,.T.);
#14067=EDGE_CURVE('',#11303,#11303,#10397,.T.);
#14068=EDGE_CURVE('',#11304,#11304,#10398,.T.);
#14069=EDGE_CURVE('',#11304,#11305,#5592,.T.);
#14070=EDGE_CURVE('',#11305,#11305,#10399,.T.);
#14071=EDGE_CURVE('',#11306,#11306,#10400,.T.);
#14072=EDGE_CURVE('',#11306,#11307,#5593,.T.);
#14073=EDGE_CURVE('',#11307,#11307,#10401,.T.);
#14074=EDGE_CURVE('',#11308,#11308,#10402,.T.);
#14075=EDGE_CURVE('',#11308,#11309,#5594,.T.);
#14076=EDGE_CURVE('',#11309,#11309,#10403,.T.);
#14077=EDGE_CURVE('',#11308,#11310,#5595,.T.);
#14078=EDGE_CURVE('',#11310,#11310,#10404,.T.);
#14079=EDGE_CURVE('',#11311,#11311,#10405,.T.);
#14080=EDGE_CURVE('',#11312,#11310,#5596,.T.);
#14081=EDGE_CURVE('',#11313,#11313,#10406,.T.);
#14082=EDGE_CURVE('',#11313,#11314,#5597,.T.);
#14083=EDGE_CURVE('',#11314,#11314,#10407,.T.);
#14084=EDGE_CURVE('',#11314,#11311,#5598,.T.);
#14085=EDGE_CURVE('',#11315,#11315,#10408,.T.);
#14086=EDGE_CURVE('',#11315,#11316,#5599,.T.);
#14087=EDGE_CURVE('',#11316,#11316,#10409,.T.);
#14088=EDGE_CURVE('',#11317,#11317,#10410,.T.);
#14089=EDGE_CURVE('',#11316,#11317,#5600,.T.);
#14090=EDGE_CURVE('',#11318,#11319,#5601,.T.);
#14091=EDGE_CURVE('',#11318,#11320,#5602,.T.);
#14092=EDGE_CURVE('',#11321,#11320,#5603,.T.);
#14093=EDGE_CURVE('',#11319,#11321,#5604,.T.);
#14094=EDGE_CURVE('',#11319,#11322,#10411,.T.);
#14095=EDGE_CURVE('',#11323,#11321,#10412,.T.);
#14096=EDGE_CURVE('',#11322,#11323,#5605,.T.);
#14097=EDGE_CURVE('',#11324,#11325,#10413,.T.);
#14098=EDGE_CURVE('',#11324,#11326,#5606,.T.);
#14099=EDGE_CURVE('',#11327,#11326,#10414,.T.);
#14100=EDGE_CURVE('',#11325,#11327,#5607,.T.);
#14101=EDGE_CURVE('',#11325,#11328,#5608,.T.);
#14102=EDGE_CURVE('',#11329,#11327,#5609,.T.);
#14103=EDGE_CURVE('',#11328,#11329,#5610,.T.);
#14104=EDGE_CURVE('',#11328,#11330,#10415,.T.);
#14105=EDGE_CURVE('',#11331,#11329,#10416,.T.);
#14106=EDGE_CURVE('',#11330,#11331,#5611,.T.);
#14107=EDGE_CURVE('',#11332,#11318,#10417,.T.);
#14108=EDGE_CURVE('',#11332,#11333,#5612,.T.);
#14109=EDGE_CURVE('',#11320,#11333,#10418,.T.);
#14110=EDGE_CURVE('',#11333,#11331,#5613,.T.);
#14111=EDGE_CURVE('',#11326,#11323,#5614,.T.);
#14112=EDGE_CURVE('',#11322,#11334,#5615,.T.);
#14113=EDGE_CURVE('',#11334,#11335,#10419,.T.);
#14114=EDGE_CURVE('',#11335,#11336,#5616,.T.);
#14115=EDGE_CURVE('',#11336,#11337,#10420,.T.);
#14116=EDGE_CURVE('',#11337,#11332,#5617,.T.);
#14117=EDGE_CURVE('',#11330,#11338,#5618,.T.);
#14118=EDGE_CURVE('',#11338,#11339,#10421,.T.);
#14119=EDGE_CURVE('',#11339,#11340,#5619,.T.);
#14120=EDGE_CURVE('',#11340,#11341,#10422,.T.);
#14121=EDGE_CURVE('',#11341,#11324,#5620,.T.);
#14122=EDGE_CURVE('',#11342,#11343,#10423,.T.);
#14123=EDGE_CURVE('',#11343,#11344,#5621,.T.);
#14124=EDGE_CURVE('',#11344,#11345,#10424,.T.);
#14125=EDGE_CURVE('',#11345,#11346,#5622,.T.);
#14126=EDGE_CURVE('',#11347,#11346,#10425,.T.);
#14127=EDGE_CURVE('',#11347,#11348,#5623,.T.);
#14128=EDGE_CURVE('',#11349,#11348,#10426,.T.);
#14129=EDGE_CURVE('',#11349,#11342,#5624,.T.);
#14130=EDGE_CURVE('',#11347,#11336,#5625,.T.);
#14131=EDGE_CURVE('',#11348,#11335,#5626,.T.);
#14132=EDGE_CURVE('',#11349,#11334,#5627,.T.);
#14133=EDGE_CURVE('',#11350,#11341,#5628,.T.);
#14134=EDGE_CURVE('',#11351,#11350,#5629,.T.);
#14135=EDGE_CURVE('',#11342,#11351,#5630,.T.);
#14136=EDGE_CURVE('',#11352,#11350,#10427,.T.);
#14137=EDGE_CURVE('',#11352,#11340,#5631,.T.);
#14138=EDGE_CURVE('',#11352,#11353,#5632,.T.);
#14139=EDGE_CURVE('',#11353,#11339,#5633,.T.);
#14140=EDGE_CURVE('',#11354,#11353,#10428,.T.);
#14141=EDGE_CURVE('',#11354,#11338,#5634,.T.);
#14142=EDGE_CURVE('',#11354,#11355,#5635,.T.);
#14143=EDGE_CURVE('',#11346,#11337,#5636,.T.);
#14144=EDGE_CURVE('',#11355,#11345,#5637,.T.);
#14145=EDGE_CURVE('',#11356,#11351,#10429,.T.);
#14146=EDGE_CURVE('',#11355,#11357,#10430,.T.);
#14147=EDGE_CURVE('',#11357,#11356,#5638,.T.);
#14148=EDGE_CURVE('',#11345,#11358,#10431,.T.);
#14149=EDGE_CURVE('',#11358,#11359,#5639,.T.);
#14150=EDGE_CURVE('',#11359,#11355,#10432,.T.);
#14151=EDGE_CURVE('',#11360,#11361,#5640,.T.);
#14152=EDGE_CURVE('',#11360,#11344,#5641,.T.);
#14153=EDGE_CURVE('',#11361,#11343,#5642,.T.);
#14154=EDGE_CURVE('',#11362,#11361,#10433,.T.);
#14155=EDGE_CURVE('',#11363,#11342,#10434,.T.);
#14156=EDGE_CURVE('',#11362,#11363,#5643,.T.);
#14157=EDGE_CURVE('',#11362,#11364,#5644,.T.);
#14158=EDGE_CURVE('',#11365,#11363,#5645,.T.);
#14159=EDGE_CURVE('',#11364,#11365,#5646,.T.);
#14160=EDGE_CURVE('',#11366,#11364,#10435,.T.);
#14161=EDGE_CURVE('',#11351,#11365,#10436,.T.);
#14162=EDGE_CURVE('',#11366,#11356,#5647,.T.);
#14163=EDGE_CURVE('',#11366,#11367,#5648,.T.);
#14164=EDGE_CURVE('',#11367,#11357,#5649,.T.);
#14165=EDGE_CURVE('',#11368,#11367,#10437,.T.);
#14166=EDGE_CURVE('',#11368,#11359,#5650,.T.);
#14167=EDGE_CURVE('',#11368,#11369,#5651,.T.);
#14168=EDGE_CURVE('',#11369,#11358,#5652,.T.);
#14169=EDGE_CURVE('',#11360,#11369,#10438,.T.);
#14170=EDGE_CURVE('',#11370,#11371,#5653,.T.);
#14171=EDGE_CURVE('',#11372,#11370,#5654,.T.);
#14172=EDGE_CURVE('',#11373,#11372,#5655,.T.);
#14173=EDGE_CURVE('',#11373,#11371,#5656,.T.);
#14174=EDGE_CURVE('',#11374,#11375,#10439,.T.);
#14175=EDGE_CURVE('',#11374,#11376,#5657,.T.);
#14176=EDGE_CURVE('',#11377,#11376,#10440,.T.);
#14177=EDGE_CURVE('',#11375,#11377,#5658,.T.);
#14178=EDGE_CURVE('',#11378,#11375,#508,.T.);
#14179=EDGE_CURVE('',#11379,#11377,#509,.T.);
#14180=EDGE_CURVE('',#11378,#11379,#5659,.T.);
#14181=EDGE_CURVE('',#11380,#11381,#5660,.T.);
#14182=EDGE_CURVE('',#11380,#11378,#5661,.T.);
#14183=EDGE_CURVE('',#11381,#11379,#5662,.T.);
#14184=EDGE_CURVE('',#11373,#11374,#510,.T.);
#14185=EDGE_CURVE('',#11376,#11372,#511,.T.);
#14186=EDGE_CURVE('',#11382,#11380,#10441,.T.);
#14187=EDGE_CURVE('',#11383,#11382,#5663,.T.);
#14188=EDGE_CURVE('',#11383,#11384,#512,.T.);
#14189=EDGE_CURVE('',#11384,#11385,#10442,.T.);
#14190=EDGE_CURVE('',#11386,#11385,#513,.T.);
#14191=EDGE_CURVE('',#11387,#11386,#5664,.T.);
#14192=EDGE_CURVE('',#11388,#11387,#10443,.T.);
#14193=EDGE_CURVE('',#11389,#11388,#5665,.T.);
#14194=EDGE_CURVE('',#11389,#11390,#514,.T.);
#14195=EDGE_CURVE('',#11390,#11391,#10444,.T.);
#14196=EDGE_CURVE('',#11392,#11391,#515,.T.);
#14197=EDGE_CURVE('',#11393,#11392,#5666,.T.);
#14198=EDGE_CURVE('',#11394,#11393,#10445,.T.);
#14199=EDGE_CURVE('',#11395,#11394,#5667,.T.);
#14200=EDGE_CURVE('',#11395,#11396,#516,.T.);
#14201=EDGE_CURVE('',#11396,#11397,#10446,.T.);
#14202=EDGE_CURVE('',#11398,#11397,#517,.T.);
#14203=EDGE_CURVE('',#11399,#11398,#5668,.T.);
#14204=EDGE_CURVE('',#11400,#11399,#10447,.T.);
#14205=EDGE_CURVE('',#11401,#11400,#5669,.T.);
#14206=EDGE_CURVE('',#11401,#11402,#518,.T.);
#14207=EDGE_CURVE('',#11402,#11403,#10448,.T.);
#14208=EDGE_CURVE('',#11404,#11403,#519,.T.);
#14209=EDGE_CURVE('',#11405,#11404,#5670,.T.);
#14210=EDGE_CURVE('',#11406,#11405,#10449,.T.);
#14211=EDGE_CURVE('',#11407,#11406,#5671,.T.);
#14212=EDGE_CURVE('',#11407,#11408,#520,.T.);
#14213=EDGE_CURVE('',#11408,#11409,#10450,.T.);
#14214=EDGE_CURVE('',#11410,#11409,#521,.T.);
#14215=EDGE_CURVE('',#11411,#11410,#5672,.T.);
#14216=EDGE_CURVE('',#11412,#11411,#10451,.T.);
#14217=EDGE_CURVE('',#11413,#11412,#5673,.T.);
#14218=EDGE_CURVE('',#11413,#11414,#522,.T.);
#14219=EDGE_CURVE('',#11414,#11415,#10452,.T.);
#14220=EDGE_CURVE('',#11416,#11415,#523,.T.);
#14221=EDGE_CURVE('',#11417,#11416,#5674,.T.);
#14222=EDGE_CURVE('',#11418,#11417,#10453,.T.);
#14223=EDGE_CURVE('',#11419,#11418,#5675,.T.);
#14224=EDGE_CURVE('',#11419,#11420,#524,.T.);
#14225=EDGE_CURVE('',#11420,#11421,#10454,.T.);
#14226=EDGE_CURVE('',#11422,#11421,#525,.T.);
#14227=EDGE_CURVE('',#11423,#11422,#5676,.T.);
#14228=EDGE_CURVE('',#11424,#11423,#10455,.T.);
#14229=EDGE_CURVE('',#11425,#11424,#5677,.T.);
#14230=EDGE_CURVE('',#11425,#11426,#526,.T.);
#14231=EDGE_CURVE('',#11426,#11427,#10456,.T.);
#14232=EDGE_CURVE('',#11428,#11427,#527,.T.);
#14233=EDGE_CURVE('',#11429,#11428,#5678,.T.);
#14234=EDGE_CURVE('',#11430,#11429,#10457,.T.);
#14235=EDGE_CURVE('',#11431,#11430,#5679,.T.);
#14236=EDGE_CURVE('',#11431,#11432,#528,.T.);
#14237=EDGE_CURVE('',#11432,#11433,#10458,.T.);
#14238=EDGE_CURVE('',#11434,#11433,#529,.T.);
#14239=EDGE_CURVE('',#11435,#11434,#5680,.T.);
#14240=EDGE_CURVE('',#11436,#11435,#10459,.T.);
#14241=EDGE_CURVE('',#11437,#11436,#5681,.T.);
#14242=EDGE_CURVE('',#11437,#11438,#530,.T.);
#14243=EDGE_CURVE('',#11438,#11439,#10460,.T.);
#14244=EDGE_CURVE('',#11440,#11439,#531,.T.);
#14245=EDGE_CURVE('',#11441,#11440,#5682,.T.);
#14246=EDGE_CURVE('',#11442,#11441,#10461,.T.);
#14247=EDGE_CURVE('',#11443,#11442,#5683,.T.);
#14248=EDGE_CURVE('',#11443,#11444,#532,.T.);
#14249=EDGE_CURVE('',#11444,#11445,#10462,.T.);
#14250=EDGE_CURVE('',#11446,#11445,#533,.T.);
#14251=EDGE_CURVE('',#11447,#11446,#5684,.T.);
#14252=EDGE_CURVE('',#11448,#11447,#10463,.T.);
#14253=EDGE_CURVE('',#11449,#11448,#5685,.T.);
#14254=EDGE_CURVE('',#11449,#11450,#534,.T.);
#14255=EDGE_CURVE('',#11450,#11451,#10464,.T.);
#14256=EDGE_CURVE('',#11452,#11451,#535,.T.);
#14257=EDGE_CURVE('',#11453,#11452,#5686,.T.);
#14258=EDGE_CURVE('',#11454,#11453,#10465,.T.);
#14259=EDGE_CURVE('',#11455,#11454,#5687,.T.);
#14260=EDGE_CURVE('',#11455,#11456,#536,.T.);
#14261=EDGE_CURVE('',#11456,#11457,#10466,.T.);
#14262=EDGE_CURVE('',#11458,#11457,#537,.T.);
#14263=EDGE_CURVE('',#11459,#11458,#5688,.T.);
#14264=EDGE_CURVE('',#11460,#11459,#10467,.T.);
#14265=EDGE_CURVE('',#11461,#11460,#5689,.T.);
#14266=EDGE_CURVE('',#11461,#11462,#538,.T.);
#14267=EDGE_CURVE('',#11462,#11463,#10468,.T.);
#14268=EDGE_CURVE('',#11464,#11463,#539,.T.);
#14269=EDGE_CURVE('',#11465,#11464,#5690,.T.);
#14270=EDGE_CURVE('',#11466,#11465,#10469,.T.);
#14271=EDGE_CURVE('',#11467,#11466,#5691,.T.);
#14272=EDGE_CURVE('',#11467,#11468,#540,.T.);
#14273=EDGE_CURVE('',#11468,#11469,#10470,.T.);
#14274=EDGE_CURVE('',#11470,#11469,#541,.T.);
#14275=EDGE_CURVE('',#11471,#11470,#5692,.T.);
#14276=EDGE_CURVE('',#11371,#11471,#10471,.T.);
#14277=EDGE_CURVE('',#11472,#11472,#10472,.T.);
#14278=EDGE_CURVE('',#11473,#11381,#10473,.T.);
#14279=EDGE_CURVE('',#11473,#11382,#5693,.T.);
#14280=EDGE_CURVE('',#11474,#11473,#5694,.T.);
#14281=EDGE_CURVE('',#11383,#11474,#5695,.T.);
#14282=EDGE_CURVE('',#11384,#11475,#5696,.T.);
#14283=EDGE_CURVE('',#11476,#11475,#10474,.T.);
#14284=EDGE_CURVE('',#11385,#11476,#5697,.T.);
#14285=EDGE_CURVE('',#11477,#11476,#542,.T.);
#14286=EDGE_CURVE('',#11386,#11477,#5698,.T.);
#14287=EDGE_CURVE('',#11387,#11478,#5699,.T.);
#14288=EDGE_CURVE('',#11478,#11477,#5700,.T.);
#14289=EDGE_CURVE('',#11475,#11474,#543,.T.);
#14290=EDGE_CURVE('',#11479,#11478,#10475,.T.);
#14291=EDGE_CURVE('',#11479,#11388,#5701,.T.);
#14292=EDGE_CURVE('',#11480,#11479,#5702,.T.);
#14293=EDGE_CURVE('',#11389,#11480,#5703,.T.);
#14294=EDGE_CURVE('',#11390,#11481,#5704,.T.);
#14295=EDGE_CURVE('',#11482,#11481,#10476,.T.);
#14296=EDGE_CURVE('',#11391,#11482,#5705,.T.);
#14297=EDGE_CURVE('',#11483,#11482,#544,.T.);
#14298=EDGE_CURVE('',#11392,#11483,#5706,.T.);
#14299=EDGE_CURVE('',#11393,#11484,#5707,.T.);
#14300=EDGE_CURVE('',#11484,#11483,#5708,.T.);
#14301=EDGE_CURVE('',#11481,#11480,#545,.T.);
#14302=EDGE_CURVE('',#11485,#11484,#10477,.T.);
#14303=EDGE_CURVE('',#11485,#11394,#5709,.T.);
#14304=EDGE_CURVE('',#11486,#11485,#5710,.T.);
#14305=EDGE_CURVE('',#11395,#11486,#5711,.T.);
#14306=EDGE_CURVE('',#11396,#11487,#5712,.T.);
#14307=EDGE_CURVE('',#11488,#11487,#10478,.T.);
#14308=EDGE_CURVE('',#11397,#11488,#5713,.T.);
#14309=EDGE_CURVE('',#11489,#11488,#546,.T.);
#14310=EDGE_CURVE('',#11398,#11489,#5714,.T.);
#14311=EDGE_CURVE('',#11399,#11490,#5715,.T.);
#14312=EDGE_CURVE('',#11490,#11489,#5716,.T.);
#14313=EDGE_CURVE('',#11487,#11486,#547,.T.);
#14314=EDGE_CURVE('',#11491,#11490,#10479,.T.);
#14315=EDGE_CURVE('',#11491,#11400,#5717,.T.);
#14316=EDGE_CURVE('',#11492,#11491,#5718,.T.);
#14317=EDGE_CURVE('',#11401,#11492,#5719,.T.);
#14318=EDGE_CURVE('',#11402,#11493,#5720,.T.);
#14319=EDGE_CURVE('',#11494,#11493,#10480,.T.);
#14320=EDGE_CURVE('',#11403,#11494,#5721,.T.);
#14321=EDGE_CURVE('',#11495,#11494,#548,.T.);
#14322=EDGE_CURVE('',#11404,#11495,#5722,.T.);
#14323=EDGE_CURVE('',#11405,#11496,#5723,.T.);
#14324=EDGE_CURVE('',#11496,#11495,#5724,.T.);
#14325=EDGE_CURVE('',#11493,#11492,#549,.T.);
#14326=EDGE_CURVE('',#11497,#11496,#10481,.T.);
#14327=EDGE_CURVE('',#11497,#11406,#5725,.T.);
#14328=EDGE_CURVE('',#11498,#11497,#5726,.T.);
#14329=EDGE_CURVE('',#11407,#11498,#5727,.T.);
#14330=EDGE_CURVE('',#11408,#11499,#5728,.T.);
#14331=EDGE_CURVE('',#11500,#11499,#10482,.T.);
#14332=EDGE_CURVE('',#11409,#11500,#5729,.T.);
#14333=EDGE_CURVE('',#11501,#11500,#550,.T.);
#14334=EDGE_CURVE('',#11410,#11501,#5730,.T.);
#14335=EDGE_CURVE('',#11411,#11502,#5731,.T.);
#14336=EDGE_CURVE('',#11502,#11501,#5732,.T.);
#14337=EDGE_CURVE('',#11499,#11498,#551,.T.);
#14338=EDGE_CURVE('',#11503,#11502,#10483,.T.);
#14339=EDGE_CURVE('',#11503,#11412,#5733,.T.);
#14340=EDGE_CURVE('',#11504,#11503,#5734,.T.);
#14341=EDGE_CURVE('',#11413,#11504,#5735,.T.);
#14342=EDGE_CURVE('',#11414,#11505,#5736,.T.);
#14343=EDGE_CURVE('',#11506,#11505,#10484,.T.);
#14344=EDGE_CURVE('',#11415,#11506,#5737,.T.);
#14345=EDGE_CURVE('',#11507,#11506,#552,.T.);
#14346=EDGE_CURVE('',#11416,#11507,#5738,.T.);
#14347=EDGE_CURVE('',#11417,#11508,#5739,.T.);
#14348=EDGE_CURVE('',#11508,#11507,#5740,.T.);
#14349=EDGE_CURVE('',#11505,#11504,#553,.T.);
#14350=EDGE_CURVE('',#11509,#11508,#10485,.T.);
#14351=EDGE_CURVE('',#11509,#11418,#5741,.T.);
#14352=EDGE_CURVE('',#11510,#11509,#5742,.T.);
#14353=EDGE_CURVE('',#11419,#11510,#5743,.T.);
#14354=EDGE_CURVE('',#11420,#11511,#5744,.T.);
#14355=EDGE_CURVE('',#11512,#11511,#10486,.T.);
#14356=EDGE_CURVE('',#11421,#11512,#5745,.T.);
#14357=EDGE_CURVE('',#11513,#11512,#554,.T.);
#14358=EDGE_CURVE('',#11422,#11513,#5746,.T.);
#14359=EDGE_CURVE('',#11423,#11514,#5747,.T.);
#14360=EDGE_CURVE('',#11514,#11513,#5748,.T.);
#14361=EDGE_CURVE('',#11511,#11510,#555,.T.);
#14362=EDGE_CURVE('',#11515,#11514,#10487,.T.);
#14363=EDGE_CURVE('',#11515,#11424,#5749,.T.);
#14364=EDGE_CURVE('',#11516,#11515,#5750,.T.);
#14365=EDGE_CURVE('',#11425,#11516,#5751,.T.);
#14366=EDGE_CURVE('',#11426,#11517,#5752,.T.);
#14367=EDGE_CURVE('',#11518,#11517,#10488,.T.);
#14368=EDGE_CURVE('',#11427,#11518,#5753,.T.);
#14369=EDGE_CURVE('',#11519,#11518,#556,.T.);
#14370=EDGE_CURVE('',#11428,#11519,#5754,.T.);
#14371=EDGE_CURVE('',#11429,#11520,#5755,.T.);
#14372=EDGE_CURVE('',#11520,#11519,#5756,.T.);
#14373=EDGE_CURVE('',#11517,#11516,#557,.T.);
#14374=EDGE_CURVE('',#11521,#11520,#10489,.T.);
#14375=EDGE_CURVE('',#11521,#11430,#5757,.T.);
#14376=EDGE_CURVE('',#11522,#11521,#5758,.T.);
#14377=EDGE_CURVE('',#11431,#11522,#5759,.T.);
#14378=EDGE_CURVE('',#11432,#11523,#5760,.T.);
#14379=EDGE_CURVE('',#11524,#11523,#10490,.T.);
#14380=EDGE_CURVE('',#11433,#11524,#5761,.T.);
#14381=EDGE_CURVE('',#11525,#11524,#558,.T.);
#14382=EDGE_CURVE('',#11434,#11525,#5762,.T.);
#14383=EDGE_CURVE('',#11435,#11526,#5763,.T.);
#14384=EDGE_CURVE('',#11526,#11525,#5764,.T.);
#14385=EDGE_CURVE('',#11523,#11522,#559,.T.);
#14386=EDGE_CURVE('',#11527,#11526,#10491,.T.);
#14387=EDGE_CURVE('',#11527,#11436,#5765,.T.);
#14388=EDGE_CURVE('',#11528,#11527,#5766,.T.);
#14389=EDGE_CURVE('',#11437,#11528,#5767,.T.);
#14390=EDGE_CURVE('',#11438,#11529,#5768,.T.);
#14391=EDGE_CURVE('',#11530,#11529,#10492,.T.);
#14392=EDGE_CURVE('',#11439,#11530,#5769,.T.);
#14393=EDGE_CURVE('',#11531,#11530,#560,.T.);
#14394=EDGE_CURVE('',#11440,#11531,#5770,.T.);
#14395=EDGE_CURVE('',#11441,#11532,#5771,.T.);
#14396=EDGE_CURVE('',#11532,#11531,#5772,.T.);
#14397=EDGE_CURVE('',#11529,#11528,#561,.T.);
#14398=EDGE_CURVE('',#11533,#11532,#10493,.T.);
#14399=EDGE_CURVE('',#11533,#11442,#5773,.T.);
#14400=EDGE_CURVE('',#11534,#11533,#5774,.T.);
#14401=EDGE_CURVE('',#11443,#11534,#5775,.T.);
#14402=EDGE_CURVE('',#11444,#11535,#5776,.T.);
#14403=EDGE_CURVE('',#11536,#11535,#10494,.T.);
#14404=EDGE_CURVE('',#11445,#11536,#5777,.T.);
#14405=EDGE_CURVE('',#11537,#11536,#562,.T.);
#14406=EDGE_CURVE('',#11446,#11537,#5778,.T.);
#14407=EDGE_CURVE('',#11447,#11538,#5779,.T.);
#14408=EDGE_CURVE('',#11538,#11537,#5780,.T.);
#14409=EDGE_CURVE('',#11535,#11534,#563,.T.);
#14410=EDGE_CURVE('',#11539,#11538,#10495,.T.);
#14411=EDGE_CURVE('',#11539,#11448,#5781,.T.);
#14412=EDGE_CURVE('',#11540,#11539,#5782,.T.);
#14413=EDGE_CURVE('',#11449,#11540,#5783,.T.);
#14414=EDGE_CURVE('',#11450,#11541,#5784,.T.);
#14415=EDGE_CURVE('',#11542,#11541,#10496,.T.);
#14416=EDGE_CURVE('',#11451,#11542,#5785,.T.);
#14417=EDGE_CURVE('',#11543,#11542,#564,.T.);
#14418=EDGE_CURVE('',#11452,#11543,#5786,.T.);
#14419=EDGE_CURVE('',#11453,#11544,#5787,.T.);
#14420=EDGE_CURVE('',#11544,#11543,#5788,.T.);
#14421=EDGE_CURVE('',#11541,#11540,#565,.T.);
#14422=EDGE_CURVE('',#11545,#11544,#10497,.T.);
#14423=EDGE_CURVE('',#11545,#11454,#5789,.T.);
#14424=EDGE_CURVE('',#11546,#11545,#5790,.T.);
#14425=EDGE_CURVE('',#11455,#11546,#5791,.T.);
#14426=EDGE_CURVE('',#11456,#11547,#5792,.T.);
#14427=EDGE_CURVE('',#11548,#11547,#10498,.T.);
#14428=EDGE_CURVE('',#11457,#11548,#5793,.T.);
#14429=EDGE_CURVE('',#11549,#11548,#566,.T.);
#14430=EDGE_CURVE('',#11458,#11549,#5794,.T.);
#14431=EDGE_CURVE('',#11459,#11550,#5795,.T.);
#14432=EDGE_CURVE('',#11550,#11549,#5796,.T.);
#14433=EDGE_CURVE('',#11547,#11546,#567,.T.);
#14434=EDGE_CURVE('',#11551,#11550,#10499,.T.);
#14435=EDGE_CURVE('',#11551,#11460,#5797,.T.);
#14436=EDGE_CURVE('',#11465,#11552,#5798,.T.);
#14437=EDGE_CURVE('',#11464,#11553,#5799,.T.);
#14438=EDGE_CURVE('',#11552,#11553,#5800,.T.);
#14439=EDGE_CURVE('',#11554,#11551,#5801,.T.);
#14440=EDGE_CURVE('',#11461,#11554,#5802,.T.);
#14441=EDGE_CURVE('',#11462,#11555,#5803,.T.);
#14442=EDGE_CURVE('',#11556,#11555,#10500,.T.);
#14443=EDGE_CURVE('',#11463,#11556,#5804,.T.);
#14444=EDGE_CURVE('',#11553,#11556,#568,.T.);
#14445=EDGE_CURVE('',#11555,#11554,#569,.T.);
#14446=EDGE_CURVE('',#11370,#11557,#10501,.T.);
#14447=EDGE_CURVE('',#11557,#11558,#5805,.T.);
#14448=EDGE_CURVE('',#11558,#11559,#570,.T.);
#14449=EDGE_CURVE('',#11559,#11560,#10502,.T.);
#14450=EDGE_CURVE('',#11560,#11561,#571,.T.);
#14451=EDGE_CURVE('',#11561,#11562,#5806,.T.);
#14452=EDGE_CURVE('',#11562,#11552,#10503,.T.);
#14453=EDGE_CURVE('',#11563,#11563,#10504,.T.);
#14454=EDGE_CURVE('',#11471,#11557,#5807,.T.);
#14455=EDGE_CURVE('',#11470,#11558,#5808,.T.);
#14456=EDGE_CURVE('',#11468,#11560,#5809,.T.);
#14457=EDGE_CURVE('',#11469,#11559,#5810,.T.);
#14458=EDGE_CURVE('',#11562,#11466,#5811,.T.);
#14459=EDGE_CURVE('',#11467,#11561,#5812,.T.);
#14460=EDGE_CURVE('',#11564,#11564,#10505,.T.);
#14461=EDGE_CURVE('',#11565,#11565,#10506,.T.);
#14462=EDGE_CURVE('',#11566,#11566,#10507,.T.);
#14463=EDGE_CURVE('',#11566,#11565,#5813,.T.);
#14464=EDGE_CURVE('',#11567,#11567,#10508,.T.);
#14465=EDGE_CURVE('',#11472,#11567,#5814,.T.);
#14466=EDGE_CURVE('',#11564,#11563,#5815,.T.);
#14467=EDGE_CURVE('',#11568,#11569,#5816,.T.);
#14468=EDGE_CURVE('',#11570,#11568,#572,.T.);
#14469=EDGE_CURVE('',#11571,#11570,#10509,.T.);
#14470=EDGE_CURVE('',#11571,#11569,#573,.T.);
#14471=EDGE_CURVE('',#11572,#11573,#5817,.T.);
#14472=EDGE_CURVE('',#11574,#11572,#574,.T.);
#14473=EDGE_CURVE('',#11568,#11574,#575,.T.);
#14474=EDGE_CURVE('',#11569,#11575,#576,.T.);
#14475=EDGE_CURVE('',#11575,#11573,#577,.T.);
#14476=EDGE_CURVE('',#11576,#11577,#5818,.T.);
#14477=EDGE_CURVE('',#11578,#11576,#578,.T.);
#14478=EDGE_CURVE('',#11572,#11578,#579,.T.);
#14479=EDGE_CURVE('',#11573,#11577,#580,.T.);
#14480=EDGE_CURVE('',#11579,#11580,#5819,.T.);
#14481=EDGE_CURVE('',#11581,#11579,#581,.F.);
#14482=EDGE_CURVE('',#11576,#11581,#582,.T.);
#14483=EDGE_CURVE('',#11577,#11582,#583,.T.);
#14484=EDGE_CURVE('',#11582,#11580,#584,.T.);
#14485=EDGE_CURVE('',#11583,#11584,#5820,.T.);
#14486=EDGE_CURVE('',#11579,#11583,#585,.F.);
#14487=EDGE_CURVE('',#11580,#11584,#586,.T.);
#14488=EDGE_CURVE('',#11585,#11586,#5821,.T.);
#14489=EDGE_CURVE('',#11587,#11585,#587,.F.);
#14490=EDGE_CURVE('',#11583,#11587,#588,.F.);
#14491=EDGE_CURVE('',#11584,#11588,#589,.T.);
#14492=EDGE_CURVE('',#11588,#11586,#590,.T.);
#14493=EDGE_CURVE('',#11589,#11590,#5822,.T.);
#14494=EDGE_CURVE('',#11585,#11589,#591,.F.);
#14495=EDGE_CURVE('',#11586,#11590,#592,.T.);
#14496=EDGE_CURVE('',#11591,#11592,#5823,.T.);
#14497=EDGE_CURVE('',#11593,#11591,#593,.T.);
#14498=EDGE_CURVE('',#11589,#11593,#594,.F.);
#14499=EDGE_CURVE('',#11590,#11594,#595,.T.);
#14500=EDGE_CURVE('',#11594,#11592,#596,.T.);
#14501=EDGE_CURVE('',#11595,#11596,#5824,.T.);
#14502=EDGE_CURVE('',#11597,#11595,#597,.F.);
#14503=EDGE_CURVE('',#11591,#11597,#598,.T.);
#14504=EDGE_CURVE('',#11592,#11596,#599,.T.);
#14505=EDGE_CURVE('',#11598,#11599,#5825,.T.);
#14506=EDGE_CURVE('',#11595,#11598,#600,.F.);
#14507=EDGE_CURVE('',#11596,#11600,#601,.T.);
#14508=EDGE_CURVE('',#11600,#11599,#602,.T.);
#14509=EDGE_CURVE('',#11601,#11602,#5826,.T.);
#14510=EDGE_CURVE('',#11603,#11601,#603,.T.);
#14511=EDGE_CURVE('',#11598,#11603,#604,.F.);
#14512=EDGE_CURVE('',#11599,#11604,#605,.T.);
#14513=EDGE_CURVE('',#11604,#11602,#606,.T.);
#14514=EDGE_CURVE('',#11605,#11606,#5827,.T.);
#14515=EDGE_CURVE('',#11605,#11607,#607,.T.);
#14516=EDGE_CURVE('',#11608,#11607,#10510,.T.);
#14517=EDGE_CURVE('',#11608,#11606,#608,.T.);
#14518=EDGE_CURVE('',#11609,#11610,#5828,.T.);
#14519=EDGE_CURVE('',#11609,#11605,#609,.T.);
#14520=EDGE_CURVE('',#11606,#11610,#610,.T.);
#14521=EDGE_CURVE('',#11611,#11612,#5829,.T.);
#14522=EDGE_CURVE('',#11611,#11609,#611,.T.);
#14523=EDGE_CURVE('',#11610,#11612,#612,.T.);
#14524=EDGE_CURVE('',#11613,#11614,#5830,.T.);
#14525=EDGE_CURVE('',#11613,#11611,#613,.T.);
#14526=EDGE_CURVE('',#11612,#11614,#614,.T.);
#14527=EDGE_CURVE('',#11615,#11616,#5831,.T.);
#14528=EDGE_CURVE('',#11615,#11613,#615,.T.);
#14529=EDGE_CURVE('',#11614,#11616,#616,.T.);
#14530=EDGE_CURVE('',#11617,#11618,#5832,.T.);
#14531=EDGE_CURVE('',#11617,#11615,#617,.T.);
#14532=EDGE_CURVE('',#11616,#11618,#618,.T.);
#14533=EDGE_CURVE('',#11619,#11620,#5833,.T.);
#14534=EDGE_CURVE('',#11619,#11617,#619,.T.);
#14535=EDGE_CURVE('',#11618,#11620,#620,.T.);
#14536=EDGE_CURVE('',#11621,#11622,#5834,.T.);
#14537=EDGE_CURVE('',#11621,#11619,#621,.T.);
#14538=EDGE_CURVE('',#11620,#11622,#622,.T.);
#14539=EDGE_CURVE('',#11623,#11624,#5835,.T.);
#14540=EDGE_CURVE('',#11623,#11621,#623,.T.);
#14541=EDGE_CURVE('',#11622,#11624,#624,.T.);
#14542=EDGE_CURVE('',#11625,#11626,#5836,.T.);
#14543=EDGE_CURVE('',#11625,#11623,#625,.T.);
#14544=EDGE_CURVE('',#11624,#11626,#626,.T.);
#14545=EDGE_CURVE('',#11627,#11628,#5837,.T.);
#14546=EDGE_CURVE('',#11627,#11625,#627,.T.);
#14547=EDGE_CURVE('',#11626,#11628,#628,.T.);
#14548=EDGE_CURVE('',#11628,#11629,#629,.T.);
#14549=EDGE_CURVE('',#11630,#11629,#10511,.T.);
#14550=EDGE_CURVE('',#11630,#11627,#630,.T.);
#14551=EDGE_CURVE('',#11602,#11631,#631,.T.);
#14552=EDGE_CURVE('',#11631,#11632,#632,.T.);
#14553=EDGE_CURVE('',#11633,#11632,#10512,.T.);
#14554=EDGE_CURVE('',#11634,#11633,#633,.T.);
#14555=EDGE_CURVE('',#11601,#11634,#634,.T.);
#14556=EDGE_CURVE('',#11635,#11636,#10513,.T.);
#14557=EDGE_CURVE('',#11635,#11633,#635,.T.);
#14558=EDGE_CURVE('',#11632,#11630,#636,.T.);
#14559=EDGE_CURVE('',#11636,#11630,#10514,.T.);
#14560=EDGE_CURVE('',#11629,#11635,#637,.T.);
#14561=EDGE_CURVE('',#11570,#11608,#638,.T.);
#14562=EDGE_CURVE('',#11637,#11638,#10515,.T.);
#14563=EDGE_CURVE('',#11637,#11571,#639,.T.);
#14564=EDGE_CURVE('',#11638,#11608,#10516,.T.);
#14565=EDGE_CURVE('',#11607,#11637,#640,.T.);
#14566=EDGE_CURVE('',#11639,#11639,#10517,.T.);
#14567=EDGE_CURVE('',#11639,#11638,#10518,.T.);
#14568=EDGE_CURVE('',#11640,#11640,#10519,.T.);
#14569=EDGE_CURVE('',#11636,#11641,#5838,.T.);
#14570=EDGE_CURVE('',#11641,#11641,#10520,.T.);
#14571=EDGE_CURVE('',#11642,#11643,#197,.T.);
#14572=EDGE_CURVE('',#11642,#11644,#5839,.T.);
#14573=EDGE_CURVE('',#11644,#11645,#5840,.T.);
#14574=EDGE_CURVE('',#11643,#11645,#5841,.T.);
#14575=EDGE_CURVE('',#11645,#11646,#10521,.T.);
#14576=EDGE_CURVE('',#11646,#11644,#5842,.T.);
#14577=EDGE_CURVE('',#11647,#11642,#198,.T.);
#14578=EDGE_CURVE('',#11646,#11647,#5843,.T.);
#14579=EDGE_CURVE('',#11648,#11649,#10522,.T.);
#14580=EDGE_CURVE('',#11649,#11650,#5844,.T.);
#14581=EDGE_CURVE('',#11651,#11650,#10523,.T.);
#14582=EDGE_CURVE('',#11650,#11651,#10524,.T.);
#14583=EDGE_CURVE('',#11649,#11652,#10525,.T.);
#14584=EDGE_CURVE('',#11652,#11653,#5845,.T.);
#14585=EDGE_CURVE('',#11654,#11653,#10526,.T.);
#14586=EDGE_CURVE('',#11654,#11655,#5846,.T.);
#14587=EDGE_CURVE('',#11655,#11656,#10527,.T.);
#14588=EDGE_CURVE('',#11656,#11657,#5847,.T.);
#14589=EDGE_CURVE('',#11658,#11657,#10528,.T.);
#14590=EDGE_CURVE('',#11658,#11659,#5848,.T.);
#14591=EDGE_CURVE('',#11659,#11660,#10529,.T.);
#14592=EDGE_CURVE('',#11660,#11661,#5849,.T.);
#14593=EDGE_CURVE('',#11662,#11661,#10530,.T.);
#14594=EDGE_CURVE('',#11662,#11663,#5850,.T.);
#14595=EDGE_CURVE('',#11663,#11664,#10531,.T.);
#14596=EDGE_CURVE('',#11664,#11665,#5851,.T.);
#14597=EDGE_CURVE('',#11666,#11665,#10532,.T.);
#14598=EDGE_CURVE('',#11666,#11667,#5852,.T.);
#14599=EDGE_CURVE('',#11667,#11668,#10533,.T.);
#14600=EDGE_CURVE('',#11668,#11669,#5853,.T.);
#14601=EDGE_CURVE('',#11670,#11669,#10534,.T.);
#14602=EDGE_CURVE('',#11670,#11671,#5854,.T.);
#14603=EDGE_CURVE('',#11671,#11672,#10535,.T.);
#14604=EDGE_CURVE('',#11672,#11673,#5855,.T.);
#14605=EDGE_CURVE('',#11674,#11673,#10536,.T.);
#14606=EDGE_CURVE('',#11674,#11675,#5856,.T.);
#14607=EDGE_CURVE('',#11675,#11676,#10537,.T.);
#14608=EDGE_CURVE('',#11676,#11677,#5857,.T.);
#14609=EDGE_CURVE('',#11678,#11677,#10538,.T.);
#14610=EDGE_CURVE('',#11678,#11679,#5858,.T.);
#14611=EDGE_CURVE('',#11679,#11680,#10539,.T.);
#14612=EDGE_CURVE('',#11680,#11681,#5859,.T.);
#14613=EDGE_CURVE('',#11682,#11681,#10540,.T.);
#14614=EDGE_CURVE('',#11682,#11683,#5860,.T.);
#14615=EDGE_CURVE('',#11683,#11684,#10541,.T.);
#14616=EDGE_CURVE('',#11684,#11685,#5861,.T.);
#14617=EDGE_CURVE('',#11686,#11685,#10542,.T.);
#14618=EDGE_CURVE('',#11686,#11687,#5862,.T.);
#14619=EDGE_CURVE('',#11687,#11688,#10543,.T.);
#14620=EDGE_CURVE('',#11688,#11689,#5863,.T.);
#14621=EDGE_CURVE('',#11690,#11689,#10544,.T.);
#14622=EDGE_CURVE('',#11690,#11691,#5864,.T.);
#14623=EDGE_CURVE('',#11691,#11692,#10545,.T.);
#14624=EDGE_CURVE('',#11692,#11693,#5865,.T.);
#14625=EDGE_CURVE('',#11694,#11693,#10546,.T.);
#14626=EDGE_CURVE('',#11694,#11695,#5866,.T.);
#14627=EDGE_CURVE('',#11695,#11696,#10547,.T.);
#14628=EDGE_CURVE('',#11696,#11697,#5867,.T.);
#14629=EDGE_CURVE('',#11698,#11697,#10548,.T.);
#14630=EDGE_CURVE('',#11698,#11699,#5868,.T.);
#14631=EDGE_CURVE('',#11699,#11700,#10549,.T.);
#14632=EDGE_CURVE('',#11700,#11701,#5869,.T.);
#14633=EDGE_CURVE('',#11702,#11701,#10550,.T.);
#14634=EDGE_CURVE('',#11702,#11703,#5870,.T.);
#14635=EDGE_CURVE('',#11703,#11704,#10551,.T.);
#14636=EDGE_CURVE('',#11704,#11705,#5871,.T.);
#14637=EDGE_CURVE('',#11706,#11705,#10552,.T.);
#14638=EDGE_CURVE('',#11706,#11707,#5872,.T.);
#14639=EDGE_CURVE('',#11707,#11708,#10553,.T.);
#14640=EDGE_CURVE('',#11708,#11709,#5873,.T.);
#14641=EDGE_CURVE('',#11710,#11709,#10554,.T.);
#14642=EDGE_CURVE('',#11710,#11711,#5874,.T.);
#14643=EDGE_CURVE('',#11711,#11712,#10555,.T.);
#14644=EDGE_CURVE('',#11712,#11713,#5875,.T.);
#14645=EDGE_CURVE('',#11714,#11713,#10556,.T.);
#14646=EDGE_CURVE('',#11714,#11715,#5876,.T.);
#14647=EDGE_CURVE('',#11715,#11716,#10557,.T.);
#14648=EDGE_CURVE('',#11716,#11717,#5877,.T.);
#14649=EDGE_CURVE('',#11643,#11717,#10558,.T.);
#14650=EDGE_CURVE('',#11718,#11647,#10559,.T.);
#14651=EDGE_CURVE('',#11718,#11719,#5878,.T.);
#14652=EDGE_CURVE('',#11719,#11720,#10560,.T.);
#14653=EDGE_CURVE('',#11720,#11721,#5879,.T.);
#14654=EDGE_CURVE('',#11722,#11721,#10561,.T.);
#14655=EDGE_CURVE('',#11722,#11723,#5880,.T.);
#14656=EDGE_CURVE('',#11723,#11724,#10562,.T.);
#14657=EDGE_CURVE('',#11724,#11725,#5881,.T.);
#14658=EDGE_CURVE('',#11726,#11725,#10563,.T.);
#14659=EDGE_CURVE('',#11726,#11727,#5882,.T.);
#14660=EDGE_CURVE('',#11727,#11728,#10564,.T.);
#14661=EDGE_CURVE('',#11728,#11729,#5883,.T.);
#14662=EDGE_CURVE('',#11730,#11729,#10565,.T.);
#14663=EDGE_CURVE('',#11730,#11731,#5884,.T.);
#14664=EDGE_CURVE('',#11731,#11732,#10566,.T.);
#14665=EDGE_CURVE('',#11732,#11733,#5885,.T.);
#14666=EDGE_CURVE('',#11734,#11733,#10567,.T.);
#14667=EDGE_CURVE('',#11734,#11735,#5886,.T.);
#14668=EDGE_CURVE('',#11735,#11736,#10568,.T.);
#14669=EDGE_CURVE('',#11736,#11737,#5887,.T.);
#14670=EDGE_CURVE('',#11738,#11737,#10569,.T.);
#14671=EDGE_CURVE('',#11738,#11739,#5888,.T.);
#14672=EDGE_CURVE('',#11739,#11740,#10570,.T.);
#14673=EDGE_CURVE('',#11740,#11741,#5889,.T.);
#14674=EDGE_CURVE('',#11742,#11741,#10571,.T.);
#14675=EDGE_CURVE('',#11742,#11743,#5890,.T.);
#14676=EDGE_CURVE('',#11743,#11744,#10572,.T.);
#14677=EDGE_CURVE('',#11744,#11745,#5891,.T.);
#14678=EDGE_CURVE('',#11746,#11745,#10573,.T.);
#14679=EDGE_CURVE('',#11746,#11747,#5892,.T.);
#14680=EDGE_CURVE('',#11747,#11748,#10574,.T.);
#14681=EDGE_CURVE('',#11748,#11749,#5893,.T.);
#14682=EDGE_CURVE('',#11750,#11749,#10575,.T.);
#14683=EDGE_CURVE('',#11750,#11751,#5894,.T.);
#14684=EDGE_CURVE('',#11751,#11752,#10576,.T.);
#14685=EDGE_CURVE('',#11752,#11753,#5895,.T.);
#14686=EDGE_CURVE('',#11754,#11753,#10577,.T.);
#14687=EDGE_CURVE('',#11754,#11755,#5896,.T.);
#14688=EDGE_CURVE('',#11755,#11756,#10578,.T.);
#14689=EDGE_CURVE('',#11756,#11757,#5897,.T.);
#14690=EDGE_CURVE('',#11758,#11757,#10579,.T.);
#14691=EDGE_CURVE('',#11758,#11759,#5898,.T.);
#14692=EDGE_CURVE('',#11759,#11760,#10580,.T.);
#14693=EDGE_CURVE('',#11760,#11761,#5899,.T.);
#14694=EDGE_CURVE('',#11762,#11761,#10581,.T.);
#14695=EDGE_CURVE('',#11762,#11763,#5900,.T.);
#14696=EDGE_CURVE('',#11763,#11764,#10582,.T.);
#14697=EDGE_CURVE('',#11764,#11765,#5901,.T.);
#14698=EDGE_CURVE('',#11766,#11765,#10583,.T.);
#14699=EDGE_CURVE('',#11766,#11767,#5902,.T.);
#14700=EDGE_CURVE('',#11767,#11768,#10584,.T.);
#14701=EDGE_CURVE('',#11768,#11769,#5903,.T.);
#14702=EDGE_CURVE('',#11770,#11769,#10585,.T.);
#14703=EDGE_CURVE('',#11770,#11771,#5904,.T.);
#14704=EDGE_CURVE('',#11771,#11772,#10586,.T.);
#14705=EDGE_CURVE('',#11772,#11773,#5905,.T.);
#14706=EDGE_CURVE('',#11774,#11773,#10587,.T.);
#14707=EDGE_CURVE('',#11774,#11775,#5906,.T.);
#14708=EDGE_CURVE('',#11775,#11776,#10588,.T.);
#14709=EDGE_CURVE('',#11776,#11777,#5907,.T.);
#14710=EDGE_CURVE('',#11778,#11777,#10589,.T.);
#14711=EDGE_CURVE('',#11778,#11779,#5908,.T.);
#14712=EDGE_CURVE('',#11779,#11780,#10590,.T.);
#14713=EDGE_CURVE('',#11780,#11781,#5909,.T.);
#14714=EDGE_CURVE('',#11782,#11781,#10591,.T.);
#14715=EDGE_CURVE('',#11782,#11783,#5910,.T.);
#14716=EDGE_CURVE('',#11783,#11784,#10592,.T.);
#14717=EDGE_CURVE('',#11784,#11785,#5911,.T.);
#14718=EDGE_CURVE('',#11786,#11785,#10593,.T.);
#14719=EDGE_CURVE('',#11786,#11787,#5912,.T.);
#14720=EDGE_CURVE('',#11787,#11788,#10594,.T.);
#14721=EDGE_CURVE('',#11788,#11789,#5913,.T.);
#14722=EDGE_CURVE('',#11790,#11789,#10595,.T.);
#14723=EDGE_CURVE('',#11790,#11648,#5914,.T.);
#14724=EDGE_CURVE('',#11791,#11714,#199,.T.);
#14725=EDGE_CURVE('',#11791,#11792,#5915,.T.);
#14726=EDGE_CURVE('',#11792,#11715,#5916,.T.);
#14727=EDGE_CURVE('',#11716,#11792,#5917,.T.);
#14728=EDGE_CURVE('',#11717,#11791,#200,.T.);
#14729=EDGE_CURVE('',#11793,#11710,#201,.T.);
#14730=EDGE_CURVE('',#11793,#11794,#5918,.T.);
#14731=EDGE_CURVE('',#11794,#11711,#5919,.T.);
#14732=EDGE_CURVE('',#11712,#11794,#5920,.T.);
#14733=EDGE_CURVE('',#11713,#11793,#202,.T.);
#14734=EDGE_CURVE('',#11795,#11706,#203,.T.);
#14735=EDGE_CURVE('',#11795,#11796,#5921,.T.);
#14736=EDGE_CURVE('',#11796,#11707,#5922,.T.);
#14737=EDGE_CURVE('',#11708,#11796,#5923,.T.);
#14738=EDGE_CURVE('',#11709,#11795,#204,.T.);
#14739=EDGE_CURVE('',#11797,#11702,#205,.T.);
#14740=EDGE_CURVE('',#11797,#11798,#5924,.T.);
#14741=EDGE_CURVE('',#11798,#11703,#5925,.T.);
#14742=EDGE_CURVE('',#11704,#11798,#5926,.T.);
#14743=EDGE_CURVE('',#11705,#11797,#206,.T.);
#14744=EDGE_CURVE('',#11799,#11698,#207,.T.);
#14745=EDGE_CURVE('',#11799,#11800,#5927,.T.);
#14746=EDGE_CURVE('',#11800,#11699,#5928,.T.);
#14747=EDGE_CURVE('',#11700,#11800,#5929,.T.);
#14748=EDGE_CURVE('',#11701,#11799,#208,.T.);
#14749=EDGE_CURVE('',#11801,#11694,#209,.T.);
#14750=EDGE_CURVE('',#11801,#11802,#5930,.T.);
#14751=EDGE_CURVE('',#11802,#11695,#5931,.T.);
#14752=EDGE_CURVE('',#11696,#11802,#5932,.T.);
#14753=EDGE_CURVE('',#11697,#11801,#210,.T.);
#14754=EDGE_CURVE('',#11803,#11690,#211,.T.);
#14755=EDGE_CURVE('',#11803,#11804,#5933,.T.);
#14756=EDGE_CURVE('',#11804,#11691,#5934,.T.);
#14757=EDGE_CURVE('',#11692,#11804,#5935,.T.);
#14758=EDGE_CURVE('',#11693,#11803,#212,.T.);
#14759=EDGE_CURVE('',#11805,#11686,#213,.T.);
#14760=EDGE_CURVE('',#11805,#11806,#5936,.T.);
#14761=EDGE_CURVE('',#11806,#11687,#5937,.T.);
#14762=EDGE_CURVE('',#11688,#11806,#5938,.T.);
#14763=EDGE_CURVE('',#11689,#11805,#214,.T.);
#14764=EDGE_CURVE('',#11807,#11682,#215,.T.);
#14765=EDGE_CURVE('',#11807,#11808,#5939,.T.);
#14766=EDGE_CURVE('',#11808,#11683,#5940,.T.);
#14767=EDGE_CURVE('',#11684,#11808,#5941,.T.);
#14768=EDGE_CURVE('',#11685,#11807,#216,.T.);
#14769=EDGE_CURVE('',#11809,#11678,#217,.T.);
#14770=EDGE_CURVE('',#11809,#11810,#5942,.T.);
#14771=EDGE_CURVE('',#11810,#11679,#5943,.T.);
#14772=EDGE_CURVE('',#11680,#11810,#5944,.T.);
#14773=EDGE_CURVE('',#11681,#11809,#218,.T.);
#14774=EDGE_CURVE('',#11811,#11674,#219,.T.);
#14775=EDGE_CURVE('',#11811,#11812,#5945,.T.);
#14776=EDGE_CURVE('',#11812,#11675,#5946,.T.);
#14777=EDGE_CURVE('',#11676,#11812,#5947,.T.);
#14778=EDGE_CURVE('',#11677,#11811,#220,.T.);
#14779=EDGE_CURVE('',#11813,#11670,#221,.T.);
#14780=EDGE_CURVE('',#11813,#11814,#5948,.T.);
#14781=EDGE_CURVE('',#11814,#11671,#5949,.T.);
#14782=EDGE_CURVE('',#11672,#11814,#5950,.T.);
#14783=EDGE_CURVE('',#11673,#11813,#222,.T.);
#14784=EDGE_CURVE('',#11815,#11666,#223,.T.);
#14785=EDGE_CURVE('',#11815,#11816,#5951,.T.);
#14786=EDGE_CURVE('',#11816,#11667,#5952,.T.);
#14787=EDGE_CURVE('',#11668,#11816,#5953,.T.);
#14788=EDGE_CURVE('',#11669,#11815,#224,.T.);
#14789=EDGE_CURVE('',#11817,#11662,#225,.T.);
#14790=EDGE_CURVE('',#11817,#11818,#5954,.T.);
#14791=EDGE_CURVE('',#11818,#11663,#5955,.T.);
#14792=EDGE_CURVE('',#11664,#11818,#5956,.T.);
#14793=EDGE_CURVE('',#11665,#11817,#226,.T.);
#14794=EDGE_CURVE('',#11819,#11658,#227,.T.);
#14795=EDGE_CURVE('',#11819,#11820,#5957,.T.);
#14796=EDGE_CURVE('',#11820,#11659,#5958,.T.);
#14797=EDGE_CURVE('',#11660,#11820,#5959,.T.);
#14798=EDGE_CURVE('',#11661,#11819,#228,.T.);
#14799=EDGE_CURVE('',#11821,#11654,#229,.T.);
#14800=EDGE_CURVE('',#11821,#11822,#5960,.T.);
#14801=EDGE_CURVE('',#11822,#11655,#5961,.T.);
#14802=EDGE_CURVE('',#11656,#11822,#5962,.T.);
#14803=EDGE_CURVE('',#11657,#11821,#230,.T.);
#14804=EDGE_CURVE('',#11823,#11790,#231,.T.);
#14805=EDGE_CURVE('',#11823,#11824,#5963,.T.);
#14806=EDGE_CURVE('',#11824,#11648,#5964,.T.);
#14807=EDGE_CURVE('',#11652,#11824,#5965,.T.);
#14808=EDGE_CURVE('',#11653,#11823,#232,.T.);
#14809=EDGE_CURVE('',#11825,#11786,#233,.T.);
#14810=EDGE_CURVE('',#11825,#11826,#5966,.T.);
#14811=EDGE_CURVE('',#11826,#11787,#5967,.T.);
#14812=EDGE_CURVE('',#11788,#11826,#5968,.T.);
#14813=EDGE_CURVE('',#11789,#11825,#234,.T.);
#14814=EDGE_CURVE('',#11827,#11782,#235,.T.);
#14815=EDGE_CURVE('',#11827,#11828,#5969,.T.);
#14816=EDGE_CURVE('',#11828,#11783,#5970,.T.);
#14817=EDGE_CURVE('',#11784,#11828,#5971,.T.);
#14818=EDGE_CURVE('',#11785,#11827,#236,.T.);
#14819=EDGE_CURVE('',#11829,#11778,#237,.T.);
#14820=EDGE_CURVE('',#11829,#11830,#5972,.T.);
#14821=EDGE_CURVE('',#11830,#11779,#5973,.T.);
#14822=EDGE_CURVE('',#11780,#11830,#5974,.T.);
#14823=EDGE_CURVE('',#11781,#11829,#238,.T.);
#14824=EDGE_CURVE('',#11831,#11774,#239,.T.);
#14825=EDGE_CURVE('',#11831,#11832,#5975,.T.);
#14826=EDGE_CURVE('',#11832,#11775,#5976,.T.);
#14827=EDGE_CURVE('',#11776,#11832,#5977,.T.);
#14828=EDGE_CURVE('',#11777,#11831,#240,.T.);
#14829=EDGE_CURVE('',#11833,#11770,#241,.T.);
#14830=EDGE_CURVE('',#11833,#11834,#5978,.T.);
#14831=EDGE_CURVE('',#11834,#11771,#5979,.T.);
#14832=EDGE_CURVE('',#11772,#11834,#5980,.T.);
#14833=EDGE_CURVE('',#11773,#11833,#242,.T.);
#14834=EDGE_CURVE('',#11835,#11766,#243,.T.);
#14835=EDGE_CURVE('',#11835,#11836,#5981,.T.);
#14836=EDGE_CURVE('',#11836,#11767,#5982,.T.);
#14837=EDGE_CURVE('',#11768,#11836,#5983,.T.);
#14838=EDGE_CURVE('',#11769,#11835,#244,.T.);
#14839=EDGE_CURVE('',#11837,#11762,#245,.T.);
#14840=EDGE_CURVE('',#11837,#11838,#5984,.T.);
#14841=EDGE_CURVE('',#11838,#11763,#5985,.T.);
#14842=EDGE_CURVE('',#11764,#11838,#5986,.T.);
#14843=EDGE_CURVE('',#11765,#11837,#246,.T.);
#14844=EDGE_CURVE('',#11839,#11758,#247,.T.);
#14845=EDGE_CURVE('',#11839,#11840,#5987,.T.);
#14846=EDGE_CURVE('',#11840,#11759,#5988,.T.);
#14847=EDGE_CURVE('',#11760,#11840,#5989,.T.);
#14848=EDGE_CURVE('',#11761,#11839,#248,.T.);
#14849=EDGE_CURVE('',#11841,#11754,#249,.T.);
#14850=EDGE_CURVE('',#11841,#11842,#5990,.T.);
#14851=EDGE_CURVE('',#11842,#11755,#5991,.T.);
#14852=EDGE_CURVE('',#11756,#11842,#5992,.T.);
#14853=EDGE_CURVE('',#11757,#11841,#250,.T.);
#14854=EDGE_CURVE('',#11843,#11750,#251,.T.);
#14855=EDGE_CURVE('',#11843,#11844,#5993,.T.);
#14856=EDGE_CURVE('',#11844,#11751,#5994,.T.);
#14857=EDGE_CURVE('',#11752,#11844,#5995,.T.);
#14858=EDGE_CURVE('',#11753,#11843,#252,.T.);
#14859=EDGE_CURVE('',#11845,#11746,#253,.T.);
#14860=EDGE_CURVE('',#11845,#11846,#5996,.T.);
#14861=EDGE_CURVE('',#11846,#11747,#5997,.T.);
#14862=EDGE_CURVE('',#11748,#11846,#5998,.T.);
#14863=EDGE_CURVE('',#11749,#11845,#254,.T.);
#14864=EDGE_CURVE('',#11847,#11742,#255,.T.);
#14865=EDGE_CURVE('',#11847,#11848,#5999,.T.);
#14866=EDGE_CURVE('',#11848,#11743,#6000,.T.);
#14867=EDGE_CURVE('',#11744,#11848,#6001,.T.);
#14868=EDGE_CURVE('',#11745,#11847,#256,.T.);
#14869=EDGE_CURVE('',#11849,#11738,#257,.T.);
#14870=EDGE_CURVE('',#11849,#11850,#6002,.T.);
#14871=EDGE_CURVE('',#11850,#11739,#6003,.T.);
#14872=EDGE_CURVE('',#11740,#11850,#6004,.T.);
#14873=EDGE_CURVE('',#11741,#11849,#258,.T.);
#14874=EDGE_CURVE('',#11851,#11734,#259,.T.);
#14875=EDGE_CURVE('',#11851,#11852,#6005,.T.);
#14876=EDGE_CURVE('',#11852,#11735,#6006,.T.);
#14877=EDGE_CURVE('',#11736,#11852,#6007,.T.);
#14878=EDGE_CURVE('',#11737,#11851,#260,.T.);
#14879=EDGE_CURVE('',#11853,#11730,#261,.T.);
#14880=EDGE_CURVE('',#11853,#11854,#6008,.T.);
#14881=EDGE_CURVE('',#11854,#11731,#6009,.T.);
#14882=EDGE_CURVE('',#11732,#11854,#6010,.T.);
#14883=EDGE_CURVE('',#11733,#11853,#262,.T.);
#14884=EDGE_CURVE('',#11855,#11726,#263,.T.);
#14885=EDGE_CURVE('',#11855,#11856,#6011,.T.);
#14886=EDGE_CURVE('',#11856,#11727,#6012,.T.);
#14887=EDGE_CURVE('',#11728,#11856,#6013,.T.);
#14888=EDGE_CURVE('',#11729,#11855,#264,.T.);
#14889=EDGE_CURVE('',#11857,#11722,#265,.T.);
#14890=EDGE_CURVE('',#11857,#11858,#6014,.T.);
#14891=EDGE_CURVE('',#11858,#11723,#6015,.T.);
#14892=EDGE_CURVE('',#11724,#11858,#6016,.T.);
#14893=EDGE_CURVE('',#11725,#11857,#266,.T.);
#14894=EDGE_CURVE('',#11859,#11718,#267,.T.);
#14895=EDGE_CURVE('',#11859,#11860,#6017,.T.);
#14896=EDGE_CURVE('',#11860,#11719,#6018,.T.);
#14897=EDGE_CURVE('',#11720,#11860,#6019,.T.);
#14898=EDGE_CURVE('',#11721,#11859,#268,.T.);
#14899=EDGE_CURVE('',#11651,#11640,#10596,.T.);
#14900=EDGE_CURVE('',#11823,#11861,#6020,.T.);
#14901=EDGE_CURVE('',#11861,#11861,#10597,.T.);
#14902=EDGE_CURVE('',#11862,#11862,#10598,.T.);
#14903=EDGE_CURVE('',#11863,#11864,#269,.T.);
#14904=EDGE_CURVE('',#11863,#11865,#10599,.T.);
#14905=EDGE_CURVE('',#11866,#11865,#270,.T.);
#14906=EDGE_CURVE('',#11867,#11866,#271,.T.);
#14907=EDGE_CURVE('',#11867,#11868,#10600,.T.);
#14908=EDGE_CURVE('',#11869,#11868,#272,.T.);
#14909=EDGE_CURVE('',#11870,#11869,#273,.T.);
#14910=EDGE_CURVE('',#11870,#11871,#10601,.T.);
#14911=EDGE_CURVE('',#11872,#11871,#274,.T.);
#14912=EDGE_CURVE('',#11873,#11872,#275,.T.);
#14913=EDGE_CURVE('',#11873,#11874,#10602,.T.);
#14914=EDGE_CURVE('',#11875,#11874,#276,.T.);
#14915=EDGE_CURVE('',#11876,#11875,#277,.T.);
#14916=EDGE_CURVE('',#11876,#11877,#10603,.T.);
#14917=EDGE_CURVE('',#11878,#11877,#278,.T.);
#14918=EDGE_CURVE('',#11879,#11878,#279,.T.);
#14919=EDGE_CURVE('',#11879,#11880,#10604,.T.);
#14920=EDGE_CURVE('',#11864,#11880,#280,.T.);
#14921=EDGE_CURVE('',#11864,#11862,#6021,.T.);
#14922=EDGE_CURVE('',#11868,#11881,#6022,.T.);
#14923=EDGE_CURVE('',#11882,#11867,#6023,.T.);
#14924=EDGE_CURVE('',#11881,#11882,#10605,.T.);
#14925=EDGE_CURVE('',#11871,#11883,#6024,.T.);
#14926=EDGE_CURVE('',#11884,#11870,#6025,.T.);
#14927=EDGE_CURVE('',#11883,#11884,#10606,.T.);
#14928=EDGE_CURVE('',#11885,#11863,#6026,.T.);
#14929=EDGE_CURVE('',#11886,#11885,#10607,.T.);
#14930=EDGE_CURVE('',#11865,#11886,#6027,.T.);
#14931=EDGE_CURVE('',#11874,#11887,#6028,.T.);
#14932=EDGE_CURVE('',#11888,#11873,#6029,.T.);
#14933=EDGE_CURVE('',#11887,#11888,#10608,.T.);
#14934=EDGE_CURVE('',#11889,#11879,#6030,.T.);
#14935=EDGE_CURVE('',#11890,#11889,#10609,.T.);
#14936=EDGE_CURVE('',#11880,#11890,#6031,.T.);
#14937=EDGE_CURVE('',#11891,#11876,#6032,.T.);
#14938=EDGE_CURVE('',#11892,#11891,#10610,.T.);
#14939=EDGE_CURVE('',#11877,#11892,#6033,.T.);
#14940=EDGE_CURVE('',#11888,#11887,#6034,.T.);
#14941=EDGE_CURVE('',#11872,#11893,#6035,.T.);
#14942=EDGE_CURVE('',#11893,#11894,#6036,.T.);
#14943=EDGE_CURVE('',#11875,#11894,#6037,.T.);
#14944=EDGE_CURVE('',#11884,#11883,#6038,.T.);
#14945=EDGE_CURVE('',#11869,#11895,#6039,.T.);
#14946=EDGE_CURVE('',#11895,#11893,#6040,.T.);
#14947=EDGE_CURVE('',#11882,#11881,#6041,.T.);
#14948=EDGE_CURVE('',#11866,#11896,#6042,.T.);
#14949=EDGE_CURVE('',#11896,#11895,#6043,.T.);
#14950=EDGE_CURVE('',#11885,#11886,#6044,.T.);
#14951=EDGE_CURVE('',#11889,#11890,#6045,.T.);
#14952=EDGE_CURVE('',#11891,#11892,#6046,.T.);
#14953=EDGE_CURVE('',#11897,#11896,#6047,.T.);
#14954=EDGE_CURVE('',#11897,#11896,#10611,.T.);
#14955=EDGE_CURVE('',#11896,#11895,#10612,.T.);
#14956=EDGE_CURVE('',#11895,#11893,#10613,.T.);
#14957=EDGE_CURVE('',#11893,#11894,#10614,.T.);
#14958=EDGE_CURVE('',#11894,#11898,#6048,.T.);
#14959=EDGE_CURVE('',#11894,#11898,#10615,.T.);
#14960=EDGE_CURVE('',#11898,#11897,#6049,.T.);
#14961=EDGE_CURVE('',#11898,#11897,#10616,.T.);
#14962=EDGE_CURVE('',#11899,#11897,#6050,.T.);
#14963=EDGE_CURVE('',#11864,#11897,#6051,.T.);
#14964=EDGE_CURVE('',#11878,#11898,#6052,.T.);
#14965=EDGE_CURVE('',#11900,#11900,#10617,.T.);
#14966=EDGE_CURVE('',#11900,#11901,#6053,.T.);
#14967=EDGE_CURVE('',#11901,#11901,#10618,.T.);
#14968=EDGE_CURVE('',#11902,#11903,#6054,.T.);
#14969=EDGE_CURVE('',#11904,#11902,#10619,.T.);
#14970=EDGE_CURVE('',#11905,#11904,#6055,.T.);
#14971=EDGE_CURVE('',#11903,#11905,#10620,.T.);
#14972=EDGE_CURVE('',#11906,#11906,#10621,.T.);
#14973=EDGE_CURVE('',#11907,#11907,#10622,.T.);
#14974=EDGE_CURVE('',#11908,#11908,#10623,.T.);
#14975=EDGE_CURVE('',#11909,#11909,#10624,.T.);
#14976=EDGE_CURVE('',#11910,#11910,#10625,.T.);
#14977=EDGE_CURVE('',#11911,#11911,#10626,.T.);
#14978=EDGE_CURVE('',#11912,#11912,#10627,.T.);
#14979=EDGE_CURVE('',#11913,#11913,#10628,.T.);
#14980=EDGE_CURVE('',#11914,#11914,#10629,.T.);
#14981=EDGE_CURVE('',#11915,#11915,#10630,.T.);
#14982=EDGE_CURVE('',#11916,#11916,#10631,.T.);
#14983=EDGE_CURVE('',#11917,#11917,#10632,.T.);
#14984=EDGE_CURVE('',#11918,#11918,#10633,.T.);
#14985=EDGE_CURVE('',#11919,#11919,#10634,.T.);
#14986=EDGE_CURVE('',#11920,#11920,#10635,.T.);
#14987=EDGE_CURVE('',#11921,#11921,#10636,.T.);
#14988=EDGE_CURVE('',#11922,#11922,#10637,.T.);
#14989=EDGE_CURVE('',#11923,#11923,#10638,.T.);
#14990=EDGE_CURVE('',#11924,#11924,#10639,.T.);
#14991=EDGE_CURVE('',#11925,#11925,#10640,.T.);
#14992=EDGE_CURVE('',#11900,#11926,#6056,.T.);
#14993=EDGE_CURVE('',#11926,#11926,#10641,.T.);
#14994=EDGE_CURVE('',#11927,#11927,#10642,.T.);
#14995=EDGE_CURVE('',#11927,#11906,#6057,.T.);
#14996=EDGE_CURVE('',#11927,#11928,#6058,.T.);
#14997=EDGE_CURVE('',#11928,#11928,#10643,.T.);
#14998=EDGE_CURVE('',#11929,#11929,#10644,.T.);
#14999=EDGE_CURVE('',#11929,#11925,#6059,.T.);
#15000=EDGE_CURVE('',#11929,#11930,#6060,.T.);
#15001=EDGE_CURVE('',#11930,#11930,#10645,.T.);
#15002=EDGE_CURVE('',#11931,#11931,#10646,.T.);
#15003=EDGE_CURVE('',#11931,#11907,#6061,.T.);
#15004=EDGE_CURVE('',#11931,#11932,#6062,.T.);
#15005=EDGE_CURVE('',#11932,#11932,#10647,.T.);
#15006=EDGE_CURVE('',#11933,#11933,#10648,.T.);
#15007=EDGE_CURVE('',#11933,#11924,#6063,.T.);
#15008=EDGE_CURVE('',#11933,#11934,#6064,.T.);
#15009=EDGE_CURVE('',#11934,#11934,#10649,.T.);
#15010=EDGE_CURVE('',#11935,#11935,#10650,.T.);
#15011=EDGE_CURVE('',#11935,#11908,#6065,.T.);
#15012=EDGE_CURVE('',#11935,#11936,#6066,.T.);
#15013=EDGE_CURVE('',#11936,#11936,#10651,.T.);
#15014=EDGE_CURVE('',#11937,#11937,#10652,.T.);
#15015=EDGE_CURVE('',#11937,#11923,#6067,.T.);
#15016=EDGE_CURVE('',#11937,#11938,#6068,.T.);
#15017=EDGE_CURVE('',#11938,#11938,#10653,.T.);
#15018=EDGE_CURVE('',#11939,#11939,#10654,.T.);
#15019=EDGE_CURVE('',#11939,#11909,#6069,.T.);
#15020=EDGE_CURVE('',#11939,#11940,#6070,.T.);
#15021=EDGE_CURVE('',#11940,#11940,#10655,.T.);
#15022=EDGE_CURVE('',#11941,#11941,#10656,.T.);
#15023=EDGE_CURVE('',#11941,#11922,#6071,.T.);
#15024=EDGE_CURVE('',#11941,#11942,#6072,.T.);
#15025=EDGE_CURVE('',#11942,#11942,#10657,.T.);
#15026=EDGE_CURVE('',#11943,#11943,#10658,.T.);
#15027=EDGE_CURVE('',#11943,#11910,#6073,.T.);
#15028=EDGE_CURVE('',#11943,#11944,#6074,.T.);
#15029=EDGE_CURVE('',#11944,#11944,#10659,.T.);
#15030=EDGE_CURVE('',#11945,#11945,#10660,.T.);
#15031=EDGE_CURVE('',#11945,#11921,#6075,.T.);
#15032=EDGE_CURVE('',#11945,#11946,#6076,.T.);
#15033=EDGE_CURVE('',#11946,#11946,#10661,.T.);
#15034=EDGE_CURVE('',#11947,#11947,#10662,.T.);
#15035=EDGE_CURVE('',#11947,#11911,#6077,.T.);
#15036=EDGE_CURVE('',#11947,#11948,#6078,.T.);
#15037=EDGE_CURVE('',#11948,#11948,#10663,.T.);
#15038=EDGE_CURVE('',#11949,#11949,#10664,.T.);
#15039=EDGE_CURVE('',#11949,#11920,#6079,.T.);
#15040=EDGE_CURVE('',#11949,#11950,#6080,.T.);
#15041=EDGE_CURVE('',#11950,#11950,#10665,.T.);
#15042=EDGE_CURVE('',#11951,#11951,#10666,.T.);
#15043=EDGE_CURVE('',#11951,#11912,#6081,.T.);
#15044=EDGE_CURVE('',#11951,#11952,#6082,.T.);
#15045=EDGE_CURVE('',#11952,#11952,#10667,.T.);
#15046=EDGE_CURVE('',#11953,#11953,#10668,.T.);
#15047=EDGE_CURVE('',#11953,#11919,#6083,.T.);
#15048=EDGE_CURVE('',#11953,#11954,#6084,.T.);
#15049=EDGE_CURVE('',#11954,#11954,#10669,.T.);
#15050=EDGE_CURVE('',#11955,#11955,#10670,.T.);
#15051=EDGE_CURVE('',#11955,#11913,#6085,.T.);
#15052=EDGE_CURVE('',#11955,#11956,#6086,.T.);
#15053=EDGE_CURVE('',#11956,#11956,#10671,.T.);
#15054=EDGE_CURVE('',#11957,#11957,#10672,.T.);
#15055=EDGE_CURVE('',#11957,#11918,#6087,.T.);
#15056=EDGE_CURVE('',#11957,#11958,#6088,.T.);
#15057=EDGE_CURVE('',#11958,#11958,#10673,.T.);
#15058=EDGE_CURVE('',#11959,#11959,#10674,.T.);
#15059=EDGE_CURVE('',#11959,#11914,#6089,.T.);
#15060=EDGE_CURVE('',#11959,#11960,#6090,.T.);
#15061=EDGE_CURVE('',#11960,#11960,#10675,.T.);
#15062=EDGE_CURVE('',#11961,#11961,#10676,.T.);
#15063=EDGE_CURVE('',#11961,#11917,#6091,.T.);
#15064=EDGE_CURVE('',#11961,#11962,#6092,.T.);
#15065=EDGE_CURVE('',#11962,#11962,#10677,.T.);
#15066=EDGE_CURVE('',#11963,#11963,#10678,.T.);
#15067=EDGE_CURVE('',#11963,#11915,#6093,.T.);
#15068=EDGE_CURVE('',#11963,#11964,#6094,.T.);
#15069=EDGE_CURVE('',#11964,#11964,#10679,.T.);
#15070=EDGE_CURVE('',#11965,#11965,#10680,.T.);
#15071=EDGE_CURVE('',#11965,#11916,#6095,.T.);
#15072=EDGE_CURVE('',#11965,#11966,#6096,.T.);
#15073=EDGE_CURVE('',#11966,#11966,#10681,.T.);
#15074=EDGE_CURVE('',#11967,#11902,#6097,.T.);
#15075=EDGE_CURVE('',#11903,#11968,#6098,.T.);
#15076=EDGE_CURVE('',#11968,#11967,#6099,.T.);
#15077=EDGE_CURVE('',#11969,#11904,#6100,.T.);
#15078=EDGE_CURVE('',#11967,#11969,#10682,.T.);
#15079=EDGE_CURVE('',#11970,#11905,#6101,.T.);
#15080=EDGE_CURVE('',#11969,#11970,#6102,.T.);
#15081=EDGE_CURVE('',#11970,#11968,#10683,.T.);
#15082=EDGE_CURVE('',#11971,#11967,#6103,.T.);
#15083=EDGE_CURVE('',#11972,#11971,#10684,.T.);
#15084=EDGE_CURVE('',#11972,#11969,#6104,.T.);
#15085=EDGE_CURVE('',#11973,#11968,#6105,.T.);
#15086=EDGE_CURVE('',#11971,#11973,#6106,.T.);
#15087=EDGE_CURVE('',#11973,#11974,#6107,.T.);
#15088=EDGE_CURVE('',#11974,#11975,#6108,.T.);
#15089=EDGE_CURVE('',#11975,#11971,#6109,.T.);
#15090=EDGE_CURVE('',#11973,#11976,#10685,.T.);
#15091=EDGE_CURVE('',#11976,#11977,#6110,.T.);
#15092=EDGE_CURVE('',#11977,#11974,#10686,.T.);
#15093=EDGE_CURVE('',#11972,#11978,#6111,.T.);
#15094=EDGE_CURVE('',#11978,#11977,#6112,.T.);
#15095=EDGE_CURVE('',#11976,#11972,#6113,.T.);
#15096=EDGE_CURVE('',#11975,#11978,#10687,.T.);
#15097=EDGE_CURVE('',#11976,#11970,#6114,.T.);
#15098=EDGE_CURVE('',#11979,#11980,#6115,.F.);
#15099=EDGE_CURVE('',#11980,#11981,#6116,.T.);
#15100=EDGE_CURVE('',#11981,#11982,#6117,.T.);
#15101=EDGE_CURVE('',#11982,#11979,#6118,.T.);
#15102=EDGE_CURVE('',#11983,#11984,#6119,.T.);
#15103=EDGE_CURVE('',#11984,#11982,#10688,.T.);
#15104=EDGE_CURVE('',#11981,#11983,#10689,.T.);
#15105=EDGE_CURVE('',#11985,#11986,#6120,.T.);
#15106=EDGE_CURVE('',#11986,#11984,#6121,.T.);
#15107=EDGE_CURVE('',#11983,#11985,#6122,.T.);
#15108=EDGE_CURVE('',#11987,#11988,#6123,.T.);
#15109=EDGE_CURVE('',#11988,#11986,#10690,.T.);
#15110=EDGE_CURVE('',#11985,#11987,#10691,.T.);
#15111=EDGE_CURVE('',#11989,#11990,#6124,.F.);
#15112=EDGE_CURVE('',#11990,#11988,#6125,.T.);
#15113=EDGE_CURVE('',#11987,#11989,#6126,.T.);
#15114=EDGE_CURVE('',#11991,#11987,#6127,.T.);
#15115=EDGE_CURVE('',#11992,#11991,#6128,.T.);
#15116=EDGE_CURVE('',#11992,#11989,#6129,.T.);
#15117=EDGE_CURVE('',#11993,#11985,#6130,.T.);
#15118=EDGE_CURVE('',#11991,#11993,#10692,.T.);
#15119=EDGE_CURVE('',#11994,#11983,#6131,.T.);
#15120=EDGE_CURVE('',#11993,#11994,#6132,.T.);
#15121=EDGE_CURVE('',#11995,#11981,#6133,.T.);
#15122=EDGE_CURVE('',#11994,#11995,#10693,.T.);
#15123=EDGE_CURVE('',#11996,#11980,#6134,.T.);
#15124=EDGE_CURVE('',#11995,#11996,#6135,.T.);
#15125=EDGE_CURVE('',#11997,#11992,#6136,.F.);
#15126=EDGE_CURVE('',#11991,#11998,#6137,.T.);
#15127=EDGE_CURVE('',#11998,#11997,#6138,.T.);
#15128=EDGE_CURVE('',#11993,#11999,#6139,.T.);
#15129=EDGE_CURVE('',#11999,#11998,#10694,.T.);
#15130=EDGE_CURVE('',#11994,#12000,#6140,.T.);
#15131=EDGE_CURVE('',#12000,#11999,#6141,.T.);
#15132=EDGE_CURVE('',#11995,#12001,#6142,.T.);
#15133=EDGE_CURVE('',#12001,#12000,#10695,.T.);
#15134=EDGE_CURVE('',#11996,#12002,#6143,.F.);
#15135=EDGE_CURVE('',#12002,#12001,#6144,.T.);
#15136=EDGE_CURVE('',#12003,#12003,#10696,.T.);
#15137=EDGE_CURVE('',#12003,#12004,#6145,.T.);
#15138=EDGE_CURVE('',#12004,#12004,#10697,.T.);
#15139=EDGE_CURVE('',#12005,#12005,#10698,.T.);
#15140=EDGE_CURVE('',#12005,#12006,#6146,.T.);
#15141=EDGE_CURVE('',#12006,#12006,#10699,.T.);
#15142=EDGE_CURVE('',#12007,#12007,#10700,.T.);
#15143=EDGE_CURVE('',#12007,#12008,#6147,.T.);
#15144=EDGE_CURVE('',#12008,#12008,#10701,.T.);
#15145=EDGE_CURVE('',#12009,#12009,#10702,.T.);
#15146=EDGE_CURVE('',#12009,#12010,#6148,.T.);
#15147=EDGE_CURVE('',#12010,#12010,#10703,.T.);
#15148=EDGE_CURVE('',#12011,#12011,#10704,.T.);
#15149=EDGE_CURVE('',#12011,#12012,#6149,.T.);
#15150=EDGE_CURVE('',#12012,#12012,#10705,.T.);
#15151=EDGE_CURVE('',#12013,#12013,#10706,.T.);
#15152=EDGE_CURVE('',#12013,#12014,#6150,.T.);
#15153=EDGE_CURVE('',#12014,#12014,#10707,.T.);
#15154=EDGE_CURVE('',#12015,#12015,#10708,.T.);
#15155=EDGE_CURVE('',#12015,#12016,#6151,.T.);
#15156=EDGE_CURVE('',#12016,#12016,#10709,.T.);
#15157=EDGE_CURVE('',#12017,#12017,#10710,.T.);
#15158=EDGE_CURVE('',#12017,#12018,#6152,.T.);
#15159=EDGE_CURVE('',#12018,#12018,#10711,.T.);
#15160=EDGE_CURVE('',#12019,#12019,#10712,.T.);
#15161=EDGE_CURVE('',#12019,#12020,#6153,.T.);
#15162=EDGE_CURVE('',#12020,#12020,#10713,.T.);
#15163=EDGE_CURVE('',#12021,#12021,#10714,.T.);
#15164=EDGE_CURVE('',#12021,#12022,#6154,.T.);
#15165=EDGE_CURVE('',#12022,#12022,#10715,.T.);
#15166=EDGE_CURVE('',#12002,#12023,#6155,.T.);
#15167=EDGE_CURVE('',#12024,#11979,#6156,.T.);
#15168=EDGE_CURVE('',#12023,#12024,#6157,.T.);
#15169=EDGE_CURVE('',#12023,#12025,#6158,.T.);
#15170=EDGE_CURVE('',#12026,#12024,#6159,.T.);
#15171=EDGE_CURVE('',#12025,#12026,#6160,.T.);
#15172=EDGE_CURVE('',#12025,#12027,#6161,.T.);
#15173=EDGE_CURVE('',#12028,#12026,#6162,.T.);
#15174=EDGE_CURVE('',#12027,#12028,#6163,.T.);
#15175=EDGE_CURVE('',#12027,#12029,#6164,.T.);
#15176=EDGE_CURVE('',#12030,#12028,#6165,.T.);
#15177=EDGE_CURVE('',#12029,#12030,#6166,.T.);
#15178=EDGE_CURVE('',#12029,#12031,#6167,.T.);
#15179=EDGE_CURVE('',#12032,#12030,#6168,.T.);
#15180=EDGE_CURVE('',#12031,#12032,#6169,.T.);
#15181=EDGE_CURVE('',#12031,#12033,#6170,.T.);
#15182=EDGE_CURVE('',#12034,#12032,#6171,.T.);
#15183=EDGE_CURVE('',#12033,#12034,#6172,.T.);
#15184=EDGE_CURVE('',#12033,#12035,#6173,.T.);
#15185=EDGE_CURVE('',#12036,#12034,#6174,.T.);
#15186=EDGE_CURVE('',#12035,#12036,#6175,.T.);
#15187=EDGE_CURVE('',#12035,#12037,#6176,.T.);
#15188=EDGE_CURVE('',#12038,#12036,#6177,.T.);
#15189=EDGE_CURVE('',#12037,#12038,#6178,.T.);
#15190=EDGE_CURVE('',#12037,#12039,#6179,.T.);
#15191=EDGE_CURVE('',#12040,#12038,#6180,.T.);
#15192=EDGE_CURVE('',#12039,#12040,#6181,.T.);
#15193=EDGE_CURVE('',#12039,#12041,#6182,.T.);
#15194=EDGE_CURVE('',#12042,#12040,#6183,.T.);
#15195=EDGE_CURVE('',#12041,#12042,#6184,.T.);
#15196=EDGE_CURVE('',#12041,#12043,#6185,.T.);
#15197=EDGE_CURVE('',#12044,#12042,#6186,.T.);
#15198=EDGE_CURVE('',#12043,#12044,#6187,.T.);
#15199=EDGE_CURVE('',#12043,#12045,#6188,.T.);
#15200=EDGE_CURVE('',#12046,#12044,#6189,.T.);
#15201=EDGE_CURVE('',#12045,#12046,#6190,.T.);
#15202=EDGE_CURVE('',#12045,#12047,#6191,.T.);
#15203=EDGE_CURVE('',#12048,#12046,#6192,.T.);
#15204=EDGE_CURVE('',#12047,#12048,#6193,.T.);
#15205=EDGE_CURVE('',#12047,#12049,#6194,.T.);
#15206=EDGE_CURVE('',#12050,#12048,#6195,.T.);
#15207=EDGE_CURVE('',#12049,#12050,#6196,.T.);
#15208=EDGE_CURVE('',#12049,#12051,#6197,.T.);
#15209=EDGE_CURVE('',#12052,#12050,#6198,.T.);
#15210=EDGE_CURVE('',#12051,#12052,#6199,.T.);
#15211=EDGE_CURVE('',#12051,#12053,#6200,.T.);
#15212=EDGE_CURVE('',#12054,#12052,#6201,.T.);
#15213=EDGE_CURVE('',#12053,#12054,#6202,.T.);
#15214=EDGE_CURVE('',#12053,#12055,#6203,.T.);
#15215=EDGE_CURVE('',#12056,#12054,#6204,.T.);
#15216=EDGE_CURVE('',#12055,#12056,#6205,.T.);
#15217=EDGE_CURVE('',#12055,#12057,#6206,.T.);
#15218=EDGE_CURVE('',#12058,#12056,#6207,.T.);
#15219=EDGE_CURVE('',#12057,#12058,#6208,.T.);
#15220=EDGE_CURVE('',#12057,#12059,#6209,.T.);
#15221=EDGE_CURVE('',#12060,#12058,#6210,.T.);
#15222=EDGE_CURVE('',#12059,#12060,#6211,.T.);
#15223=EDGE_CURVE('',#12059,#12061,#6212,.T.);
#15224=EDGE_CURVE('',#12062,#12060,#6213,.T.);
#15225=EDGE_CURVE('',#12061,#12062,#6214,.T.);
#15226=EDGE_CURVE('',#12061,#12063,#6215,.T.);
#15227=EDGE_CURVE('',#12064,#12062,#6216,.T.);
#15228=EDGE_CURVE('',#12063,#12064,#6217,.T.);
#15229=EDGE_CURVE('',#12063,#12065,#6218,.T.);
#15230=EDGE_CURVE('',#12066,#12064,#6219,.T.);
#15231=EDGE_CURVE('',#12065,#12066,#6220,.T.);
#15232=EDGE_CURVE('',#12065,#12067,#6221,.T.);
#15233=EDGE_CURVE('',#12068,#12066,#6222,.T.);
#15234=EDGE_CURVE('',#12067,#12068,#6223,.T.);
#15235=EDGE_CURVE('',#12067,#12069,#6224,.T.);
#15236=EDGE_CURVE('',#12070,#12068,#6225,.T.);
#15237=EDGE_CURVE('',#12069,#12070,#6226,.T.);
#15238=EDGE_CURVE('',#12069,#12071,#6227,.T.);
#15239=EDGE_CURVE('',#12072,#12070,#6228,.T.);
#15240=EDGE_CURVE('',#12071,#12072,#6229,.T.);
#15241=EDGE_CURVE('',#12071,#12073,#6230,.T.);
#15242=EDGE_CURVE('',#12074,#12072,#6231,.T.);
#15243=EDGE_CURVE('',#12073,#12074,#6232,.T.);
#15244=EDGE_CURVE('',#12073,#12075,#6233,.T.);
#15245=EDGE_CURVE('',#12076,#12074,#6234,.T.);
#15246=EDGE_CURVE('',#12075,#12076,#6235,.T.);
#15247=EDGE_CURVE('',#12075,#12077,#6236,.T.);
#15248=EDGE_CURVE('',#12078,#12076,#6237,.T.);
#15249=EDGE_CURVE('',#12077,#12078,#6238,.T.);
#15250=EDGE_CURVE('',#12077,#12079,#6239,.T.);
#15251=EDGE_CURVE('',#12080,#12078,#6240,.T.);
#15252=EDGE_CURVE('',#12079,#12080,#6241,.T.);
#15253=EDGE_CURVE('',#12079,#12081,#6242,.T.);
#15254=EDGE_CURVE('',#12082,#12080,#6243,.T.);
#15255=EDGE_CURVE('',#12081,#12082,#6244,.T.);
#15256=EDGE_CURVE('',#12081,#12083,#6245,.T.);
#15257=EDGE_CURVE('',#12084,#12082,#6246,.T.);
#15258=EDGE_CURVE('',#12083,#12084,#6247,.T.);
#15259=EDGE_CURVE('',#12083,#12085,#6248,.T.);
#15260=EDGE_CURVE('',#12086,#12084,#6249,.T.);
#15261=EDGE_CURVE('',#12085,#12086,#6250,.T.);
#15262=EDGE_CURVE('',#12085,#12087,#6251,.T.);
#15263=EDGE_CURVE('',#12088,#12086,#6252,.T.);
#15264=EDGE_CURVE('',#12087,#12088,#6253,.T.);
#15265=EDGE_CURVE('',#12087,#12089,#6254,.T.);
#15266=EDGE_CURVE('',#12090,#12088,#6255,.T.);
#15267=EDGE_CURVE('',#12089,#12090,#6256,.T.);
#15268=EDGE_CURVE('',#12089,#12091,#6257,.T.);
#15269=EDGE_CURVE('',#12092,#12090,#6258,.T.);
#15270=EDGE_CURVE('',#12091,#12092,#6259,.T.);
#15271=EDGE_CURVE('',#12091,#12093,#6260,.T.);
#15272=EDGE_CURVE('',#12094,#12092,#6261,.T.);
#15273=EDGE_CURVE('',#12093,#12094,#6262,.T.);
#15274=EDGE_CURVE('',#12093,#12095,#6263,.T.);
#15275=EDGE_CURVE('',#12096,#12094,#6264,.T.);
#15276=EDGE_CURVE('',#12095,#12096,#6265,.T.);
#15277=EDGE_CURVE('',#12095,#12097,#6266,.T.);
#15278=EDGE_CURVE('',#12098,#12096,#6267,.T.);
#15279=EDGE_CURVE('',#12097,#12098,#6268,.T.);
#15280=EDGE_CURVE('',#12097,#12099,#6269,.T.);
#15281=EDGE_CURVE('',#12100,#12098,#6270,.T.);
#15282=EDGE_CURVE('',#12099,#12100,#6271,.T.);
#15283=EDGE_CURVE('',#12099,#12101,#6272,.T.);
#15284=EDGE_CURVE('',#12102,#12100,#6273,.T.);
#15285=EDGE_CURVE('',#12101,#12102,#6274,.T.);
#15286=EDGE_CURVE('',#12101,#12103,#6275,.T.);
#15287=EDGE_CURVE('',#12104,#12102,#6276,.T.);
#15288=EDGE_CURVE('',#12103,#12104,#6277,.T.);
#15289=EDGE_CURVE('',#12103,#12105,#6278,.T.);
#15290=EDGE_CURVE('',#12106,#12104,#6279,.T.);
#15291=EDGE_CURVE('',#12105,#12106,#6280,.T.);
#15292=EDGE_CURVE('',#12105,#12107,#6281,.T.);
#15293=EDGE_CURVE('',#12108,#12106,#6282,.T.);
#15294=EDGE_CURVE('',#12107,#12108,#6283,.T.);
#15295=EDGE_CURVE('',#12107,#12109,#6284,.T.);
#15296=EDGE_CURVE('',#12110,#12108,#6285,.T.);
#15297=EDGE_CURVE('',#12109,#12110,#6286,.T.);
#15298=EDGE_CURVE('',#12109,#12111,#6287,.T.);
#15299=EDGE_CURVE('',#12112,#12110,#6288,.T.);
#15300=EDGE_CURVE('',#12111,#12112,#6289,.T.);
#15301=EDGE_CURVE('',#12111,#12113,#6290,.T.);
#15302=EDGE_CURVE('',#12114,#12112,#6291,.T.);
#15303=EDGE_CURVE('',#12113,#12114,#6292,.T.);
#15304=EDGE_CURVE('',#12113,#12115,#6293,.T.);
#15305=EDGE_CURVE('',#12116,#12114,#6294,.T.);
#15306=EDGE_CURVE('',#12115,#12116,#6295,.T.);
#15307=EDGE_CURVE('',#12115,#12117,#6296,.T.);
#15308=EDGE_CURVE('',#12118,#12116,#6297,.T.);
#15309=EDGE_CURVE('',#12117,#12118,#6298,.T.);
#15310=EDGE_CURVE('',#12117,#12119,#6299,.T.);
#15311=EDGE_CURVE('',#12120,#12118,#6300,.T.);
#15312=EDGE_CURVE('',#12119,#12120,#6301,.T.);
#15313=EDGE_CURVE('',#12119,#12121,#6302,.T.);
#15314=EDGE_CURVE('',#12122,#12120,#6303,.T.);
#15315=EDGE_CURVE('',#12121,#12122,#6304,.T.);
#15316=EDGE_CURVE('',#12121,#12123,#6305,.T.);
#15317=EDGE_CURVE('',#12124,#12122,#6306,.T.);
#15318=EDGE_CURVE('',#12123,#12124,#6307,.T.);
#15319=EDGE_CURVE('',#12123,#12125,#6308,.T.);
#15320=EDGE_CURVE('',#12126,#12124,#6309,.T.);
#15321=EDGE_CURVE('',#12125,#12126,#6310,.T.);
#15322=EDGE_CURVE('',#12125,#12127,#6311,.T.);
#15323=EDGE_CURVE('',#12128,#12126,#6312,.T.);
#15324=EDGE_CURVE('',#12127,#12128,#6313,.T.);
#15325=EDGE_CURVE('',#12127,#12129,#6314,.T.);
#15326=EDGE_CURVE('',#12130,#12128,#6315,.T.);
#15327=EDGE_CURVE('',#12129,#12130,#6316,.T.);
#15328=EDGE_CURVE('',#12129,#12131,#6317,.T.);
#15329=EDGE_CURVE('',#12132,#12130,#6318,.T.);
#15330=EDGE_CURVE('',#12131,#12132,#6319,.T.);
#15331=EDGE_CURVE('',#12131,#12133,#6320,.T.);
#15332=EDGE_CURVE('',#12134,#12132,#6321,.T.);
#15333=EDGE_CURVE('',#12133,#12134,#6322,.T.);
#15334=EDGE_CURVE('',#12133,#12135,#6323,.T.);
#15335=EDGE_CURVE('',#12136,#12134,#6324,.T.);
#15336=EDGE_CURVE('',#12135,#12136,#6325,.T.);
#15337=EDGE_CURVE('',#12135,#12137,#6326,.T.);
#15338=EDGE_CURVE('',#12138,#12136,#6327,.T.);
#15339=EDGE_CURVE('',#12137,#12138,#6328,.T.);
#15340=EDGE_CURVE('',#12137,#12139,#6329,.T.);
#15341=EDGE_CURVE('',#12140,#12138,#6330,.T.);
#15342=EDGE_CURVE('',#12139,#12140,#6331,.T.);
#15343=EDGE_CURVE('',#12139,#12141,#6332,.T.);
#15344=EDGE_CURVE('',#12142,#12140,#6333,.T.);
#15345=EDGE_CURVE('',#12141,#12142,#6334,.T.);
#15346=EDGE_CURVE('',#12141,#12143,#6335,.T.);
#15347=EDGE_CURVE('',#12144,#12142,#6336,.T.);
#15348=EDGE_CURVE('',#12143,#12144,#6337,.T.);
#15349=EDGE_CURVE('',#12143,#12145,#6338,.T.);
#15350=EDGE_CURVE('',#12146,#12144,#6339,.T.);
#15351=EDGE_CURVE('',#12145,#12146,#6340,.T.);
#15352=EDGE_CURVE('',#12145,#12147,#6341,.T.);
#15353=EDGE_CURVE('',#12148,#12146,#6342,.T.);
#15354=EDGE_CURVE('',#12147,#12148,#6343,.T.);
#15355=EDGE_CURVE('',#12147,#12149,#6344,.T.);
#15356=EDGE_CURVE('',#12150,#12148,#6345,.T.);
#15357=EDGE_CURVE('',#12149,#12150,#6346,.T.);
#15358=EDGE_CURVE('',#12149,#12151,#6347,.T.);
#15359=EDGE_CURVE('',#12152,#12150,#6348,.T.);
#15360=EDGE_CURVE('',#12151,#12152,#6349,.T.);
#15361=EDGE_CURVE('',#12151,#12153,#6350,.T.);
#15362=EDGE_CURVE('',#12154,#12152,#6351,.T.);
#15363=EDGE_CURVE('',#12153,#12154,#6352,.T.);
#15364=EDGE_CURVE('',#12153,#12155,#6353,.T.);
#15365=EDGE_CURVE('',#12156,#12154,#6354,.T.);
#15366=EDGE_CURVE('',#12155,#12156,#6355,.T.);
#15367=EDGE_CURVE('',#12155,#12157,#6356,.T.);
#15368=EDGE_CURVE('',#12158,#12156,#6357,.T.);
#15369=EDGE_CURVE('',#12157,#12158,#6358,.T.);
#15370=EDGE_CURVE('',#12157,#12159,#6359,.T.);
#15371=EDGE_CURVE('',#12160,#12158,#6360,.T.);
#15372=EDGE_CURVE('',#12159,#12160,#6361,.T.);
#15373=EDGE_CURVE('',#12159,#12161,#6362,.T.);
#15374=EDGE_CURVE('',#12162,#12160,#6363,.T.);
#15375=EDGE_CURVE('',#12161,#12162,#6364,.T.);
#15376=EDGE_CURVE('',#12161,#12163,#6365,.T.);
#15377=EDGE_CURVE('',#12164,#12162,#6366,.T.);
#15378=EDGE_CURVE('',#12163,#12164,#6367,.T.);
#15379=EDGE_CURVE('',#12163,#12165,#6368,.T.);
#15380=EDGE_CURVE('',#12166,#12164,#6369,.T.);
#15381=EDGE_CURVE('',#12165,#12166,#6370,.T.);
#15382=EDGE_CURVE('',#12165,#12167,#6371,.T.);
#15383=EDGE_CURVE('',#12168,#12166,#6372,.T.);
#15384=EDGE_CURVE('',#12167,#12168,#6373,.T.);
#15385=EDGE_CURVE('',#12167,#12169,#6374,.T.);
#15386=EDGE_CURVE('',#12170,#12168,#6375,.T.);
#15387=EDGE_CURVE('',#12169,#12170,#6376,.T.);
#15388=EDGE_CURVE('',#12169,#12171,#6377,.T.);
#15389=EDGE_CURVE('',#12172,#12170,#6378,.T.);
#15390=EDGE_CURVE('',#12171,#12172,#6379,.T.);
#15391=EDGE_CURVE('',#12171,#12173,#6380,.T.);
#15392=EDGE_CURVE('',#12174,#12172,#6381,.T.);
#15393=EDGE_CURVE('',#12173,#12174,#6382,.T.);
#15394=EDGE_CURVE('',#12173,#12175,#6383,.T.);
#15395=EDGE_CURVE('',#12176,#12174,#6384,.T.);
#15396=EDGE_CURVE('',#12175,#12176,#6385,.T.);
#15397=EDGE_CURVE('',#12175,#12177,#6386,.T.);
#15398=EDGE_CURVE('',#12178,#12176,#6387,.T.);
#15399=EDGE_CURVE('',#12177,#12178,#6388,.T.);
#15400=EDGE_CURVE('',#12177,#12179,#6389,.T.);
#15401=EDGE_CURVE('',#12180,#12178,#6390,.T.);
#15402=EDGE_CURVE('',#12179,#12180,#6391,.T.);
#15403=EDGE_CURVE('',#12179,#12181,#6392,.T.);
#15404=EDGE_CURVE('',#12182,#12180,#6393,.T.);
#15405=EDGE_CURVE('',#12181,#12182,#6394,.T.);
#15406=EDGE_CURVE('',#12181,#12183,#6395,.T.);
#15407=EDGE_CURVE('',#12184,#12182,#6396,.T.);
#15408=EDGE_CURVE('',#12183,#12184,#6397,.T.);
#15409=EDGE_CURVE('',#12183,#12185,#6398,.T.);
#15410=EDGE_CURVE('',#12186,#12184,#6399,.T.);
#15411=EDGE_CURVE('',#12185,#12186,#6400,.T.);
#15412=EDGE_CURVE('',#12185,#12187,#6401,.T.);
#15413=EDGE_CURVE('',#12188,#12186,#6402,.T.);
#15414=EDGE_CURVE('',#12187,#12188,#6403,.T.);
#15415=EDGE_CURVE('',#12187,#12189,#6404,.T.);
#15416=EDGE_CURVE('',#12190,#12188,#6405,.T.);
#15417=EDGE_CURVE('',#12189,#12190,#6406,.T.);
#15418=EDGE_CURVE('',#12189,#12191,#6407,.T.);
#15419=EDGE_CURVE('',#12192,#12190,#6408,.T.);
#15420=EDGE_CURVE('',#12191,#12192,#6409,.T.);
#15421=EDGE_CURVE('',#12191,#12193,#6410,.T.);
#15422=EDGE_CURVE('',#12194,#12192,#6411,.T.);
#15423=EDGE_CURVE('',#12193,#12194,#6412,.T.);
#15424=EDGE_CURVE('',#12193,#12195,#6413,.T.);
#15425=EDGE_CURVE('',#12196,#12194,#6414,.T.);
#15426=EDGE_CURVE('',#12195,#12196,#6415,.T.);
#15427=EDGE_CURVE('',#12195,#12197,#6416,.T.);
#15428=EDGE_CURVE('',#12198,#12196,#6417,.T.);
#15429=EDGE_CURVE('',#12197,#12198,#6418,.T.);
#15430=EDGE_CURVE('',#12197,#12199,#6419,.T.);
#15431=EDGE_CURVE('',#12200,#12198,#6420,.T.);
#15432=EDGE_CURVE('',#12199,#12200,#6421,.T.);
#15433=EDGE_CURVE('',#12199,#12201,#6422,.T.);
#15434=EDGE_CURVE('',#12202,#12200,#6423,.T.);
#15435=EDGE_CURVE('',#12201,#12202,#6424,.T.);
#15436=EDGE_CURVE('',#12201,#12203,#6425,.T.);
#15437=EDGE_CURVE('',#12204,#12202,#6426,.T.);
#15438=EDGE_CURVE('',#12203,#12204,#6427,.T.);
#15439=EDGE_CURVE('',#12203,#12205,#6428,.T.);
#15440=EDGE_CURVE('',#12206,#12204,#6429,.T.);
#15441=EDGE_CURVE('',#12205,#12206,#6430,.T.);
#15442=EDGE_CURVE('',#12205,#12207,#6431,.T.);
#15443=EDGE_CURVE('',#12208,#12206,#6432,.T.);
#15444=EDGE_CURVE('',#12207,#12208,#6433,.T.);
#15445=EDGE_CURVE('',#12207,#12209,#6434,.T.);
#15446=EDGE_CURVE('',#12210,#12208,#6435,.T.);
#15447=EDGE_CURVE('',#12209,#12210,#6436,.T.);
#15448=EDGE_CURVE('',#12209,#12211,#6437,.T.);
#15449=EDGE_CURVE('',#12212,#12210,#6438,.T.);
#15450=EDGE_CURVE('',#12211,#12212,#6439,.T.);
#15451=EDGE_CURVE('',#12211,#12213,#6440,.T.);
#15452=EDGE_CURVE('',#12214,#12212,#6441,.T.);
#15453=EDGE_CURVE('',#12213,#12214,#6442,.T.);
#15454=EDGE_CURVE('',#12213,#12215,#6443,.T.);
#15455=EDGE_CURVE('',#12216,#12214,#6444,.T.);
#15456=EDGE_CURVE('',#12215,#12216,#6445,.T.);
#15457=EDGE_CURVE('',#12215,#12217,#6446,.T.);
#15458=EDGE_CURVE('',#12218,#12216,#6447,.T.);
#15459=EDGE_CURVE('',#12217,#12218,#6448,.T.);
#15460=EDGE_CURVE('',#12217,#12219,#6449,.T.);
#15461=EDGE_CURVE('',#12220,#12218,#6450,.T.);
#15462=EDGE_CURVE('',#12219,#12220,#6451,.T.);
#15463=EDGE_CURVE('',#12219,#12221,#6452,.T.);
#15464=EDGE_CURVE('',#12222,#12220,#6453,.T.);
#15465=EDGE_CURVE('',#12221,#12222,#6454,.T.);
#15466=EDGE_CURVE('',#12221,#12223,#6455,.T.);
#15467=EDGE_CURVE('',#12224,#12222,#6456,.T.);
#15468=EDGE_CURVE('',#12223,#12224,#6457,.T.);
#15469=EDGE_CURVE('',#12223,#12225,#6458,.T.);
#15470=EDGE_CURVE('',#12226,#12224,#6459,.T.);
#15471=EDGE_CURVE('',#12225,#12226,#6460,.T.);
#15472=EDGE_CURVE('',#12225,#12227,#6461,.T.);
#15473=EDGE_CURVE('',#12228,#12226,#6462,.T.);
#15474=EDGE_CURVE('',#12227,#12228,#6463,.T.);
#15475=EDGE_CURVE('',#12227,#12229,#6464,.T.);
#15476=EDGE_CURVE('',#12230,#12228,#6465,.T.);
#15477=EDGE_CURVE('',#12229,#12230,#6466,.T.);
#15478=EDGE_CURVE('',#12229,#12231,#6467,.T.);
#15479=EDGE_CURVE('',#12232,#12230,#6468,.T.);
#15480=EDGE_CURVE('',#12231,#12232,#6469,.T.);
#15481=EDGE_CURVE('',#12231,#12233,#6470,.T.);
#15482=EDGE_CURVE('',#12234,#12232,#6471,.T.);
#15483=EDGE_CURVE('',#12233,#12234,#6472,.T.);
#15484=EDGE_CURVE('',#12233,#12235,#6473,.T.);
#15485=EDGE_CURVE('',#12236,#12234,#6474,.T.);
#15486=EDGE_CURVE('',#12235,#12236,#6475,.T.);
#15487=EDGE_CURVE('',#12235,#12237,#6476,.T.);
#15488=EDGE_CURVE('',#12238,#12236,#6477,.T.);
#15489=EDGE_CURVE('',#12237,#12238,#6478,.T.);
#15490=EDGE_CURVE('',#12237,#12239,#6479,.T.);
#15491=EDGE_CURVE('',#12240,#12238,#6480,.T.);
#15492=EDGE_CURVE('',#12239,#12240,#6481,.T.);
#15493=EDGE_CURVE('',#12239,#12241,#6482,.T.);
#15494=EDGE_CURVE('',#12242,#12240,#6483,.T.);
#15495=EDGE_CURVE('',#12241,#12242,#6484,.T.);
#15496=EDGE_CURVE('',#12241,#12243,#6485,.T.);
#15497=EDGE_CURVE('',#12244,#12242,#6486,.T.);
#15498=EDGE_CURVE('',#12243,#12244,#6487,.T.);
#15499=EDGE_CURVE('',#12243,#12245,#6488,.T.);
#15500=EDGE_CURVE('',#12246,#12244,#6489,.T.);
#15501=EDGE_CURVE('',#12245,#12246,#6490,.T.);
#15502=EDGE_CURVE('',#12245,#12247,#6491,.T.);
#15503=EDGE_CURVE('',#12248,#12246,#6492,.T.);
#15504=EDGE_CURVE('',#12247,#12248,#6493,.T.);
#15505=EDGE_CURVE('',#12247,#12249,#6494,.T.);
#15506=EDGE_CURVE('',#12250,#12248,#6495,.T.);
#15507=EDGE_CURVE('',#12249,#12250,#6496,.T.);
#15508=EDGE_CURVE('',#12249,#12251,#6497,.T.);
#15509=EDGE_CURVE('',#12252,#12250,#6498,.T.);
#15510=EDGE_CURVE('',#12251,#12252,#6499,.T.);
#15511=EDGE_CURVE('',#12251,#12253,#6500,.T.);
#15512=EDGE_CURVE('',#12254,#12252,#6501,.T.);
#15513=EDGE_CURVE('',#12253,#12254,#6502,.T.);
#15514=EDGE_CURVE('',#12253,#12255,#6503,.T.);
#15515=EDGE_CURVE('',#12256,#12254,#6504,.T.);
#15516=EDGE_CURVE('',#12255,#12256,#6505,.T.);
#15517=EDGE_CURVE('',#12255,#12257,#6506,.T.);
#15518=EDGE_CURVE('',#12258,#12256,#6507,.T.);
#15519=EDGE_CURVE('',#12257,#12258,#6508,.T.);
#15520=EDGE_CURVE('',#12257,#12259,#6509,.T.);
#15521=EDGE_CURVE('',#12260,#12258,#6510,.T.);
#15522=EDGE_CURVE('',#12259,#12260,#6511,.T.);
#15523=EDGE_CURVE('',#12259,#12261,#6512,.T.);
#15524=EDGE_CURVE('',#12262,#12260,#6513,.T.);
#15525=EDGE_CURVE('',#12261,#12262,#6514,.T.);
#15526=EDGE_CURVE('',#12261,#12263,#6515,.T.);
#15527=EDGE_CURVE('',#12264,#12262,#6516,.T.);
#15528=EDGE_CURVE('',#12263,#12264,#6517,.T.);
#15529=EDGE_CURVE('',#12263,#12265,#6518,.T.);
#15530=EDGE_CURVE('',#12266,#12264,#6519,.T.);
#15531=EDGE_CURVE('',#12265,#12266,#6520,.T.);
#15532=EDGE_CURVE('',#12265,#12267,#6521,.T.);
#15533=EDGE_CURVE('',#12268,#12266,#6522,.T.);
#15534=EDGE_CURVE('',#12267,#12268,#6523,.T.);
#15535=EDGE_CURVE('',#12267,#12269,#6524,.T.);
#15536=EDGE_CURVE('',#12270,#12268,#6525,.T.);
#15537=EDGE_CURVE('',#12269,#12270,#6526,.T.);
#15538=EDGE_CURVE('',#12269,#12271,#6527,.T.);
#15539=EDGE_CURVE('',#12272,#12270,#6528,.T.);
#15540=EDGE_CURVE('',#12271,#12272,#6529,.T.);
#15541=EDGE_CURVE('',#12271,#12273,#6530,.T.);
#15542=EDGE_CURVE('',#12274,#12272,#6531,.T.);
#15543=EDGE_CURVE('',#12273,#12274,#6532,.T.);
#15544=EDGE_CURVE('',#12273,#12275,#6533,.T.);
#15545=EDGE_CURVE('',#12276,#12274,#6534,.T.);
#15546=EDGE_CURVE('',#12275,#12276,#6535,.T.);
#15547=EDGE_CURVE('',#12275,#12277,#6536,.T.);
#15548=EDGE_CURVE('',#12278,#12276,#6537,.T.);
#15549=EDGE_CURVE('',#12277,#12278,#6538,.T.);
#15550=EDGE_CURVE('',#12277,#12279,#6539,.T.);
#15551=EDGE_CURVE('',#12280,#12278,#6540,.T.);
#15552=EDGE_CURVE('',#12279,#12280,#6541,.T.);
#15553=EDGE_CURVE('',#12279,#12281,#6542,.T.);
#15554=EDGE_CURVE('',#12282,#12280,#6543,.T.);
#15555=EDGE_CURVE('',#12281,#12282,#6544,.T.);
#15556=EDGE_CURVE('',#12281,#12283,#6545,.T.);
#15557=EDGE_CURVE('',#12284,#12282,#6546,.T.);
#15558=EDGE_CURVE('',#12283,#12284,#6547,.T.);
#15559=EDGE_CURVE('',#12283,#12285,#6548,.T.);
#15560=EDGE_CURVE('',#12286,#12284,#6549,.T.);
#15561=EDGE_CURVE('',#12285,#12286,#6550,.T.);
#15562=EDGE_CURVE('',#12285,#12287,#6551,.T.);
#15563=EDGE_CURVE('',#12288,#12286,#6552,.T.);
#15564=EDGE_CURVE('',#12287,#12288,#6553,.T.);
#15565=EDGE_CURVE('',#12287,#12289,#6554,.T.);
#15566=EDGE_CURVE('',#12290,#12288,#6555,.T.);
#15567=EDGE_CURVE('',#12289,#12290,#6556,.T.);
#15568=EDGE_CURVE('',#12289,#12291,#6557,.T.);
#15569=EDGE_CURVE('',#12292,#12290,#6558,.T.);
#15570=EDGE_CURVE('',#12291,#12292,#6559,.T.);
#15571=EDGE_CURVE('',#12291,#12293,#6560,.T.);
#15572=EDGE_CURVE('',#12294,#12292,#6561,.T.);
#15573=EDGE_CURVE('',#12293,#12294,#6562,.T.);
#15574=EDGE_CURVE('',#12293,#12295,#6563,.T.);
#15575=EDGE_CURVE('',#12296,#12294,#6564,.T.);
#15576=EDGE_CURVE('',#12295,#12296,#6565,.T.);
#15577=EDGE_CURVE('',#12295,#12297,#6566,.T.);
#15578=EDGE_CURVE('',#12298,#12296,#6567,.T.);
#15579=EDGE_CURVE('',#12297,#12298,#6568,.T.);
#15580=EDGE_CURVE('',#12297,#12299,#6569,.T.);
#15581=EDGE_CURVE('',#12300,#12298,#6570,.T.);
#15582=EDGE_CURVE('',#12299,#12300,#6571,.T.);
#15583=EDGE_CURVE('',#12299,#12301,#6572,.T.);
#15584=EDGE_CURVE('',#12302,#12300,#6573,.T.);
#15585=EDGE_CURVE('',#12301,#12302,#6574,.T.);
#15586=EDGE_CURVE('',#12301,#12303,#6575,.T.);
#15587=EDGE_CURVE('',#12304,#12302,#6576,.T.);
#15588=EDGE_CURVE('',#12303,#12304,#6577,.T.);
#15589=EDGE_CURVE('',#12303,#12305,#6578,.T.);
#15590=EDGE_CURVE('',#12306,#12304,#6579,.T.);
#15591=EDGE_CURVE('',#12305,#12306,#6580,.T.);
#15592=EDGE_CURVE('',#12305,#12307,#6581,.T.);
#15593=EDGE_CURVE('',#12308,#12306,#6582,.T.);
#15594=EDGE_CURVE('',#12307,#12308,#6583,.T.);
#15595=EDGE_CURVE('',#12307,#12309,#6584,.T.);
#15596=EDGE_CURVE('',#12310,#12308,#6585,.T.);
#15597=EDGE_CURVE('',#12309,#12310,#6586,.T.);
#15598=EDGE_CURVE('',#12309,#12311,#6587,.T.);
#15599=EDGE_CURVE('',#12312,#12310,#6588,.T.);
#15600=EDGE_CURVE('',#12311,#12312,#6589,.T.);
#15601=EDGE_CURVE('',#12311,#12313,#6590,.T.);
#15602=EDGE_CURVE('',#12314,#12312,#6591,.T.);
#15603=EDGE_CURVE('',#12313,#12314,#6592,.T.);
#15604=EDGE_CURVE('',#12313,#12315,#6593,.T.);
#15605=EDGE_CURVE('',#12316,#12314,#6594,.T.);
#15606=EDGE_CURVE('',#12315,#12316,#6595,.T.);
#15607=EDGE_CURVE('',#12315,#12317,#6596,.T.);
#15608=EDGE_CURVE('',#12318,#12316,#6597,.T.);
#15609=EDGE_CURVE('',#12317,#12318,#6598,.T.);
#15610=EDGE_CURVE('',#12317,#12319,#6599,.T.);
#15611=EDGE_CURVE('',#12320,#12318,#6600,.T.);
#15612=EDGE_CURVE('',#12319,#12320,#6601,.T.);
#15613=EDGE_CURVE('',#12319,#12321,#6602,.T.);
#15614=EDGE_CURVE('',#12322,#12320,#6603,.T.);
#15615=EDGE_CURVE('',#12321,#12322,#6604,.T.);
#15616=EDGE_CURVE('',#12321,#12323,#6605,.T.);
#15617=EDGE_CURVE('',#12324,#12322,#6606,.T.);
#15618=EDGE_CURVE('',#12323,#12324,#6607,.T.);
#15619=EDGE_CURVE('',#12323,#12325,#6608,.T.);
#15620=EDGE_CURVE('',#12326,#12324,#6609,.T.);
#15621=EDGE_CURVE('',#12325,#12326,#6610,.T.);
#15622=EDGE_CURVE('',#12325,#12327,#6611,.T.);
#15623=EDGE_CURVE('',#12328,#12326,#6612,.T.);
#15624=EDGE_CURVE('',#12327,#12328,#6613,.T.);
#15625=EDGE_CURVE('',#12327,#12329,#6614,.T.);
#15626=EDGE_CURVE('',#12330,#12328,#6615,.T.);
#15627=EDGE_CURVE('',#12329,#12330,#6616,.T.);
#15628=EDGE_CURVE('',#12329,#12331,#6617,.T.);
#15629=EDGE_CURVE('',#12332,#12330,#6618,.T.);
#15630=EDGE_CURVE('',#12331,#12332,#6619,.T.);
#15631=EDGE_CURVE('',#12331,#12333,#6620,.T.);
#15632=EDGE_CURVE('',#12334,#12332,#6621,.T.);
#15633=EDGE_CURVE('',#12333,#12334,#6622,.T.);
#15634=EDGE_CURVE('',#12333,#12335,#6623,.T.);
#15635=EDGE_CURVE('',#12336,#12334,#6624,.T.);
#15636=EDGE_CURVE('',#12335,#12336,#6625,.T.);
#15637=EDGE_CURVE('',#12335,#12337,#6626,.T.);
#15638=EDGE_CURVE('',#12338,#12336,#6627,.T.);
#15639=EDGE_CURVE('',#12337,#12338,#6628,.T.);
#15640=EDGE_CURVE('',#12337,#12339,#6629,.T.);
#15641=EDGE_CURVE('',#12340,#12338,#6630,.T.);
#15642=EDGE_CURVE('',#12339,#12340,#6631,.T.);
#15643=EDGE_CURVE('',#12339,#12341,#6632,.T.);
#15644=EDGE_CURVE('',#12342,#12340,#6633,.T.);
#15645=EDGE_CURVE('',#12341,#12342,#6634,.T.);
#15646=EDGE_CURVE('',#12341,#12343,#6635,.T.);
#15647=EDGE_CURVE('',#12344,#12342,#6636,.T.);
#15648=EDGE_CURVE('',#12343,#12344,#6637,.T.);
#15649=EDGE_CURVE('',#12343,#12345,#6638,.T.);
#15650=EDGE_CURVE('',#12346,#12344,#6639,.T.);
#15651=EDGE_CURVE('',#12345,#12346,#6640,.T.);
#15652=EDGE_CURVE('',#12345,#12347,#6641,.T.);
#15653=EDGE_CURVE('',#12348,#12346,#6642,.T.);
#15654=EDGE_CURVE('',#12347,#12348,#6643,.T.);
#15655=EDGE_CURVE('',#12347,#12349,#6644,.T.);
#15656=EDGE_CURVE('',#12350,#12348,#6645,.T.);
#15657=EDGE_CURVE('',#12349,#12350,#6646,.T.);
#15658=EDGE_CURVE('',#12349,#12351,#6647,.T.);
#15659=EDGE_CURVE('',#12352,#12350,#6648,.T.);
#15660=EDGE_CURVE('',#12351,#12352,#6649,.T.);
#15661=EDGE_CURVE('',#12351,#12353,#6650,.T.);
#15662=EDGE_CURVE('',#12354,#12352,#6651,.T.);
#15663=EDGE_CURVE('',#12353,#12354,#6652,.T.);
#15664=EDGE_CURVE('',#12353,#12355,#6653,.T.);
#15665=EDGE_CURVE('',#12356,#12354,#6654,.T.);
#15666=EDGE_CURVE('',#12355,#12356,#6655,.T.);
#15667=EDGE_CURVE('',#12355,#12357,#6656,.T.);
#15668=EDGE_CURVE('',#12358,#12356,#6657,.T.);
#15669=EDGE_CURVE('',#12357,#12358,#6658,.T.);
#15670=EDGE_CURVE('',#12357,#12359,#6659,.T.);
#15671=EDGE_CURVE('',#12360,#12358,#6660,.T.);
#15672=EDGE_CURVE('',#12359,#12360,#6661,.T.);
#15673=EDGE_CURVE('',#12359,#12361,#6662,.T.);
#15674=EDGE_CURVE('',#12362,#12360,#6663,.T.);
#15675=EDGE_CURVE('',#12361,#12362,#6664,.T.);
#15676=EDGE_CURVE('',#12361,#12363,#6665,.T.);
#15677=EDGE_CURVE('',#12364,#12362,#6666,.T.);
#15678=EDGE_CURVE('',#12363,#12364,#6667,.T.);
#15679=EDGE_CURVE('',#12363,#12365,#6668,.T.);
#15680=EDGE_CURVE('',#12366,#12364,#6669,.T.);
#15681=EDGE_CURVE('',#12365,#12366,#6670,.T.);
#15682=EDGE_CURVE('',#12365,#12367,#6671,.T.);
#15683=EDGE_CURVE('',#12368,#12366,#6672,.T.);
#15684=EDGE_CURVE('',#12367,#12368,#6673,.T.);
#15685=EDGE_CURVE('',#12367,#12369,#6674,.T.);
#15686=EDGE_CURVE('',#12370,#12368,#6675,.T.);
#15687=EDGE_CURVE('',#12369,#12370,#6676,.T.);
#15688=EDGE_CURVE('',#12369,#12371,#6677,.T.);
#15689=EDGE_CURVE('',#12372,#12370,#6678,.T.);
#15690=EDGE_CURVE('',#12371,#12372,#6679,.T.);
#15691=EDGE_CURVE('',#12371,#12373,#6680,.T.);
#15692=EDGE_CURVE('',#12374,#12372,#6681,.T.);
#15693=EDGE_CURVE('',#12373,#12374,#6682,.T.);
#15694=EDGE_CURVE('',#12373,#12375,#6683,.T.);
#15695=EDGE_CURVE('',#12376,#12374,#6684,.T.);
#15696=EDGE_CURVE('',#12375,#12376,#6685,.T.);
#15697=EDGE_CURVE('',#12375,#12377,#6686,.T.);
#15698=EDGE_CURVE('',#12378,#12376,#6687,.T.);
#15699=EDGE_CURVE('',#12377,#12378,#6688,.T.);
#15700=EDGE_CURVE('',#12377,#12379,#6689,.T.);
#15701=EDGE_CURVE('',#12380,#12378,#6690,.T.);
#15702=EDGE_CURVE('',#12379,#12380,#6691,.T.);
#15703=EDGE_CURVE('',#12379,#12381,#6692,.T.);
#15704=EDGE_CURVE('',#12382,#12380,#6693,.T.);
#15705=EDGE_CURVE('',#12381,#12382,#6694,.T.);
#15706=EDGE_CURVE('',#12381,#12383,#6695,.T.);
#15707=EDGE_CURVE('',#12384,#12382,#6696,.T.);
#15708=EDGE_CURVE('',#12383,#12384,#6697,.T.);
#15709=EDGE_CURVE('',#12383,#12385,#6698,.T.);
#15710=EDGE_CURVE('',#12386,#12384,#6699,.T.);
#15711=EDGE_CURVE('',#12385,#12386,#6700,.T.);
#15712=EDGE_CURVE('',#12385,#12387,#6701,.T.);
#15713=EDGE_CURVE('',#12388,#12386,#6702,.T.);
#15714=EDGE_CURVE('',#12387,#12388,#6703,.T.);
#15715=EDGE_CURVE('',#12387,#12389,#6704,.T.);
#15716=EDGE_CURVE('',#12390,#12388,#6705,.T.);
#15717=EDGE_CURVE('',#12389,#12390,#6706,.T.);
#15718=EDGE_CURVE('',#12389,#12391,#6707,.T.);
#15719=EDGE_CURVE('',#12392,#12390,#6708,.T.);
#15720=EDGE_CURVE('',#12391,#12392,#6709,.T.);
#15721=EDGE_CURVE('',#12391,#12393,#6710,.T.);
#15722=EDGE_CURVE('',#12394,#12392,#6711,.T.);
#15723=EDGE_CURVE('',#12393,#12394,#6712,.T.);
#15724=EDGE_CURVE('',#12393,#12395,#6713,.T.);
#15725=EDGE_CURVE('',#12396,#12394,#6714,.T.);
#15726=EDGE_CURVE('',#12395,#12396,#6715,.T.);
#15727=EDGE_CURVE('',#12395,#12397,#6716,.T.);
#15728=EDGE_CURVE('',#12398,#12396,#6717,.T.);
#15729=EDGE_CURVE('',#12397,#12398,#6718,.T.);
#15730=EDGE_CURVE('',#12397,#12399,#6719,.T.);
#15731=EDGE_CURVE('',#12400,#12398,#6720,.T.);
#15732=EDGE_CURVE('',#12399,#12400,#6721,.T.);
#15733=EDGE_CURVE('',#12399,#12401,#6722,.T.);
#15734=EDGE_CURVE('',#12402,#12400,#6723,.T.);
#15735=EDGE_CURVE('',#12401,#12402,#6724,.T.);
#15736=EDGE_CURVE('',#12401,#12403,#6725,.T.);
#15737=EDGE_CURVE('',#12404,#12402,#6726,.T.);
#15738=EDGE_CURVE('',#12403,#12404,#6727,.T.);
#15739=EDGE_CURVE('',#12403,#12405,#6728,.T.);
#15740=EDGE_CURVE('',#12406,#12404,#6729,.T.);
#15741=EDGE_CURVE('',#12405,#12406,#6730,.T.);
#15742=EDGE_CURVE('',#12405,#12407,#6731,.T.);
#15743=EDGE_CURVE('',#12408,#12406,#6732,.T.);
#15744=EDGE_CURVE('',#12407,#12408,#6733,.T.);
#15745=EDGE_CURVE('',#12407,#12409,#6734,.T.);
#15746=EDGE_CURVE('',#12410,#12408,#6735,.T.);
#15747=EDGE_CURVE('',#12409,#12410,#6736,.T.);
#15748=EDGE_CURVE('',#12409,#12411,#6737,.T.);
#15749=EDGE_CURVE('',#12412,#12410,#6738,.T.);
#15750=EDGE_CURVE('',#12411,#12412,#6739,.T.);
#15751=EDGE_CURVE('',#12411,#12413,#6740,.T.);
#15752=EDGE_CURVE('',#12414,#12412,#6741,.T.);
#15753=EDGE_CURVE('',#12413,#12414,#6742,.T.);
#15754=EDGE_CURVE('',#12413,#12415,#6743,.T.);
#15755=EDGE_CURVE('',#12416,#12414,#6744,.T.);
#15756=EDGE_CURVE('',#12415,#12416,#6745,.T.);
#15757=EDGE_CURVE('',#12415,#12417,#6746,.T.);
#15758=EDGE_CURVE('',#12418,#12416,#6747,.T.);
#15759=EDGE_CURVE('',#12417,#12418,#6748,.T.);
#15760=EDGE_CURVE('',#12417,#12419,#6749,.T.);
#15761=EDGE_CURVE('',#12420,#12418,#6750,.T.);
#15762=EDGE_CURVE('',#12419,#12420,#6751,.T.);
#15763=EDGE_CURVE('',#12419,#12421,#6752,.T.);
#15764=EDGE_CURVE('',#12422,#12420,#6753,.T.);
#15765=EDGE_CURVE('',#12421,#12422,#6754,.T.);
#15766=EDGE_CURVE('',#12421,#12423,#6755,.T.);
#15767=EDGE_CURVE('',#12424,#12422,#6756,.T.);
#15768=EDGE_CURVE('',#12423,#12424,#6757,.T.);
#15769=EDGE_CURVE('',#12423,#12425,#6758,.T.);
#15770=EDGE_CURVE('',#12426,#12424,#6759,.T.);
#15771=EDGE_CURVE('',#12425,#12426,#6760,.T.);
#15772=EDGE_CURVE('',#12425,#12427,#6761,.T.);
#15773=EDGE_CURVE('',#12428,#12426,#6762,.T.);
#15774=EDGE_CURVE('',#12427,#12428,#6763,.T.);
#15775=EDGE_CURVE('',#12427,#12429,#6764,.T.);
#15776=EDGE_CURVE('',#12430,#12428,#6765,.T.);
#15777=EDGE_CURVE('',#12429,#12430,#6766,.T.);
#15778=EDGE_CURVE('',#12429,#12431,#6767,.T.);
#15779=EDGE_CURVE('',#12432,#12430,#6768,.T.);
#15780=EDGE_CURVE('',#12431,#12432,#6769,.T.);
#15781=EDGE_CURVE('',#12431,#12433,#6770,.T.);
#15782=EDGE_CURVE('',#12434,#12432,#6771,.T.);
#15783=EDGE_CURVE('',#12433,#12434,#6772,.T.);
#15784=EDGE_CURVE('',#12433,#12435,#6773,.T.);
#15785=EDGE_CURVE('',#12436,#12434,#6774,.T.);
#15786=EDGE_CURVE('',#12435,#12436,#6775,.T.);
#15787=EDGE_CURVE('',#12435,#12437,#6776,.T.);
#15788=EDGE_CURVE('',#12438,#12436,#6777,.T.);
#15789=EDGE_CURVE('',#12437,#12438,#6778,.T.);
#15790=EDGE_CURVE('',#12437,#12439,#6779,.T.);
#15791=EDGE_CURVE('',#12440,#12438,#6780,.T.);
#15792=EDGE_CURVE('',#12439,#12440,#6781,.T.);
#15793=EDGE_CURVE('',#12439,#12441,#6782,.T.);
#15794=EDGE_CURVE('',#12442,#12440,#6783,.T.);
#15795=EDGE_CURVE('',#12441,#12442,#6784,.T.);
#15796=EDGE_CURVE('',#12441,#12443,#6785,.T.);
#15797=EDGE_CURVE('',#12444,#12442,#6786,.T.);
#15798=EDGE_CURVE('',#12443,#12444,#6787,.T.);
#15799=EDGE_CURVE('',#12443,#12445,#6788,.T.);
#15800=EDGE_CURVE('',#12446,#12444,#6789,.T.);
#15801=EDGE_CURVE('',#12445,#12446,#6790,.T.);
#15802=EDGE_CURVE('',#12445,#12447,#6791,.T.);
#15803=EDGE_CURVE('',#12448,#12446,#6792,.T.);
#15804=EDGE_CURVE('',#12447,#12448,#6793,.T.);
#15805=EDGE_CURVE('',#12447,#12449,#6794,.T.);
#15806=EDGE_CURVE('',#12450,#12448,#6795,.T.);
#15807=EDGE_CURVE('',#12449,#12450,#6796,.T.);
#15808=EDGE_CURVE('',#12449,#12451,#6797,.T.);
#15809=EDGE_CURVE('',#12452,#12450,#6798,.T.);
#15810=EDGE_CURVE('',#12451,#12452,#6799,.T.);
#15811=EDGE_CURVE('',#12451,#12453,#6800,.T.);
#15812=EDGE_CURVE('',#12454,#12452,#6801,.T.);
#15813=EDGE_CURVE('',#12453,#12454,#6802,.T.);
#15814=EDGE_CURVE('',#12453,#12455,#6803,.T.);
#15815=EDGE_CURVE('',#12456,#12454,#6804,.T.);
#15816=EDGE_CURVE('',#12455,#12456,#6805,.T.);
#15817=EDGE_CURVE('',#12455,#12457,#6806,.T.);
#15818=EDGE_CURVE('',#12458,#12456,#6807,.T.);
#15819=EDGE_CURVE('',#12457,#12458,#6808,.T.);
#15820=EDGE_CURVE('',#12457,#12459,#6809,.T.);
#15821=EDGE_CURVE('',#12460,#12458,#6810,.T.);
#15822=EDGE_CURVE('',#12459,#12460,#6811,.T.);
#15823=EDGE_CURVE('',#12459,#12461,#6812,.T.);
#15824=EDGE_CURVE('',#12462,#12460,#6813,.T.);
#15825=EDGE_CURVE('',#12461,#12462,#6814,.T.);
#15826=EDGE_CURVE('',#12461,#12463,#6815,.T.);
#15827=EDGE_CURVE('',#12464,#12462,#6816,.T.);
#15828=EDGE_CURVE('',#12463,#12464,#6817,.T.);
#15829=EDGE_CURVE('',#12463,#12465,#6818,.T.);
#15830=EDGE_CURVE('',#12466,#12464,#6819,.T.);
#15831=EDGE_CURVE('',#12465,#12466,#6820,.T.);
#15832=EDGE_CURVE('',#12465,#12467,#6821,.T.);
#15833=EDGE_CURVE('',#12468,#12466,#6822,.T.);
#15834=EDGE_CURVE('',#12467,#12468,#6823,.T.);
#15835=EDGE_CURVE('',#12467,#12469,#6824,.T.);
#15836=EDGE_CURVE('',#12470,#12468,#6825,.T.);
#15837=EDGE_CURVE('',#12469,#12470,#6826,.T.);
#15838=EDGE_CURVE('',#12469,#12471,#6827,.T.);
#15839=EDGE_CURVE('',#12472,#12470,#6828,.T.);
#15840=EDGE_CURVE('',#12471,#12472,#6829,.T.);
#15841=EDGE_CURVE('',#12471,#12473,#6830,.T.);
#15842=EDGE_CURVE('',#12474,#12472,#6831,.T.);
#15843=EDGE_CURVE('',#12473,#12474,#6832,.T.);
#15844=EDGE_CURVE('',#12473,#12475,#6833,.T.);
#15845=EDGE_CURVE('',#12476,#12474,#6834,.T.);
#15846=EDGE_CURVE('',#12475,#12476,#6835,.T.);
#15847=EDGE_CURVE('',#12475,#12477,#6836,.T.);
#15848=EDGE_CURVE('',#12478,#12476,#6837,.T.);
#15849=EDGE_CURVE('',#12477,#12478,#6838,.T.);
#15850=EDGE_CURVE('',#12477,#12479,#6839,.T.);
#15851=EDGE_CURVE('',#12480,#12478,#6840,.T.);
#15852=EDGE_CURVE('',#12479,#12480,#6841,.T.);
#15853=EDGE_CURVE('',#12479,#12481,#6842,.T.);
#15854=EDGE_CURVE('',#12482,#12480,#6843,.T.);
#15855=EDGE_CURVE('',#12481,#12482,#6844,.T.);
#15856=EDGE_CURVE('',#12481,#12483,#6845,.T.);
#15857=EDGE_CURVE('',#12484,#12482,#6846,.T.);
#15858=EDGE_CURVE('',#12483,#12484,#6847,.T.);
#15859=EDGE_CURVE('',#12483,#12485,#6848,.T.);
#15860=EDGE_CURVE('',#12486,#12484,#6849,.T.);
#15861=EDGE_CURVE('',#12485,#12486,#6850,.T.);
#15862=EDGE_CURVE('',#12485,#12487,#6851,.T.);
#15863=EDGE_CURVE('',#12488,#12486,#6852,.T.);
#15864=EDGE_CURVE('',#12487,#12488,#6853,.T.);
#15865=EDGE_CURVE('',#12487,#12489,#6854,.T.);
#15866=EDGE_CURVE('',#12490,#12488,#6855,.T.);
#15867=EDGE_CURVE('',#12489,#12490,#6856,.T.);
#15868=EDGE_CURVE('',#12489,#12491,#6857,.T.);
#15869=EDGE_CURVE('',#12492,#12490,#6858,.T.);
#15870=EDGE_CURVE('',#12491,#12492,#6859,.T.);
#15871=EDGE_CURVE('',#12491,#12493,#6860,.T.);
#15872=EDGE_CURVE('',#12494,#12492,#6861,.T.);
#15873=EDGE_CURVE('',#12493,#12494,#6862,.T.);
#15874=EDGE_CURVE('',#12493,#12495,#6863,.T.);
#15875=EDGE_CURVE('',#12496,#12494,#6864,.T.);
#15876=EDGE_CURVE('',#12495,#12496,#6865,.T.);
#15877=EDGE_CURVE('',#12495,#12497,#6866,.T.);
#15878=EDGE_CURVE('',#12498,#12496,#6867,.T.);
#15879=EDGE_CURVE('',#12497,#12498,#6868,.T.);
#15880=EDGE_CURVE('',#12497,#12499,#6869,.T.);
#15881=EDGE_CURVE('',#12500,#12498,#6870,.T.);
#15882=EDGE_CURVE('',#12499,#12500,#6871,.T.);
#15883=EDGE_CURVE('',#12499,#12501,#6872,.T.);
#15884=EDGE_CURVE('',#12502,#12500,#6873,.T.);
#15885=EDGE_CURVE('',#12501,#12502,#6874,.T.);
#15886=EDGE_CURVE('',#12501,#12503,#6875,.T.);
#15887=EDGE_CURVE('',#12504,#12502,#6876,.T.);
#15888=EDGE_CURVE('',#12503,#12504,#6877,.T.);
#15889=EDGE_CURVE('',#12503,#12505,#6878,.T.);
#15890=EDGE_CURVE('',#12506,#12504,#6879,.T.);
#15891=EDGE_CURVE('',#12505,#12506,#6880,.T.);
#15892=EDGE_CURVE('',#12505,#12507,#6881,.T.);
#15893=EDGE_CURVE('',#12508,#12506,#6882,.T.);
#15894=EDGE_CURVE('',#12507,#12508,#6883,.T.);
#15895=EDGE_CURVE('',#12507,#12509,#6884,.T.);
#15896=EDGE_CURVE('',#12510,#12508,#6885,.T.);
#15897=EDGE_CURVE('',#12509,#12510,#6886,.T.);
#15898=EDGE_CURVE('',#12509,#12511,#6887,.T.);
#15899=EDGE_CURVE('',#12512,#12510,#6888,.T.);
#15900=EDGE_CURVE('',#12511,#12512,#6889,.T.);
#15901=EDGE_CURVE('',#12511,#12513,#6890,.T.);
#15902=EDGE_CURVE('',#12514,#12512,#6891,.T.);
#15903=EDGE_CURVE('',#12513,#12514,#6892,.T.);
#15904=EDGE_CURVE('',#12513,#12515,#6893,.T.);
#15905=EDGE_CURVE('',#12516,#12514,#6894,.T.);
#15906=EDGE_CURVE('',#12515,#12516,#6895,.T.);
#15907=EDGE_CURVE('',#12515,#12517,#6896,.T.);
#15908=EDGE_CURVE('',#12518,#12516,#6897,.T.);
#15909=EDGE_CURVE('',#12517,#12518,#6898,.T.);
#15910=EDGE_CURVE('',#12517,#12519,#6899,.T.);
#15911=EDGE_CURVE('',#12520,#12518,#6900,.T.);
#15912=EDGE_CURVE('',#12519,#12520,#6901,.T.);
#15913=EDGE_CURVE('',#12519,#12521,#6902,.T.);
#15914=EDGE_CURVE('',#12522,#12520,#6903,.T.);
#15915=EDGE_CURVE('',#12521,#12522,#6904,.T.);
#15916=EDGE_CURVE('',#12521,#12523,#6905,.T.);
#15917=EDGE_CURVE('',#12524,#12522,#6906,.T.);
#15918=EDGE_CURVE('',#12523,#12524,#6907,.T.);
#15919=EDGE_CURVE('',#12523,#12525,#6908,.T.);
#15920=EDGE_CURVE('',#12526,#12524,#6909,.T.);
#15921=EDGE_CURVE('',#12525,#12526,#6910,.T.);
#15922=EDGE_CURVE('',#12525,#12527,#6911,.T.);
#15923=EDGE_CURVE('',#12528,#12526,#6912,.T.);
#15924=EDGE_CURVE('',#12527,#12528,#6913,.T.);
#15925=EDGE_CURVE('',#12527,#12529,#6914,.T.);
#15926=EDGE_CURVE('',#12530,#12528,#6915,.T.);
#15927=EDGE_CURVE('',#12529,#12530,#6916,.T.);
#15928=EDGE_CURVE('',#12529,#12531,#6917,.T.);
#15929=EDGE_CURVE('',#12532,#12530,#6918,.T.);
#15930=EDGE_CURVE('',#12531,#12532,#6919,.T.);
#15931=EDGE_CURVE('',#12531,#12533,#6920,.T.);
#15932=EDGE_CURVE('',#12534,#12532,#6921,.T.);
#15933=EDGE_CURVE('',#12533,#12534,#6922,.T.);
#15934=EDGE_CURVE('',#12533,#12535,#6923,.T.);
#15935=EDGE_CURVE('',#12536,#12534,#6924,.T.);
#15936=EDGE_CURVE('',#12535,#12536,#6925,.T.);
#15937=EDGE_CURVE('',#12535,#12537,#6926,.T.);
#15938=EDGE_CURVE('',#12538,#12536,#6927,.T.);
#15939=EDGE_CURVE('',#12537,#12538,#6928,.T.);
#15940=EDGE_CURVE('',#12537,#12539,#6929,.T.);
#15941=EDGE_CURVE('',#12540,#12538,#6930,.T.);
#15942=EDGE_CURVE('',#12539,#12540,#6931,.T.);
#15943=EDGE_CURVE('',#12539,#12541,#6932,.T.);
#15944=EDGE_CURVE('',#12542,#12540,#6933,.T.);
#15945=EDGE_CURVE('',#12541,#12542,#6934,.T.);
#15946=EDGE_CURVE('',#12541,#12543,#6935,.T.);
#15947=EDGE_CURVE('',#12544,#12542,#6936,.T.);
#15948=EDGE_CURVE('',#12543,#12544,#6937,.T.);
#15949=EDGE_CURVE('',#12543,#12545,#6938,.T.);
#15950=EDGE_CURVE('',#12546,#12544,#6939,.T.);
#15951=EDGE_CURVE('',#12545,#12546,#6940,.T.);
#15952=EDGE_CURVE('',#12545,#12547,#6941,.T.);
#15953=EDGE_CURVE('',#12548,#12546,#6942,.T.);
#15954=EDGE_CURVE('',#12547,#12548,#6943,.T.);
#15955=EDGE_CURVE('',#12547,#12549,#6944,.T.);
#15956=EDGE_CURVE('',#12550,#12548,#6945,.T.);
#15957=EDGE_CURVE('',#12549,#12550,#6946,.T.);
#15958=EDGE_CURVE('',#12549,#12551,#6947,.T.);
#15959=EDGE_CURVE('',#12552,#12550,#6948,.T.);
#15960=EDGE_CURVE('',#12551,#12552,#6949,.T.);
#15961=EDGE_CURVE('',#12551,#12553,#6950,.T.);
#15962=EDGE_CURVE('',#12554,#12552,#6951,.T.);
#15963=EDGE_CURVE('',#12553,#12554,#6952,.T.);
#15964=EDGE_CURVE('',#12553,#12555,#6953,.T.);
#15965=EDGE_CURVE('',#12556,#12554,#6954,.T.);
#15966=EDGE_CURVE('',#12555,#12556,#6955,.T.);
#15967=EDGE_CURVE('',#12555,#12557,#6956,.T.);
#15968=EDGE_CURVE('',#12558,#12556,#6957,.T.);
#15969=EDGE_CURVE('',#12557,#12558,#6958,.T.);
#15970=EDGE_CURVE('',#12557,#12559,#6959,.T.);
#15971=EDGE_CURVE('',#12560,#12558,#6960,.T.);
#15972=EDGE_CURVE('',#12559,#12560,#6961,.T.);
#15973=EDGE_CURVE('',#12559,#12561,#6962,.T.);
#15974=EDGE_CURVE('',#12562,#12560,#6963,.T.);
#15975=EDGE_CURVE('',#12561,#12562,#6964,.T.);
#15976=EDGE_CURVE('',#12561,#12563,#6965,.T.);
#15977=EDGE_CURVE('',#12564,#12562,#6966,.T.);
#15978=EDGE_CURVE('',#12563,#12564,#6967,.T.);
#15979=EDGE_CURVE('',#12563,#12565,#6968,.T.);
#15980=EDGE_CURVE('',#12566,#12564,#6969,.T.);
#15981=EDGE_CURVE('',#12565,#12566,#6970,.T.);
#15982=EDGE_CURVE('',#12565,#12567,#6971,.T.);
#15983=EDGE_CURVE('',#12568,#12566,#6972,.T.);
#15984=EDGE_CURVE('',#12567,#12568,#6973,.T.);
#15985=EDGE_CURVE('',#12567,#12569,#6974,.T.);
#15986=EDGE_CURVE('',#12570,#12568,#6975,.T.);
#15987=EDGE_CURVE('',#12569,#12570,#6976,.T.);
#15988=EDGE_CURVE('',#12569,#12571,#6977,.T.);
#15989=EDGE_CURVE('',#12572,#12570,#6978,.T.);
#15990=EDGE_CURVE('',#12571,#12572,#6979,.T.);
#15991=EDGE_CURVE('',#12571,#12573,#6980,.T.);
#15992=EDGE_CURVE('',#12574,#12572,#6981,.T.);
#15993=EDGE_CURVE('',#12573,#12574,#6982,.T.);
#15994=EDGE_CURVE('',#12573,#12575,#6983,.T.);
#15995=EDGE_CURVE('',#12576,#12574,#6984,.T.);
#15996=EDGE_CURVE('',#12575,#12576,#6985,.T.);
#15997=EDGE_CURVE('',#12575,#12577,#6986,.T.);
#15998=EDGE_CURVE('',#12578,#12576,#6987,.T.);
#15999=EDGE_CURVE('',#12577,#12578,#6988,.T.);
#16000=EDGE_CURVE('',#12577,#11997,#6989,.T.);
#16001=EDGE_CURVE('',#11990,#12578,#6990,.T.);
#16002=EDGE_CURVE('',#12579,#12579,#10716,.T.);
#16003=EDGE_CURVE('',#12579,#12580,#6991,.T.);
#16004=EDGE_CURVE('',#12580,#12580,#10717,.T.);
#16005=EDGE_CURVE('',#12581,#12582,#6992,.T.);
#16006=EDGE_CURVE('',#12583,#12581,#6993,.T.);
#16007=EDGE_CURVE('',#12584,#12583,#6994,.T.);
#16008=EDGE_CURVE('',#12585,#12584,#6995,.T.);
#16009=EDGE_CURVE('',#12586,#12585,#6996,.T.);
#16010=EDGE_CURVE('',#12587,#12586,#6997,.T.);
#16011=EDGE_CURVE('',#12588,#12587,#6998,.T.);
#16012=EDGE_CURVE('',#12582,#12588,#6999,.T.);
#16013=EDGE_CURVE('',#12589,#12589,#10718,.T.);
#16014=EDGE_CURVE('',#12590,#12590,#10719,.T.);
#16015=EDGE_CURVE('',#12591,#12591,#10720,.T.);
#16016=EDGE_CURVE('',#12592,#12592,#10721,.T.);
#16017=EDGE_CURVE('',#12593,#12594,#7000,.T.);
#16018=EDGE_CURVE('',#12594,#12595,#7001,.T.);
#16019=EDGE_CURVE('',#12595,#12596,#7002,.T.);
#16020=EDGE_CURVE('',#12596,#12597,#7003,.T.);
#16021=EDGE_CURVE('',#12597,#12598,#7004,.T.);
#16022=EDGE_CURVE('',#12598,#12593,#7005,.T.);
#16023=EDGE_CURVE('',#12599,#12600,#7006,.T.);
#16024=EDGE_CURVE('',#12600,#12601,#7007,.T.);
#16025=EDGE_CURVE('',#12601,#12602,#7008,.T.);
#16026=EDGE_CURVE('',#12602,#12603,#7009,.T.);
#16027=EDGE_CURVE('',#12603,#12604,#7010,.T.);
#16028=EDGE_CURVE('',#12604,#12599,#7011,.T.);
#16029=EDGE_CURVE('',#12605,#12605,#10722,.T.);
#16030=EDGE_CURVE('',#12606,#12606,#10723,.T.);
#16031=EDGE_CURVE('',#12607,#12607,#10724,.T.);
#16032=EDGE_CURVE('',#12579,#12608,#7012,.T.);
#16033=EDGE_CURVE('',#12608,#12608,#10725,.T.);
#16034=EDGE_CURVE('',#12609,#12609,#10726,.T.);
#16035=EDGE_CURVE('',#12609,#12589,#7013,.T.);
#16036=EDGE_CURVE('',#12609,#12610,#7014,.T.);
#16037=EDGE_CURVE('',#12610,#12610,#10727,.T.);
#16038=EDGE_CURVE('',#12611,#12611,#10728,.T.);
#16039=EDGE_CURVE('',#12611,#12607,#7015,.T.);
#16040=EDGE_CURVE('',#12611,#12612,#7016,.T.);
#16041=EDGE_CURVE('',#12612,#12612,#10729,.T.);
#16042=EDGE_CURVE('',#12613,#12613,#10730,.T.);
#16043=EDGE_CURVE('',#12613,#12590,#7017,.T.);
#16044=EDGE_CURVE('',#12613,#12614,#7018,.T.);
#16045=EDGE_CURVE('',#12614,#12614,#10731,.T.);
#16046=EDGE_CURVE('',#12615,#12615,#10732,.T.);
#16047=EDGE_CURVE('',#12615,#12606,#7019,.T.);
#16048=EDGE_CURVE('',#12615,#12616,#7020,.T.);
#16049=EDGE_CURVE('',#12616,#12616,#10733,.T.);
#16050=EDGE_CURVE('',#12617,#12617,#10734,.T.);
#16051=EDGE_CURVE('',#12617,#12591,#7021,.T.);
#16052=EDGE_CURVE('',#12617,#12618,#7022,.T.);
#16053=EDGE_CURVE('',#12618,#12618,#10735,.T.);
#16054=EDGE_CURVE('',#12619,#12619,#10736,.T.);
#16055=EDGE_CURVE('',#12619,#12605,#7023,.T.);
#16056=EDGE_CURVE('',#12619,#12620,#7024,.T.);
#16057=EDGE_CURVE('',#12620,#12620,#10737,.T.);
#16058=EDGE_CURVE('',#12621,#12621,#10738,.T.);
#16059=EDGE_CURVE('',#12621,#12592,#7025,.T.);
#16060=EDGE_CURVE('',#12621,#12622,#7026,.T.);
#16061=EDGE_CURVE('',#12622,#12622,#10739,.T.);
#16062=EDGE_CURVE('',#12623,#12624,#7027,.T.);
#16063=EDGE_CURVE('',#12623,#12600,#7028,.T.);
#16064=EDGE_CURVE('',#12624,#12599,#7029,.T.);
#16065=EDGE_CURVE('',#12625,#12623,#7030,.T.);
#16066=EDGE_CURVE('',#12625,#12601,#7031,.T.);
#16067=EDGE_CURVE('',#12626,#12625,#7032,.T.);
#16068=EDGE_CURVE('',#12626,#12602,#7033,.T.);
#16069=EDGE_CURVE('',#12627,#12626,#7034,.T.);
#16070=EDGE_CURVE('',#12627,#12603,#7035,.T.);
#16071=EDGE_CURVE('',#12628,#12627,#7036,.T.);
#16072=EDGE_CURVE('',#12628,#12604,#7037,.T.);
#16073=EDGE_CURVE('',#12624,#12628,#7038,.T.);
#16074=EDGE_CURVE('',#12629,#12630,#7039,.T.);
#16075=EDGE_CURVE('',#12629,#12594,#7040,.T.);
#16076=EDGE_CURVE('',#12630,#12593,#7041,.T.);
#16077=EDGE_CURVE('',#12631,#12629,#7042,.T.);
#16078=EDGE_CURVE('',#12631,#12595,#7043,.T.);
#16079=EDGE_CURVE('',#12632,#12631,#7044,.T.);
#16080=EDGE_CURVE('',#12632,#12596,#7045,.T.);
#16081=EDGE_CURVE('',#12633,#12632,#7046,.T.);
#16082=EDGE_CURVE('',#12633,#12597,#7047,.T.);
#16083=EDGE_CURVE('',#12634,#12633,#7048,.T.);
#16084=EDGE_CURVE('',#12634,#12598,#7049,.T.);
#16085=EDGE_CURVE('',#12630,#12634,#7050,.T.);
#16086=EDGE_CURVE('',#12582,#12635,#7051,.T.);
#16087=EDGE_CURVE('',#12635,#12636,#7052,.T.);
#16088=EDGE_CURVE('',#12581,#12636,#7053,.T.);
#16089=EDGE_CURVE('',#12588,#12637,#7054,.T.);
#16090=EDGE_CURVE('',#12637,#12635,#7055,.T.);
#16091=EDGE_CURVE('',#12587,#12638,#7056,.T.);
#16092=EDGE_CURVE('',#12638,#12637,#7057,.T.);
#16093=EDGE_CURVE('',#12586,#12639,#7058,.T.);
#16094=EDGE_CURVE('',#12639,#12638,#7059,.T.);
#16095=EDGE_CURVE('',#12585,#12640,#7060,.T.);
#16096=EDGE_CURVE('',#12640,#12639,#7061,.T.);
#16097=EDGE_CURVE('',#12641,#12640,#7062,.T.);
#16098=EDGE_CURVE('',#12584,#12641,#7063,.T.);
#16099=EDGE_CURVE('',#12642,#12641,#7064,.T.);
#16100=EDGE_CURVE('',#12583,#12642,#7065,.T.);
#16101=EDGE_CURVE('',#12636,#12642,#7066,.T.);
#16102=EDGE_CURVE('',#12643,#12641,#7067,.T.);
#16103=EDGE_CURVE('',#12644,#12643,#7068,.T.);
#16104=EDGE_CURVE('',#12644,#12640,#7069,.T.);
#16105=EDGE_CURVE('',#12645,#12642,#7070,.T.);
#16106=EDGE_CURVE('',#12643,#12645,#7071,.T.);
#16107=EDGE_CURVE('',#12646,#12636,#7072,.T.);
#16108=EDGE_CURVE('',#12645,#12646,#7073,.T.);
#16109=EDGE_CURVE('',#12647,#12635,#7074,.T.);
#16110=EDGE_CURVE('',#12646,#12647,#7075,.T.);
#16111=EDGE_CURVE('',#12648,#12644,#7076,.T.);
#16112=EDGE_CURVE('',#12648,#12639,#7077,.T.);
#16113=EDGE_CURVE('',#12649,#12637,#7078,.T.);
#16114=EDGE_CURVE('',#12647,#12649,#7079,.T.);
#16115=EDGE_CURVE('',#12650,#12638,#7080,.T.);
#16116=EDGE_CURVE('',#12649,#12650,#7081,.T.);
#16117=EDGE_CURVE('',#12650,#12648,#7082,.T.);
#16118=EDGE_CURVE('',#12651,#12651,#10740,.T.);
#16119=EDGE_CURVE('',#12651,#12652,#7083,.T.);
#16120=EDGE_CURVE('',#12652,#12652,#10741,.T.);
#16121=EDGE_CURVE('',#12653,#12653,#10742,.T.);
#16122=EDGE_CURVE('',#12653,#12654,#7084,.T.);
#16123=EDGE_CURVE('',#12654,#12654,#10743,.T.);
#16124=EDGE_CURVE('',#12655,#12655,#10744,.T.);
#16125=EDGE_CURVE('',#12655,#12656,#7085,.T.);
#16126=EDGE_CURVE('',#12656,#12656,#10745,.T.);
#16127=EDGE_CURVE('',#12655,#12657,#7086,.T.);
#16128=EDGE_CURVE('',#12658,#12657,#191,.T.);
#16129=EDGE_CURVE('',#12658,#12659,#10746,.T.);
#16130=EDGE_CURVE('',#12660,#12659,#192,.T.);
#16131=EDGE_CURVE('',#12660,#12661,#10747,.T.);
#16132=EDGE_CURVE('',#12657,#12661,#193,.T.);
#16133=EDGE_CURVE('',#12662,#12663,#7087,.T.);
#16134=EDGE_CURVE('',#12663,#12664,#7088,.T.);
#16135=EDGE_CURVE('',#12665,#12664,#7089,.T.);
#16136=EDGE_CURVE('',#12662,#12665,#7090,.T.);
#16137=EDGE_CURVE('',#12666,#12666,#10748,.T.);
#16138=EDGE_CURVE('',#12666,#12667,#7091,.T.);
#16139=EDGE_CURVE('',#12667,#12667,#10749,.T.);
#16140=EDGE_CURVE('',#12666,#12668,#7092,.T.);
#16141=EDGE_CURVE('',#12669,#12668,#194,.T.);
#16142=EDGE_CURVE('',#12669,#12670,#10750,.T.);
#16143=EDGE_CURVE('',#12671,#12670,#195,.T.);
#16144=EDGE_CURVE('',#12671,#12672,#10751,.T.);
#16145=EDGE_CURVE('',#12668,#12672,#196,.T.);
#16146=EDGE_CURVE('',#12673,#12674,#7093,.T.);
#16147=EDGE_CURVE('',#12674,#12675,#7094,.T.);
#16148=EDGE_CURVE('',#12676,#12675,#7095,.T.);
#16149=EDGE_CURVE('',#12673,#12676,#7096,.T.);
#16150=EDGE_CURVE('',#12659,#12658,#641,.T.);
#16151=EDGE_CURVE('',#12661,#12660,#642,.T.);
#16152=EDGE_CURVE('',#12677,#12677,#10752,.T.);
#16153=EDGE_CURVE('',#12677,#12678,#7097,.T.);
#16154=EDGE_CURVE('',#12678,#12679,#10753,.T.);
#16155=EDGE_CURVE('',#12679,#12678,#10754,.T.);
#16156=EDGE_CURVE('',#12672,#12671,#643,.T.);
#16157=EDGE_CURVE('',#12670,#12669,#644,.T.);
#16158=EDGE_CURVE('',#12680,#12680,#10755,.T.);
#16159=EDGE_CURVE('',#12680,#12681,#7098,.T.);
#16160=EDGE_CURVE('',#12681,#12682,#10756,.T.);
#16161=EDGE_CURVE('',#12682,#12681,#10757,.T.);
#16162=EDGE_CURVE('',#12677,#12683,#7099,.T.);
#16163=EDGE_CURVE('',#12683,#12683,#10758,.T.);
#16164=EDGE_CURVE('',#12684,#12685,#7100,.T.);
#16165=EDGE_CURVE('',#12686,#12684,#7101,.T.);
#16166=EDGE_CURVE('',#12687,#12686,#7102,.T.);
#16167=EDGE_CURVE('',#12687,#12662,#7103,.T.);
#16168=EDGE_CURVE('',#12685,#12665,#7104,.T.);
#16169=EDGE_CURVE('',#12688,#12679,#7105,.T.);
#16170=EDGE_CURVE('',#12680,#12689,#7106,.T.);
#16171=EDGE_CURVE('',#12689,#12689,#10759,.T.);
#16172=EDGE_CURVE('',#12690,#12691,#7107,.T.);
#16173=EDGE_CURVE('',#12675,#12690,#7108,.T.);
#16174=EDGE_CURVE('',#12674,#12692,#7109,.T.);
#16175=EDGE_CURVE('',#12693,#12692,#7110,.T.);
#16176=EDGE_CURVE('',#12693,#12691,#7111,.T.);
#16177=EDGE_CURVE('',#12694,#12682,#7112,.T.);
#16178=EDGE_CURVE('',#12685,#12690,#7113,.T.);
#16179=EDGE_CURVE('',#12691,#12684,#7114,.T.);
#16180=EDGE_CURVE('',#12686,#12693,#7115,.T.);
#16181=EDGE_CURVE('',#12692,#12687,#7116,.T.);
#16182=EDGE_CURVE('',#12695,#12673,#7117,.T.);
#16183=EDGE_CURVE('',#12696,#12676,#7118,.T.);
#16184=EDGE_CURVE('',#12695,#12696,#7119,.T.);
#16185=EDGE_CURVE('',#12697,#12695,#7120,.T.);
#16186=EDGE_CURVE('',#12698,#12696,#7121,.T.);
#16187=EDGE_CURVE('',#12697,#12698,#7122,.T.);
#16188=EDGE_CURVE('',#12663,#12697,#7123,.T.);
#16189=EDGE_CURVE('',#12664,#12698,#7124,.T.);
#16190=EDGE_CURVE('',#12699,#12700,#7125,.T.);
#16191=EDGE_CURVE('',#12701,#12699,#645,.F.);
#16192=EDGE_CURVE('',#12702,#12701,#10760,.T.);
#16193=EDGE_CURVE('',#12702,#12700,#646,.T.);
#16194=EDGE_CURVE('',#12703,#12704,#7126,.T.);
#16195=EDGE_CURVE('',#12699,#12703,#647,.F.);
#16196=EDGE_CURVE('',#12700,#12704,#648,.T.);
#16197=EDGE_CURVE('',#12705,#12706,#7127,.T.);
#16198=EDGE_CURVE('',#12707,#12705,#649,.F.);
#16199=EDGE_CURVE('',#12703,#12707,#650,.F.);
#16200=EDGE_CURVE('',#12704,#12708,#651,.T.);
#16201=EDGE_CURVE('',#12708,#12706,#652,.T.);
#16202=EDGE_CURVE('',#12709,#12710,#7128,.T.);
#16203=EDGE_CURVE('',#12705,#12709,#653,.F.);
#16204=EDGE_CURVE('',#12706,#12710,#654,.T.);
#16205=EDGE_CURVE('',#12711,#12712,#7129,.T.);
#16206=EDGE_CURVE('',#12713,#12711,#655,.F.);
#16207=EDGE_CURVE('',#12709,#12713,#656,.F.);
#16208=EDGE_CURVE('',#12710,#12714,#657,.T.);
#16209=EDGE_CURVE('',#12714,#12712,#658,.T.);
#16210=EDGE_CURVE('',#12715,#12716,#7130,.T.);
#16211=EDGE_CURVE('',#12711,#12715,#659,.F.);
#16212=EDGE_CURVE('',#12712,#12716,#660,.T.);
#16213=EDGE_CURVE('',#12717,#12718,#7131,.T.);
#16214=EDGE_CURVE('',#12719,#12717,#661,.F.);
#16215=EDGE_CURVE('',#12715,#12719,#662,.F.);
#16216=EDGE_CURVE('',#12716,#12720,#663,.T.);
#16217=EDGE_CURVE('',#12720,#12718,#664,.F.);
#16218=EDGE_CURVE('',#12721,#12722,#665,.T.);
#16219=EDGE_CURVE('',#12723,#12722,#10761,.T.);
#16220=EDGE_CURVE('',#12723,#12724,#666,.T.);
#16221=EDGE_CURVE('',#12724,#12725,#667,.T.);
#16222=EDGE_CURVE('',#12725,#12726,#668,.T.);
#16223=EDGE_CURVE('',#12726,#12727,#669,.T.);
#16224=EDGE_CURVE('',#12727,#12728,#670,.T.);
#16225=EDGE_CURVE('',#12728,#12729,#671,.T.);
#16226=EDGE_CURVE('',#12729,#12730,#672,.T.);
#16227=EDGE_CURVE('',#12730,#12731,#673,.T.);
#16228=EDGE_CURVE('',#12731,#12732,#674,.T.);
#16229=EDGE_CURVE('',#12733,#12732,#10762,.T.);
#16230=EDGE_CURVE('',#12733,#12734,#675,.T.);
#16231=EDGE_CURVE('',#12734,#12735,#676,.T.);
#16232=EDGE_CURVE('',#12735,#12736,#677,.T.);
#16233=EDGE_CURVE('',#12736,#12737,#678,.T.);
#16234=EDGE_CURVE('',#12737,#12738,#679,.T.);
#16235=EDGE_CURVE('',#12738,#12739,#680,.T.);
#16236=EDGE_CURVE('',#12739,#12740,#681,.T.);
#16237=EDGE_CURVE('',#12740,#12721,#682,.T.);
#16238=EDGE_CURVE('',#12718,#12741,#683,.F.);
#16239=EDGE_CURVE('',#12742,#12741,#10763,.T.);
#16240=EDGE_CURVE('',#12717,#12742,#684,.F.);
#16241=EDGE_CURVE('',#12743,#12744,#10764,.T.);
#16242=EDGE_CURVE('',#12743,#12742,#685,.T.);
#16243=EDGE_CURVE('',#12741,#12745,#686,.T.);
#16244=EDGE_CURVE('',#12745,#12733,#687,.T.);
#16245=EDGE_CURVE('',#12744,#12733,#10765,.T.);
#16246=EDGE_CURVE('',#12732,#12743,#688,.T.);
#16247=EDGE_CURVE('',#12746,#12723,#689,.T.);
#16248=EDGE_CURVE('',#12746,#12701,#690,.T.);
#16249=EDGE_CURVE('',#12747,#12748,#10766,.T.);
#16250=EDGE_CURVE('',#12747,#12702,#691,.T.);
#16251=EDGE_CURVE('',#12748,#12723,#10767,.T.);
#16252=EDGE_CURVE('',#12722,#12747,#692,.T.);
#16253=EDGE_CURVE('',#12749,#12749,#10768,.T.);
#16254=EDGE_CURVE('',#12749,#12748,#10769,.T.);
#16255=EDGE_CURVE('',#12750,#12750,#10770,.T.);
#16256=EDGE_CURVE('',#12744,#12751,#7132,.T.);
#16257=EDGE_CURVE('',#12751,#12751,#10771,.T.);
#16258=EDGE_CURVE('',#12752,#12753,#7133,.T.);
#16259=EDGE_CURVE('',#12752,#12754,#7134,.T.);
#16260=EDGE_CURVE('',#12755,#12754,#7135,.T.);
#16261=EDGE_CURVE('',#12753,#12755,#281,.T.);
#16262=EDGE_CURVE('',#12756,#12757,#7136,.T.);
#16263=EDGE_CURVE('',#12755,#12756,#282,.T.);
#16264=EDGE_CURVE('',#12754,#12757,#7137,.T.);
#16265=EDGE_CURVE('',#12757,#12752,#10772,.T.);
#16266=EDGE_CURVE('',#12758,#12759,#283,.T.);
#16267=EDGE_CURVE('',#12759,#12760,#10773,.T.);
#16268=EDGE_CURVE('',#12760,#12761,#284,.T.);
#16269=EDGE_CURVE('',#12761,#12762,#285,.T.);
#16270=EDGE_CURVE('',#12762,#12763,#10774,.T.);
#16271=EDGE_CURVE('',#12763,#12764,#286,.T.);
#16272=EDGE_CURVE('',#12764,#12765,#287,.T.);
#16273=EDGE_CURVE('',#12765,#12766,#10775,.T.);
#16274=EDGE_CURVE('',#12766,#12767,#288,.T.);
#16275=EDGE_CURVE('',#12767,#12768,#289,.T.);
#16276=EDGE_CURVE('',#12768,#12769,#10776,.T.);
#16277=EDGE_CURVE('',#12769,#12770,#290,.T.);
#16278=EDGE_CURVE('',#12770,#12771,#291,.T.);
#16279=EDGE_CURVE('',#12771,#12772,#10777,.T.);
#16280=EDGE_CURVE('',#12772,#12773,#292,.T.);
#16281=EDGE_CURVE('',#12773,#12774,#293,.T.);
#16282=EDGE_CURVE('',#12774,#12775,#10778,.T.);
#16283=EDGE_CURVE('',#12775,#12776,#294,.T.);
#16284=EDGE_CURVE('',#12776,#12777,#295,.T.);
#16285=EDGE_CURVE('',#12777,#12778,#10779,.T.);
#16286=EDGE_CURVE('',#12778,#12779,#296,.T.);
#16287=EDGE_CURVE('',#12779,#12780,#297,.T.);
#16288=EDGE_CURVE('',#12780,#12781,#10780,.T.);
#16289=EDGE_CURVE('',#12781,#12782,#298,.T.);
#16290=EDGE_CURVE('',#12782,#12783,#299,.T.);
#16291=EDGE_CURVE('',#12783,#12784,#10781,.T.);
#16292=EDGE_CURVE('',#12784,#12785,#300,.T.);
#16293=EDGE_CURVE('',#12785,#12786,#301,.T.);
#16294=EDGE_CURVE('',#12786,#12787,#10782,.T.);
#16295=EDGE_CURVE('',#12787,#12788,#302,.T.);
#16296=EDGE_CURVE('',#12788,#12789,#303,.T.);
#16297=EDGE_CURVE('',#12789,#12790,#10783,.T.);
#16298=EDGE_CURVE('',#12790,#12791,#304,.T.);
#16299=EDGE_CURVE('',#12791,#12792,#305,.T.);
#16300=EDGE_CURVE('',#12792,#12793,#10784,.T.);
#16301=EDGE_CURVE('',#12793,#12794,#306,.T.);
#16302=EDGE_CURVE('',#12794,#12795,#307,.T.);
#16303=EDGE_CURVE('',#12795,#12796,#10785,.T.);
#16304=EDGE_CURVE('',#12796,#12797,#308,.T.);
#16305=EDGE_CURVE('',#12797,#12798,#309,.T.);
#16306=EDGE_CURVE('',#12798,#12799,#10786,.T.);
#16307=EDGE_CURVE('',#12799,#12800,#310,.T.);
#16308=EDGE_CURVE('',#12800,#12801,#311,.T.);
#16309=EDGE_CURVE('',#12801,#12802,#10787,.T.);
#16310=EDGE_CURVE('',#12802,#12803,#312,.T.);
#16311=EDGE_CURVE('',#12803,#12804,#313,.T.);
#16312=EDGE_CURVE('',#12804,#12805,#10788,.T.);
#16313=EDGE_CURVE('',#12805,#12806,#314,.T.);
#16314=EDGE_CURVE('',#12806,#12807,#315,.T.);
#16315=EDGE_CURVE('',#12807,#12808,#10789,.T.);
#16316=EDGE_CURVE('',#12808,#12809,#316,.T.);
#16317=EDGE_CURVE('',#12809,#12810,#317,.T.);
#16318=EDGE_CURVE('',#12810,#12811,#10790,.T.);
#16319=EDGE_CURVE('',#12811,#12812,#318,.T.);
#16320=EDGE_CURVE('',#12812,#12813,#319,.T.);
#16321=EDGE_CURVE('',#12813,#12814,#10791,.T.);
#16322=EDGE_CURVE('',#12814,#12815,#320,.T.);
#16323=EDGE_CURVE('',#12815,#12816,#321,.T.);
#16324=EDGE_CURVE('',#12816,#12817,#10792,.T.);
#16325=EDGE_CURVE('',#12817,#12818,#322,.T.);
#16326=EDGE_CURVE('',#12818,#12819,#323,.T.);
#16327=EDGE_CURVE('',#12819,#12820,#10793,.T.);
#16328=EDGE_CURVE('',#12820,#12821,#324,.T.);
#16329=EDGE_CURVE('',#12821,#12822,#325,.T.);
#16330=EDGE_CURVE('',#12822,#12823,#10794,.T.);
#16331=EDGE_CURVE('',#12823,#12824,#326,.T.);
#16332=EDGE_CURVE('',#12824,#12825,#327,.T.);
#16333=EDGE_CURVE('',#12825,#12826,#10795,.T.);
#16334=EDGE_CURVE('',#12826,#12827,#328,.T.);
#16335=EDGE_CURVE('',#12827,#12828,#329,.T.);
#16336=EDGE_CURVE('',#12828,#12829,#10796,.T.);
#16337=EDGE_CURVE('',#12829,#12830,#330,.T.);
#16338=EDGE_CURVE('',#12830,#12831,#331,.T.);
#16339=EDGE_CURVE('',#12831,#12832,#10797,.T.);
#16340=EDGE_CURVE('',#12832,#12833,#332,.T.);
#16341=EDGE_CURVE('',#12833,#12834,#333,.T.);
#16342=EDGE_CURVE('',#12834,#12835,#10798,.T.);
#16343=EDGE_CURVE('',#12835,#12836,#334,.T.);
#16344=EDGE_CURVE('',#12836,#12837,#335,.T.);
#16345=EDGE_CURVE('',#12837,#12838,#10799,.T.);
#16346=EDGE_CURVE('',#12838,#12839,#336,.T.);
#16347=EDGE_CURVE('',#12839,#12840,#337,.T.);
#16348=EDGE_CURVE('',#12840,#12753,#10800,.T.);
#16349=EDGE_CURVE('',#12756,#12841,#10801,.T.);
#16350=EDGE_CURVE('',#12841,#12842,#338,.T.);
#16351=EDGE_CURVE('',#12842,#12843,#339,.T.);
#16352=EDGE_CURVE('',#12843,#12844,#10802,.T.);
#16353=EDGE_CURVE('',#12844,#12845,#340,.T.);
#16354=EDGE_CURVE('',#12845,#12846,#341,.T.);
#16355=EDGE_CURVE('',#12846,#12847,#10803,.T.);
#16356=EDGE_CURVE('',#12847,#12848,#342,.T.);
#16357=EDGE_CURVE('',#12848,#12849,#343,.T.);
#16358=EDGE_CURVE('',#12849,#12850,#10804,.T.);
#16359=EDGE_CURVE('',#12850,#12851,#344,.T.);
#16360=EDGE_CURVE('',#12851,#12852,#345,.T.);
#16361=EDGE_CURVE('',#12852,#12853,#10805,.T.);
#16362=EDGE_CURVE('',#12853,#12854,#346,.T.);
#16363=EDGE_CURVE('',#12854,#12855,#347,.T.);
#16364=EDGE_CURVE('',#12855,#12856,#10806,.T.);
#16365=EDGE_CURVE('',#12856,#12857,#348,.T.);
#16366=EDGE_CURVE('',#12857,#12858,#349,.T.);
#16367=EDGE_CURVE('',#12858,#12859,#10807,.T.);
#16368=EDGE_CURVE('',#12859,#12860,#350,.T.);
#16369=EDGE_CURVE('',#12860,#12861,#351,.T.);
#16370=EDGE_CURVE('',#12861,#12862,#10808,.T.);
#16371=EDGE_CURVE('',#12862,#12758,#352,.T.);
#16372=EDGE_CURVE('',#12758,#12863,#7138,.T.);
#16373=EDGE_CURVE('',#12863,#12863,#10809,.T.);
#16374=EDGE_CURVE('',#12864,#12841,#7139,.T.);
#16375=EDGE_CURVE('',#12864,#12865,#7140,.T.);
#16376=EDGE_CURVE('',#12842,#12865,#7141,.T.);
#16377=EDGE_CURVE('',#12843,#12866,#7142,.T.);
#16378=EDGE_CURVE('',#12865,#12866,#7143,.T.);
#16379=EDGE_CURVE('',#12866,#12864,#10810,.T.);
#16380=EDGE_CURVE('',#12867,#12844,#7144,.T.);
#16381=EDGE_CURVE('',#12867,#12868,#7145,.T.);
#16382=EDGE_CURVE('',#12845,#12868,#7146,.T.);
#16383=EDGE_CURVE('',#12846,#12869,#7147,.T.);
#16384=EDGE_CURVE('',#12868,#12869,#7148,.T.);
#16385=EDGE_CURVE('',#12869,#12867,#10811,.T.);
#16386=EDGE_CURVE('',#12870,#12847,#7149,.T.);
#16387=EDGE_CURVE('',#12870,#12871,#7150,.T.);
#16388=EDGE_CURVE('',#12848,#12871,#7151,.T.);
#16389=EDGE_CURVE('',#12849,#12872,#7152,.T.);
#16390=EDGE_CURVE('',#12871,#12872,#7153,.T.);
#16391=EDGE_CURVE('',#12872,#12870,#10812,.T.);
#16392=EDGE_CURVE('',#12873,#12850,#7154,.T.);
#16393=EDGE_CURVE('',#12873,#12874,#7155,.T.);
#16394=EDGE_CURVE('',#12851,#12874,#7156,.T.);
#16395=EDGE_CURVE('',#12852,#12875,#7157,.T.);
#16396=EDGE_CURVE('',#12874,#12875,#7158,.T.);
#16397=EDGE_CURVE('',#12875,#12873,#10813,.T.);
#16398=EDGE_CURVE('',#12876,#12853,#7159,.T.);
#16399=EDGE_CURVE('',#12876,#12877,#7160,.T.);
#16400=EDGE_CURVE('',#12854,#12877,#7161,.T.);
#16401=EDGE_CURVE('',#12855,#12878,#7162,.T.);
#16402=EDGE_CURVE('',#12877,#12878,#7163,.T.);
#16403=EDGE_CURVE('',#12878,#12876,#10814,.T.);
#16404=EDGE_CURVE('',#12879,#12856,#7164,.T.);
#16405=EDGE_CURVE('',#12879,#12880,#7165,.T.);
#16406=EDGE_CURVE('',#12857,#12880,#7166,.T.);
#16407=EDGE_CURVE('',#12858,#12881,#7167,.T.);
#16408=EDGE_CURVE('',#12880,#12881,#7168,.T.);
#16409=EDGE_CURVE('',#12881,#12879,#10815,.T.);
#16410=EDGE_CURVE('',#12882,#12859,#7169,.T.);
#16411=EDGE_CURVE('',#12882,#12883,#7170,.T.);
#16412=EDGE_CURVE('',#12860,#12883,#7171,.T.);
#16413=EDGE_CURVE('',#12861,#12884,#7172,.T.);
#16414=EDGE_CURVE('',#12883,#12884,#7173,.T.);
#16415=EDGE_CURVE('',#12884,#12882,#10816,.T.);
#16416=EDGE_CURVE('',#12885,#12862,#7174,.T.);
#16417=EDGE_CURVE('',#12885,#12886,#7175,.T.);
#16418=EDGE_CURVE('',#12758,#12886,#7176,.T.);
#16419=EDGE_CURVE('',#12759,#12887,#7177,.T.);
#16420=EDGE_CURVE('',#12886,#12887,#7178,.T.);
#16421=EDGE_CURVE('',#12887,#12888,#10817,.T.);
#16422=EDGE_CURVE('',#12888,#12885,#10818,.T.);
#16423=EDGE_CURVE('',#12889,#12760,#7179,.T.);
#16424=EDGE_CURVE('',#12889,#12890,#7180,.T.);
#16425=EDGE_CURVE('',#12761,#12890,#7181,.T.);
#16426=EDGE_CURVE('',#12762,#12891,#7182,.T.);
#16427=EDGE_CURVE('',#12890,#12891,#7183,.T.);
#16428=EDGE_CURVE('',#12891,#12889,#10819,.T.);
#16429=EDGE_CURVE('',#12892,#12763,#7184,.T.);
#16430=EDGE_CURVE('',#12892,#12893,#7185,.T.);
#16431=EDGE_CURVE('',#12764,#12893,#7186,.T.);
#16432=EDGE_CURVE('',#12765,#12894,#7187,.T.);
#16433=EDGE_CURVE('',#12893,#12894,#7188,.T.);
#16434=EDGE_CURVE('',#12894,#12892,#10820,.T.);
#16435=EDGE_CURVE('',#12895,#12766,#7189,.T.);
#16436=EDGE_CURVE('',#12895,#12896,#7190,.T.);
#16437=EDGE_CURVE('',#12767,#12896,#7191,.T.);
#16438=EDGE_CURVE('',#12768,#12897,#7192,.T.);
#16439=EDGE_CURVE('',#12896,#12897,#7193,.T.);
#16440=EDGE_CURVE('',#12897,#12895,#10821,.T.);
#16441=EDGE_CURVE('',#12898,#12769,#7194,.T.);
#16442=EDGE_CURVE('',#12898,#12899,#7195,.T.);
#16443=EDGE_CURVE('',#12770,#12899,#7196,.T.);
#16444=EDGE_CURVE('',#12771,#12900,#7197,.T.);
#16445=EDGE_CURVE('',#12899,#12900,#7198,.T.);
#16446=EDGE_CURVE('',#12900,#12898,#10822,.T.);
#16447=EDGE_CURVE('',#12901,#12772,#7199,.T.);
#16448=EDGE_CURVE('',#12901,#12902,#7200,.T.);
#16449=EDGE_CURVE('',#12773,#12902,#7201,.T.);
#16450=EDGE_CURVE('',#12774,#12903,#7202,.T.);
#16451=EDGE_CURVE('',#12902,#12903,#7203,.T.);
#16452=EDGE_CURVE('',#12903,#12901,#10823,.T.);
#16453=EDGE_CURVE('',#12904,#12775,#7204,.T.);
#16454=EDGE_CURVE('',#12904,#12905,#7205,.T.);
#16455=EDGE_CURVE('',#12776,#12905,#7206,.T.);
#16456=EDGE_CURVE('',#12777,#12906,#7207,.T.);
#16457=EDGE_CURVE('',#12905,#12906,#7208,.T.);
#16458=EDGE_CURVE('',#12906,#12904,#10824,.T.);
#16459=EDGE_CURVE('',#12907,#12778,#7209,.T.);
#16460=EDGE_CURVE('',#12907,#12908,#7210,.T.);
#16461=EDGE_CURVE('',#12779,#12908,#7211,.T.);
#16462=EDGE_CURVE('',#12780,#12909,#7212,.T.);
#16463=EDGE_CURVE('',#12908,#12909,#7213,.T.);
#16464=EDGE_CURVE('',#12909,#12907,#10825,.T.);
#16465=EDGE_CURVE('',#12910,#12781,#7214,.T.);
#16466=EDGE_CURVE('',#12910,#12911,#7215,.T.);
#16467=EDGE_CURVE('',#12782,#12911,#7216,.T.);
#16468=EDGE_CURVE('',#12783,#12912,#7217,.T.);
#16469=EDGE_CURVE('',#12911,#12912,#7218,.T.);
#16470=EDGE_CURVE('',#12912,#12910,#10826,.T.);
#16471=EDGE_CURVE('',#12913,#12784,#7219,.T.);
#16472=EDGE_CURVE('',#12913,#12914,#7220,.T.);
#16473=EDGE_CURVE('',#12785,#12914,#7221,.T.);
#16474=EDGE_CURVE('',#12786,#12915,#7222,.T.);
#16475=EDGE_CURVE('',#12914,#12915,#7223,.T.);
#16476=EDGE_CURVE('',#12915,#12913,#10827,.T.);
#16477=EDGE_CURVE('',#12916,#12787,#7224,.T.);
#16478=EDGE_CURVE('',#12916,#12917,#7225,.T.);
#16479=EDGE_CURVE('',#12788,#12917,#7226,.T.);
#16480=EDGE_CURVE('',#12789,#12918,#7227,.T.);
#16481=EDGE_CURVE('',#12917,#12918,#7228,.T.);
#16482=EDGE_CURVE('',#12918,#12916,#10828,.T.);
#16483=EDGE_CURVE('',#12919,#12790,#7229,.T.);
#16484=EDGE_CURVE('',#12919,#12920,#7230,.T.);
#16485=EDGE_CURVE('',#12791,#12920,#7231,.T.);
#16486=EDGE_CURVE('',#12792,#12921,#7232,.T.);
#16487=EDGE_CURVE('',#12920,#12921,#7233,.T.);
#16488=EDGE_CURVE('',#12921,#12919,#10829,.T.);
#16489=EDGE_CURVE('',#12922,#12793,#7234,.T.);
#16490=EDGE_CURVE('',#12922,#12923,#7235,.T.);
#16491=EDGE_CURVE('',#12794,#12923,#7236,.T.);
#16492=EDGE_CURVE('',#12795,#12924,#7237,.T.);
#16493=EDGE_CURVE('',#12923,#12924,#7238,.T.);
#16494=EDGE_CURVE('',#12924,#12922,#10830,.T.);
#16495=EDGE_CURVE('',#12925,#12796,#7239,.T.);
#16496=EDGE_CURVE('',#12925,#12926,#7240,.T.);
#16497=EDGE_CURVE('',#12797,#12926,#7241,.T.);
#16498=EDGE_CURVE('',#12798,#12927,#7242,.T.);
#16499=EDGE_CURVE('',#12926,#12927,#7243,.T.);
#16500=EDGE_CURVE('',#12927,#12925,#10831,.T.);
#16501=EDGE_CURVE('',#12928,#12799,#7244,.T.);
#16502=EDGE_CURVE('',#12928,#12929,#7245,.T.);
#16503=EDGE_CURVE('',#12800,#12929,#7246,.T.);
#16504=EDGE_CURVE('',#12801,#12930,#7247,.T.);
#16505=EDGE_CURVE('',#12929,#12930,#7248,.T.);
#16506=EDGE_CURVE('',#12930,#12928,#10832,.T.);
#16507=EDGE_CURVE('',#12931,#12802,#7249,.T.);
#16508=EDGE_CURVE('',#12931,#12932,#7250,.T.);
#16509=EDGE_CURVE('',#12803,#12932,#7251,.T.);
#16510=EDGE_CURVE('',#12804,#12933,#7252,.T.);
#16511=EDGE_CURVE('',#12932,#12933,#7253,.T.);
#16512=EDGE_CURVE('',#12933,#12931,#10833,.T.);
#16513=EDGE_CURVE('',#12934,#12805,#7254,.T.);
#16514=EDGE_CURVE('',#12934,#12935,#7255,.T.);
#16515=EDGE_CURVE('',#12806,#12935,#7256,.T.);
#16516=EDGE_CURVE('',#12807,#12936,#7257,.T.);
#16517=EDGE_CURVE('',#12935,#12936,#7258,.T.);
#16518=EDGE_CURVE('',#12936,#12934,#10834,.T.);
#16519=EDGE_CURVE('',#12937,#12808,#7259,.T.);
#16520=EDGE_CURVE('',#12937,#12938,#7260,.T.);
#16521=EDGE_CURVE('',#12809,#12938,#7261,.T.);
#16522=EDGE_CURVE('',#12810,#12939,#7262,.T.);
#16523=EDGE_CURVE('',#12938,#12939,#7263,.T.);
#16524=EDGE_CURVE('',#12939,#12937,#10835,.T.);
#16525=EDGE_CURVE('',#12940,#12811,#7264,.T.);
#16526=EDGE_CURVE('',#12940,#12941,#7265,.T.);
#16527=EDGE_CURVE('',#12812,#12941,#7266,.T.);
#16528=EDGE_CURVE('',#12813,#12942,#7267,.T.);
#16529=EDGE_CURVE('',#12941,#12942,#7268,.T.);
#16530=EDGE_CURVE('',#12942,#12940,#10836,.T.);
#16531=EDGE_CURVE('',#12943,#12814,#7269,.T.);
#16532=EDGE_CURVE('',#12943,#12944,#7270,.T.);
#16533=EDGE_CURVE('',#12815,#12944,#7271,.T.);
#16534=EDGE_CURVE('',#12816,#12945,#7272,.T.);
#16535=EDGE_CURVE('',#12944,#12945,#7273,.T.);
#16536=EDGE_CURVE('',#12945,#12943,#10837,.T.);
#16537=EDGE_CURVE('',#12946,#12817,#7274,.T.);
#16538=EDGE_CURVE('',#12946,#12947,#7275,.T.);
#16539=EDGE_CURVE('',#12818,#12947,#7276,.T.);
#16540=EDGE_CURVE('',#12819,#12948,#7277,.T.);
#16541=EDGE_CURVE('',#12947,#12948,#7278,.T.);
#16542=EDGE_CURVE('',#12948,#12946,#10838,.T.);
#16543=EDGE_CURVE('',#12949,#12820,#7279,.T.);
#16544=EDGE_CURVE('',#12949,#12950,#7280,.T.);
#16545=EDGE_CURVE('',#12821,#12950,#7281,.T.);
#16546=EDGE_CURVE('',#12822,#12951,#7282,.T.);
#16547=EDGE_CURVE('',#12950,#12951,#7283,.T.);
#16548=EDGE_CURVE('',#12951,#12949,#10839,.T.);
#16549=EDGE_CURVE('',#12952,#12823,#7284,.T.);
#16550=EDGE_CURVE('',#12952,#12953,#7285,.T.);
#16551=EDGE_CURVE('',#12824,#12953,#7286,.T.);
#16552=EDGE_CURVE('',#12825,#12954,#7287,.T.);
#16553=EDGE_CURVE('',#12953,#12954,#7288,.T.);
#16554=EDGE_CURVE('',#12954,#12952,#10840,.T.);
#16555=EDGE_CURVE('',#12955,#12826,#7289,.T.);
#16556=EDGE_CURVE('',#12955,#12956,#7290,.T.);
#16557=EDGE_CURVE('',#12827,#12956,#7291,.T.);
#16558=EDGE_CURVE('',#12828,#12957,#7292,.T.);
#16559=EDGE_CURVE('',#12956,#12957,#7293,.T.);
#16560=EDGE_CURVE('',#12957,#12955,#10841,.T.);
#16561=EDGE_CURVE('',#12958,#12829,#7294,.T.);
#16562=EDGE_CURVE('',#12958,#12959,#7295,.T.);
#16563=EDGE_CURVE('',#12830,#12959,#7296,.T.);
#16564=EDGE_CURVE('',#12831,#12960,#7297,.T.);
#16565=EDGE_CURVE('',#12959,#12960,#7298,.T.);
#16566=EDGE_CURVE('',#12960,#12958,#10842,.T.);
#16567=EDGE_CURVE('',#12961,#12832,#7299,.T.);
#16568=EDGE_CURVE('',#12961,#12962,#7300,.T.);
#16569=EDGE_CURVE('',#12833,#12962,#7301,.T.);
#16570=EDGE_CURVE('',#12834,#12963,#7302,.T.);
#16571=EDGE_CURVE('',#12962,#12963,#7303,.T.);
#16572=EDGE_CURVE('',#12963,#12961,#10843,.T.);
#16573=EDGE_CURVE('',#12964,#12835,#7304,.T.);
#16574=EDGE_CURVE('',#12964,#12965,#7305,.T.);
#16575=EDGE_CURVE('',#12836,#12965,#7306,.T.);
#16576=EDGE_CURVE('',#12837,#12966,#7307,.T.);
#16577=EDGE_CURVE('',#12965,#12966,#7308,.T.);
#16578=EDGE_CURVE('',#12966,#12964,#10844,.T.);
#16579=EDGE_CURVE('',#12967,#12838,#7309,.T.);
#16580=EDGE_CURVE('',#12967,#12968,#7310,.T.);
#16581=EDGE_CURVE('',#12839,#12968,#7311,.T.);
#16582=EDGE_CURVE('',#12840,#12969,#7312,.T.);
#16583=EDGE_CURVE('',#12968,#12969,#7313,.T.);
#16584=EDGE_CURVE('',#12969,#12967,#10845,.T.);
#16585=EDGE_CURVE('',#12888,#12750,#7314,.T.);
#16586=EDGE_CURVE('',#12970,#12971,#7315,.T.);
#16587=EDGE_CURVE('',#12971,#12972,#7316,.T.);
#16588=EDGE_CURVE('',#12972,#12973,#7317,.T.);
#16589=EDGE_CURVE('',#12973,#12974,#7318,.T.);
#16590=EDGE_CURVE('',#12974,#12975,#7319,.T.);
#16591=EDGE_CURVE('',#12975,#12970,#7320,.T.);
#16592=EDGE_CURVE('',#12976,#12977,#7321,.T.);
#16593=EDGE_CURVE('',#12977,#12976,#10846,.T.);
#16594=EDGE_CURVE('',#12977,#12978,#7322,.T.);
#16595=EDGE_CURVE('',#12978,#12977,#10847,.T.);
#16596=EDGE_CURVE('',#12978,#12979,#7323,.T.);
#16597=EDGE_CURVE('',#12979,#12978,#10848,.T.);
#16598=EDGE_CURVE('',#12979,#12980,#7324,.T.);
#16599=EDGE_CURVE('',#12980,#12979,#10849,.T.);
#16600=EDGE_CURVE('',#12980,#12981,#7325,.T.);
#16601=EDGE_CURVE('',#12981,#12980,#10850,.T.);
#16602=EDGE_CURVE('',#12981,#12976,#7326,.T.);
#16603=EDGE_CURVE('',#12976,#12981,#10851,.T.);
#16604=EDGE_CURVE('',#12982,#12980,#7327,.T.);
#16605=EDGE_CURVE('',#12970,#12976,#7328,.T.);
#16606=EDGE_CURVE('',#12971,#12977,#7329,.T.);
#16607=EDGE_CURVE('',#12975,#12981,#7330,.T.);
#16608=EDGE_CURVE('',#12974,#12980,#7331,.T.);
#16609=EDGE_CURVE('',#12973,#12979,#7332,.T.);
#16610=EDGE_CURVE('',#12972,#12978,#7333,.T.);
#16611=EDGE_CURVE('',#12983,#12984,#7334,.T.);
#16612=EDGE_CURVE('',#12985,#12983,#693,.T.);
#16613=EDGE_CURVE('',#12986,#12985,#10852,.T.);
#16614=EDGE_CURVE('',#12986,#12984,#694,.T.);
#16615=EDGE_CURVE('',#12987,#12988,#7335,.T.);
#16616=EDGE_CURVE('',#12989,#12987,#695,.T.);
#16617=EDGE_CURVE('',#12983,#12989,#696,.T.);
#16618=EDGE_CURVE('',#12984,#12990,#697,.T.);
#16619=EDGE_CURVE('',#12990,#12988,#698,.T.);
#16620=EDGE_CURVE('',#12991,#12992,#7336,.T.);
#16621=EDGE_CURVE('',#12993,#12991,#699,.T.);
#16622=EDGE_CURVE('',#12987,#12993,#700,.T.);
#16623=EDGE_CURVE('',#12988,#12992,#701,.T.);
#16624=EDGE_CURVE('',#12994,#12995,#7337,.T.);
#16625=EDGE_CURVE('',#12996,#12994,#702,.T.);
#16626=EDGE_CURVE('',#12991,#12996,#703,.T.);
#16627=EDGE_CURVE('',#12992,#12997,#704,.T.);
#16628=EDGE_CURVE('',#12997,#12995,#705,.T.);
#16629=EDGE_CURVE('',#12998,#12999,#7338,.T.);
#16630=EDGE_CURVE('',#13000,#12998,#706,.T.);
#16631=EDGE_CURVE('',#12994,#13000,#707,.T.);
#16632=EDGE_CURVE('',#12995,#13001,#708,.T.);
#16633=EDGE_CURVE('',#13001,#12999,#709,.T.);
#16634=EDGE_CURVE('',#13002,#13003,#7339,.T.);
#16635=EDGE_CURVE('',#13004,#13002,#710,.F.);
#16636=EDGE_CURVE('',#12998,#13004,#711,.T.);
#16637=EDGE_CURVE('',#12999,#13003,#712,.T.);
#16638=EDGE_CURVE('',#13005,#13006,#7340,.T.);
#16639=EDGE_CURVE('',#13002,#13005,#713,.F.);
#16640=EDGE_CURVE('',#13003,#13007,#714,.T.);
#16641=EDGE_CURVE('',#13007,#13006,#715,.T.);
#16642=EDGE_CURVE('',#13008,#13009,#7341,.T.);
#16643=EDGE_CURVE('',#13010,#13008,#716,.F.);
#16644=EDGE_CURVE('',#13005,#13010,#717,.F.);
#16645=EDGE_CURVE('',#13006,#13009,#718,.T.);
#16646=EDGE_CURVE('',#13011,#13012,#7342,.T.);
#16647=EDGE_CURVE('',#13008,#13011,#719,.F.);
#16648=EDGE_CURVE('',#13009,#13013,#720,.T.);
#16649=EDGE_CURVE('',#13013,#13012,#721,.T.);
#16650=EDGE_CURVE('',#13014,#13015,#722,.T.);
#16651=EDGE_CURVE('',#13016,#13015,#10853,.T.);
#16652=EDGE_CURVE('',#13016,#13017,#723,.T.);
#16653=EDGE_CURVE('',#13017,#13018,#724,.T.);
#16654=EDGE_CURVE('',#13018,#13019,#725,.T.);
#16655=EDGE_CURVE('',#13019,#13020,#726,.T.);
#16656=EDGE_CURVE('',#13020,#13021,#727,.T.);
#16657=EDGE_CURVE('',#13021,#13022,#728,.T.);
#16658=EDGE_CURVE('',#13022,#13023,#729,.T.);
#16659=EDGE_CURVE('',#13023,#13024,#730,.T.);
#16660=EDGE_CURVE('',#13024,#13025,#731,.T.);
#16661=EDGE_CURVE('',#13025,#13026,#732,.T.);
#16662=EDGE_CURVE('',#13026,#13027,#733,.T.);
#16663=EDGE_CURVE('',#13028,#13027,#10854,.T.);
#16664=EDGE_CURVE('',#13028,#13029,#734,.T.);
#16665=EDGE_CURVE('',#13029,#13030,#735,.T.);
#16666=EDGE_CURVE('',#13030,#13031,#736,.T.);
#16667=EDGE_CURVE('',#13031,#13032,#737,.T.);
#16668=EDGE_CURVE('',#13032,#13033,#738,.T.);
#16669=EDGE_CURVE('',#13033,#13034,#739,.T.);
#16670=EDGE_CURVE('',#13034,#13035,#740,.T.);
#16671=EDGE_CURVE('',#13035,#13036,#741,.T.);
#16672=EDGE_CURVE('',#13036,#13037,#742,.T.);
#16673=EDGE_CURVE('',#13037,#13014,#743,.T.);
#16674=EDGE_CURVE('',#13012,#13038,#744,.T.);
#16675=EDGE_CURVE('',#13038,#13039,#745,.T.);
#16676=EDGE_CURVE('',#13040,#13039,#10855,.T.);
#16677=EDGE_CURVE('',#13041,#13040,#746,.T.);
#16678=EDGE_CURVE('',#13011,#13041,#747,.F.);
#16679=EDGE_CURVE('',#13042,#13043,#10856,.T.);
#16680=EDGE_CURVE('',#13042,#13040,#748,.T.);
#16681=EDGE_CURVE('',#13039,#13028,#749,.T.);
#16682=EDGE_CURVE('',#13043,#13028,#10857,.T.);
#16683=EDGE_CURVE('',#13027,#13042,#750,.T.);
#16684=EDGE_CURVE('',#12985,#13016,#751,.T.);
#16685=EDGE_CURVE('',#13044,#13045,#10858,.T.);
#16686=EDGE_CURVE('',#13044,#12986,#752,.T.);
#16687=EDGE_CURVE('',#13045,#13016,#10859,.T.);
#16688=EDGE_CURVE('',#13015,#13044,#753,.T.);
#16689=EDGE_CURVE('',#13046,#13046,#10860,.T.);
#16690=EDGE_CURVE('',#13046,#13045,#10861,.T.);
#16691=EDGE_CURVE('',#13047,#13047,#10862,.T.);
#16692=EDGE_CURVE('',#13043,#13048,#7343,.T.);
#16693=EDGE_CURVE('',#13048,#13048,#10863,.T.);
#16694=EDGE_CURVE('',#13049,#13050,#7344,.T.);
#16695=EDGE_CURVE('',#13049,#13051,#7345,.T.);
#16696=EDGE_CURVE('',#13052,#13051,#7346,.T.);
#16697=EDGE_CURVE('',#13050,#13052,#353,.T.);
#16698=EDGE_CURVE('',#13053,#13054,#7347,.T.);
#16699=EDGE_CURVE('',#13052,#13053,#354,.T.);
#16700=EDGE_CURVE('',#13051,#13054,#7348,.T.);
#16701=EDGE_CURVE('',#13054,#13049,#10864,.T.);
#16702=EDGE_CURVE('',#13055,#13056,#355,.T.);
#16703=EDGE_CURVE('',#13056,#13057,#10865,.T.);
#16704=EDGE_CURVE('',#13057,#13058,#356,.T.);
#16705=EDGE_CURVE('',#13058,#13059,#357,.T.);
#16706=EDGE_CURVE('',#13059,#13060,#10866,.T.);
#16707=EDGE_CURVE('',#13060,#13061,#358,.T.);
#16708=EDGE_CURVE('',#13061,#13062,#359,.T.);
#16709=EDGE_CURVE('',#13062,#13063,#10867,.T.);
#16710=EDGE_CURVE('',#13063,#13064,#360,.T.);
#16711=EDGE_CURVE('',#13064,#13065,#361,.T.);
#16712=EDGE_CURVE('',#13065,#13066,#10868,.T.);
#16713=EDGE_CURVE('',#13066,#13067,#362,.T.);
#16714=EDGE_CURVE('',#13067,#13068,#363,.T.);
#16715=EDGE_CURVE('',#13068,#13069,#10869,.T.);
#16716=EDGE_CURVE('',#13069,#13070,#364,.T.);
#16717=EDGE_CURVE('',#13070,#13071,#365,.T.);
#16718=EDGE_CURVE('',#13071,#13072,#10870,.T.);
#16719=EDGE_CURVE('',#13072,#13073,#366,.T.);
#16720=EDGE_CURVE('',#13073,#13074,#367,.T.);
#16721=EDGE_CURVE('',#13074,#13075,#10871,.T.);
#16722=EDGE_CURVE('',#13075,#13076,#368,.T.);
#16723=EDGE_CURVE('',#13076,#13077,#369,.T.);
#16724=EDGE_CURVE('',#13077,#13078,#10872,.T.);
#16725=EDGE_CURVE('',#13078,#13079,#370,.T.);
#16726=EDGE_CURVE('',#13079,#13080,#371,.T.);
#16727=EDGE_CURVE('',#13080,#13081,#10873,.T.);
#16728=EDGE_CURVE('',#13081,#13082,#372,.T.);
#16729=EDGE_CURVE('',#13082,#13083,#373,.T.);
#16730=EDGE_CURVE('',#13083,#13084,#10874,.T.);
#16731=EDGE_CURVE('',#13084,#13085,#374,.T.);
#16732=EDGE_CURVE('',#13085,#13086,#375,.T.);
#16733=EDGE_CURVE('',#13086,#13087,#10875,.T.);
#16734=EDGE_CURVE('',#13087,#13088,#376,.T.);
#16735=EDGE_CURVE('',#13088,#13089,#377,.T.);
#16736=EDGE_CURVE('',#13089,#13090,#10876,.T.);
#16737=EDGE_CURVE('',#13090,#13091,#378,.T.);
#16738=EDGE_CURVE('',#13091,#13092,#379,.T.);
#16739=EDGE_CURVE('',#13092,#13093,#10877,.T.);
#16740=EDGE_CURVE('',#13093,#13094,#380,.T.);
#16741=EDGE_CURVE('',#13094,#13095,#381,.T.);
#16742=EDGE_CURVE('',#13095,#13096,#10878,.T.);
#16743=EDGE_CURVE('',#13096,#13097,#382,.T.);
#16744=EDGE_CURVE('',#13097,#13098,#383,.T.);
#16745=EDGE_CURVE('',#13098,#13099,#10879,.T.);
#16746=EDGE_CURVE('',#13099,#13100,#384,.T.);
#16747=EDGE_CURVE('',#13100,#13101,#385,.T.);
#16748=EDGE_CURVE('',#13101,#13102,#10880,.T.);
#16749=EDGE_CURVE('',#13102,#13103,#386,.T.);
#16750=EDGE_CURVE('',#13103,#13104,#387,.T.);
#16751=EDGE_CURVE('',#13104,#13105,#10881,.T.);
#16752=EDGE_CURVE('',#13105,#13106,#388,.T.);
#16753=EDGE_CURVE('',#13106,#13107,#389,.T.);
#16754=EDGE_CURVE('',#13107,#13108,#10882,.T.);
#16755=EDGE_CURVE('',#13108,#13109,#390,.T.);
#16756=EDGE_CURVE('',#13109,#13110,#391,.T.);
#16757=EDGE_CURVE('',#13110,#13050,#10883,.T.);
#16758=EDGE_CURVE('',#13053,#13111,#10884,.T.);
#16759=EDGE_CURVE('',#13111,#13112,#392,.T.);
#16760=EDGE_CURVE('',#13112,#13113,#393,.T.);
#16761=EDGE_CURVE('',#13113,#13114,#10885,.T.);
#16762=EDGE_CURVE('',#13114,#13115,#394,.T.);
#16763=EDGE_CURVE('',#13115,#13116,#395,.T.);
#16764=EDGE_CURVE('',#13116,#13117,#10886,.T.);
#16765=EDGE_CURVE('',#13117,#13118,#396,.T.);
#16766=EDGE_CURVE('',#13118,#13119,#397,.T.);
#16767=EDGE_CURVE('',#13119,#13120,#10887,.T.);
#16768=EDGE_CURVE('',#13120,#13121,#398,.T.);
#16769=EDGE_CURVE('',#13121,#13122,#399,.T.);
#16770=EDGE_CURVE('',#13122,#13123,#10888,.T.);
#16771=EDGE_CURVE('',#13123,#13124,#400,.T.);
#16772=EDGE_CURVE('',#13124,#13125,#401,.T.);
#16773=EDGE_CURVE('',#13125,#13126,#10889,.T.);
#16774=EDGE_CURVE('',#13126,#13127,#402,.T.);
#16775=EDGE_CURVE('',#13127,#13128,#403,.T.);
#16776=EDGE_CURVE('',#13128,#13129,#10890,.T.);
#16777=EDGE_CURVE('',#13129,#13130,#404,.T.);
#16778=EDGE_CURVE('',#13130,#13131,#405,.T.);
#16779=EDGE_CURVE('',#13131,#13132,#10891,.T.);
#16780=EDGE_CURVE('',#13132,#13133,#406,.T.);
#16781=EDGE_CURVE('',#13133,#13134,#407,.T.);
#16782=EDGE_CURVE('',#13134,#13135,#10892,.T.);
#16783=EDGE_CURVE('',#13135,#13136,#408,.T.);
#16784=EDGE_CURVE('',#13136,#13137,#409,.T.);
#16785=EDGE_CURVE('',#13137,#13138,#10893,.T.);
#16786=EDGE_CURVE('',#13138,#13139,#410,.T.);
#16787=EDGE_CURVE('',#13139,#13140,#411,.T.);
#16788=EDGE_CURVE('',#13140,#13141,#10894,.T.);
#16789=EDGE_CURVE('',#13141,#13142,#412,.T.);
#16790=EDGE_CURVE('',#13142,#13143,#413,.T.);
#16791=EDGE_CURVE('',#13143,#13144,#10895,.T.);
#16792=EDGE_CURVE('',#13144,#13145,#414,.T.);
#16793=EDGE_CURVE('',#13145,#13146,#415,.T.);
#16794=EDGE_CURVE('',#13146,#13147,#10896,.T.);
#16795=EDGE_CURVE('',#13147,#13148,#416,.T.);
#16796=EDGE_CURVE('',#13148,#13149,#417,.T.);
#16797=EDGE_CURVE('',#13149,#13150,#10897,.T.);
#16798=EDGE_CURVE('',#13150,#13151,#418,.T.);
#16799=EDGE_CURVE('',#13151,#13152,#419,.T.);
#16800=EDGE_CURVE('',#13152,#13153,#10898,.T.);
#16801=EDGE_CURVE('',#13153,#13154,#420,.T.);
#16802=EDGE_CURVE('',#13154,#13155,#421,.T.);
#16803=EDGE_CURVE('',#13155,#13156,#10899,.T.);
#16804=EDGE_CURVE('',#13156,#13157,#422,.T.);
#16805=EDGE_CURVE('',#13157,#13158,#423,.T.);
#16806=EDGE_CURVE('',#13158,#13159,#10900,.T.);
#16807=EDGE_CURVE('',#13159,#13055,#424,.T.);
#16808=EDGE_CURVE('',#13055,#13160,#7349,.T.);
#16809=EDGE_CURVE('',#13160,#13160,#10901,.T.);
#16810=EDGE_CURVE('',#13161,#13111,#7350,.T.);
#16811=EDGE_CURVE('',#13161,#13162,#7351,.T.);
#16812=EDGE_CURVE('',#13112,#13162,#7352,.T.);
#16813=EDGE_CURVE('',#13113,#13163,#7353,.T.);
#16814=EDGE_CURVE('',#13162,#13163,#7354,.T.);
#16815=EDGE_CURVE('',#13163,#13161,#10902,.T.);
#16816=EDGE_CURVE('',#13164,#13114,#7355,.T.);
#16817=EDGE_CURVE('',#13164,#13165,#7356,.T.);
#16818=EDGE_CURVE('',#13115,#13165,#7357,.T.);
#16819=EDGE_CURVE('',#13116,#13166,#7358,.T.);
#16820=EDGE_CURVE('',#13165,#13166,#7359,.T.);
#16821=EDGE_CURVE('',#13166,#13164,#10903,.T.);
#16822=EDGE_CURVE('',#13167,#13117,#7360,.T.);
#16823=EDGE_CURVE('',#13167,#13168,#7361,.T.);
#16824=EDGE_CURVE('',#13118,#13168,#7362,.T.);
#16825=EDGE_CURVE('',#13119,#13169,#7363,.T.);
#16826=EDGE_CURVE('',#13168,#13169,#7364,.T.);
#16827=EDGE_CURVE('',#13169,#13167,#10904,.T.);
#16828=EDGE_CURVE('',#13170,#13120,#7365,.T.);
#16829=EDGE_CURVE('',#13170,#13171,#7366,.T.);
#16830=EDGE_CURVE('',#13121,#13171,#7367,.T.);
#16831=EDGE_CURVE('',#13122,#13172,#7368,.T.);
#16832=EDGE_CURVE('',#13171,#13172,#7369,.T.);
#16833=EDGE_CURVE('',#13172,#13170,#10905,.T.);
#16834=EDGE_CURVE('',#13173,#13123,#7370,.T.);
#16835=EDGE_CURVE('',#13173,#13174,#7371,.T.);
#16836=EDGE_CURVE('',#13124,#13174,#7372,.T.);
#16837=EDGE_CURVE('',#13125,#13175,#7373,.T.);
#16838=EDGE_CURVE('',#13174,#13175,#7374,.T.);
#16839=EDGE_CURVE('',#13175,#13173,#10906,.T.);
#16840=EDGE_CURVE('',#13176,#13126,#7375,.T.);
#16841=EDGE_CURVE('',#13176,#13177,#7376,.T.);
#16842=EDGE_CURVE('',#13127,#13177,#7377,.T.);
#16843=EDGE_CURVE('',#13128,#13178,#7378,.T.);
#16844=EDGE_CURVE('',#13177,#13178,#7379,.T.);
#16845=EDGE_CURVE('',#13178,#13176,#10907,.T.);
#16846=EDGE_CURVE('',#13179,#13129,#7380,.T.);
#16847=EDGE_CURVE('',#13179,#13180,#7381,.T.);
#16848=EDGE_CURVE('',#13130,#13180,#7382,.T.);
#16849=EDGE_CURVE('',#13131,#13181,#7383,.T.);
#16850=EDGE_CURVE('',#13180,#13181,#7384,.T.);
#16851=EDGE_CURVE('',#13181,#13179,#10908,.T.);
#16852=EDGE_CURVE('',#13182,#13132,#7385,.T.);
#16853=EDGE_CURVE('',#13182,#13183,#7386,.T.);
#16854=EDGE_CURVE('',#13133,#13183,#7387,.T.);
#16855=EDGE_CURVE('',#13134,#13184,#7388,.T.);
#16856=EDGE_CURVE('',#13183,#13184,#7389,.T.);
#16857=EDGE_CURVE('',#13184,#13182,#10909,.T.);
#16858=EDGE_CURVE('',#13185,#13135,#7390,.T.);
#16859=EDGE_CURVE('',#13185,#13186,#7391,.T.);
#16860=EDGE_CURVE('',#13136,#13186,#7392,.T.);
#16861=EDGE_CURVE('',#13137,#13187,#7393,.T.);
#16862=EDGE_CURVE('',#13186,#13187,#7394,.T.);
#16863=EDGE_CURVE('',#13187,#13185,#10910,.T.);
#16864=EDGE_CURVE('',#13188,#13138,#7395,.T.);
#16865=EDGE_CURVE('',#13188,#13189,#7396,.T.);
#16866=EDGE_CURVE('',#13139,#13189,#7397,.T.);
#16867=EDGE_CURVE('',#13140,#13190,#7398,.T.);
#16868=EDGE_CURVE('',#13189,#13190,#7399,.T.);
#16869=EDGE_CURVE('',#13190,#13188,#10911,.T.);
#16870=EDGE_CURVE('',#13191,#13141,#7400,.T.);
#16871=EDGE_CURVE('',#13191,#13192,#7401,.T.);
#16872=EDGE_CURVE('',#13142,#13192,#7402,.T.);
#16873=EDGE_CURVE('',#13143,#13193,#7403,.T.);
#16874=EDGE_CURVE('',#13192,#13193,#7404,.T.);
#16875=EDGE_CURVE('',#13193,#13191,#10912,.T.);
#16876=EDGE_CURVE('',#13194,#13144,#7405,.T.);
#16877=EDGE_CURVE('',#13194,#13195,#7406,.T.);
#16878=EDGE_CURVE('',#13145,#13195,#7407,.T.);
#16879=EDGE_CURVE('',#13146,#13196,#7408,.T.);
#16880=EDGE_CURVE('',#13195,#13196,#7409,.T.);
#16881=EDGE_CURVE('',#13196,#13194,#10913,.T.);
#16882=EDGE_CURVE('',#13197,#13147,#7410,.T.);
#16883=EDGE_CURVE('',#13197,#13198,#7411,.T.);
#16884=EDGE_CURVE('',#13148,#13198,#7412,.T.);
#16885=EDGE_CURVE('',#13149,#13199,#7413,.T.);
#16886=EDGE_CURVE('',#13198,#13199,#7414,.T.);
#16887=EDGE_CURVE('',#13199,#13197,#10914,.T.);
#16888=EDGE_CURVE('',#13200,#13150,#7415,.T.);
#16889=EDGE_CURVE('',#13200,#13201,#7416,.T.);
#16890=EDGE_CURVE('',#13151,#13201,#7417,.T.);
#16891=EDGE_CURVE('',#13152,#13202,#7418,.T.);
#16892=EDGE_CURVE('',#13201,#13202,#7419,.T.);
#16893=EDGE_CURVE('',#13202,#13200,#10915,.T.);
#16894=EDGE_CURVE('',#13203,#13153,#7420,.T.);
#16895=EDGE_CURVE('',#13203,#13204,#7421,.T.);
#16896=EDGE_CURVE('',#13154,#13204,#7422,.T.);
#16897=EDGE_CURVE('',#13155,#13205,#7423,.T.);
#16898=EDGE_CURVE('',#13204,#13205,#7424,.T.);
#16899=EDGE_CURVE('',#13205,#13203,#10916,.T.);
#16900=EDGE_CURVE('',#13206,#13156,#7425,.T.);
#16901=EDGE_CURVE('',#13206,#13207,#7426,.T.);
#16902=EDGE_CURVE('',#13157,#13207,#7427,.T.);
#16903=EDGE_CURVE('',#13158,#13208,#7428,.T.);
#16904=EDGE_CURVE('',#13207,#13208,#7429,.T.);
#16905=EDGE_CURVE('',#13208,#13206,#10917,.T.);
#16906=EDGE_CURVE('',#13209,#13159,#7430,.T.);
#16907=EDGE_CURVE('',#13209,#13210,#7431,.T.);
#16908=EDGE_CURVE('',#13055,#13210,#7432,.T.);
#16909=EDGE_CURVE('',#13056,#13211,#7433,.T.);
#16910=EDGE_CURVE('',#13210,#13211,#7434,.T.);
#16911=EDGE_CURVE('',#13211,#13212,#10918,.T.);
#16912=EDGE_CURVE('',#13212,#13209,#10919,.T.);
#16913=EDGE_CURVE('',#13213,#13057,#7435,.T.);
#16914=EDGE_CURVE('',#13213,#13214,#7436,.T.);
#16915=EDGE_CURVE('',#13058,#13214,#7437,.T.);
#16916=EDGE_CURVE('',#13059,#13215,#7438,.T.);
#16917=EDGE_CURVE('',#13214,#13215,#7439,.T.);
#16918=EDGE_CURVE('',#13215,#13213,#10920,.T.);
#16919=EDGE_CURVE('',#13216,#13060,#7440,.T.);
#16920=EDGE_CURVE('',#13216,#13217,#7441,.T.);
#16921=EDGE_CURVE('',#13061,#13217,#7442,.T.);
#16922=EDGE_CURVE('',#13062,#13218,#7443,.T.);
#16923=EDGE_CURVE('',#13217,#13218,#7444,.T.);
#16924=EDGE_CURVE('',#13218,#13216,#10921,.T.);
#16925=EDGE_CURVE('',#13219,#13063,#7445,.T.);
#16926=EDGE_CURVE('',#13219,#13220,#7446,.T.);
#16927=EDGE_CURVE('',#13064,#13220,#7447,.T.);
#16928=EDGE_CURVE('',#13065,#13221,#7448,.T.);
#16929=EDGE_CURVE('',#13220,#13221,#7449,.T.);
#16930=EDGE_CURVE('',#13221,#13219,#10922,.T.);
#16931=EDGE_CURVE('',#13222,#13066,#7450,.T.);
#16932=EDGE_CURVE('',#13222,#13223,#7451,.T.);
#16933=EDGE_CURVE('',#13067,#13223,#7452,.T.);
#16934=EDGE_CURVE('',#13068,#13224,#7453,.T.);
#16935=EDGE_CURVE('',#13223,#13224,#7454,.T.);
#16936=EDGE_CURVE('',#13224,#13222,#10923,.T.);
#16937=EDGE_CURVE('',#13225,#13069,#7455,.T.);
#16938=EDGE_CURVE('',#13225,#13226,#7456,.T.);
#16939=EDGE_CURVE('',#13070,#13226,#7457,.T.);
#16940=EDGE_CURVE('',#13071,#13227,#7458,.T.);
#16941=EDGE_CURVE('',#13226,#13227,#7459,.T.);
#16942=EDGE_CURVE('',#13227,#13225,#10924,.T.);
#16943=EDGE_CURVE('',#13228,#13072,#7460,.T.);
#16944=EDGE_CURVE('',#13228,#13229,#7461,.T.);
#16945=EDGE_CURVE('',#13073,#13229,#7462,.T.);
#16946=EDGE_CURVE('',#13074,#13230,#7463,.T.);
#16947=EDGE_CURVE('',#13229,#13230,#7464,.T.);
#16948=EDGE_CURVE('',#13230,#13228,#10925,.T.);
#16949=EDGE_CURVE('',#13231,#13075,#7465,.T.);
#16950=EDGE_CURVE('',#13231,#13232,#7466,.T.);
#16951=EDGE_CURVE('',#13076,#13232,#7467,.T.);
#16952=EDGE_CURVE('',#13077,#13233,#7468,.T.);
#16953=EDGE_CURVE('',#13232,#13233,#7469,.T.);
#16954=EDGE_CURVE('',#13233,#13231,#10926,.T.);
#16955=EDGE_CURVE('',#13234,#13078,#7470,.T.);
#16956=EDGE_CURVE('',#13234,#13235,#7471,.T.);
#16957=EDGE_CURVE('',#13079,#13235,#7472,.T.);
#16958=EDGE_CURVE('',#13080,#13236,#7473,.T.);
#16959=EDGE_CURVE('',#13235,#13236,#7474,.T.);
#16960=EDGE_CURVE('',#13236,#13234,#10927,.T.);
#16961=EDGE_CURVE('',#13237,#13081,#7475,.T.);
#16962=EDGE_CURVE('',#13237,#13238,#7476,.T.);
#16963=EDGE_CURVE('',#13082,#13238,#7477,.T.);
#16964=EDGE_CURVE('',#13083,#13239,#7478,.T.);
#16965=EDGE_CURVE('',#13238,#13239,#7479,.T.);
#16966=EDGE_CURVE('',#13239,#13237,#10928,.T.);
#16967=EDGE_CURVE('',#13240,#13084,#7480,.T.);
#16968=EDGE_CURVE('',#13240,#13241,#7481,.T.);
#16969=EDGE_CURVE('',#13085,#13241,#7482,.T.);
#16970=EDGE_CURVE('',#13086,#13242,#7483,.T.);
#16971=EDGE_CURVE('',#13241,#13242,#7484,.T.);
#16972=EDGE_CURVE('',#13242,#13240,#10929,.T.);
#16973=EDGE_CURVE('',#13243,#13087,#7485,.T.);
#16974=EDGE_CURVE('',#13243,#13244,#7486,.T.);
#16975=EDGE_CURVE('',#13088,#13244,#7487,.T.);
#16976=EDGE_CURVE('',#13089,#13245,#7488,.T.);
#16977=EDGE_CURVE('',#13244,#13245,#7489,.T.);
#16978=EDGE_CURVE('',#13245,#13243,#10930,.T.);
#16979=EDGE_CURVE('',#13246,#13090,#7490,.T.);
#16980=EDGE_CURVE('',#13246,#13247,#7491,.T.);
#16981=EDGE_CURVE('',#13091,#13247,#7492,.T.);
#16982=EDGE_CURVE('',#13092,#13248,#7493,.T.);
#16983=EDGE_CURVE('',#13247,#13248,#7494,.T.);
#16984=EDGE_CURVE('',#13248,#13246,#10931,.T.);
#16985=EDGE_CURVE('',#13249,#13093,#7495,.T.);
#16986=EDGE_CURVE('',#13249,#13250,#7496,.T.);
#16987=EDGE_CURVE('',#13094,#13250,#7497,.T.);
#16988=EDGE_CURVE('',#13095,#13251,#7498,.T.);
#16989=EDGE_CURVE('',#13250,#13251,#7499,.T.);
#16990=EDGE_CURVE('',#13251,#13249,#10932,.T.);
#16991=EDGE_CURVE('',#13252,#13096,#7500,.T.);
#16992=EDGE_CURVE('',#13252,#13253,#7501,.T.);
#16993=EDGE_CURVE('',#13097,#13253,#7502,.T.);
#16994=EDGE_CURVE('',#13098,#13254,#7503,.T.);
#16995=EDGE_CURVE('',#13253,#13254,#7504,.T.);
#16996=EDGE_CURVE('',#13254,#13252,#10933,.T.);
#16997=EDGE_CURVE('',#13255,#13099,#7505,.T.);
#16998=EDGE_CURVE('',#13255,#13256,#7506,.T.);
#16999=EDGE_CURVE('',#13100,#13256,#7507,.T.);
#17000=EDGE_CURVE('',#13101,#13257,#7508,.T.);
#17001=EDGE_CURVE('',#13256,#13257,#7509,.T.);
#17002=EDGE_CURVE('',#13257,#13255,#10934,.T.);
#17003=EDGE_CURVE('',#13258,#13102,#7510,.T.);
#17004=EDGE_CURVE('',#13258,#13259,#7511,.T.);
#17005=EDGE_CURVE('',#13103,#13259,#7512,.T.);
#17006=EDGE_CURVE('',#13104,#13260,#7513,.T.);
#17007=EDGE_CURVE('',#13259,#13260,#7514,.T.);
#17008=EDGE_CURVE('',#13260,#13258,#10935,.T.);
#17009=EDGE_CURVE('',#13261,#13105,#7515,.T.);
#17010=EDGE_CURVE('',#13261,#13262,#7516,.T.);
#17011=EDGE_CURVE('',#13106,#13262,#7517,.T.);
#17012=EDGE_CURVE('',#13107,#13263,#7518,.T.);
#17013=EDGE_CURVE('',#13262,#13263,#7519,.T.);
#17014=EDGE_CURVE('',#13263,#13261,#10936,.T.);
#17015=EDGE_CURVE('',#13264,#13108,#7520,.T.);
#17016=EDGE_CURVE('',#13264,#13265,#7521,.T.);
#17017=EDGE_CURVE('',#13109,#13265,#7522,.T.);
#17018=EDGE_CURVE('',#13110,#13266,#7523,.T.);
#17019=EDGE_CURVE('',#13265,#13266,#7524,.T.);
#17020=EDGE_CURVE('',#13266,#13264,#10937,.T.);
#17021=EDGE_CURVE('',#13212,#13047,#7525,.T.);
#17022=EDGE_CURVE('',#13267,#13268,#7526,.T.);
#17023=EDGE_CURVE('',#13268,#13269,#7527,.T.);
#17024=EDGE_CURVE('',#13269,#13270,#7528,.T.);
#17025=EDGE_CURVE('',#13270,#13271,#7529,.T.);
#17026=EDGE_CURVE('',#13271,#13272,#7530,.T.);
#17027=EDGE_CURVE('',#13272,#13267,#7531,.T.);
#17028=EDGE_CURVE('',#13273,#13274,#7532,.T.);
#17029=EDGE_CURVE('',#13273,#13274,#10938,.T.);
#17030=EDGE_CURVE('',#13274,#13275,#7533,.T.);
#17031=EDGE_CURVE('',#13274,#13275,#10939,.T.);
#17032=EDGE_CURVE('',#13275,#13276,#7534,.T.);
#17033=EDGE_CURVE('',#13275,#13276,#10940,.T.);
#17034=EDGE_CURVE('',#13276,#13277,#7535,.T.);
#17035=EDGE_CURVE('',#13276,#13277,#10941,.T.);
#17036=EDGE_CURVE('',#13277,#13278,#7536,.T.);
#17037=EDGE_CURVE('',#13277,#13278,#10942,.T.);
#17038=EDGE_CURVE('',#13278,#13273,#7537,.T.);
#17039=EDGE_CURVE('',#13278,#13273,#10943,.T.);
#17040=EDGE_CURVE('',#13279,#13273,#7538,.T.);
#17041=EDGE_CURVE('',#13267,#13273,#7539,.T.);
#17042=EDGE_CURVE('',#13268,#13274,#7540,.T.);
#17043=EDGE_CURVE('',#13272,#13278,#7541,.T.);
#17044=EDGE_CURVE('',#13271,#13277,#7542,.T.);
#17045=EDGE_CURVE('',#13270,#13276,#7543,.T.);
#17046=EDGE_CURVE('',#13269,#13275,#7544,.T.);
#17047=EDGE_CURVE('',#13280,#13281,#7545,.T.);
#17048=EDGE_CURVE('',#13282,#13280,#754,.F.);
#17049=EDGE_CURVE('',#13283,#13282,#10944,.T.);
#17050=EDGE_CURVE('',#13283,#13281,#755,.T.);
#17051=EDGE_CURVE('',#13284,#13285,#7546,.T.);
#17052=EDGE_CURVE('',#13280,#13284,#756,.F.);
#17053=EDGE_CURVE('',#13281,#13285,#757,.T.);
#17054=EDGE_CURVE('',#13286,#13287,#7547,.T.);
#17055=EDGE_CURVE('',#13288,#13286,#758,.T.);
#17056=EDGE_CURVE('',#13284,#13288,#759,.F.);
#17057=EDGE_CURVE('',#13285,#13289,#760,.T.);
#17058=EDGE_CURVE('',#13289,#13287,#761,.T.);
#17059=EDGE_CURVE('',#13290,#13291,#7548,.T.);
#17060=EDGE_CURVE('',#13292,#13290,#762,.T.);
#17061=EDGE_CURVE('',#13286,#13292,#763,.T.);
#17062=EDGE_CURVE('',#13287,#13291,#764,.T.);
#17063=EDGE_CURVE('',#13293,#13294,#7549,.T.);
#17064=EDGE_CURVE('',#13295,#13293,#765,.F.);
#17065=EDGE_CURVE('',#13290,#13295,#766,.T.);
#17066=EDGE_CURVE('',#13291,#13296,#767,.T.);
#17067=EDGE_CURVE('',#13296,#13294,#768,.T.);
#17068=EDGE_CURVE('',#13297,#13298,#7550,.T.);
#17069=EDGE_CURVE('',#13293,#13297,#769,.F.);
#17070=EDGE_CURVE('',#13294,#13298,#770,.T.);
#17071=EDGE_CURVE('',#13299,#13300,#7551,.T.);
#17072=EDGE_CURVE('',#13301,#13299,#771,.F.);
#17073=EDGE_CURVE('',#13297,#13301,#772,.F.);
#17074=EDGE_CURVE('',#13298,#13302,#773,.T.);
#17075=EDGE_CURVE('',#13302,#13300,#774,.T.);
#17076=EDGE_CURVE('',#13303,#13304,#7552,.T.);
#17077=EDGE_CURVE('',#13299,#13303,#775,.F.);
#17078=EDGE_CURVE('',#13300,#13304,#776,.T.);
#17079=EDGE_CURVE('',#13305,#13306,#7553,.T.);
#17080=EDGE_CURVE('',#13307,#13305,#777,.T.);
#17081=EDGE_CURVE('',#13303,#13307,#778,.F.);
#17082=EDGE_CURVE('',#13304,#13308,#779,.T.);
#17083=EDGE_CURVE('',#13308,#13306,#780,.T.);
#17084=EDGE_CURVE('',#13309,#13310,#7554,.T.);
#17085=EDGE_CURVE('',#13311,#13309,#781,.T.);
#17086=EDGE_CURVE('',#13305,#13311,#782,.T.);
#17087=EDGE_CURVE('',#13306,#13310,#783,.T.);
#17088=EDGE_CURVE('',#13312,#13313,#7555,.T.);
#17089=EDGE_CURVE('',#13314,#13312,#784,.F.);
#17090=EDGE_CURVE('',#13309,#13314,#785,.T.);
#17091=EDGE_CURVE('',#13310,#13315,#786,.T.);
#17092=EDGE_CURVE('',#13315,#13313,#787,.T.);
#17093=EDGE_CURVE('',#13316,#13317,#7556,.T.);
#17094=EDGE_CURVE('',#13312,#13316,#788,.F.);
#17095=EDGE_CURVE('',#13313,#13318,#789,.T.);
#17096=EDGE_CURVE('',#13318,#13317,#790,.T.);
#17097=EDGE_CURVE('',#13319,#13320,#7557,.T.);
#17098=EDGE_CURVE('',#13321,#13319,#791,.F.);
#17099=EDGE_CURVE('',#13316,#13321,#792,.F.);
#17100=EDGE_CURVE('',#13317,#13320,#793,.T.);
#17101=EDGE_CURVE('',#13322,#13323,#7558,.T.);
#17102=EDGE_CURVE('',#13319,#13322,#794,.F.);
#17103=EDGE_CURVE('',#13320,#13324,#795,.T.);
#17104=EDGE_CURVE('',#13324,#13323,#796,.T.);
#17105=EDGE_CURVE('',#13325,#13326,#7559,.T.);
#17106=EDGE_CURVE('',#13327,#13325,#797,.F.);
#17107=EDGE_CURVE('',#13322,#13327,#798,.F.);
#17108=EDGE_CURVE('',#13323,#13326,#799,.T.);
#17109=EDGE_CURVE('',#13328,#13329,#7560,.T.);
#17110=EDGE_CURVE('',#13325,#13328,#800,.F.);
#17111=EDGE_CURVE('',#13326,#13329,#801,.T.);
#17112=EDGE_CURVE('',#13330,#13331,#7561,.T.);
#17113=EDGE_CURVE('',#13332,#13330,#802,.F.);
#17114=EDGE_CURVE('',#13328,#13332,#803,.F.);
#17115=EDGE_CURVE('',#13329,#13333,#804,.T.);
#17116=EDGE_CURVE('',#13333,#13331,#805,.T.);
#17117=EDGE_CURVE('',#13334,#13335,#7562,.T.);
#17118=EDGE_CURVE('',#13330,#13334,#806,.F.);
#17119=EDGE_CURVE('',#13331,#13336,#807,.T.);
#17120=EDGE_CURVE('',#13336,#13335,#808,.T.);
#17121=EDGE_CURVE('',#13337,#13338,#7563,.T.);
#17122=EDGE_CURVE('',#13339,#13337,#809,.F.);
#17123=EDGE_CURVE('',#13334,#13339,#810,.F.);
#17124=EDGE_CURVE('',#13335,#13340,#811,.T.);
#17125=EDGE_CURVE('',#13340,#13338,#812,.F.);
#17126=EDGE_CURVE('',#13341,#13342,#813,.T.);
#17127=EDGE_CURVE('',#13343,#13342,#10945,.T.);
#17128=EDGE_CURVE('',#13343,#13344,#814,.T.);
#17129=EDGE_CURVE('',#13344,#13345,#815,.T.);
#17130=EDGE_CURVE('',#13345,#13346,#816,.T.);
#17131=EDGE_CURVE('',#13346,#13347,#817,.T.);
#17132=EDGE_CURVE('',#13347,#13348,#818,.T.);
#17133=EDGE_CURVE('',#13348,#13349,#819,.T.);
#17134=EDGE_CURVE('',#13349,#13350,#820,.T.);
#17135=EDGE_CURVE('',#13350,#13351,#821,.T.);
#17136=EDGE_CURVE('',#13351,#13352,#822,.T.);
#17137=EDGE_CURVE('',#13352,#13353,#823,.T.);
#17138=EDGE_CURVE('',#13353,#13354,#824,.T.);
#17139=EDGE_CURVE('',#13354,#13355,#825,.T.);
#17140=EDGE_CURVE('',#13355,#13356,#826,.T.);
#17141=EDGE_CURVE('',#13356,#13357,#827,.T.);
#17142=EDGE_CURVE('',#13357,#13358,#828,.T.);
#17143=EDGE_CURVE('',#13358,#13359,#829,.T.);
#17144=EDGE_CURVE('',#13359,#13360,#830,.T.);
#17145=EDGE_CURVE('',#13360,#13361,#831,.T.);
#17146=EDGE_CURVE('',#13361,#13362,#832,.T.);
#17147=EDGE_CURVE('',#13362,#13363,#833,.T.);
#17148=EDGE_CURVE('',#13363,#13364,#834,.T.);
#17149=EDGE_CURVE('',#13365,#13364,#10946,.T.);
#17150=EDGE_CURVE('',#13365,#13366,#835,.T.);
#17151=EDGE_CURVE('',#13366,#13367,#836,.T.);
#17152=EDGE_CURVE('',#13367,#13368,#837,.T.);
#17153=EDGE_CURVE('',#13368,#13369,#838,.T.);
#17154=EDGE_CURVE('',#13369,#13370,#839,.T.);
#17155=EDGE_CURVE('',#13370,#13371,#840,.T.);
#17156=EDGE_CURVE('',#13371,#13372,#841,.T.);
#17157=EDGE_CURVE('',#13372,#13373,#842,.T.);
#17158=EDGE_CURVE('',#13373,#13374,#843,.T.);
#17159=EDGE_CURVE('',#13374,#13375,#844,.T.);
#17160=EDGE_CURVE('',#13375,#13376,#845,.T.);
#17161=EDGE_CURVE('',#13376,#13377,#846,.T.);
#17162=EDGE_CURVE('',#13377,#13378,#847,.T.);
#17163=EDGE_CURVE('',#13378,#13379,#848,.T.);
#17164=EDGE_CURVE('',#13379,#13380,#849,.T.);
#17165=EDGE_CURVE('',#13380,#13381,#850,.T.);
#17166=EDGE_CURVE('',#13381,#13382,#851,.T.);
#17167=EDGE_CURVE('',#13382,#13383,#852,.T.);
#17168=EDGE_CURVE('',#13383,#13384,#853,.T.);
#17169=EDGE_CURVE('',#13384,#13341,#854,.T.);
#17170=EDGE_CURVE('',#13338,#13385,#855,.F.);
#17171=EDGE_CURVE('',#13386,#13385,#10947,.T.);
#17172=EDGE_CURVE('',#13337,#13386,#856,.F.);
#17173=EDGE_CURVE('',#13387,#13388,#10948,.T.);
#17174=EDGE_CURVE('',#13387,#13386,#857,.T.);
#17175=EDGE_CURVE('',#13385,#13389,#858,.T.);
#17176=EDGE_CURVE('',#13389,#13365,#859,.T.);
#17177=EDGE_CURVE('',#13388,#13365,#10949,.T.);
#17178=EDGE_CURVE('',#13364,#13387,#860,.T.);
#17179=EDGE_CURVE('',#13390,#13343,#861,.T.);
#17180=EDGE_CURVE('',#13390,#13282,#862,.T.);
#17181=EDGE_CURVE('',#13391,#13392,#10950,.T.);
#17182=EDGE_CURVE('',#13391,#13283,#863,.T.);
#17183=EDGE_CURVE('',#13392,#13343,#10951,.T.);
#17184=EDGE_CURVE('',#13342,#13391,#864,.T.);
#17185=EDGE_CURVE('',#13393,#13393,#10952,.T.);
#17186=EDGE_CURVE('',#13393,#13392,#10953,.T.);
#17187=EDGE_CURVE('',#13394,#13394,#10954,.T.);
#17188=EDGE_CURVE('',#13388,#13395,#7564,.T.);
#17189=EDGE_CURVE('',#13395,#13395,#10955,.T.);
#17190=EDGE_CURVE('',#13396,#13397,#7565,.T.);
#17191=EDGE_CURVE('',#13396,#13398,#7566,.T.);
#17192=EDGE_CURVE('',#13399,#13398,#7567,.T.);
#17193=EDGE_CURVE('',#13397,#13399,#425,.T.);
#17194=EDGE_CURVE('',#13400,#13401,#7568,.T.);
#17195=EDGE_CURVE('',#13399,#13400,#426,.T.);
#17196=EDGE_CURVE('',#13398,#13401,#7569,.T.);
#17197=EDGE_CURVE('',#13401,#13396,#10956,.T.);
#17198=EDGE_CURVE('',#13402,#13403,#427,.T.);
#17199=EDGE_CURVE('',#13403,#13404,#10957,.T.);
#17200=EDGE_CURVE('',#13404,#13405,#428,.T.);
#17201=EDGE_CURVE('',#13405,#13406,#429,.T.);
#17202=EDGE_CURVE('',#13406,#13407,#10958,.T.);
#17203=EDGE_CURVE('',#13407,#13408,#430,.T.);
#17204=EDGE_CURVE('',#13408,#13409,#431,.T.);
#17205=EDGE_CURVE('',#13409,#13410,#10959,.T.);
#17206=EDGE_CURVE('',#13410,#13411,#432,.T.);
#17207=EDGE_CURVE('',#13411,#13412,#433,.T.);
#17208=EDGE_CURVE('',#13412,#13413,#10960,.T.);
#17209=EDGE_CURVE('',#13413,#13414,#434,.T.);
#17210=EDGE_CURVE('',#13414,#13415,#435,.T.);
#17211=EDGE_CURVE('',#13415,#13416,#10961,.T.);
#17212=EDGE_CURVE('',#13416,#13417,#436,.T.);
#17213=EDGE_CURVE('',#13417,#13418,#437,.T.);
#17214=EDGE_CURVE('',#13418,#13419,#10962,.T.);
#17215=EDGE_CURVE('',#13419,#13420,#438,.T.);
#17216=EDGE_CURVE('',#13420,#13421,#439,.T.);
#17217=EDGE_CURVE('',#13421,#13422,#10963,.T.);
#17218=EDGE_CURVE('',#13422,#13423,#440,.T.);
#17219=EDGE_CURVE('',#13423,#13424,#441,.T.);
#17220=EDGE_CURVE('',#13424,#13425,#10964,.T.);
#17221=EDGE_CURVE('',#13425,#13426,#442,.T.);
#17222=EDGE_CURVE('',#13426,#13427,#443,.T.);
#17223=EDGE_CURVE('',#13427,#13428,#10965,.T.);
#17224=EDGE_CURVE('',#13428,#13429,#444,.T.);
#17225=EDGE_CURVE('',#13429,#13430,#445,.T.);
#17226=EDGE_CURVE('',#13430,#13431,#10966,.T.);
#17227=EDGE_CURVE('',#13431,#13432,#446,.T.);
#17228=EDGE_CURVE('',#13432,#13433,#447,.T.);
#17229=EDGE_CURVE('',#13433,#13434,#10967,.T.);
#17230=EDGE_CURVE('',#13434,#13435,#448,.T.);
#17231=EDGE_CURVE('',#13435,#13436,#449,.T.);
#17232=EDGE_CURVE('',#13436,#13437,#10968,.T.);
#17233=EDGE_CURVE('',#13437,#13438,#450,.T.);
#17234=EDGE_CURVE('',#13438,#13439,#451,.T.);
#17235=EDGE_CURVE('',#13439,#13440,#10969,.T.);
#17236=EDGE_CURVE('',#13440,#13441,#452,.T.);
#17237=EDGE_CURVE('',#13441,#13442,#453,.T.);
#17238=EDGE_CURVE('',#13442,#13443,#10970,.T.);
#17239=EDGE_CURVE('',#13443,#13444,#454,.T.);
#17240=EDGE_CURVE('',#13444,#13445,#455,.T.);
#17241=EDGE_CURVE('',#13445,#13446,#10971,.T.);
#17242=EDGE_CURVE('',#13446,#13447,#456,.T.);
#17243=EDGE_CURVE('',#13447,#13448,#457,.T.);
#17244=EDGE_CURVE('',#13448,#13449,#10972,.T.);
#17245=EDGE_CURVE('',#13449,#13450,#458,.T.);
#17246=EDGE_CURVE('',#13450,#13451,#459,.T.);
#17247=EDGE_CURVE('',#13451,#13452,#10973,.T.);
#17248=EDGE_CURVE('',#13452,#13453,#460,.T.);
#17249=EDGE_CURVE('',#13453,#13454,#461,.T.);
#17250=EDGE_CURVE('',#13454,#13455,#10974,.T.);
#17251=EDGE_CURVE('',#13455,#13456,#462,.T.);
#17252=EDGE_CURVE('',#13456,#13457,#463,.T.);
#17253=EDGE_CURVE('',#13457,#13397,#10975,.T.);
#17254=EDGE_CURVE('',#13400,#13458,#10976,.T.);
#17255=EDGE_CURVE('',#13458,#13459,#464,.T.);
#17256=EDGE_CURVE('',#13459,#13460,#465,.T.);
#17257=EDGE_CURVE('',#13460,#13461,#10977,.T.);
#17258=EDGE_CURVE('',#13461,#13462,#466,.T.);
#17259=EDGE_CURVE('',#13462,#13463,#467,.T.);
#17260=EDGE_CURVE('',#13463,#13464,#10978,.T.);
#17261=EDGE_CURVE('',#13464,#13465,#468,.T.);
#17262=EDGE_CURVE('',#13465,#13466,#469,.T.);
#17263=EDGE_CURVE('',#13466,#13467,#10979,.T.);
#17264=EDGE_CURVE('',#13467,#13468,#470,.T.);
#17265=EDGE_CURVE('',#13468,#13469,#471,.T.);
#17266=EDGE_CURVE('',#13469,#13470,#10980,.T.);
#17267=EDGE_CURVE('',#13470,#13471,#472,.T.);
#17268=EDGE_CURVE('',#13471,#13472,#473,.T.);
#17269=EDGE_CURVE('',#13472,#13473,#10981,.T.);
#17270=EDGE_CURVE('',#13473,#13474,#474,.T.);
#17271=EDGE_CURVE('',#13474,#13475,#475,.T.);
#17272=EDGE_CURVE('',#13475,#13476,#10982,.T.);
#17273=EDGE_CURVE('',#13476,#13477,#476,.T.);
#17274=EDGE_CURVE('',#13477,#13478,#477,.T.);
#17275=EDGE_CURVE('',#13478,#13479,#10983,.T.);
#17276=EDGE_CURVE('',#13479,#13480,#478,.T.);
#17277=EDGE_CURVE('',#13480,#13481,#479,.T.);
#17278=EDGE_CURVE('',#13481,#13482,#10984,.T.);
#17279=EDGE_CURVE('',#13482,#13483,#480,.T.);
#17280=EDGE_CURVE('',#13483,#13484,#481,.T.);
#17281=EDGE_CURVE('',#13484,#13485,#10985,.T.);
#17282=EDGE_CURVE('',#13485,#13486,#482,.T.);
#17283=EDGE_CURVE('',#13486,#13487,#483,.T.);
#17284=EDGE_CURVE('',#13487,#13488,#10986,.T.);
#17285=EDGE_CURVE('',#13488,#13489,#484,.T.);
#17286=EDGE_CURVE('',#13489,#13490,#485,.T.);
#17287=EDGE_CURVE('',#13490,#13491,#10987,.T.);
#17288=EDGE_CURVE('',#13491,#13492,#486,.T.);
#17289=EDGE_CURVE('',#13492,#13493,#487,.T.);
#17290=EDGE_CURVE('',#13493,#13494,#10988,.T.);
#17291=EDGE_CURVE('',#13494,#13495,#488,.T.);
#17292=EDGE_CURVE('',#13495,#13496,#489,.T.);
#17293=EDGE_CURVE('',#13496,#13497,#10989,.T.);
#17294=EDGE_CURVE('',#13497,#13498,#490,.T.);
#17295=EDGE_CURVE('',#13498,#13499,#491,.T.);
#17296=EDGE_CURVE('',#13499,#13500,#10990,.T.);
#17297=EDGE_CURVE('',#13500,#13501,#492,.T.);
#17298=EDGE_CURVE('',#13501,#13502,#493,.T.);
#17299=EDGE_CURVE('',#13502,#13503,#10991,.T.);
#17300=EDGE_CURVE('',#13503,#13504,#494,.T.);
#17301=EDGE_CURVE('',#13504,#13505,#495,.T.);
#17302=EDGE_CURVE('',#13505,#13506,#10992,.T.);
#17303=EDGE_CURVE('',#13506,#13402,#496,.T.);
#17304=EDGE_CURVE('',#13402,#13507,#7570,.T.);
#17305=EDGE_CURVE('',#13507,#13507,#10993,.T.);
#17306=EDGE_CURVE('',#13508,#13458,#7571,.T.);
#17307=EDGE_CURVE('',#13508,#13509,#7572,.T.);
#17308=EDGE_CURVE('',#13459,#13509,#7573,.T.);
#17309=EDGE_CURVE('',#13460,#13510,#7574,.T.);
#17310=EDGE_CURVE('',#13509,#13510,#7575,.T.);
#17311=EDGE_CURVE('',#13510,#13508,#10994,.T.);
#17312=EDGE_CURVE('',#13511,#13461,#7576,.T.);
#17313=EDGE_CURVE('',#13511,#13512,#7577,.T.);
#17314=EDGE_CURVE('',#13462,#13512,#7578,.T.);
#17315=EDGE_CURVE('',#13463,#13513,#7579,.T.);
#17316=EDGE_CURVE('',#13512,#13513,#7580,.T.);
#17317=EDGE_CURVE('',#13513,#13511,#10995,.T.);
#17318=EDGE_CURVE('',#13514,#13464,#7581,.T.);
#17319=EDGE_CURVE('',#13514,#13515,#7582,.T.);
#17320=EDGE_CURVE('',#13465,#13515,#7583,.T.);
#17321=EDGE_CURVE('',#13466,#13516,#7584,.T.);
#17322=EDGE_CURVE('',#13515,#13516,#7585,.T.);
#17323=EDGE_CURVE('',#13516,#13514,#10996,.T.);
#17324=EDGE_CURVE('',#13517,#13467,#7586,.T.);
#17325=EDGE_CURVE('',#13517,#13518,#7587,.T.);
#17326=EDGE_CURVE('',#13468,#13518,#7588,.T.);
#17327=EDGE_CURVE('',#13469,#13519,#7589,.T.);
#17328=EDGE_CURVE('',#13518,#13519,#7590,.T.);
#17329=EDGE_CURVE('',#13519,#13517,#10997,.T.);
#17330=EDGE_CURVE('',#13520,#13470,#7591,.T.);
#17331=EDGE_CURVE('',#13520,#13521,#7592,.T.);
#17332=EDGE_CURVE('',#13471,#13521,#7593,.T.);
#17333=EDGE_CURVE('',#13472,#13522,#7594,.T.);
#17334=EDGE_CURVE('',#13521,#13522,#7595,.T.);
#17335=EDGE_CURVE('',#13522,#13520,#10998,.T.);
#17336=EDGE_CURVE('',#13523,#13473,#7596,.T.);
#17337=EDGE_CURVE('',#13523,#13524,#7597,.T.);
#17338=EDGE_CURVE('',#13474,#13524,#7598,.T.);
#17339=EDGE_CURVE('',#13475,#13525,#7599,.T.);
#17340=EDGE_CURVE('',#13524,#13525,#7600,.T.);
#17341=EDGE_CURVE('',#13525,#13523,#10999,.T.);
#17342=EDGE_CURVE('',#13526,#13476,#7601,.T.);
#17343=EDGE_CURVE('',#13526,#13527,#7602,.T.);
#17344=EDGE_CURVE('',#13477,#13527,#7603,.T.);
#17345=EDGE_CURVE('',#13478,#13528,#7604,.T.);
#17346=EDGE_CURVE('',#13527,#13528,#7605,.T.);
#17347=EDGE_CURVE('',#13528,#13526,#11000,.T.);
#17348=EDGE_CURVE('',#13529,#13479,#7606,.T.);
#17349=EDGE_CURVE('',#13529,#13530,#7607,.T.);
#17350=EDGE_CURVE('',#13480,#13530,#7608,.T.);
#17351=EDGE_CURVE('',#13481,#13531,#7609,.T.);
#17352=EDGE_CURVE('',#13530,#13531,#7610,.T.);
#17353=EDGE_CURVE('',#13531,#13529,#11001,.T.);
#17354=EDGE_CURVE('',#13532,#13482,#7611,.T.);
#17355=EDGE_CURVE('',#13532,#13533,#7612,.T.);
#17356=EDGE_CURVE('',#13483,#13533,#7613,.T.);
#17357=EDGE_CURVE('',#13484,#13534,#7614,.T.);
#17358=EDGE_CURVE('',#13533,#13534,#7615,.T.);
#17359=EDGE_CURVE('',#13534,#13532,#11002,.T.);
#17360=EDGE_CURVE('',#13535,#13485,#7616,.T.);
#17361=EDGE_CURVE('',#13535,#13536,#7617,.T.);
#17362=EDGE_CURVE('',#13486,#13536,#7618,.T.);
#17363=EDGE_CURVE('',#13487,#13537,#7619,.T.);
#17364=EDGE_CURVE('',#13536,#13537,#7620,.T.);
#17365=EDGE_CURVE('',#13537,#13535,#11003,.T.);
#17366=EDGE_CURVE('',#13538,#13488,#7621,.T.);
#17367=EDGE_CURVE('',#13538,#13539,#7622,.T.);
#17368=EDGE_CURVE('',#13489,#13539,#7623,.T.);
#17369=EDGE_CURVE('',#13490,#13540,#7624,.T.);
#17370=EDGE_CURVE('',#13539,#13540,#7625,.T.);
#17371=EDGE_CURVE('',#13540,#13538,#11004,.T.);
#17372=EDGE_CURVE('',#13541,#13491,#7626,.T.);
#17373=EDGE_CURVE('',#13541,#13542,#7627,.T.);
#17374=EDGE_CURVE('',#13492,#13542,#7628,.T.);
#17375=EDGE_CURVE('',#13493,#13543,#7629,.T.);
#17376=EDGE_CURVE('',#13542,#13543,#7630,.T.);
#17377=EDGE_CURVE('',#13543,#13541,#11005,.T.);
#17378=EDGE_CURVE('',#13544,#13494,#7631,.T.);
#17379=EDGE_CURVE('',#13544,#13545,#7632,.T.);
#17380=EDGE_CURVE('',#13495,#13545,#7633,.T.);
#17381=EDGE_CURVE('',#13496,#13546,#7634,.T.);
#17382=EDGE_CURVE('',#13545,#13546,#7635,.T.);
#17383=EDGE_CURVE('',#13546,#13544,#11006,.T.);
#17384=EDGE_CURVE('',#13547,#13497,#7636,.T.);
#17385=EDGE_CURVE('',#13547,#13548,#7637,.T.);
#17386=EDGE_CURVE('',#13498,#13548,#7638,.T.);
#17387=EDGE_CURVE('',#13499,#13549,#7639,.T.);
#17388=EDGE_CURVE('',#13548,#13549,#7640,.T.);
#17389=EDGE_CURVE('',#13549,#13547,#11007,.T.);
#17390=EDGE_CURVE('',#13550,#13500,#7641,.T.);
#17391=EDGE_CURVE('',#13550,#13551,#7642,.T.);
#17392=EDGE_CURVE('',#13501,#13551,#7643,.T.);
#17393=EDGE_CURVE('',#13502,#13552,#7644,.T.);
#17394=EDGE_CURVE('',#13551,#13552,#7645,.T.);
#17395=EDGE_CURVE('',#13552,#13550,#11008,.T.);
#17396=EDGE_CURVE('',#13553,#13503,#7646,.T.);
#17397=EDGE_CURVE('',#13553,#13554,#7647,.T.);
#17398=EDGE_CURVE('',#13504,#13554,#7648,.T.);
#17399=EDGE_CURVE('',#13505,#13555,#7649,.T.);
#17400=EDGE_CURVE('',#13554,#13555,#7650,.T.);
#17401=EDGE_CURVE('',#13555,#13553,#11009,.T.);
#17402=EDGE_CURVE('',#13556,#13506,#7651,.T.);
#17403=EDGE_CURVE('',#13556,#13557,#7652,.T.);
#17404=EDGE_CURVE('',#13402,#13557,#7653,.T.);
#17405=EDGE_CURVE('',#13403,#13558,#7654,.T.);
#17406=EDGE_CURVE('',#13557,#13558,#7655,.T.);
#17407=EDGE_CURVE('',#13558,#13559,#11010,.T.);
#17408=EDGE_CURVE('',#13559,#13556,#11011,.T.);
#17409=EDGE_CURVE('',#13560,#13404,#7656,.T.);
#17410=EDGE_CURVE('',#13560,#13561,#7657,.T.);
#17411=EDGE_CURVE('',#13405,#13561,#7658,.T.);
#17412=EDGE_CURVE('',#13406,#13562,#7659,.T.);
#17413=EDGE_CURVE('',#13561,#13562,#7660,.T.);
#17414=EDGE_CURVE('',#13562,#13560,#11012,.T.);
#17415=EDGE_CURVE('',#13563,#13407,#7661,.T.);
#17416=EDGE_CURVE('',#13563,#13564,#7662,.T.);
#17417=EDGE_CURVE('',#13408,#13564,#7663,.T.);
#17418=EDGE_CURVE('',#13409,#13565,#7664,.T.);
#17419=EDGE_CURVE('',#13564,#13565,#7665,.T.);
#17420=EDGE_CURVE('',#13565,#13563,#11013,.T.);
#17421=EDGE_CURVE('',#13566,#13410,#7666,.T.);
#17422=EDGE_CURVE('',#13566,#13567,#7667,.T.);
#17423=EDGE_CURVE('',#13411,#13567,#7668,.T.);
#17424=EDGE_CURVE('',#13412,#13568,#7669,.T.);
#17425=EDGE_CURVE('',#13567,#13568,#7670,.T.);
#17426=EDGE_CURVE('',#13568,#13566,#11014,.T.);
#17427=EDGE_CURVE('',#13569,#13413,#7671,.T.);
#17428=EDGE_CURVE('',#13569,#13570,#7672,.T.);
#17429=EDGE_CURVE('',#13414,#13570,#7673,.T.);
#17430=EDGE_CURVE('',#13415,#13571,#7674,.T.);
#17431=EDGE_CURVE('',#13570,#13571,#7675,.T.);
#17432=EDGE_CURVE('',#13571,#13569,#11015,.T.);
#17433=EDGE_CURVE('',#13572,#13416,#7676,.T.);
#17434=EDGE_CURVE('',#13572,#13573,#7677,.T.);
#17435=EDGE_CURVE('',#13417,#13573,#7678,.T.);
#17436=EDGE_CURVE('',#13418,#13574,#7679,.T.);
#17437=EDGE_CURVE('',#13573,#13574,#7680,.T.);
#17438=EDGE_CURVE('',#13574,#13572,#11016,.T.);
#17439=EDGE_CURVE('',#13575,#13419,#7681,.T.);
#17440=EDGE_CURVE('',#13575,#13576,#7682,.T.);
#17441=EDGE_CURVE('',#13420,#13576,#7683,.T.);
#17442=EDGE_CURVE('',#13421,#13577,#7684,.T.);
#17443=EDGE_CURVE('',#13576,#13577,#7685,.T.);
#17444=EDGE_CURVE('',#13577,#13575,#11017,.T.);
#17445=EDGE_CURVE('',#13578,#13422,#7686,.T.);
#17446=EDGE_CURVE('',#13578,#13579,#7687,.T.);
#17447=EDGE_CURVE('',#13423,#13579,#7688,.T.);
#17448=EDGE_CURVE('',#13424,#13580,#7689,.T.);
#17449=EDGE_CURVE('',#13579,#13580,#7690,.T.);
#17450=EDGE_CURVE('',#13580,#13578,#11018,.T.);
#17451=EDGE_CURVE('',#13581,#13425,#7691,.T.);
#17452=EDGE_CURVE('',#13581,#13582,#7692,.T.);
#17453=EDGE_CURVE('',#13426,#13582,#7693,.T.);
#17454=EDGE_CURVE('',#13427,#13583,#7694,.T.);
#17455=EDGE_CURVE('',#13582,#13583,#7695,.T.);
#17456=EDGE_CURVE('',#13583,#13581,#11019,.T.);
#17457=EDGE_CURVE('',#13584,#13428,#7696,.T.);
#17458=EDGE_CURVE('',#13584,#13585,#7697,.T.);
#17459=EDGE_CURVE('',#13429,#13585,#7698,.T.);
#17460=EDGE_CURVE('',#13430,#13586,#7699,.T.);
#17461=EDGE_CURVE('',#13585,#13586,#7700,.T.);
#17462=EDGE_CURVE('',#13586,#13584,#11020,.T.);
#17463=EDGE_CURVE('',#13587,#13431,#7701,.T.);
#17464=EDGE_CURVE('',#13587,#13588,#7702,.T.);
#17465=EDGE_CURVE('',#13432,#13588,#7703,.T.);
#17466=EDGE_CURVE('',#13433,#13589,#7704,.T.);
#17467=EDGE_CURVE('',#13588,#13589,#7705,.T.);
#17468=EDGE_CURVE('',#13589,#13587,#11021,.T.);
#17469=EDGE_CURVE('',#13590,#13434,#7706,.T.);
#17470=EDGE_CURVE('',#13590,#13591,#7707,.T.);
#17471=EDGE_CURVE('',#13435,#13591,#7708,.T.);
#17472=EDGE_CURVE('',#13436,#13592,#7709,.T.);
#17473=EDGE_CURVE('',#13591,#13592,#7710,.T.);
#17474=EDGE_CURVE('',#13592,#13590,#11022,.T.);
#17475=EDGE_CURVE('',#13593,#13437,#7711,.T.);
#17476=EDGE_CURVE('',#13593,#13594,#7712,.T.);
#17477=EDGE_CURVE('',#13438,#13594,#7713,.T.);
#17478=EDGE_CURVE('',#13439,#13595,#7714,.T.);
#17479=EDGE_CURVE('',#13594,#13595,#7715,.T.);
#17480=EDGE_CURVE('',#13595,#13593,#11023,.T.);
#17481=EDGE_CURVE('',#13596,#13440,#7716,.T.);
#17482=EDGE_CURVE('',#13596,#13597,#7717,.T.);
#17483=EDGE_CURVE('',#13441,#13597,#7718,.T.);
#17484=EDGE_CURVE('',#13442,#13598,#7719,.T.);
#17485=EDGE_CURVE('',#13597,#13598,#7720,.T.);
#17486=EDGE_CURVE('',#13598,#13596,#11024,.T.);
#17487=EDGE_CURVE('',#13599,#13443,#7721,.T.);
#17488=EDGE_CURVE('',#13599,#13600,#7722,.T.);
#17489=EDGE_CURVE('',#13444,#13600,#7723,.T.);
#17490=EDGE_CURVE('',#13445,#13601,#7724,.T.);
#17491=EDGE_CURVE('',#13600,#13601,#7725,.T.);
#17492=EDGE_CURVE('',#13601,#13599,#11025,.T.);
#17493=EDGE_CURVE('',#13602,#13446,#7726,.T.);
#17494=EDGE_CURVE('',#13602,#13603,#7727,.T.);
#17495=EDGE_CURVE('',#13447,#13603,#7728,.T.);
#17496=EDGE_CURVE('',#13448,#13604,#7729,.T.);
#17497=EDGE_CURVE('',#13603,#13604,#7730,.T.);
#17498=EDGE_CURVE('',#13604,#13602,#11026,.T.);
#17499=EDGE_CURVE('',#13605,#13449,#7731,.T.);
#17500=EDGE_CURVE('',#13605,#13606,#7732,.T.);
#17501=EDGE_CURVE('',#13450,#13606,#7733,.T.);
#17502=EDGE_CURVE('',#13451,#13607,#7734,.T.);
#17503=EDGE_CURVE('',#13606,#13607,#7735,.T.);
#17504=EDGE_CURVE('',#13607,#13605,#11027,.T.);
#17505=EDGE_CURVE('',#13608,#13452,#7736,.T.);
#17506=EDGE_CURVE('',#13608,#13609,#7737,.T.);
#17507=EDGE_CURVE('',#13453,#13609,#7738,.T.);
#17508=EDGE_CURVE('',#13454,#13610,#7739,.T.);
#17509=EDGE_CURVE('',#13609,#13610,#7740,.T.);
#17510=EDGE_CURVE('',#13610,#13608,#11028,.T.);
#17511=EDGE_CURVE('',#13611,#13455,#7741,.T.);
#17512=EDGE_CURVE('',#13611,#13612,#7742,.T.);
#17513=EDGE_CURVE('',#13456,#13612,#7743,.T.);
#17514=EDGE_CURVE('',#13457,#13613,#7744,.T.);
#17515=EDGE_CURVE('',#13612,#13613,#7745,.T.);
#17516=EDGE_CURVE('',#13613,#13611,#11029,.T.);
#17517=EDGE_CURVE('',#13559,#13394,#7746,.T.);
#17518=EDGE_CURVE('',#13614,#13615,#7747,.T.);
#17519=EDGE_CURVE('',#13615,#13616,#7748,.T.);
#17520=EDGE_CURVE('',#13616,#13617,#7749,.T.);
#17521=EDGE_CURVE('',#13617,#13618,#7750,.T.);
#17522=EDGE_CURVE('',#13618,#13619,#7751,.T.);
#17523=EDGE_CURVE('',#13619,#13614,#7752,.T.);
#17524=EDGE_CURVE('',#13620,#13621,#7753,.T.);
#17525=EDGE_CURVE('',#13620,#13621,#11030,.T.);
#17526=EDGE_CURVE('',#13621,#13622,#7754,.T.);
#17527=EDGE_CURVE('',#13621,#13622,#11031,.T.);
#17528=EDGE_CURVE('',#13622,#13623,#7755,.T.);
#17529=EDGE_CURVE('',#13622,#13623,#11032,.T.);
#17530=EDGE_CURVE('',#13623,#13624,#7756,.T.);
#17531=EDGE_CURVE('',#13623,#13624,#11033,.T.);
#17532=EDGE_CURVE('',#13624,#13625,#7757,.T.);
#17533=EDGE_CURVE('',#13624,#13625,#11034,.T.);
#17534=EDGE_CURVE('',#13625,#13620,#7758,.T.);
#17535=EDGE_CURVE('',#13625,#13620,#11035,.T.);
#17536=EDGE_CURVE('',#13626,#13620,#7759,.T.);
#17537=EDGE_CURVE('',#13614,#13620,#7760,.T.);
#17538=EDGE_CURVE('',#13615,#13621,#7761,.T.);
#17539=EDGE_CURVE('',#13619,#13625,#7762,.T.);
#17540=EDGE_CURVE('',#13618,#13624,#7763,.T.);
#17541=EDGE_CURVE('',#13617,#13623,#7764,.T.);
#17542=EDGE_CURVE('',#13616,#13622,#7765,.T.);
#17543=EDGE_CURVE('',#13627,#13627,#11036,.T.);
#17544=EDGE_CURVE('',#13627,#13628,#7766,.T.);
#17545=EDGE_CURVE('',#13628,#13628,#11037,.T.);
#17546=EDGE_CURVE('',#13629,#13629,#11038,.T.);
#17547=EDGE_CURVE('',#13630,#13630,#11039,.T.);
#17548=EDGE_CURVE('',#13630,#13629,#7767,.T.);
#17549=EDGE_CURVE('',#13630,#13631,#7768,.T.);
#17550=EDGE_CURVE('',#13631,#13631,#11040,.T.);
#17551=EDGE_CURVE('',#13632,#13632,#11041,.T.);
#17552=EDGE_CURVE('',#13627,#13632,#7769,.T.);
#17553=EDGE_CURVE('',#13633,#13633,#11042,.T.);
#17554=EDGE_CURVE('',#13633,#13634,#7770,.T.);
#17555=EDGE_CURVE('',#13634,#13634,#11043,.T.);
#17556=EDGE_CURVE('',#13633,#13635,#7771,.T.);
#17557=EDGE_CURVE('',#13635,#13635,#11044,.T.);
#17558=EDGE_CURVE('',#13636,#13636,#11045,.T.);
#17559=EDGE_CURVE('',#13637,#13637,#11046,.T.);
#17560=EDGE_CURVE('',#13637,#13638,#7772,.T.);
#17561=EDGE_CURVE('',#13638,#13638,#11047,.T.);
#17562=EDGE_CURVE('',#13637,#13639,#7773,.T.);
#17563=EDGE_CURVE('',#13639,#13639,#11048,.T.);
#17564=EDGE_CURVE('',#13640,#13640,#11049,.T.);
#17565=EDGE_CURVE('',#13641,#13641,#11050,.T.);
#17566=EDGE_CURVE('',#13641,#13640,#7774,.T.);
#17567=EDGE_CURVE('',#13642,#13643,#497,.T.);
#17568=EDGE_CURVE('',#13644,#13642,#498,.T.);
#17569=EDGE_CURVE('',#13645,#13644,#499,.T.);
#17570=EDGE_CURVE('',#13646,#13645,#500,.T.);
#17571=EDGE_CURVE('',#13647,#13646,#501,.T.);
#17572=EDGE_CURVE('',#13643,#13647,#502,.T.);
#17573=EDGE_CURVE('',#13643,#13636,#7775,.T.);
#17574=EDGE_CURVE('',#13648,#13643,#7776,.T.);
#17575=EDGE_CURVE('',#13649,#13648,#7777,.T.);
#17576=EDGE_CURVE('',#13649,#13642,#7778,.T.);
#17577=EDGE_CURVE('',#13650,#13647,#7779,.T.);
#17578=EDGE_CURVE('',#13648,#13650,#7780,.T.);
#17579=EDGE_CURVE('',#13651,#13646,#7781,.T.);
#17580=EDGE_CURVE('',#13650,#13651,#7782,.T.);
#17581=EDGE_CURVE('',#13652,#13645,#7783,.T.);
#17582=EDGE_CURVE('',#13651,#13652,#7784,.T.);
#17583=EDGE_CURVE('',#13653,#13644,#7785,.T.);
#17584=EDGE_CURVE('',#13652,#13653,#7786,.T.);
#17585=EDGE_CURVE('',#13653,#13649,#7787,.T.);
#17586=ORIENTED_EDGE('',*,*,#13654,.T.);
#17587=ORIENTED_EDGE('',*,*,#13655,.T.);
#17588=ORIENTED_EDGE('',*,*,#13656,.T.);
#17589=ORIENTED_EDGE('',*,*,#13655,.F.);
#17590=ORIENTED_EDGE('',*,*,#13654,.F.);
#17591=ORIENTED_EDGE('',*,*,#13657,.T.);
#17592=ORIENTED_EDGE('',*,*,#13658,.T.);
#17593=ORIENTED_EDGE('',*,*,#13659,.T.);
#17594=ORIENTED_EDGE('',*,*,#13657,.F.);
#17595=ORIENTED_EDGE('',*,*,#13660,.F.);
#17596=ORIENTED_EDGE('',*,*,#13661,.F.);
#17597=ORIENTED_EDGE('',*,*,#13662,.F.);
#17598=ORIENTED_EDGE('',*,*,#13663,.T.);
#17599=ORIENTED_EDGE('',*,*,#13656,.F.);
#17600=ORIENTED_EDGE('',*,*,#13664,.T.);
#17601=ORIENTED_EDGE('',*,*,#13665,.T.);
#17602=ORIENTED_EDGE('',*,*,#13666,.T.);
#17603=ORIENTED_EDGE('',*,*,#13665,.F.);
#17604=ORIENTED_EDGE('',*,*,#13664,.F.);
#17605=ORIENTED_EDGE('',*,*,#13667,.T.);
#17606=ORIENTED_EDGE('',*,*,#13668,.T.);
#17607=ORIENTED_EDGE('',*,*,#13669,.T.);
#17608=ORIENTED_EDGE('',*,*,#13667,.F.);
#17609=ORIENTED_EDGE('',*,*,#13670,.F.);
#17610=ORIENTED_EDGE('',*,*,#13671,.T.);
#17611=ORIENTED_EDGE('',*,*,#13672,.F.);
#17612=ORIENTED_EDGE('',*,*,#13673,.T.);
#17613=ORIENTED_EDGE('',*,*,#13666,.F.);
#17614=ORIENTED_EDGE('',*,*,#13674,.T.);
#17615=ORIENTED_EDGE('',*,*,#13658,.F.);
#17616=ORIENTED_EDGE('',*,*,#13659,.F.);
#17617=ORIENTED_EDGE('',*,*,#13674,.F.);
#17618=ORIENTED_EDGE('',*,*,#13675,.T.);
#17619=ORIENTED_EDGE('',*,*,#13668,.F.);
#17620=ORIENTED_EDGE('',*,*,#13669,.F.);
#17621=ORIENTED_EDGE('',*,*,#13675,.F.);
#17622=ORIENTED_EDGE('',*,*,#13676,.T.);
#17623=ORIENTED_EDGE('',*,*,#13677,.T.);
#17624=ORIENTED_EDGE('',*,*,#13678,.T.);
#17625=ORIENTED_EDGE('',*,*,#13677,.F.);
#17626=ORIENTED_EDGE('',*,*,#13676,.F.);
#17627=ORIENTED_EDGE('',*,*,#13679,.T.);
#17628=ORIENTED_EDGE('',*,*,#13680,.T.);
#17629=ORIENTED_EDGE('',*,*,#13681,.T.);
#17630=ORIENTED_EDGE('',*,*,#13679,.F.);
#17631=ORIENTED_EDGE('',*,*,#13682,.F.);
#17632=ORIENTED_EDGE('',*,*,#13683,.T.);
#17633=ORIENTED_EDGE('',*,*,#13684,.F.);
#17634=ORIENTED_EDGE('',*,*,#13685,.T.);
#17635=ORIENTED_EDGE('',*,*,#13678,.F.);
#17636=ORIENTED_EDGE('',*,*,#13686,.T.);
#17637=ORIENTED_EDGE('',*,*,#13687,.T.);
#17638=ORIENTED_EDGE('',*,*,#13688,.T.);
#17639=ORIENTED_EDGE('',*,*,#13687,.F.);
#17640=ORIENTED_EDGE('',*,*,#13686,.F.);
#17641=ORIENTED_EDGE('',*,*,#13689,.T.);
#17642=ORIENTED_EDGE('',*,*,#13690,.T.);
#17643=ORIENTED_EDGE('',*,*,#13691,.T.);
#17644=ORIENTED_EDGE('',*,*,#13689,.F.);
#17645=ORIENTED_EDGE('',*,*,#13692,.F.);
#17646=ORIENTED_EDGE('',*,*,#13693,.F.);
#17647=ORIENTED_EDGE('',*,*,#13694,.F.);
#17648=ORIENTED_EDGE('',*,*,#13695,.T.);
#17649=ORIENTED_EDGE('',*,*,#13688,.F.);
#17650=ORIENTED_EDGE('',*,*,#13696,.T.);
#17651=ORIENTED_EDGE('',*,*,#13680,.F.);
#17652=ORIENTED_EDGE('',*,*,#13681,.F.);
#17653=ORIENTED_EDGE('',*,*,#13696,.F.);
#17654=ORIENTED_EDGE('',*,*,#13697,.T.);
#17655=ORIENTED_EDGE('',*,*,#13690,.F.);
#17656=ORIENTED_EDGE('',*,*,#13691,.F.);
#17657=ORIENTED_EDGE('',*,*,#13697,.F.);
#17658=ORIENTED_EDGE('',*,*,#13698,.F.);
#17659=ORIENTED_EDGE('',*,*,#13699,.T.);
#17660=ORIENTED_EDGE('',*,*,#13700,.F.);
#17661=ORIENTED_EDGE('',*,*,#13699,.F.);
#17662=ORIENTED_EDGE('',*,*,#13701,.F.);
#17663=ORIENTED_EDGE('',*,*,#13702,.T.);
#17664=ORIENTED_EDGE('',*,*,#13703,.F.);
#17665=ORIENTED_EDGE('',*,*,#13702,.F.);
#17666=ORIENTED_EDGE('',*,*,#13704,.F.);
#17667=ORIENTED_EDGE('',*,*,#13705,.T.);
#17668=ORIENTED_EDGE('',*,*,#13706,.F.);
#17669=ORIENTED_EDGE('',*,*,#13705,.F.);
#17670=ORIENTED_EDGE('',*,*,#13707,.F.);
#17671=ORIENTED_EDGE('',*,*,#13708,.T.);
#17672=ORIENTED_EDGE('',*,*,#13709,.F.);
#17673=ORIENTED_EDGE('',*,*,#13708,.F.);
#17674=ORIENTED_EDGE('',*,*,#13710,.T.);
#17675=ORIENTED_EDGE('',*,*,#13711,.T.);
#17676=ORIENTED_EDGE('',*,*,#13712,.T.);
#17677=ORIENTED_EDGE('',*,*,#13711,.F.);
#17678=ORIENTED_EDGE('',*,*,#13713,.F.);
#17679=ORIENTED_EDGE('',*,*,#13714,.F.);
#17680=ORIENTED_EDGE('',*,*,#13715,.F.);
#17681=ORIENTED_EDGE('',*,*,#13716,.F.);
#17682=ORIENTED_EDGE('',*,*,#13717,.F.);
#17683=ORIENTED_EDGE('',*,*,#13718,.F.);
#17684=ORIENTED_EDGE('',*,*,#13719,.F.);
#17685=ORIENTED_EDGE('',*,*,#13720,.F.);
#17686=ORIENTED_EDGE('',*,*,#13721,.F.);
#17687=ORIENTED_EDGE('',*,*,#13722,.F.);
#17688=ORIENTED_EDGE('',*,*,#13723,.F.);
#17689=ORIENTED_EDGE('',*,*,#13724,.F.);
#17690=ORIENTED_EDGE('',*,*,#13725,.F.);
#17691=ORIENTED_EDGE('',*,*,#13726,.F.);
#17692=ORIENTED_EDGE('',*,*,#13727,.F.);
#17693=ORIENTED_EDGE('',*,*,#13728,.F.);
#17694=ORIENTED_EDGE('',*,*,#13729,.F.);
#17695=ORIENTED_EDGE('',*,*,#13730,.F.);
#17696=ORIENTED_EDGE('',*,*,#13731,.F.);
#17697=ORIENTED_EDGE('',*,*,#13732,.F.);
#17698=ORIENTED_EDGE('',*,*,#13712,.F.);
#17699=ORIENTED_EDGE('',*,*,#13733,.F.);
#17700=ORIENTED_EDGE('',*,*,#13734,.F.);
#17701=ORIENTED_EDGE('',*,*,#13735,.F.);
#17702=ORIENTED_EDGE('',*,*,#13736,.F.);
#17703=ORIENTED_EDGE('',*,*,#13707,.T.);
#17704=ORIENTED_EDGE('',*,*,#13704,.T.);
#17705=ORIENTED_EDGE('',*,*,#13701,.T.);
#17706=ORIENTED_EDGE('',*,*,#13698,.T.);
#17707=ORIENTED_EDGE('',*,*,#13710,.F.);
#17708=ORIENTED_EDGE('',*,*,#13737,.T.);
#17709=ORIENTED_EDGE('',*,*,#13738,.F.);
#17710=ORIENTED_EDGE('',*,*,#13737,.F.);
#17711=ORIENTED_EDGE('',*,*,#13739,.T.);
#17712=ORIENTED_EDGE('',*,*,#13740,.T.);
#17713=ORIENTED_EDGE('',*,*,#13736,.T.);
#17714=ORIENTED_EDGE('',*,*,#13740,.F.);
#17715=ORIENTED_EDGE('',*,*,#13739,.F.);
#17716=ORIENTED_EDGE('',*,*,#13741,.T.);
#17717=ORIENTED_EDGE('',*,*,#13742,.F.);
#17718=ORIENTED_EDGE('',*,*,#13741,.F.);
#17719=ORIENTED_EDGE('',*,*,#13743,.T.);
#17720=ORIENTED_EDGE('',*,*,#13744,.T.);
#17721=ORIENTED_EDGE('',*,*,#13733,.T.);
#17722=ORIENTED_EDGE('',*,*,#13744,.F.);
#17723=ORIENTED_EDGE('',*,*,#13743,.F.);
#17724=ORIENTED_EDGE('',*,*,#13745,.T.);
#17725=ORIENTED_EDGE('',*,*,#13746,.F.);
#17726=ORIENTED_EDGE('',*,*,#13745,.F.);
#17727=ORIENTED_EDGE('',*,*,#13747,.T.);
#17728=ORIENTED_EDGE('',*,*,#13748,.T.);
#17729=ORIENTED_EDGE('',*,*,#13735,.T.);
#17730=ORIENTED_EDGE('',*,*,#13748,.F.);
#17731=ORIENTED_EDGE('',*,*,#13747,.F.);
#17732=ORIENTED_EDGE('',*,*,#13749,.T.);
#17733=ORIENTED_EDGE('',*,*,#13750,.F.);
#17734=ORIENTED_EDGE('',*,*,#13749,.F.);
#17735=ORIENTED_EDGE('',*,*,#13751,.T.);
#17736=ORIENTED_EDGE('',*,*,#13752,.T.);
#17737=ORIENTED_EDGE('',*,*,#13734,.T.);
#17738=ORIENTED_EDGE('',*,*,#13752,.F.);
#17739=ORIENTED_EDGE('',*,*,#13751,.F.);
#17740=ORIENTED_EDGE('',*,*,#13753,.T.);
#17741=ORIENTED_EDGE('',*,*,#13754,.F.);
#17742=ORIENTED_EDGE('',*,*,#13753,.F.);
#17743=ORIENTED_EDGE('',*,*,#13723,.T.);
#17744=ORIENTED_EDGE('',*,*,#13755,.T.);
#17745=ORIENTED_EDGE('',*,*,#13756,.T.);
#17746=ORIENTED_EDGE('',*,*,#13757,.T.);
#17747=ORIENTED_EDGE('',*,*,#13722,.T.);
#17748=ORIENTED_EDGE('',*,*,#13758,.T.);
#17749=ORIENTED_EDGE('',*,*,#13759,.T.);
#17750=ORIENTED_EDGE('',*,*,#13755,.F.);
#17751=ORIENTED_EDGE('',*,*,#13721,.T.);
#17752=ORIENTED_EDGE('',*,*,#13760,.T.);
#17753=ORIENTED_EDGE('',*,*,#13670,.T.);
#17754=ORIENTED_EDGE('',*,*,#13758,.F.);
#17755=ORIENTED_EDGE('',*,*,#13761,.T.);
#17756=ORIENTED_EDGE('',*,*,#13762,.T.);
#17757=ORIENTED_EDGE('',*,*,#13729,.T.);
#17758=ORIENTED_EDGE('',*,*,#13763,.T.);
#17759=ORIENTED_EDGE('',*,*,#13720,.T.);
#17760=ORIENTED_EDGE('',*,*,#13764,.T.);
#17761=ORIENTED_EDGE('',*,*,#13765,.T.);
#17762=ORIENTED_EDGE('',*,*,#13760,.F.);
#17763=ORIENTED_EDGE('',*,*,#13718,.T.);
#17764=ORIENTED_EDGE('',*,*,#13766,.T.);
#17765=ORIENTED_EDGE('',*,*,#13767,.T.);
#17766=ORIENTED_EDGE('',*,*,#13768,.T.);
#17767=ORIENTED_EDGE('',*,*,#13717,.T.);
#17768=ORIENTED_EDGE('',*,*,#13769,.T.);
#17769=ORIENTED_EDGE('',*,*,#13660,.T.);
#17770=ORIENTED_EDGE('',*,*,#13766,.F.);
#17771=ORIENTED_EDGE('',*,*,#13770,.T.);
#17772=ORIENTED_EDGE('',*,*,#13771,.T.);
#17773=ORIENTED_EDGE('',*,*,#13713,.T.);
#17774=ORIENTED_EDGE('',*,*,#13772,.T.);
#17775=ORIENTED_EDGE('',*,*,#13716,.T.);
#17776=ORIENTED_EDGE('',*,*,#13773,.T.);
#17777=ORIENTED_EDGE('',*,*,#13774,.T.);
#17778=ORIENTED_EDGE('',*,*,#13769,.F.);
#17779=ORIENTED_EDGE('',*,*,#13775,.T.);
#17780=ORIENTED_EDGE('',*,*,#13776,.T.);
#17781=ORIENTED_EDGE('',*,*,#13714,.T.);
#17782=ORIENTED_EDGE('',*,*,#13771,.F.);
#17783=ORIENTED_EDGE('',*,*,#13715,.T.);
#17784=ORIENTED_EDGE('',*,*,#13776,.F.);
#17785=ORIENTED_EDGE('',*,*,#13777,.T.);
#17786=ORIENTED_EDGE('',*,*,#13773,.F.);
#17787=ORIENTED_EDGE('',*,*,#13778,.T.);
#17788=ORIENTED_EDGE('',*,*,#13772,.F.);
#17789=ORIENTED_EDGE('',*,*,#13732,.T.);
#17790=ORIENTED_EDGE('',*,*,#13779,.T.);
#17791=ORIENTED_EDGE('',*,*,#13682,.T.);
#17792=ORIENTED_EDGE('',*,*,#13779,.F.);
#17793=ORIENTED_EDGE('',*,*,#13731,.T.);
#17794=ORIENTED_EDGE('',*,*,#13780,.T.);
#17795=ORIENTED_EDGE('',*,*,#13719,.T.);
#17796=ORIENTED_EDGE('',*,*,#13768,.F.);
#17797=ORIENTED_EDGE('',*,*,#13781,.T.);
#17798=ORIENTED_EDGE('',*,*,#13764,.F.);
#17799=ORIENTED_EDGE('',*,*,#13782,.T.);
#17800=ORIENTED_EDGE('',*,*,#13780,.F.);
#17801=ORIENTED_EDGE('',*,*,#13730,.T.);
#17802=ORIENTED_EDGE('',*,*,#13762,.F.);
#17803=ORIENTED_EDGE('',*,*,#13783,.T.);
#17804=ORIENTED_EDGE('',*,*,#13763,.F.);
#17805=ORIENTED_EDGE('',*,*,#13728,.T.);
#17806=ORIENTED_EDGE('',*,*,#13784,.T.);
#17807=ORIENTED_EDGE('',*,*,#13692,.T.);
#17808=ORIENTED_EDGE('',*,*,#13784,.F.);
#17809=ORIENTED_EDGE('',*,*,#13727,.T.);
#17810=ORIENTED_EDGE('',*,*,#13785,.T.);
#17811=ORIENTED_EDGE('',*,*,#13786,.T.);
#17812=ORIENTED_EDGE('',*,*,#13785,.F.);
#17813=ORIENTED_EDGE('',*,*,#13726,.T.);
#17814=ORIENTED_EDGE('',*,*,#13787,.T.);
#17815=ORIENTED_EDGE('',*,*,#13724,.T.);
#17816=ORIENTED_EDGE('',*,*,#13757,.F.);
#17817=ORIENTED_EDGE('',*,*,#13788,.T.);
#17818=ORIENTED_EDGE('',*,*,#13789,.T.);
#17819=ORIENTED_EDGE('',*,*,#13725,.T.);
#17820=ORIENTED_EDGE('',*,*,#13789,.F.);
#17821=ORIENTED_EDGE('',*,*,#13790,.T.);
#17822=ORIENTED_EDGE('',*,*,#13787,.F.);
#17823=ORIENTED_EDGE('',*,*,#13759,.F.);
#17824=ORIENTED_EDGE('',*,*,#13673,.F.);
#17825=ORIENTED_EDGE('',*,*,#13791,.F.);
#17826=ORIENTED_EDGE('',*,*,#13792,.T.);
#17827=ORIENTED_EDGE('',*,*,#13765,.F.);
#17828=ORIENTED_EDGE('',*,*,#13793,.F.);
#17829=ORIENTED_EDGE('',*,*,#13794,.F.);
#17830=ORIENTED_EDGE('',*,*,#13671,.F.);
#17831=ORIENTED_EDGE('',*,*,#13781,.F.);
#17832=ORIENTED_EDGE('',*,*,#13795,.F.);
#17833=ORIENTED_EDGE('',*,*,#13796,.F.);
#17834=ORIENTED_EDGE('',*,*,#13793,.T.);
#17835=ORIENTED_EDGE('',*,*,#13767,.F.);
#17836=ORIENTED_EDGE('',*,*,#13663,.F.);
#17837=ORIENTED_EDGE('',*,*,#13797,.F.);
#17838=ORIENTED_EDGE('',*,*,#13795,.T.);
#17839=ORIENTED_EDGE('',*,*,#13774,.F.);
#17840=ORIENTED_EDGE('',*,*,#13798,.T.);
#17841=ORIENTED_EDGE('',*,*,#13799,.F.);
#17842=ORIENTED_EDGE('',*,*,#13661,.T.);
#17843=ORIENTED_EDGE('',*,*,#13777,.F.);
#17844=ORIENTED_EDGE('',*,*,#13800,.F.);
#17845=ORIENTED_EDGE('',*,*,#13801,.F.);
#17846=ORIENTED_EDGE('',*,*,#13798,.F.);
#17847=ORIENTED_EDGE('',*,*,#13775,.F.);
#17848=ORIENTED_EDGE('',*,*,#13802,.F.);
#17849=ORIENTED_EDGE('',*,*,#13803,.F.);
#17850=ORIENTED_EDGE('',*,*,#13800,.T.);
#17851=ORIENTED_EDGE('',*,*,#13770,.F.);
#17852=ORIENTED_EDGE('',*,*,#13804,.F.);
#17853=ORIENTED_EDGE('',*,*,#13805,.F.);
#17854=ORIENTED_EDGE('',*,*,#13802,.T.);
#17855=ORIENTED_EDGE('',*,*,#13790,.F.);
#17856=ORIENTED_EDGE('',*,*,#13806,.F.);
#17857=ORIENTED_EDGE('',*,*,#13807,.F.);
#17858=ORIENTED_EDGE('',*,*,#13808,.F.);
#17859=ORIENTED_EDGE('',*,*,#13756,.F.);
#17860=ORIENTED_EDGE('',*,*,#13792,.F.);
#17861=ORIENTED_EDGE('',*,*,#13809,.F.);
#17862=ORIENTED_EDGE('',*,*,#13810,.T.);
#17863=ORIENTED_EDGE('',*,*,#13788,.F.);
#17864=ORIENTED_EDGE('',*,*,#13810,.F.);
#17865=ORIENTED_EDGE('',*,*,#13811,.F.);
#17866=ORIENTED_EDGE('',*,*,#13806,.T.);
#17867=ORIENTED_EDGE('',*,*,#13778,.F.);
#17868=ORIENTED_EDGE('',*,*,#13685,.F.);
#17869=ORIENTED_EDGE('',*,*,#13812,.F.);
#17870=ORIENTED_EDGE('',*,*,#13804,.T.);
#17871=ORIENTED_EDGE('',*,*,#13786,.F.);
#17872=ORIENTED_EDGE('',*,*,#13808,.T.);
#17873=ORIENTED_EDGE('',*,*,#13813,.F.);
#17874=ORIENTED_EDGE('',*,*,#13693,.T.);
#17875=ORIENTED_EDGE('',*,*,#13801,.T.);
#17876=ORIENTED_EDGE('',*,*,#13803,.T.);
#17877=ORIENTED_EDGE('',*,*,#13805,.T.);
#17878=ORIENTED_EDGE('',*,*,#13812,.T.);
#17879=ORIENTED_EDGE('',*,*,#13684,.T.);
#17880=ORIENTED_EDGE('',*,*,#13814,.T.);
#17881=ORIENTED_EDGE('',*,*,#13815,.T.);
#17882=ORIENTED_EDGE('',*,*,#13816,.T.);
#17883=ORIENTED_EDGE('',*,*,#13694,.T.);
#17884=ORIENTED_EDGE('',*,*,#13813,.T.);
#17885=ORIENTED_EDGE('',*,*,#13807,.T.);
#17886=ORIENTED_EDGE('',*,*,#13811,.T.);
#17887=ORIENTED_EDGE('',*,*,#13809,.T.);
#17888=ORIENTED_EDGE('',*,*,#13791,.T.);
#17889=ORIENTED_EDGE('',*,*,#13672,.T.);
#17890=ORIENTED_EDGE('',*,*,#13794,.T.);
#17891=ORIENTED_EDGE('',*,*,#13796,.T.);
#17892=ORIENTED_EDGE('',*,*,#13797,.T.);
#17893=ORIENTED_EDGE('',*,*,#13662,.T.);
#17894=ORIENTED_EDGE('',*,*,#13799,.T.);
#17895=ORIENTED_EDGE('',*,*,#13750,.T.);
#17896=ORIENTED_EDGE('',*,*,#13746,.T.);
#17897=ORIENTED_EDGE('',*,*,#13742,.T.);
#17898=ORIENTED_EDGE('',*,*,#13738,.T.);
#17899=ORIENTED_EDGE('',*,*,#13754,.T.);
#17900=ORIENTED_EDGE('',*,*,#13709,.T.);
#17901=ORIENTED_EDGE('',*,*,#13706,.T.);
#17902=ORIENTED_EDGE('',*,*,#13703,.T.);
#17903=ORIENTED_EDGE('',*,*,#13700,.T.);
#17904=ORIENTED_EDGE('',*,*,#13761,.F.);
#17905=ORIENTED_EDGE('',*,*,#13817,.F.);
#17906=ORIENTED_EDGE('',*,*,#13815,.F.);
#17907=ORIENTED_EDGE('',*,*,#13818,.T.);
#17908=ORIENTED_EDGE('',*,*,#13782,.F.);
#17909=ORIENTED_EDGE('',*,*,#13818,.F.);
#17910=ORIENTED_EDGE('',*,*,#13814,.F.);
#17911=ORIENTED_EDGE('',*,*,#13683,.F.);
#17912=ORIENTED_EDGE('',*,*,#13783,.F.);
#17913=ORIENTED_EDGE('',*,*,#13695,.F.);
#17914=ORIENTED_EDGE('',*,*,#13816,.F.);
#17915=ORIENTED_EDGE('',*,*,#13817,.T.);
#17916=ORIENTED_EDGE('',*,*,#13819,.T.);
#17917=ORIENTED_EDGE('',*,*,#13820,.T.);
#17918=ORIENTED_EDGE('',*,*,#13821,.T.);
#17919=ORIENTED_EDGE('',*,*,#13820,.F.);
#17920=ORIENTED_EDGE('',*,*,#13822,.T.);
#17921=ORIENTED_EDGE('',*,*,#13823,.F.);
#17922=ORIENTED_EDGE('',*,*,#13824,.T.);
#17923=ORIENTED_EDGE('',*,*,#13825,.F.);
#17924=ORIENTED_EDGE('',*,*,#13826,.T.);
#17925=ORIENTED_EDGE('',*,*,#13827,.T.);
#17926=ORIENTED_EDGE('',*,*,#13828,.T.);
#17927=ORIENTED_EDGE('',*,*,#13829,.T.);
#17928=ORIENTED_EDGE('',*,*,#13830,.T.);
#17929=ORIENTED_EDGE('',*,*,#13831,.T.);
#17930=ORIENTED_EDGE('',*,*,#13832,.T.);
#17931=ORIENTED_EDGE('',*,*,#13833,.T.);
#17932=ORIENTED_EDGE('',*,*,#13834,.T.);
#17933=ORIENTED_EDGE('',*,*,#13835,.F.);
#17934=ORIENTED_EDGE('',*,*,#13836,.T.);
#17935=ORIENTED_EDGE('',*,*,#13837,.F.);
#17936=ORIENTED_EDGE('',*,*,#13838,.T.);
#17937=ORIENTED_EDGE('',*,*,#13839,.F.);
#17938=ORIENTED_EDGE('',*,*,#13840,.F.);
#17939=ORIENTED_EDGE('',*,*,#13841,.F.);
#17940=ORIENTED_EDGE('',*,*,#13842,.T.);
#17941=ORIENTED_EDGE('',*,*,#13843,.F.);
#17942=ORIENTED_EDGE('',*,*,#13844,.F.);
#17943=ORIENTED_EDGE('',*,*,#13845,.F.);
#17944=ORIENTED_EDGE('',*,*,#13846,.F.);
#17945=ORIENTED_EDGE('',*,*,#13847,.F.);
#17946=ORIENTED_EDGE('',*,*,#13848,.T.);
#17947=ORIENTED_EDGE('',*,*,#13849,.T.);
#17948=ORIENTED_EDGE('',*,*,#13850,.T.);
#17949=ORIENTED_EDGE('',*,*,#13851,.T.);
#17950=ORIENTED_EDGE('',*,*,#13852,.T.);
#17951=ORIENTED_EDGE('',*,*,#13853,.T.);
#17952=ORIENTED_EDGE('',*,*,#13854,.T.);
#17953=ORIENTED_EDGE('',*,*,#13855,.T.);
#17954=ORIENTED_EDGE('',*,*,#13856,.T.);
#17955=ORIENTED_EDGE('',*,*,#13857,.T.);
#17956=ORIENTED_EDGE('',*,*,#13858,.T.);
#17957=ORIENTED_EDGE('',*,*,#13859,.T.);
#17958=ORIENTED_EDGE('',*,*,#13860,.T.);
#17959=ORIENTED_EDGE('',*,*,#13861,.T.);
#17960=ORIENTED_EDGE('',*,*,#13862,.T.);
#17961=ORIENTED_EDGE('',*,*,#13863,.T.);
#17962=ORIENTED_EDGE('',*,*,#13864,.T.);
#17963=ORIENTED_EDGE('',*,*,#13865,.T.);
#17964=ORIENTED_EDGE('',*,*,#13866,.T.);
#17965=ORIENTED_EDGE('',*,*,#13867,.T.);
#17966=ORIENTED_EDGE('',*,*,#13868,.F.);
#17967=ORIENTED_EDGE('',*,*,#13821,.F.);
#17968=ORIENTED_EDGE('',*,*,#13869,.F.);
#17969=ORIENTED_EDGE('',*,*,#13870,.T.);
#17970=ORIENTED_EDGE('',*,*,#13819,.F.);
#17971=ORIENTED_EDGE('',*,*,#13870,.F.);
#17972=ORIENTED_EDGE('',*,*,#13871,.T.);
#17973=ORIENTED_EDGE('',*,*,#13872,.T.);
#17974=ORIENTED_EDGE('',*,*,#13846,.T.);
#17975=ORIENTED_EDGE('',*,*,#13872,.F.);
#17976=ORIENTED_EDGE('',*,*,#13873,.F.);
#17977=ORIENTED_EDGE('',*,*,#13874,.T.);
#17978=ORIENTED_EDGE('',*,*,#13871,.F.);
#17979=ORIENTED_EDGE('',*,*,#13874,.F.);
#17980=ORIENTED_EDGE('',*,*,#13875,.T.);
#17981=ORIENTED_EDGE('',*,*,#13876,.T.);
#17982=ORIENTED_EDGE('',*,*,#13868,.T.);
#17983=ORIENTED_EDGE('',*,*,#13876,.F.);
#17984=ORIENTED_EDGE('',*,*,#13877,.F.);
#17985=ORIENTED_EDGE('',*,*,#13878,.T.);
#17986=ORIENTED_EDGE('',*,*,#13875,.F.);
#17987=ORIENTED_EDGE('',*,*,#13878,.F.);
#17988=ORIENTED_EDGE('',*,*,#13879,.T.);
#17989=ORIENTED_EDGE('',*,*,#13880,.T.);
#17990=ORIENTED_EDGE('',*,*,#13847,.T.);
#17991=ORIENTED_EDGE('',*,*,#13880,.F.);
#17992=ORIENTED_EDGE('',*,*,#13881,.F.);
#17993=ORIENTED_EDGE('',*,*,#13882,.T.);
#17994=ORIENTED_EDGE('',*,*,#13879,.F.);
#17995=ORIENTED_EDGE('',*,*,#13882,.F.);
#17996=ORIENTED_EDGE('',*,*,#13883,.T.);
#17997=ORIENTED_EDGE('',*,*,#13884,.T.);
#17998=ORIENTED_EDGE('',*,*,#13885,.T.);
#17999=ORIENTED_EDGE('',*,*,#13884,.F.);
#18000=ORIENTED_EDGE('',*,*,#13886,.F.);
#18001=ORIENTED_EDGE('',*,*,#13887,.F.);
#18002=ORIENTED_EDGE('',*,*,#13888,.F.);
#18003=ORIENTED_EDGE('',*,*,#13889,.F.);
#18004=ORIENTED_EDGE('',*,*,#13890,.F.);
#18005=ORIENTED_EDGE('',*,*,#13891,.F.);
#18006=ORIENTED_EDGE('',*,*,#13892,.F.);
#18007=ORIENTED_EDGE('',*,*,#13893,.F.);
#18008=ORIENTED_EDGE('',*,*,#13894,.F.);
#18009=ORIENTED_EDGE('',*,*,#13895,.F.);
#18010=ORIENTED_EDGE('',*,*,#13896,.F.);
#18011=ORIENTED_EDGE('',*,*,#13897,.F.);
#18012=ORIENTED_EDGE('',*,*,#13898,.F.);
#18013=ORIENTED_EDGE('',*,*,#13899,.F.);
#18014=ORIENTED_EDGE('',*,*,#13900,.F.);
#18015=ORIENTED_EDGE('',*,*,#13901,.F.);
#18016=ORIENTED_EDGE('',*,*,#13902,.F.);
#18017=ORIENTED_EDGE('',*,*,#13903,.F.);
#18018=ORIENTED_EDGE('',*,*,#13904,.F.);
#18019=ORIENTED_EDGE('',*,*,#13905,.F.);
#18020=ORIENTED_EDGE('',*,*,#13906,.F.);
#18021=ORIENTED_EDGE('',*,*,#13907,.F.);
#18022=ORIENTED_EDGE('',*,*,#13908,.F.);
#18023=ORIENTED_EDGE('',*,*,#13909,.F.);
#18024=ORIENTED_EDGE('',*,*,#13885,.F.);
#18025=ORIENTED_EDGE('',*,*,#13910,.F.);
#18026=ORIENTED_EDGE('',*,*,#13911,.F.);
#18027=ORIENTED_EDGE('',*,*,#13912,.F.);
#18028=ORIENTED_EDGE('',*,*,#13913,.F.);
#18029=ORIENTED_EDGE('',*,*,#13914,.F.);
#18030=ORIENTED_EDGE('',*,*,#13915,.F.);
#18031=ORIENTED_EDGE('',*,*,#13916,.F.);
#18032=ORIENTED_EDGE('',*,*,#13917,.F.);
#18033=ORIENTED_EDGE('',*,*,#13918,.F.);
#18034=ORIENTED_EDGE('',*,*,#13919,.F.);
#18035=ORIENTED_EDGE('',*,*,#13920,.F.);
#18036=ORIENTED_EDGE('',*,*,#13921,.F.);
#18037=ORIENTED_EDGE('',*,*,#13922,.F.);
#18038=ORIENTED_EDGE('',*,*,#13923,.F.);
#18039=ORIENTED_EDGE('',*,*,#13924,.F.);
#18040=ORIENTED_EDGE('',*,*,#13925,.F.);
#18041=ORIENTED_EDGE('',*,*,#13926,.F.);
#18042=ORIENTED_EDGE('',*,*,#13927,.F.);
#18043=ORIENTED_EDGE('',*,*,#13928,.F.);
#18044=ORIENTED_EDGE('',*,*,#13869,.T.);
#18045=ORIENTED_EDGE('',*,*,#13873,.T.);
#18046=ORIENTED_EDGE('',*,*,#13877,.T.);
#18047=ORIENTED_EDGE('',*,*,#13881,.T.);
#18048=ORIENTED_EDGE('',*,*,#13883,.F.);
#18049=ORIENTED_EDGE('',*,*,#13929,.T.);
#18050=ORIENTED_EDGE('',*,*,#13851,.F.);
#18051=ORIENTED_EDGE('',*,*,#13929,.F.);
#18052=ORIENTED_EDGE('',*,*,#13930,.T.);
#18053=ORIENTED_EDGE('',*,*,#13931,.T.);
#18054=ORIENTED_EDGE('',*,*,#13928,.T.);
#18055=ORIENTED_EDGE('',*,*,#13931,.F.);
#18056=ORIENTED_EDGE('',*,*,#13930,.F.);
#18057=ORIENTED_EDGE('',*,*,#13932,.T.);
#18058=ORIENTED_EDGE('',*,*,#13850,.F.);
#18059=ORIENTED_EDGE('',*,*,#13932,.F.);
#18060=ORIENTED_EDGE('',*,*,#13933,.T.);
#18061=ORIENTED_EDGE('',*,*,#13934,.T.);
#18062=ORIENTED_EDGE('',*,*,#13910,.T.);
#18063=ORIENTED_EDGE('',*,*,#13934,.F.);
#18064=ORIENTED_EDGE('',*,*,#13933,.F.);
#18065=ORIENTED_EDGE('',*,*,#13935,.T.);
#18066=ORIENTED_EDGE('',*,*,#13849,.F.);
#18067=ORIENTED_EDGE('',*,*,#13935,.F.);
#18068=ORIENTED_EDGE('',*,*,#13936,.T.);
#18069=ORIENTED_EDGE('',*,*,#13937,.T.);
#18070=ORIENTED_EDGE('',*,*,#13927,.T.);
#18071=ORIENTED_EDGE('',*,*,#13937,.F.);
#18072=ORIENTED_EDGE('',*,*,#13936,.F.);
#18073=ORIENTED_EDGE('',*,*,#13938,.T.);
#18074=ORIENTED_EDGE('',*,*,#13848,.F.);
#18075=ORIENTED_EDGE('',*,*,#13938,.F.);
#18076=ORIENTED_EDGE('',*,*,#13906,.T.);
#18077=ORIENTED_EDGE('',*,*,#13939,.T.);
#18078=ORIENTED_EDGE('',*,*,#13940,.T.);
#18079=ORIENTED_EDGE('',*,*,#13941,.F.);
#18080=ORIENTED_EDGE('',*,*,#13905,.T.);
#18081=ORIENTED_EDGE('',*,*,#13942,.T.);
#18082=ORIENTED_EDGE('',*,*,#13943,.T.);
#18083=ORIENTED_EDGE('',*,*,#13939,.F.);
#18084=ORIENTED_EDGE('',*,*,#13904,.T.);
#18085=ORIENTED_EDGE('',*,*,#13944,.T.);
#18086=ORIENTED_EDGE('',*,*,#13945,.T.);
#18087=ORIENTED_EDGE('',*,*,#13942,.F.);
#18088=ORIENTED_EDGE('',*,*,#13903,.T.);
#18089=ORIENTED_EDGE('',*,*,#13946,.T.);
#18090=ORIENTED_EDGE('',*,*,#13947,.T.);
#18091=ORIENTED_EDGE('',*,*,#13944,.F.);
#18092=ORIENTED_EDGE('',*,*,#13948,.T.);
#18093=ORIENTED_EDGE('',*,*,#13949,.T.);
#18094=ORIENTED_EDGE('',*,*,#13898,.T.);
#18095=ORIENTED_EDGE('',*,*,#13950,.T.);
#18096=ORIENTED_EDGE('',*,*,#13897,.T.);
#18097=ORIENTED_EDGE('',*,*,#13951,.T.);
#18098=ORIENTED_EDGE('',*,*,#13952,.T.);
#18099=ORIENTED_EDGE('',*,*,#13950,.F.);
#18100=ORIENTED_EDGE('',*,*,#13896,.T.);
#18101=ORIENTED_EDGE('',*,*,#13953,.T.);
#18102=ORIENTED_EDGE('',*,*,#13954,.T.);
#18103=ORIENTED_EDGE('',*,*,#13951,.F.);
#18104=ORIENTED_EDGE('',*,*,#13895,.T.);
#18105=ORIENTED_EDGE('',*,*,#13955,.T.);
#18106=ORIENTED_EDGE('',*,*,#13956,.T.);
#18107=ORIENTED_EDGE('',*,*,#13953,.F.);
#18108=ORIENTED_EDGE('',*,*,#13894,.T.);
#18109=ORIENTED_EDGE('',*,*,#13957,.T.);
#18110=ORIENTED_EDGE('',*,*,#13958,.T.);
#18111=ORIENTED_EDGE('',*,*,#13955,.F.);
#18112=ORIENTED_EDGE('',*,*,#13959,.T.);
#18113=ORIENTED_EDGE('',*,*,#13957,.F.);
#18114=ORIENTED_EDGE('',*,*,#13893,.T.);
#18115=ORIENTED_EDGE('',*,*,#13960,.T.);
#18116=ORIENTED_EDGE('',*,*,#13961,.T.);
#18117=ORIENTED_EDGE('',*,*,#13960,.F.);
#18118=ORIENTED_EDGE('',*,*,#13892,.T.);
#18119=ORIENTED_EDGE('',*,*,#13962,.T.);
#18120=ORIENTED_EDGE('',*,*,#13963,.T.);
#18121=ORIENTED_EDGE('',*,*,#13962,.F.);
#18122=ORIENTED_EDGE('',*,*,#13891,.T.);
#18123=ORIENTED_EDGE('',*,*,#13964,.T.);
#18124=ORIENTED_EDGE('',*,*,#13965,.T.);
#18125=ORIENTED_EDGE('',*,*,#13966,.T.);
#18126=ORIENTED_EDGE('',*,*,#13886,.T.);
#18127=ORIENTED_EDGE('',*,*,#13967,.T.);
#18128=ORIENTED_EDGE('',*,*,#13968,.T.);
#18129=ORIENTED_EDGE('',*,*,#13887,.T.);
#18130=ORIENTED_EDGE('',*,*,#13966,.F.);
#18131=ORIENTED_EDGE('',*,*,#13969,.T.);
#18132=ORIENTED_EDGE('',*,*,#13970,.T.);
#18133=ORIENTED_EDGE('',*,*,#13888,.T.);
#18134=ORIENTED_EDGE('',*,*,#13968,.F.);
#18135=ORIENTED_EDGE('',*,*,#13971,.T.);
#18136=ORIENTED_EDGE('',*,*,#13972,.T.);
#18137=ORIENTED_EDGE('',*,*,#13889,.T.);
#18138=ORIENTED_EDGE('',*,*,#13970,.F.);
#18139=ORIENTED_EDGE('',*,*,#13973,.T.);
#18140=ORIENTED_EDGE('',*,*,#13890,.T.);
#18141=ORIENTED_EDGE('',*,*,#13972,.F.);
#18142=ORIENTED_EDGE('',*,*,#13974,.T.);
#18143=ORIENTED_EDGE('',*,*,#13964,.F.);
#18144=ORIENTED_EDGE('',*,*,#13975,.T.);
#18145=ORIENTED_EDGE('',*,*,#13899,.T.);
#18146=ORIENTED_EDGE('',*,*,#13949,.F.);
#18147=ORIENTED_EDGE('',*,*,#13976,.T.);
#18148=ORIENTED_EDGE('',*,*,#13977,.T.);
#18149=ORIENTED_EDGE('',*,*,#13900,.T.);
#18150=ORIENTED_EDGE('',*,*,#13975,.F.);
#18151=ORIENTED_EDGE('',*,*,#13978,.T.);
#18152=ORIENTED_EDGE('',*,*,#13979,.T.);
#18153=ORIENTED_EDGE('',*,*,#13901,.T.);
#18154=ORIENTED_EDGE('',*,*,#13977,.F.);
#18155=ORIENTED_EDGE('',*,*,#13980,.T.);
#18156=ORIENTED_EDGE('',*,*,#13902,.T.);
#18157=ORIENTED_EDGE('',*,*,#13979,.F.);
#18158=ORIENTED_EDGE('',*,*,#13981,.T.);
#18159=ORIENTED_EDGE('',*,*,#13946,.F.);
#18160=ORIENTED_EDGE('',*,*,#13982,.T.);
#18161=ORIENTED_EDGE('',*,*,#13967,.F.);
#18162=ORIENTED_EDGE('',*,*,#13909,.T.);
#18163=ORIENTED_EDGE('',*,*,#13983,.T.);
#18164=ORIENTED_EDGE('',*,*,#13984,.T.);
#18165=ORIENTED_EDGE('',*,*,#13983,.F.);
#18166=ORIENTED_EDGE('',*,*,#13908,.T.);
#18167=ORIENTED_EDGE('',*,*,#13985,.T.);
#18168=ORIENTED_EDGE('',*,*,#13986,.T.);
#18169=ORIENTED_EDGE('',*,*,#13985,.F.);
#18170=ORIENTED_EDGE('',*,*,#13907,.T.);
#18171=ORIENTED_EDGE('',*,*,#13941,.T.);
#18172=ORIENTED_EDGE('',*,*,#13952,.F.);
#18173=ORIENTED_EDGE('',*,*,#13987,.F.);
#18174=ORIENTED_EDGE('',*,*,#13839,.T.);
#18175=ORIENTED_EDGE('',*,*,#13988,.F.);
#18176=ORIENTED_EDGE('',*,*,#13954,.F.);
#18177=ORIENTED_EDGE('',*,*,#13989,.F.);
#18178=ORIENTED_EDGE('',*,*,#13840,.T.);
#18179=ORIENTED_EDGE('',*,*,#13987,.T.);
#18180=ORIENTED_EDGE('',*,*,#13956,.F.);
#18181=ORIENTED_EDGE('',*,*,#13990,.F.);
#18182=ORIENTED_EDGE('',*,*,#13841,.T.);
#18183=ORIENTED_EDGE('',*,*,#13989,.T.);
#18184=ORIENTED_EDGE('',*,*,#13958,.F.);
#18185=ORIENTED_EDGE('',*,*,#13991,.T.);
#18186=ORIENTED_EDGE('',*,*,#13842,.F.);
#18187=ORIENTED_EDGE('',*,*,#13990,.T.);
#18188=ORIENTED_EDGE('',*,*,#13959,.F.);
#18189=ORIENTED_EDGE('',*,*,#13992,.F.);
#18190=ORIENTED_EDGE('',*,*,#13843,.T.);
#18191=ORIENTED_EDGE('',*,*,#13991,.F.);
#18192=ORIENTED_EDGE('',*,*,#13961,.F.);
#18193=ORIENTED_EDGE('',*,*,#13993,.F.);
#18194=ORIENTED_EDGE('',*,*,#13844,.T.);
#18195=ORIENTED_EDGE('',*,*,#13992,.T.);
#18196=ORIENTED_EDGE('',*,*,#13963,.F.);
#18197=ORIENTED_EDGE('',*,*,#13994,.F.);
#18198=ORIENTED_EDGE('',*,*,#13845,.T.);
#18199=ORIENTED_EDGE('',*,*,#13993,.T.);
#18200=ORIENTED_EDGE('',*,*,#13974,.F.);
#18201=ORIENTED_EDGE('',*,*,#13995,.F.);
#18202=ORIENTED_EDGE('',*,*,#13822,.F.);
#18203=ORIENTED_EDGE('',*,*,#13994,.T.);
#18204=ORIENTED_EDGE('',*,*,#13973,.F.);
#18205=ORIENTED_EDGE('',*,*,#13996,.F.);
#18206=ORIENTED_EDGE('',*,*,#13823,.T.);
#18207=ORIENTED_EDGE('',*,*,#13995,.T.);
#18208=ORIENTED_EDGE('',*,*,#13971,.F.);
#18209=ORIENTED_EDGE('',*,*,#13997,.F.);
#18210=ORIENTED_EDGE('',*,*,#13824,.F.);
#18211=ORIENTED_EDGE('',*,*,#13996,.T.);
#18212=ORIENTED_EDGE('',*,*,#13969,.F.);
#18213=ORIENTED_EDGE('',*,*,#13998,.F.);
#18214=ORIENTED_EDGE('',*,*,#13825,.T.);
#18215=ORIENTED_EDGE('',*,*,#13997,.T.);
#18216=ORIENTED_EDGE('',*,*,#13965,.F.);
#18217=ORIENTED_EDGE('',*,*,#13999,.T.);
#18218=ORIENTED_EDGE('',*,*,#13826,.F.);
#18219=ORIENTED_EDGE('',*,*,#13998,.T.);
#18220=ORIENTED_EDGE('',*,*,#14000,.T.);
#18221=ORIENTED_EDGE('',*,*,#14001,.T.);
#18222=ORIENTED_EDGE('',*,*,#13924,.T.);
#18223=ORIENTED_EDGE('',*,*,#14002,.T.);
#18224=ORIENTED_EDGE('',*,*,#14003,.T.);
#18225=ORIENTED_EDGE('',*,*,#14004,.T.);
#18226=ORIENTED_EDGE('',*,*,#13919,.T.);
#18227=ORIENTED_EDGE('',*,*,#14005,.T.);
#18228=ORIENTED_EDGE('',*,*,#14006,.T.);
#18229=ORIENTED_EDGE('',*,*,#14007,.T.);
#18230=ORIENTED_EDGE('',*,*,#13916,.T.);
#18231=ORIENTED_EDGE('',*,*,#14008,.T.);
#18232=ORIENTED_EDGE('',*,*,#14009,.T.);
#18233=ORIENTED_EDGE('',*,*,#13917,.T.);
#18234=ORIENTED_EDGE('',*,*,#14007,.F.);
#18235=ORIENTED_EDGE('',*,*,#14010,.T.);
#18236=ORIENTED_EDGE('',*,*,#13918,.T.);
#18237=ORIENTED_EDGE('',*,*,#14009,.F.);
#18238=ORIENTED_EDGE('',*,*,#14011,.T.);
#18239=ORIENTED_EDGE('',*,*,#14005,.F.);
#18240=ORIENTED_EDGE('',*,*,#14012,.T.);
#18241=ORIENTED_EDGE('',*,*,#14013,.T.);
#18242=ORIENTED_EDGE('',*,*,#13911,.T.);
#18243=ORIENTED_EDGE('',*,*,#14014,.T.);
#18244=ORIENTED_EDGE('',*,*,#14015,.T.);
#18245=ORIENTED_EDGE('',*,*,#13912,.T.);
#18246=ORIENTED_EDGE('',*,*,#14013,.F.);
#18247=ORIENTED_EDGE('',*,*,#14016,.T.);
#18248=ORIENTED_EDGE('',*,*,#14017,.T.);
#18249=ORIENTED_EDGE('',*,*,#13913,.T.);
#18250=ORIENTED_EDGE('',*,*,#14015,.F.);
#18251=ORIENTED_EDGE('',*,*,#14018,.T.);
#18252=ORIENTED_EDGE('',*,*,#14019,.T.);
#18253=ORIENTED_EDGE('',*,*,#13914,.T.);
#18254=ORIENTED_EDGE('',*,*,#14017,.F.);
#18255=ORIENTED_EDGE('',*,*,#14020,.T.);
#18256=ORIENTED_EDGE('',*,*,#13915,.T.);
#18257=ORIENTED_EDGE('',*,*,#14019,.F.);
#18258=ORIENTED_EDGE('',*,*,#14021,.T.);
#18259=ORIENTED_EDGE('',*,*,#14008,.F.);
#18260=ORIENTED_EDGE('',*,*,#14022,.T.);
#18261=ORIENTED_EDGE('',*,*,#13920,.T.);
#18262=ORIENTED_EDGE('',*,*,#14004,.F.);
#18263=ORIENTED_EDGE('',*,*,#14023,.T.);
#18264=ORIENTED_EDGE('',*,*,#14024,.T.);
#18265=ORIENTED_EDGE('',*,*,#13921,.T.);
#18266=ORIENTED_EDGE('',*,*,#14022,.F.);
#18267=ORIENTED_EDGE('',*,*,#14025,.T.);
#18268=ORIENTED_EDGE('',*,*,#14026,.T.);
#18269=ORIENTED_EDGE('',*,*,#13922,.T.);
#18270=ORIENTED_EDGE('',*,*,#14024,.F.);
#18271=ORIENTED_EDGE('',*,*,#14027,.T.);
#18272=ORIENTED_EDGE('',*,*,#13923,.T.);
#18273=ORIENTED_EDGE('',*,*,#14026,.F.);
#18274=ORIENTED_EDGE('',*,*,#14028,.T.);
#18275=ORIENTED_EDGE('',*,*,#14002,.F.);
#18276=ORIENTED_EDGE('',*,*,#14029,.T.);
#18277=ORIENTED_EDGE('',*,*,#13925,.T.);
#18278=ORIENTED_EDGE('',*,*,#14001,.F.);
#18279=ORIENTED_EDGE('',*,*,#14030,.T.);
#18280=ORIENTED_EDGE('',*,*,#13926,.T.);
#18281=ORIENTED_EDGE('',*,*,#14029,.F.);
#18282=ORIENTED_EDGE('',*,*,#14031,.T.);
#18283=ORIENTED_EDGE('',*,*,#14014,.F.);
#18284=ORIENTED_EDGE('',*,*,#14011,.F.);
#18285=ORIENTED_EDGE('',*,*,#14032,.F.);
#18286=ORIENTED_EDGE('',*,*,#13866,.F.);
#18287=ORIENTED_EDGE('',*,*,#14033,.F.);
#18288=ORIENTED_EDGE('',*,*,#14010,.F.);
#18289=ORIENTED_EDGE('',*,*,#14034,.F.);
#18290=ORIENTED_EDGE('',*,*,#13867,.F.);
#18291=ORIENTED_EDGE('',*,*,#14032,.T.);
#18292=ORIENTED_EDGE('',*,*,#14006,.F.);
#18293=ORIENTED_EDGE('',*,*,#14035,.F.);
#18294=ORIENTED_EDGE('',*,*,#13852,.F.);
#18295=ORIENTED_EDGE('',*,*,#14034,.T.);
#18296=ORIENTED_EDGE('',*,*,#14021,.F.);
#18297=ORIENTED_EDGE('',*,*,#14036,.F.);
#18298=ORIENTED_EDGE('',*,*,#13853,.F.);
#18299=ORIENTED_EDGE('',*,*,#14035,.T.);
#18300=ORIENTED_EDGE('',*,*,#14020,.F.);
#18301=ORIENTED_EDGE('',*,*,#14037,.F.);
#18302=ORIENTED_EDGE('',*,*,#13854,.F.);
#18303=ORIENTED_EDGE('',*,*,#14036,.T.);
#18304=ORIENTED_EDGE('',*,*,#14018,.F.);
#18305=ORIENTED_EDGE('',*,*,#14038,.F.);
#18306=ORIENTED_EDGE('',*,*,#13855,.F.);
#18307=ORIENTED_EDGE('',*,*,#14037,.T.);
#18308=ORIENTED_EDGE('',*,*,#14016,.F.);
#18309=ORIENTED_EDGE('',*,*,#14039,.F.);
#18310=ORIENTED_EDGE('',*,*,#13856,.F.);
#18311=ORIENTED_EDGE('',*,*,#14038,.T.);
#18312=ORIENTED_EDGE('',*,*,#14012,.F.);
#18313=ORIENTED_EDGE('',*,*,#14040,.T.);
#18314=ORIENTED_EDGE('',*,*,#13857,.F.);
#18315=ORIENTED_EDGE('',*,*,#14039,.T.);
#18316=ORIENTED_EDGE('',*,*,#14031,.F.);
#18317=ORIENTED_EDGE('',*,*,#14041,.F.);
#18318=ORIENTED_EDGE('',*,*,#13858,.F.);
#18319=ORIENTED_EDGE('',*,*,#14040,.F.);
#18320=ORIENTED_EDGE('',*,*,#14000,.F.);
#18321=ORIENTED_EDGE('',*,*,#14042,.F.);
#18322=ORIENTED_EDGE('',*,*,#13860,.F.);
#18323=ORIENTED_EDGE('',*,*,#14043,.T.);
#18324=ORIENTED_EDGE('',*,*,#14030,.F.);
#18325=ORIENTED_EDGE('',*,*,#14043,.F.);
#18326=ORIENTED_EDGE('',*,*,#13859,.F.);
#18327=ORIENTED_EDGE('',*,*,#14041,.T.);
#18328=ORIENTED_EDGE('',*,*,#14003,.F.);
#18329=ORIENTED_EDGE('',*,*,#14033,.T.);
#18330=ORIENTED_EDGE('',*,*,#13865,.F.);
#18331=ORIENTED_EDGE('',*,*,#14044,.T.);
#18332=ORIENTED_EDGE('',*,*,#14028,.F.);
#18333=ORIENTED_EDGE('',*,*,#14045,.F.);
#18334=ORIENTED_EDGE('',*,*,#13861,.F.);
#18335=ORIENTED_EDGE('',*,*,#14042,.T.);
#18336=ORIENTED_EDGE('',*,*,#14023,.F.);
#18337=ORIENTED_EDGE('',*,*,#14044,.F.);
#18338=ORIENTED_EDGE('',*,*,#13864,.F.);
#18339=ORIENTED_EDGE('',*,*,#14046,.T.);
#18340=ORIENTED_EDGE('',*,*,#14025,.F.);
#18341=ORIENTED_EDGE('',*,*,#14046,.F.);
#18342=ORIENTED_EDGE('',*,*,#13863,.F.);
#18343=ORIENTED_EDGE('',*,*,#14047,.T.);
#18344=ORIENTED_EDGE('',*,*,#14027,.F.);
#18345=ORIENTED_EDGE('',*,*,#14047,.F.);
#18346=ORIENTED_EDGE('',*,*,#13862,.F.);
#18347=ORIENTED_EDGE('',*,*,#14045,.T.);
#18348=ORIENTED_EDGE('',*,*,#13982,.F.);
#18349=ORIENTED_EDGE('',*,*,#14048,.F.);
#18350=ORIENTED_EDGE('',*,*,#13827,.F.);
#18351=ORIENTED_EDGE('',*,*,#13999,.F.);
#18352=ORIENTED_EDGE('',*,*,#13986,.F.);
#18353=ORIENTED_EDGE('',*,*,#14049,.F.);
#18354=ORIENTED_EDGE('',*,*,#13829,.F.);
#18355=ORIENTED_EDGE('',*,*,#14050,.T.);
#18356=ORIENTED_EDGE('',*,*,#13984,.F.);
#18357=ORIENTED_EDGE('',*,*,#14050,.F.);
#18358=ORIENTED_EDGE('',*,*,#13828,.F.);
#18359=ORIENTED_EDGE('',*,*,#14048,.T.);
#18360=ORIENTED_EDGE('',*,*,#13940,.F.);
#18361=ORIENTED_EDGE('',*,*,#14051,.T.);
#18362=ORIENTED_EDGE('',*,*,#13830,.F.);
#18363=ORIENTED_EDGE('',*,*,#14049,.T.);
#18364=ORIENTED_EDGE('',*,*,#13947,.F.);
#18365=ORIENTED_EDGE('',*,*,#14052,.F.);
#18366=ORIENTED_EDGE('',*,*,#13833,.F.);
#18367=ORIENTED_EDGE('',*,*,#14053,.T.);
#18368=ORIENTED_EDGE('',*,*,#13943,.F.);
#18369=ORIENTED_EDGE('',*,*,#14054,.F.);
#18370=ORIENTED_EDGE('',*,*,#13831,.F.);
#18371=ORIENTED_EDGE('',*,*,#14051,.F.);
#18372=ORIENTED_EDGE('',*,*,#13945,.F.);
#18373=ORIENTED_EDGE('',*,*,#14053,.F.);
#18374=ORIENTED_EDGE('',*,*,#13832,.F.);
#18375=ORIENTED_EDGE('',*,*,#14054,.T.);
#18376=ORIENTED_EDGE('',*,*,#13981,.F.);
#18377=ORIENTED_EDGE('',*,*,#14055,.F.);
#18378=ORIENTED_EDGE('',*,*,#13834,.F.);
#18379=ORIENTED_EDGE('',*,*,#14052,.T.);
#18380=ORIENTED_EDGE('',*,*,#13980,.F.);
#18381=ORIENTED_EDGE('',*,*,#14056,.F.);
#18382=ORIENTED_EDGE('',*,*,#13835,.T.);
#18383=ORIENTED_EDGE('',*,*,#14055,.T.);
#18384=ORIENTED_EDGE('',*,*,#13978,.F.);
#18385=ORIENTED_EDGE('',*,*,#14057,.F.);
#18386=ORIENTED_EDGE('',*,*,#13836,.F.);
#18387=ORIENTED_EDGE('',*,*,#14056,.T.);
#18388=ORIENTED_EDGE('',*,*,#13976,.F.);
#18389=ORIENTED_EDGE('',*,*,#14058,.F.);
#18390=ORIENTED_EDGE('',*,*,#13837,.T.);
#18391=ORIENTED_EDGE('',*,*,#14057,.T.);
#18392=ORIENTED_EDGE('',*,*,#13948,.F.);
#18393=ORIENTED_EDGE('',*,*,#13988,.T.);
#18394=ORIENTED_EDGE('',*,*,#13838,.F.);
#18395=ORIENTED_EDGE('',*,*,#14058,.T.);
#18396=ORIENTED_EDGE('',*,*,#14059,.F.);
#18397=ORIENTED_EDGE('',*,*,#14060,.T.);
#18398=ORIENTED_EDGE('',*,*,#14061,.F.);
#18399=ORIENTED_EDGE('',*,*,#14060,.F.);
#18400=ORIENTED_EDGE('',*,*,#14059,.T.);
#18401=ORIENTED_EDGE('',*,*,#14062,.F.);
#18402=ORIENTED_EDGE('',*,*,#14063,.T.);
#18403=ORIENTED_EDGE('',*,*,#14064,.F.);
#18404=ORIENTED_EDGE('',*,*,#14063,.F.);
#18405=ORIENTED_EDGE('',*,*,#14065,.F.);
#18406=ORIENTED_EDGE('',*,*,#14066,.T.);
#18407=ORIENTED_EDGE('',*,*,#14067,.F.);
#18408=ORIENTED_EDGE('',*,*,#14066,.F.);
#18409=ORIENTED_EDGE('',*,*,#14068,.F.);
#18410=ORIENTED_EDGE('',*,*,#14069,.T.);
#18411=ORIENTED_EDGE('',*,*,#14070,.F.);
#18412=ORIENTED_EDGE('',*,*,#14069,.F.);
#18413=ORIENTED_EDGE('',*,*,#14071,.F.);
#18414=ORIENTED_EDGE('',*,*,#14072,.T.);
#18415=ORIENTED_EDGE('',*,*,#14073,.F.);
#18416=ORIENTED_EDGE('',*,*,#14072,.F.);
#18417=ORIENTED_EDGE('',*,*,#14074,.T.);
#18418=ORIENTED_EDGE('',*,*,#14075,.T.);
#18419=ORIENTED_EDGE('',*,*,#14076,.T.);
#18420=ORIENTED_EDGE('',*,*,#14075,.F.);
#18421=ORIENTED_EDGE('',*,*,#14074,.F.);
#18422=ORIENTED_EDGE('',*,*,#14077,.T.);
#18423=ORIENTED_EDGE('',*,*,#14078,.T.);
#18424=ORIENTED_EDGE('',*,*,#14077,.F.);
#18425=ORIENTED_EDGE('',*,*,#14079,.F.);
#18426=ORIENTED_EDGE('',*,*,#14076,.F.);
#18427=ORIENTED_EDGE('',*,*,#14080,.T.);
#18428=ORIENTED_EDGE('',*,*,#14078,.F.);
#18429=ORIENTED_EDGE('',*,*,#14080,.F.);
#18430=ORIENTED_EDGE('',*,*,#14081,.F.);
#18431=ORIENTED_EDGE('',*,*,#14082,.T.);
#18432=ORIENTED_EDGE('',*,*,#14083,.T.);
#18433=ORIENTED_EDGE('',*,*,#14082,.F.);
#18434=ORIENTED_EDGE('',*,*,#14083,.F.);
#18435=ORIENTED_EDGE('',*,*,#14084,.T.);
#18436=ORIENTED_EDGE('',*,*,#14079,.T.);
#18437=ORIENTED_EDGE('',*,*,#14084,.F.);
#18438=ORIENTED_EDGE('',*,*,#14085,.F.);
#18439=ORIENTED_EDGE('',*,*,#14086,.T.);
#18440=ORIENTED_EDGE('',*,*,#14087,.T.);
#18441=ORIENTED_EDGE('',*,*,#14086,.F.);
#18442=ORIENTED_EDGE('',*,*,#14088,.F.);
#18443=ORIENTED_EDGE('',*,*,#14081,.T.);
#18444=ORIENTED_EDGE('',*,*,#14087,.F.);
#18445=ORIENTED_EDGE('',*,*,#14089,.T.);
#18446=ORIENTED_EDGE('',*,*,#14088,.T.);
#18447=ORIENTED_EDGE('',*,*,#14089,.F.);
#18448=ORIENTED_EDGE('',*,*,#14090,.F.);
#18449=ORIENTED_EDGE('',*,*,#14091,.T.);
#18450=ORIENTED_EDGE('',*,*,#14092,.F.);
#18451=ORIENTED_EDGE('',*,*,#14093,.F.);
#18452=ORIENTED_EDGE('',*,*,#14094,.F.);
#18453=ORIENTED_EDGE('',*,*,#14093,.T.);
#18454=ORIENTED_EDGE('',*,*,#14095,.F.);
#18455=ORIENTED_EDGE('',*,*,#14096,.F.);
#18456=ORIENTED_EDGE('',*,*,#14097,.F.);
#18457=ORIENTED_EDGE('',*,*,#14098,.T.);
#18458=ORIENTED_EDGE('',*,*,#14099,.F.);
#18459=ORIENTED_EDGE('',*,*,#14100,.F.);
#18460=ORIENTED_EDGE('',*,*,#14101,.F.);
#18461=ORIENTED_EDGE('',*,*,#14100,.T.);
#18462=ORIENTED_EDGE('',*,*,#14102,.F.);
#18463=ORIENTED_EDGE('',*,*,#14103,.F.);
#18464=ORIENTED_EDGE('',*,*,#14104,.F.);
#18465=ORIENTED_EDGE('',*,*,#14103,.T.);
#18466=ORIENTED_EDGE('',*,*,#14105,.F.);
#18467=ORIENTED_EDGE('',*,*,#14106,.F.);
#18468=ORIENTED_EDGE('',*,*,#14107,.F.);
#18469=ORIENTED_EDGE('',*,*,#14108,.T.);
#18470=ORIENTED_EDGE('',*,*,#14109,.F.);
#18471=ORIENTED_EDGE('',*,*,#14091,.F.);
#18472=ORIENTED_EDGE('',*,*,#14109,.T.);
#18473=ORIENTED_EDGE('',*,*,#14110,.T.);
#18474=ORIENTED_EDGE('',*,*,#14105,.T.);
#18475=ORIENTED_EDGE('',*,*,#14102,.T.);
#18476=ORIENTED_EDGE('',*,*,#14099,.T.);
#18477=ORIENTED_EDGE('',*,*,#14111,.T.);
#18478=ORIENTED_EDGE('',*,*,#14095,.T.);
#18479=ORIENTED_EDGE('',*,*,#14092,.T.);
#18480=ORIENTED_EDGE('',*,*,#14085,.T.);
#18481=ORIENTED_EDGE('',*,*,#14094,.T.);
#18482=ORIENTED_EDGE('',*,*,#14112,.T.);
#18483=ORIENTED_EDGE('',*,*,#14113,.T.);
#18484=ORIENTED_EDGE('',*,*,#14114,.T.);
#18485=ORIENTED_EDGE('',*,*,#14115,.T.);
#18486=ORIENTED_EDGE('',*,*,#14116,.T.);
#18487=ORIENTED_EDGE('',*,*,#14107,.T.);
#18488=ORIENTED_EDGE('',*,*,#14090,.T.);
#18489=ORIENTED_EDGE('',*,*,#14062,.T.);
#18490=ORIENTED_EDGE('',*,*,#14071,.T.);
#18491=ORIENTED_EDGE('',*,*,#14097,.T.);
#18492=ORIENTED_EDGE('',*,*,#14101,.T.);
#18493=ORIENTED_EDGE('',*,*,#14104,.T.);
#18494=ORIENTED_EDGE('',*,*,#14117,.T.);
#18495=ORIENTED_EDGE('',*,*,#14118,.T.);
#18496=ORIENTED_EDGE('',*,*,#14119,.T.);
#18497=ORIENTED_EDGE('',*,*,#14120,.T.);
#18498=ORIENTED_EDGE('',*,*,#14121,.T.);
#18499=ORIENTED_EDGE('',*,*,#14065,.T.);
#18500=ORIENTED_EDGE('',*,*,#14068,.T.);
#18501=ORIENTED_EDGE('',*,*,#14122,.T.);
#18502=ORIENTED_EDGE('',*,*,#14123,.T.);
#18503=ORIENTED_EDGE('',*,*,#14124,.T.);
#18504=ORIENTED_EDGE('',*,*,#14125,.T.);
#18505=ORIENTED_EDGE('',*,*,#14126,.F.);
#18506=ORIENTED_EDGE('',*,*,#14127,.T.);
#18507=ORIENTED_EDGE('',*,*,#14128,.F.);
#18508=ORIENTED_EDGE('',*,*,#14129,.T.);
#18509=ORIENTED_EDGE('',*,*,#14064,.T.);
#18510=ORIENTED_EDGE('',*,*,#14073,.T.);
#18511=ORIENTED_EDGE('',*,*,#14127,.F.);
#18512=ORIENTED_EDGE('',*,*,#14130,.T.);
#18513=ORIENTED_EDGE('',*,*,#14114,.F.);
#18514=ORIENTED_EDGE('',*,*,#14131,.F.);
#18515=ORIENTED_EDGE('',*,*,#14128,.T.);
#18516=ORIENTED_EDGE('',*,*,#14131,.T.);
#18517=ORIENTED_EDGE('',*,*,#14113,.F.);
#18518=ORIENTED_EDGE('',*,*,#14132,.F.);
#18519=ORIENTED_EDGE('',*,*,#14129,.F.);
#18520=ORIENTED_EDGE('',*,*,#14132,.T.);
#18521=ORIENTED_EDGE('',*,*,#14112,.F.);
#18522=ORIENTED_EDGE('',*,*,#14096,.T.);
#18523=ORIENTED_EDGE('',*,*,#14111,.F.);
#18524=ORIENTED_EDGE('',*,*,#14098,.F.);
#18525=ORIENTED_EDGE('',*,*,#14121,.F.);
#18526=ORIENTED_EDGE('',*,*,#14133,.F.);
#18527=ORIENTED_EDGE('',*,*,#14134,.F.);
#18528=ORIENTED_EDGE('',*,*,#14135,.F.);
#18529=ORIENTED_EDGE('',*,*,#14136,.T.);
#18530=ORIENTED_EDGE('',*,*,#14133,.T.);
#18531=ORIENTED_EDGE('',*,*,#14120,.F.);
#18532=ORIENTED_EDGE('',*,*,#14137,.F.);
#18533=ORIENTED_EDGE('',*,*,#14138,.F.);
#18534=ORIENTED_EDGE('',*,*,#14137,.T.);
#18535=ORIENTED_EDGE('',*,*,#14119,.F.);
#18536=ORIENTED_EDGE('',*,*,#14139,.F.);
#18537=ORIENTED_EDGE('',*,*,#14140,.T.);
#18538=ORIENTED_EDGE('',*,*,#14139,.T.);
#18539=ORIENTED_EDGE('',*,*,#14118,.F.);
#18540=ORIENTED_EDGE('',*,*,#14141,.F.);
#18541=ORIENTED_EDGE('',*,*,#14142,.F.);
#18542=ORIENTED_EDGE('',*,*,#14141,.T.);
#18543=ORIENTED_EDGE('',*,*,#14117,.F.);
#18544=ORIENTED_EDGE('',*,*,#14106,.T.);
#18545=ORIENTED_EDGE('',*,*,#14110,.F.);
#18546=ORIENTED_EDGE('',*,*,#14108,.F.);
#18547=ORIENTED_EDGE('',*,*,#14116,.F.);
#18548=ORIENTED_EDGE('',*,*,#14143,.F.);
#18549=ORIENTED_EDGE('',*,*,#14125,.F.);
#18550=ORIENTED_EDGE('',*,*,#14144,.F.);
#18551=ORIENTED_EDGE('',*,*,#14126,.T.);
#18552=ORIENTED_EDGE('',*,*,#14143,.T.);
#18553=ORIENTED_EDGE('',*,*,#14115,.F.);
#18554=ORIENTED_EDGE('',*,*,#14130,.F.);
#18555=ORIENTED_EDGE('',*,*,#14145,.T.);
#18556=ORIENTED_EDGE('',*,*,#14134,.T.);
#18557=ORIENTED_EDGE('',*,*,#14136,.F.);
#18558=ORIENTED_EDGE('',*,*,#14138,.T.);
#18559=ORIENTED_EDGE('',*,*,#14140,.F.);
#18560=ORIENTED_EDGE('',*,*,#14142,.T.);
#18561=ORIENTED_EDGE('',*,*,#14146,.T.);
#18562=ORIENTED_EDGE('',*,*,#14147,.T.);
#18563=ORIENTED_EDGE('',*,*,#14067,.T.);
#18564=ORIENTED_EDGE('',*,*,#14070,.T.);
#18565=ORIENTED_EDGE('',*,*,#14144,.T.);
#18566=ORIENTED_EDGE('',*,*,#14148,.T.);
#18567=ORIENTED_EDGE('',*,*,#14149,.T.);
#18568=ORIENTED_EDGE('',*,*,#14150,.T.);
#18569=ORIENTED_EDGE('',*,*,#14151,.F.);
#18570=ORIENTED_EDGE('',*,*,#14152,.T.);
#18571=ORIENTED_EDGE('',*,*,#14123,.F.);
#18572=ORIENTED_EDGE('',*,*,#14153,.F.);
#18573=ORIENTED_EDGE('',*,*,#14154,.T.);
#18574=ORIENTED_EDGE('',*,*,#14153,.T.);
#18575=ORIENTED_EDGE('',*,*,#14122,.F.);
#18576=ORIENTED_EDGE('',*,*,#14155,.F.);
#18577=ORIENTED_EDGE('',*,*,#14156,.F.);
#18578=ORIENTED_EDGE('',*,*,#14157,.F.);
#18579=ORIENTED_EDGE('',*,*,#14156,.T.);
#18580=ORIENTED_EDGE('',*,*,#14158,.F.);
#18581=ORIENTED_EDGE('',*,*,#14159,.F.);
#18582=ORIENTED_EDGE('',*,*,#14160,.T.);
#18583=ORIENTED_EDGE('',*,*,#14159,.T.);
#18584=ORIENTED_EDGE('',*,*,#14161,.F.);
#18585=ORIENTED_EDGE('',*,*,#14145,.F.);
#18586=ORIENTED_EDGE('',*,*,#14162,.F.);
#18587=ORIENTED_EDGE('',*,*,#14163,.F.);
#18588=ORIENTED_EDGE('',*,*,#14162,.T.);
#18589=ORIENTED_EDGE('',*,*,#14147,.F.);
#18590=ORIENTED_EDGE('',*,*,#14164,.F.);
#18591=ORIENTED_EDGE('',*,*,#14061,.T.);
#18592=ORIENTED_EDGE('',*,*,#14165,.T.);
#18593=ORIENTED_EDGE('',*,*,#14164,.T.);
#18594=ORIENTED_EDGE('',*,*,#14146,.F.);
#18595=ORIENTED_EDGE('',*,*,#14150,.F.);
#18596=ORIENTED_EDGE('',*,*,#14166,.F.);
#18597=ORIENTED_EDGE('',*,*,#14167,.F.);
#18598=ORIENTED_EDGE('',*,*,#14166,.T.);
#18599=ORIENTED_EDGE('',*,*,#14149,.F.);
#18600=ORIENTED_EDGE('',*,*,#14168,.F.);
#18601=ORIENTED_EDGE('',*,*,#14169,.T.);
#18602=ORIENTED_EDGE('',*,*,#14168,.T.);
#18603=ORIENTED_EDGE('',*,*,#14148,.F.);
#18604=ORIENTED_EDGE('',*,*,#14124,.F.);
#18605=ORIENTED_EDGE('',*,*,#14152,.F.);
#18606=ORIENTED_EDGE('',*,*,#14135,.T.);
#18607=ORIENTED_EDGE('',*,*,#14161,.T.);
#18608=ORIENTED_EDGE('',*,*,#14158,.T.);
#18609=ORIENTED_EDGE('',*,*,#14155,.T.);
#18610=ORIENTED_EDGE('',*,*,#14169,.F.);
#18611=ORIENTED_EDGE('',*,*,#14151,.T.);
#18612=ORIENTED_EDGE('',*,*,#14154,.F.);
#18613=ORIENTED_EDGE('',*,*,#14157,.T.);
#18614=ORIENTED_EDGE('',*,*,#14160,.F.);
#18615=ORIENTED_EDGE('',*,*,#14163,.T.);
#18616=ORIENTED_EDGE('',*,*,#14165,.F.);
#18617=ORIENTED_EDGE('',*,*,#14167,.T.);
#18618=ORIENTED_EDGE('',*,*,#14170,.F.);
#18619=ORIENTED_EDGE('',*,*,#14171,.F.);
#18620=ORIENTED_EDGE('',*,*,#14172,.F.);
#18621=ORIENTED_EDGE('',*,*,#14173,.T.);
#18622=ORIENTED_EDGE('',*,*,#14174,.F.);
#18623=ORIENTED_EDGE('',*,*,#14175,.T.);
#18624=ORIENTED_EDGE('',*,*,#14176,.F.);
#18625=ORIENTED_EDGE('',*,*,#14177,.F.);
#18626=ORIENTED_EDGE('',*,*,#14178,.T.);
#18627=ORIENTED_EDGE('',*,*,#14177,.T.);
#18628=ORIENTED_EDGE('',*,*,#14179,.F.);
#18629=ORIENTED_EDGE('',*,*,#14180,.F.);
#18630=ORIENTED_EDGE('',*,*,#14181,.F.);
#18631=ORIENTED_EDGE('',*,*,#14182,.T.);
#18632=ORIENTED_EDGE('',*,*,#14180,.T.);
#18633=ORIENTED_EDGE('',*,*,#14183,.F.);
#18634=ORIENTED_EDGE('',*,*,#14184,.F.);
#18635=ORIENTED_EDGE('',*,*,#14172,.T.);
#18636=ORIENTED_EDGE('',*,*,#14185,.F.);
#18637=ORIENTED_EDGE('',*,*,#14175,.F.);
#18638=ORIENTED_EDGE('',*,*,#14186,.F.);
#18639=ORIENTED_EDGE('',*,*,#14187,.F.);
#18640=ORIENTED_EDGE('',*,*,#14188,.T.);
#18641=ORIENTED_EDGE('',*,*,#14189,.T.);
#18642=ORIENTED_EDGE('',*,*,#14190,.F.);
#18643=ORIENTED_EDGE('',*,*,#14191,.F.);
#18644=ORIENTED_EDGE('',*,*,#14192,.F.);
#18645=ORIENTED_EDGE('',*,*,#14193,.F.);
#18646=ORIENTED_EDGE('',*,*,#14194,.T.);
#18647=ORIENTED_EDGE('',*,*,#14195,.T.);
#18648=ORIENTED_EDGE('',*,*,#14196,.F.);
#18649=ORIENTED_EDGE('',*,*,#14197,.F.);
#18650=ORIENTED_EDGE('',*,*,#14198,.F.);
#18651=ORIENTED_EDGE('',*,*,#14199,.F.);
#18652=ORIENTED_EDGE('',*,*,#14200,.T.);
#18653=ORIENTED_EDGE('',*,*,#14201,.T.);
#18654=ORIENTED_EDGE('',*,*,#14202,.F.);
#18655=ORIENTED_EDGE('',*,*,#14203,.F.);
#18656=ORIENTED_EDGE('',*,*,#14204,.F.);
#18657=ORIENTED_EDGE('',*,*,#14205,.F.);
#18658=ORIENTED_EDGE('',*,*,#14206,.T.);
#18659=ORIENTED_EDGE('',*,*,#14207,.T.);
#18660=ORIENTED_EDGE('',*,*,#14208,.F.);
#18661=ORIENTED_EDGE('',*,*,#14209,.F.);
#18662=ORIENTED_EDGE('',*,*,#14210,.F.);
#18663=ORIENTED_EDGE('',*,*,#14211,.F.);
#18664=ORIENTED_EDGE('',*,*,#14212,.T.);
#18665=ORIENTED_EDGE('',*,*,#14213,.T.);
#18666=ORIENTED_EDGE('',*,*,#14214,.F.);
#18667=ORIENTED_EDGE('',*,*,#14215,.F.);
#18668=ORIENTED_EDGE('',*,*,#14216,.F.);
#18669=ORIENTED_EDGE('',*,*,#14217,.F.);
#18670=ORIENTED_EDGE('',*,*,#14218,.T.);
#18671=ORIENTED_EDGE('',*,*,#14219,.T.);
#18672=ORIENTED_EDGE('',*,*,#14220,.F.);
#18673=ORIENTED_EDGE('',*,*,#14221,.F.);
#18674=ORIENTED_EDGE('',*,*,#14222,.F.);
#18675=ORIENTED_EDGE('',*,*,#14223,.F.);
#18676=ORIENTED_EDGE('',*,*,#14224,.T.);
#18677=ORIENTED_EDGE('',*,*,#14225,.T.);
#18678=ORIENTED_EDGE('',*,*,#14226,.F.);
#18679=ORIENTED_EDGE('',*,*,#14227,.F.);
#18680=ORIENTED_EDGE('',*,*,#14228,.F.);
#18681=ORIENTED_EDGE('',*,*,#14229,.F.);
#18682=ORIENTED_EDGE('',*,*,#14230,.T.);
#18683=ORIENTED_EDGE('',*,*,#14231,.T.);
#18684=ORIENTED_EDGE('',*,*,#14232,.F.);
#18685=ORIENTED_EDGE('',*,*,#14233,.F.);
#18686=ORIENTED_EDGE('',*,*,#14234,.F.);
#18687=ORIENTED_EDGE('',*,*,#14235,.F.);
#18688=ORIENTED_EDGE('',*,*,#14236,.T.);
#18689=ORIENTED_EDGE('',*,*,#14237,.T.);
#18690=ORIENTED_EDGE('',*,*,#14238,.F.);
#18691=ORIENTED_EDGE('',*,*,#14239,.F.);
#18692=ORIENTED_EDGE('',*,*,#14240,.F.);
#18693=ORIENTED_EDGE('',*,*,#14241,.F.);
#18694=ORIENTED_EDGE('',*,*,#14242,.T.);
#18695=ORIENTED_EDGE('',*,*,#14243,.T.);
#18696=ORIENTED_EDGE('',*,*,#14244,.F.);
#18697=ORIENTED_EDGE('',*,*,#14245,.F.);
#18698=ORIENTED_EDGE('',*,*,#14246,.F.);
#18699=ORIENTED_EDGE('',*,*,#14247,.F.);
#18700=ORIENTED_EDGE('',*,*,#14248,.T.);
#18701=ORIENTED_EDGE('',*,*,#14249,.T.);
#18702=ORIENTED_EDGE('',*,*,#14250,.F.);
#18703=ORIENTED_EDGE('',*,*,#14251,.F.);
#18704=ORIENTED_EDGE('',*,*,#14252,.F.);
#18705=ORIENTED_EDGE('',*,*,#14253,.F.);
#18706=ORIENTED_EDGE('',*,*,#14254,.T.);
#18707=ORIENTED_EDGE('',*,*,#14255,.T.);
#18708=ORIENTED_EDGE('',*,*,#14256,.F.);
#18709=ORIENTED_EDGE('',*,*,#14257,.F.);
#18710=ORIENTED_EDGE('',*,*,#14258,.F.);
#18711=ORIENTED_EDGE('',*,*,#14259,.F.);
#18712=ORIENTED_EDGE('',*,*,#14260,.T.);
#18713=ORIENTED_EDGE('',*,*,#14261,.T.);
#18714=ORIENTED_EDGE('',*,*,#14262,.F.);
#18715=ORIENTED_EDGE('',*,*,#14263,.F.);
#18716=ORIENTED_EDGE('',*,*,#14264,.F.);
#18717=ORIENTED_EDGE('',*,*,#14265,.F.);
#18718=ORIENTED_EDGE('',*,*,#14266,.T.);
#18719=ORIENTED_EDGE('',*,*,#14267,.T.);
#18720=ORIENTED_EDGE('',*,*,#14268,.F.);
#18721=ORIENTED_EDGE('',*,*,#14269,.F.);
#18722=ORIENTED_EDGE('',*,*,#14270,.F.);
#18723=ORIENTED_EDGE('',*,*,#14271,.F.);
#18724=ORIENTED_EDGE('',*,*,#14272,.T.);
#18725=ORIENTED_EDGE('',*,*,#14273,.T.);
#18726=ORIENTED_EDGE('',*,*,#14274,.F.);
#18727=ORIENTED_EDGE('',*,*,#14275,.F.);
#18728=ORIENTED_EDGE('',*,*,#14276,.F.);
#18729=ORIENTED_EDGE('',*,*,#14173,.F.);
#18730=ORIENTED_EDGE('',*,*,#14184,.T.);
#18731=ORIENTED_EDGE('',*,*,#14174,.T.);
#18732=ORIENTED_EDGE('',*,*,#14178,.F.);
#18733=ORIENTED_EDGE('',*,*,#14182,.F.);
#18734=ORIENTED_EDGE('',*,*,#14277,.T.);
#18735=ORIENTED_EDGE('',*,*,#14181,.T.);
#18736=ORIENTED_EDGE('',*,*,#14278,.F.);
#18737=ORIENTED_EDGE('',*,*,#14279,.T.);
#18738=ORIENTED_EDGE('',*,*,#14186,.T.);
#18739=ORIENTED_EDGE('',*,*,#14279,.F.);
#18740=ORIENTED_EDGE('',*,*,#14280,.F.);
#18741=ORIENTED_EDGE('',*,*,#14281,.F.);
#18742=ORIENTED_EDGE('',*,*,#14187,.T.);
#18743=ORIENTED_EDGE('',*,*,#14189,.F.);
#18744=ORIENTED_EDGE('',*,*,#14282,.T.);
#18745=ORIENTED_EDGE('',*,*,#14283,.F.);
#18746=ORIENTED_EDGE('',*,*,#14284,.F.);
#18747=ORIENTED_EDGE('',*,*,#14190,.T.);
#18748=ORIENTED_EDGE('',*,*,#14284,.T.);
#18749=ORIENTED_EDGE('',*,*,#14285,.F.);
#18750=ORIENTED_EDGE('',*,*,#14286,.F.);
#18751=ORIENTED_EDGE('',*,*,#14287,.F.);
#18752=ORIENTED_EDGE('',*,*,#14191,.T.);
#18753=ORIENTED_EDGE('',*,*,#14286,.T.);
#18754=ORIENTED_EDGE('',*,*,#14288,.F.);
#18755=ORIENTED_EDGE('',*,*,#14188,.F.);
#18756=ORIENTED_EDGE('',*,*,#14281,.T.);
#18757=ORIENTED_EDGE('',*,*,#14289,.F.);
#18758=ORIENTED_EDGE('',*,*,#14282,.F.);
#18759=ORIENTED_EDGE('',*,*,#14287,.T.);
#18760=ORIENTED_EDGE('',*,*,#14290,.F.);
#18761=ORIENTED_EDGE('',*,*,#14291,.T.);
#18762=ORIENTED_EDGE('',*,*,#14192,.T.);
#18763=ORIENTED_EDGE('',*,*,#14291,.F.);
#18764=ORIENTED_EDGE('',*,*,#14292,.F.);
#18765=ORIENTED_EDGE('',*,*,#14293,.F.);
#18766=ORIENTED_EDGE('',*,*,#14193,.T.);
#18767=ORIENTED_EDGE('',*,*,#14195,.F.);
#18768=ORIENTED_EDGE('',*,*,#14294,.T.);
#18769=ORIENTED_EDGE('',*,*,#14295,.F.);
#18770=ORIENTED_EDGE('',*,*,#14296,.F.);
#18771=ORIENTED_EDGE('',*,*,#14196,.T.);
#18772=ORIENTED_EDGE('',*,*,#14296,.T.);
#18773=ORIENTED_EDGE('',*,*,#14297,.F.);
#18774=ORIENTED_EDGE('',*,*,#14298,.F.);
#18775=ORIENTED_EDGE('',*,*,#14299,.F.);
#18776=ORIENTED_EDGE('',*,*,#14197,.T.);
#18777=ORIENTED_EDGE('',*,*,#14298,.T.);
#18778=ORIENTED_EDGE('',*,*,#14300,.F.);
#18779=ORIENTED_EDGE('',*,*,#14194,.F.);
#18780=ORIENTED_EDGE('',*,*,#14293,.T.);
#18781=ORIENTED_EDGE('',*,*,#14301,.F.);
#18782=ORIENTED_EDGE('',*,*,#14294,.F.);
#18783=ORIENTED_EDGE('',*,*,#14299,.T.);
#18784=ORIENTED_EDGE('',*,*,#14302,.F.);
#18785=ORIENTED_EDGE('',*,*,#14303,.T.);
#18786=ORIENTED_EDGE('',*,*,#14198,.T.);
#18787=ORIENTED_EDGE('',*,*,#14303,.F.);
#18788=ORIENTED_EDGE('',*,*,#14304,.F.);
#18789=ORIENTED_EDGE('',*,*,#14305,.F.);
#18790=ORIENTED_EDGE('',*,*,#14199,.T.);
#18791=ORIENTED_EDGE('',*,*,#14201,.F.);
#18792=ORIENTED_EDGE('',*,*,#14306,.T.);
#18793=ORIENTED_EDGE('',*,*,#14307,.F.);
#18794=ORIENTED_EDGE('',*,*,#14308,.F.);
#18795=ORIENTED_EDGE('',*,*,#14202,.T.);
#18796=ORIENTED_EDGE('',*,*,#14308,.T.);
#18797=ORIENTED_EDGE('',*,*,#14309,.F.);
#18798=ORIENTED_EDGE('',*,*,#14310,.F.);
#18799=ORIENTED_EDGE('',*,*,#14311,.F.);
#18800=ORIENTED_EDGE('',*,*,#14203,.T.);
#18801=ORIENTED_EDGE('',*,*,#14310,.T.);
#18802=ORIENTED_EDGE('',*,*,#14312,.F.);
#18803=ORIENTED_EDGE('',*,*,#14200,.F.);
#18804=ORIENTED_EDGE('',*,*,#14305,.T.);
#18805=ORIENTED_EDGE('',*,*,#14313,.F.);
#18806=ORIENTED_EDGE('',*,*,#14306,.F.);
#18807=ORIENTED_EDGE('',*,*,#14311,.T.);
#18808=ORIENTED_EDGE('',*,*,#14314,.F.);
#18809=ORIENTED_EDGE('',*,*,#14315,.T.);
#18810=ORIENTED_EDGE('',*,*,#14204,.T.);
#18811=ORIENTED_EDGE('',*,*,#14315,.F.);
#18812=ORIENTED_EDGE('',*,*,#14316,.F.);
#18813=ORIENTED_EDGE('',*,*,#14317,.F.);
#18814=ORIENTED_EDGE('',*,*,#14205,.T.);
#18815=ORIENTED_EDGE('',*,*,#14207,.F.);
#18816=ORIENTED_EDGE('',*,*,#14318,.T.);
#18817=ORIENTED_EDGE('',*,*,#14319,.F.);
#18818=ORIENTED_EDGE('',*,*,#14320,.F.);
#18819=ORIENTED_EDGE('',*,*,#14208,.T.);
#18820=ORIENTED_EDGE('',*,*,#14320,.T.);
#18821=ORIENTED_EDGE('',*,*,#14321,.F.);
#18822=ORIENTED_EDGE('',*,*,#14322,.F.);
#18823=ORIENTED_EDGE('',*,*,#14323,.F.);
#18824=ORIENTED_EDGE('',*,*,#14209,.T.);
#18825=ORIENTED_EDGE('',*,*,#14322,.T.);
#18826=ORIENTED_EDGE('',*,*,#14324,.F.);
#18827=ORIENTED_EDGE('',*,*,#14206,.F.);
#18828=ORIENTED_EDGE('',*,*,#14317,.T.);
#18829=ORIENTED_EDGE('',*,*,#14325,.F.);
#18830=ORIENTED_EDGE('',*,*,#14318,.F.);
#18831=ORIENTED_EDGE('',*,*,#14323,.T.);
#18832=ORIENTED_EDGE('',*,*,#14326,.F.);
#18833=ORIENTED_EDGE('',*,*,#14327,.T.);
#18834=ORIENTED_EDGE('',*,*,#14210,.T.);
#18835=ORIENTED_EDGE('',*,*,#14327,.F.);
#18836=ORIENTED_EDGE('',*,*,#14328,.F.);
#18837=ORIENTED_EDGE('',*,*,#14329,.F.);
#18838=ORIENTED_EDGE('',*,*,#14211,.T.);
#18839=ORIENTED_EDGE('',*,*,#14213,.F.);
#18840=ORIENTED_EDGE('',*,*,#14330,.T.);
#18841=ORIENTED_EDGE('',*,*,#14331,.F.);
#18842=ORIENTED_EDGE('',*,*,#14332,.F.);
#18843=ORIENTED_EDGE('',*,*,#14214,.T.);
#18844=ORIENTED_EDGE('',*,*,#14332,.T.);
#18845=ORIENTED_EDGE('',*,*,#14333,.F.);
#18846=ORIENTED_EDGE('',*,*,#14334,.F.);
#18847=ORIENTED_EDGE('',*,*,#14335,.F.);
#18848=ORIENTED_EDGE('',*,*,#14215,.T.);
#18849=ORIENTED_EDGE('',*,*,#14334,.T.);
#18850=ORIENTED_EDGE('',*,*,#14336,.F.);
#18851=ORIENTED_EDGE('',*,*,#14212,.F.);
#18852=ORIENTED_EDGE('',*,*,#14329,.T.);
#18853=ORIENTED_EDGE('',*,*,#14337,.F.);
#18854=ORIENTED_EDGE('',*,*,#14330,.F.);
#18855=ORIENTED_EDGE('',*,*,#14335,.T.);
#18856=ORIENTED_EDGE('',*,*,#14338,.F.);
#18857=ORIENTED_EDGE('',*,*,#14339,.T.);
#18858=ORIENTED_EDGE('',*,*,#14216,.T.);
#18859=ORIENTED_EDGE('',*,*,#14339,.F.);
#18860=ORIENTED_EDGE('',*,*,#14340,.F.);
#18861=ORIENTED_EDGE('',*,*,#14341,.F.);
#18862=ORIENTED_EDGE('',*,*,#14217,.T.);
#18863=ORIENTED_EDGE('',*,*,#14219,.F.);
#18864=ORIENTED_EDGE('',*,*,#14342,.T.);
#18865=ORIENTED_EDGE('',*,*,#14343,.F.);
#18866=ORIENTED_EDGE('',*,*,#14344,.F.);
#18867=ORIENTED_EDGE('',*,*,#14220,.T.);
#18868=ORIENTED_EDGE('',*,*,#14344,.T.);
#18869=ORIENTED_EDGE('',*,*,#14345,.F.);
#18870=ORIENTED_EDGE('',*,*,#14346,.F.);
#18871=ORIENTED_EDGE('',*,*,#14347,.F.);
#18872=ORIENTED_EDGE('',*,*,#14221,.T.);
#18873=ORIENTED_EDGE('',*,*,#14346,.T.);
#18874=ORIENTED_EDGE('',*,*,#14348,.F.);
#18875=ORIENTED_EDGE('',*,*,#14218,.F.);
#18876=ORIENTED_EDGE('',*,*,#14341,.T.);
#18877=ORIENTED_EDGE('',*,*,#14349,.F.);
#18878=ORIENTED_EDGE('',*,*,#14342,.F.);
#18879=ORIENTED_EDGE('',*,*,#14347,.T.);
#18880=ORIENTED_EDGE('',*,*,#14350,.F.);
#18881=ORIENTED_EDGE('',*,*,#14351,.T.);
#18882=ORIENTED_EDGE('',*,*,#14222,.T.);
#18883=ORIENTED_EDGE('',*,*,#14351,.F.);
#18884=ORIENTED_EDGE('',*,*,#14352,.F.);
#18885=ORIENTED_EDGE('',*,*,#14353,.F.);
#18886=ORIENTED_EDGE('',*,*,#14223,.T.);
#18887=ORIENTED_EDGE('',*,*,#14225,.F.);
#18888=ORIENTED_EDGE('',*,*,#14354,.T.);
#18889=ORIENTED_EDGE('',*,*,#14355,.F.);
#18890=ORIENTED_EDGE('',*,*,#14356,.F.);
#18891=ORIENTED_EDGE('',*,*,#14226,.T.);
#18892=ORIENTED_EDGE('',*,*,#14356,.T.);
#18893=ORIENTED_EDGE('',*,*,#14357,.F.);
#18894=ORIENTED_EDGE('',*,*,#14358,.F.);
#18895=ORIENTED_EDGE('',*,*,#14359,.F.);
#18896=ORIENTED_EDGE('',*,*,#14227,.T.);
#18897=ORIENTED_EDGE('',*,*,#14358,.T.);
#18898=ORIENTED_EDGE('',*,*,#14360,.F.);
#18899=ORIENTED_EDGE('',*,*,#14224,.F.);
#18900=ORIENTED_EDGE('',*,*,#14353,.T.);
#18901=ORIENTED_EDGE('',*,*,#14361,.F.);
#18902=ORIENTED_EDGE('',*,*,#14354,.F.);
#18903=ORIENTED_EDGE('',*,*,#14359,.T.);
#18904=ORIENTED_EDGE('',*,*,#14362,.F.);
#18905=ORIENTED_EDGE('',*,*,#14363,.T.);
#18906=ORIENTED_EDGE('',*,*,#14228,.T.);
#18907=ORIENTED_EDGE('',*,*,#14363,.F.);
#18908=ORIENTED_EDGE('',*,*,#14364,.F.);
#18909=ORIENTED_EDGE('',*,*,#14365,.F.);
#18910=ORIENTED_EDGE('',*,*,#14229,.T.);
#18911=ORIENTED_EDGE('',*,*,#14231,.F.);
#18912=ORIENTED_EDGE('',*,*,#14366,.T.);
#18913=ORIENTED_EDGE('',*,*,#14367,.F.);
#18914=ORIENTED_EDGE('',*,*,#14368,.F.);
#18915=ORIENTED_EDGE('',*,*,#14232,.T.);
#18916=ORIENTED_EDGE('',*,*,#14368,.T.);
#18917=ORIENTED_EDGE('',*,*,#14369,.F.);
#18918=ORIENTED_EDGE('',*,*,#14370,.F.);
#18919=ORIENTED_EDGE('',*,*,#14371,.F.);
#18920=ORIENTED_EDGE('',*,*,#14233,.T.);
#18921=ORIENTED_EDGE('',*,*,#14370,.T.);
#18922=ORIENTED_EDGE('',*,*,#14372,.F.);
#18923=ORIENTED_EDGE('',*,*,#14230,.F.);
#18924=ORIENTED_EDGE('',*,*,#14365,.T.);
#18925=ORIENTED_EDGE('',*,*,#14373,.F.);
#18926=ORIENTED_EDGE('',*,*,#14366,.F.);
#18927=ORIENTED_EDGE('',*,*,#14371,.T.);
#18928=ORIENTED_EDGE('',*,*,#14374,.F.);
#18929=ORIENTED_EDGE('',*,*,#14375,.T.);
#18930=ORIENTED_EDGE('',*,*,#14234,.T.);
#18931=ORIENTED_EDGE('',*,*,#14375,.F.);
#18932=ORIENTED_EDGE('',*,*,#14376,.F.);
#18933=ORIENTED_EDGE('',*,*,#14377,.F.);
#18934=ORIENTED_EDGE('',*,*,#14235,.T.);
#18935=ORIENTED_EDGE('',*,*,#14237,.F.);
#18936=ORIENTED_EDGE('',*,*,#14378,.T.);
#18937=ORIENTED_EDGE('',*,*,#14379,.F.);
#18938=ORIENTED_EDGE('',*,*,#14380,.F.);
#18939=ORIENTED_EDGE('',*,*,#14238,.T.);
#18940=ORIENTED_EDGE('',*,*,#14380,.T.);
#18941=ORIENTED_EDGE('',*,*,#14381,.F.);
#18942=ORIENTED_EDGE('',*,*,#14382,.F.);
#18943=ORIENTED_EDGE('',*,*,#14383,.F.);
#18944=ORIENTED_EDGE('',*,*,#14239,.T.);
#18945=ORIENTED_EDGE('',*,*,#14382,.T.);
#18946=ORIENTED_EDGE('',*,*,#14384,.F.);
#18947=ORIENTED_EDGE('',*,*,#14236,.F.);
#18948=ORIENTED_EDGE('',*,*,#14377,.T.);
#18949=ORIENTED_EDGE('',*,*,#14385,.F.);
#18950=ORIENTED_EDGE('',*,*,#14378,.F.);
#18951=ORIENTED_EDGE('',*,*,#14383,.T.);
#18952=ORIENTED_EDGE('',*,*,#14386,.F.);
#18953=ORIENTED_EDGE('',*,*,#14387,.T.);
#18954=ORIENTED_EDGE('',*,*,#14240,.T.);
#18955=ORIENTED_EDGE('',*,*,#14387,.F.);
#18956=ORIENTED_EDGE('',*,*,#14388,.F.);
#18957=ORIENTED_EDGE('',*,*,#14389,.F.);
#18958=ORIENTED_EDGE('',*,*,#14241,.T.);
#18959=ORIENTED_EDGE('',*,*,#14243,.F.);
#18960=ORIENTED_EDGE('',*,*,#14390,.T.);
#18961=ORIENTED_EDGE('',*,*,#14391,.F.);
#18962=ORIENTED_EDGE('',*,*,#14392,.F.);
#18963=ORIENTED_EDGE('',*,*,#14244,.T.);
#18964=ORIENTED_EDGE('',*,*,#14392,.T.);
#18965=ORIENTED_EDGE('',*,*,#14393,.F.);
#18966=ORIENTED_EDGE('',*,*,#14394,.F.);
#18967=ORIENTED_EDGE('',*,*,#14395,.F.);
#18968=ORIENTED_EDGE('',*,*,#14245,.T.);
#18969=ORIENTED_EDGE('',*,*,#14394,.T.);
#18970=ORIENTED_EDGE('',*,*,#14396,.F.);
#18971=ORIENTED_EDGE('',*,*,#14242,.F.);
#18972=ORIENTED_EDGE('',*,*,#14389,.T.);
#18973=ORIENTED_EDGE('',*,*,#14397,.F.);
#18974=ORIENTED_EDGE('',*,*,#14390,.F.);
#18975=ORIENTED_EDGE('',*,*,#14395,.T.);
#18976=ORIENTED_EDGE('',*,*,#14398,.F.);
#18977=ORIENTED_EDGE('',*,*,#14399,.T.);
#18978=ORIENTED_EDGE('',*,*,#14246,.T.);
#18979=ORIENTED_EDGE('',*,*,#14399,.F.);
#18980=ORIENTED_EDGE('',*,*,#14400,.F.);
#18981=ORIENTED_EDGE('',*,*,#14401,.F.);
#18982=ORIENTED_EDGE('',*,*,#14247,.T.);
#18983=ORIENTED_EDGE('',*,*,#14249,.F.);
#18984=ORIENTED_EDGE('',*,*,#14402,.T.);
#18985=ORIENTED_EDGE('',*,*,#14403,.F.);
#18986=ORIENTED_EDGE('',*,*,#14404,.F.);
#18987=ORIENTED_EDGE('',*,*,#14250,.T.);
#18988=ORIENTED_EDGE('',*,*,#14404,.T.);
#18989=ORIENTED_EDGE('',*,*,#14405,.F.);
#18990=ORIENTED_EDGE('',*,*,#14406,.F.);
#18991=ORIENTED_EDGE('',*,*,#14407,.F.);
#18992=ORIENTED_EDGE('',*,*,#14251,.T.);
#18993=ORIENTED_EDGE('',*,*,#14406,.T.);
#18994=ORIENTED_EDGE('',*,*,#14408,.F.);
#18995=ORIENTED_EDGE('',*,*,#14248,.F.);
#18996=ORIENTED_EDGE('',*,*,#14401,.T.);
#18997=ORIENTED_EDGE('',*,*,#14409,.F.);
#18998=ORIENTED_EDGE('',*,*,#14402,.F.);
#18999=ORIENTED_EDGE('',*,*,#14407,.T.);
#19000=ORIENTED_EDGE('',*,*,#14410,.F.);
#19001=ORIENTED_EDGE('',*,*,#14411,.T.);
#19002=ORIENTED_EDGE('',*,*,#14252,.T.);
#19003=ORIENTED_EDGE('',*,*,#14411,.F.);
#19004=ORIENTED_EDGE('',*,*,#14412,.F.);
#19005=ORIENTED_EDGE('',*,*,#14413,.F.);
#19006=ORIENTED_EDGE('',*,*,#14253,.T.);
#19007=ORIENTED_EDGE('',*,*,#14255,.F.);
#19008=ORIENTED_EDGE('',*,*,#14414,.T.);
#19009=ORIENTED_EDGE('',*,*,#14415,.F.);
#19010=ORIENTED_EDGE('',*,*,#14416,.F.);
#19011=ORIENTED_EDGE('',*,*,#14256,.T.);
#19012=ORIENTED_EDGE('',*,*,#14416,.T.);
#19013=ORIENTED_EDGE('',*,*,#14417,.F.);
#19014=ORIENTED_EDGE('',*,*,#14418,.F.);
#19015=ORIENTED_EDGE('',*,*,#14419,.F.);
#19016=ORIENTED_EDGE('',*,*,#14257,.T.);
#19017=ORIENTED_EDGE('',*,*,#14418,.T.);
#19018=ORIENTED_EDGE('',*,*,#14420,.F.);
#19019=ORIENTED_EDGE('',*,*,#14254,.F.);
#19020=ORIENTED_EDGE('',*,*,#14413,.T.);
#19021=ORIENTED_EDGE('',*,*,#14421,.F.);
#19022=ORIENTED_EDGE('',*,*,#14414,.F.);
#19023=ORIENTED_EDGE('',*,*,#14419,.T.);
#19024=ORIENTED_EDGE('',*,*,#14422,.F.);
#19025=ORIENTED_EDGE('',*,*,#14423,.T.);
#19026=ORIENTED_EDGE('',*,*,#14258,.T.);
#19027=ORIENTED_EDGE('',*,*,#14423,.F.);
#19028=ORIENTED_EDGE('',*,*,#14424,.F.);
#19029=ORIENTED_EDGE('',*,*,#14425,.F.);
#19030=ORIENTED_EDGE('',*,*,#14259,.T.);
#19031=ORIENTED_EDGE('',*,*,#14261,.F.);
#19032=ORIENTED_EDGE('',*,*,#14426,.T.);
#19033=ORIENTED_EDGE('',*,*,#14427,.F.);
#19034=ORIENTED_EDGE('',*,*,#14428,.F.);
#19035=ORIENTED_EDGE('',*,*,#14262,.T.);
#19036=ORIENTED_EDGE('',*,*,#14428,.T.);
#19037=ORIENTED_EDGE('',*,*,#14429,.F.);
#19038=ORIENTED_EDGE('',*,*,#14430,.F.);
#19039=ORIENTED_EDGE('',*,*,#14431,.F.);
#19040=ORIENTED_EDGE('',*,*,#14263,.T.);
#19041=ORIENTED_EDGE('',*,*,#14430,.T.);
#19042=ORIENTED_EDGE('',*,*,#14432,.F.);
#19043=ORIENTED_EDGE('',*,*,#14260,.F.);
#19044=ORIENTED_EDGE('',*,*,#14425,.T.);
#19045=ORIENTED_EDGE('',*,*,#14433,.F.);
#19046=ORIENTED_EDGE('',*,*,#14426,.F.);
#19047=ORIENTED_EDGE('',*,*,#14431,.T.);
#19048=ORIENTED_EDGE('',*,*,#14434,.F.);
#19049=ORIENTED_EDGE('',*,*,#14435,.T.);
#19050=ORIENTED_EDGE('',*,*,#14264,.T.);
#19051=ORIENTED_EDGE('',*,*,#14436,.F.);
#19052=ORIENTED_EDGE('',*,*,#14269,.T.);
#19053=ORIENTED_EDGE('',*,*,#14437,.T.);
#19054=ORIENTED_EDGE('',*,*,#14438,.F.);
#19055=ORIENTED_EDGE('',*,*,#14435,.F.);
#19056=ORIENTED_EDGE('',*,*,#14439,.F.);
#19057=ORIENTED_EDGE('',*,*,#14440,.F.);
#19058=ORIENTED_EDGE('',*,*,#14265,.T.);
#19059=ORIENTED_EDGE('',*,*,#14267,.F.);
#19060=ORIENTED_EDGE('',*,*,#14441,.T.);
#19061=ORIENTED_EDGE('',*,*,#14442,.F.);
#19062=ORIENTED_EDGE('',*,*,#14443,.F.);
#19063=ORIENTED_EDGE('',*,*,#14268,.T.);
#19064=ORIENTED_EDGE('',*,*,#14443,.T.);
#19065=ORIENTED_EDGE('',*,*,#14444,.F.);
#19066=ORIENTED_EDGE('',*,*,#14437,.F.);
#19067=ORIENTED_EDGE('',*,*,#14266,.F.);
#19068=ORIENTED_EDGE('',*,*,#14440,.T.);
#19069=ORIENTED_EDGE('',*,*,#14445,.F.);
#19070=ORIENTED_EDGE('',*,*,#14441,.F.);
#19071=ORIENTED_EDGE('',*,*,#14446,.T.);
#19072=ORIENTED_EDGE('',*,*,#14447,.T.);
#19073=ORIENTED_EDGE('',*,*,#14448,.T.);
#19074=ORIENTED_EDGE('',*,*,#14449,.T.);
#19075=ORIENTED_EDGE('',*,*,#14450,.T.);
#19076=ORIENTED_EDGE('',*,*,#14451,.T.);
#19077=ORIENTED_EDGE('',*,*,#14452,.T.);
#19078=ORIENTED_EDGE('',*,*,#14438,.T.);
#19079=ORIENTED_EDGE('',*,*,#14444,.T.);
#19080=ORIENTED_EDGE('',*,*,#14442,.T.);
#19081=ORIENTED_EDGE('',*,*,#14445,.T.);
#19082=ORIENTED_EDGE('',*,*,#14439,.T.);
#19083=ORIENTED_EDGE('',*,*,#14434,.T.);
#19084=ORIENTED_EDGE('',*,*,#14432,.T.);
#19085=ORIENTED_EDGE('',*,*,#14429,.T.);
#19086=ORIENTED_EDGE('',*,*,#14427,.T.);
#19087=ORIENTED_EDGE('',*,*,#14433,.T.);
#19088=ORIENTED_EDGE('',*,*,#14424,.T.);
#19089=ORIENTED_EDGE('',*,*,#14422,.T.);
#19090=ORIENTED_EDGE('',*,*,#14420,.T.);
#19091=ORIENTED_EDGE('',*,*,#14417,.T.);
#19092=ORIENTED_EDGE('',*,*,#14415,.T.);
#19093=ORIENTED_EDGE('',*,*,#14421,.T.);
#19094=ORIENTED_EDGE('',*,*,#14412,.T.);
#19095=ORIENTED_EDGE('',*,*,#14410,.T.);
#19096=ORIENTED_EDGE('',*,*,#14408,.T.);
#19097=ORIENTED_EDGE('',*,*,#14405,.T.);
#19098=ORIENTED_EDGE('',*,*,#14403,.T.);
#19099=ORIENTED_EDGE('',*,*,#14409,.T.);
#19100=ORIENTED_EDGE('',*,*,#14400,.T.);
#19101=ORIENTED_EDGE('',*,*,#14398,.T.);
#19102=ORIENTED_EDGE('',*,*,#14396,.T.);
#19103=ORIENTED_EDGE('',*,*,#14393,.T.);
#19104=ORIENTED_EDGE('',*,*,#14391,.T.);
#19105=ORIENTED_EDGE('',*,*,#14397,.T.);
#19106=ORIENTED_EDGE('',*,*,#14388,.T.);
#19107=ORIENTED_EDGE('',*,*,#14386,.T.);
#19108=ORIENTED_EDGE('',*,*,#14384,.T.);
#19109=ORIENTED_EDGE('',*,*,#14381,.T.);
#19110=ORIENTED_EDGE('',*,*,#14379,.T.);
#19111=ORIENTED_EDGE('',*,*,#14385,.T.);
#19112=ORIENTED_EDGE('',*,*,#14376,.T.);
#19113=ORIENTED_EDGE('',*,*,#14374,.T.);
#19114=ORIENTED_EDGE('',*,*,#14372,.T.);
#19115=ORIENTED_EDGE('',*,*,#14369,.T.);
#19116=ORIENTED_EDGE('',*,*,#14367,.T.);
#19117=ORIENTED_EDGE('',*,*,#14373,.T.);
#19118=ORIENTED_EDGE('',*,*,#14364,.T.);
#19119=ORIENTED_EDGE('',*,*,#14362,.T.);
#19120=ORIENTED_EDGE('',*,*,#14360,.T.);
#19121=ORIENTED_EDGE('',*,*,#14357,.T.);
#19122=ORIENTED_EDGE('',*,*,#14355,.T.);
#19123=ORIENTED_EDGE('',*,*,#14361,.T.);
#19124=ORIENTED_EDGE('',*,*,#14352,.T.);
#19125=ORIENTED_EDGE('',*,*,#14350,.T.);
#19126=ORIENTED_EDGE('',*,*,#14348,.T.);
#19127=ORIENTED_EDGE('',*,*,#14345,.T.);
#19128=ORIENTED_EDGE('',*,*,#14343,.T.);
#19129=ORIENTED_EDGE('',*,*,#14349,.T.);
#19130=ORIENTED_EDGE('',*,*,#14340,.T.);
#19131=ORIENTED_EDGE('',*,*,#14338,.T.);
#19132=ORIENTED_EDGE('',*,*,#14336,.T.);
#19133=ORIENTED_EDGE('',*,*,#14333,.T.);
#19134=ORIENTED_EDGE('',*,*,#14331,.T.);
#19135=ORIENTED_EDGE('',*,*,#14337,.T.);
#19136=ORIENTED_EDGE('',*,*,#14328,.T.);
#19137=ORIENTED_EDGE('',*,*,#14326,.T.);
#19138=ORIENTED_EDGE('',*,*,#14324,.T.);
#19139=ORIENTED_EDGE('',*,*,#14321,.T.);
#19140=ORIENTED_EDGE('',*,*,#14319,.T.);
#19141=ORIENTED_EDGE('',*,*,#14325,.T.);
#19142=ORIENTED_EDGE('',*,*,#14316,.T.);
#19143=ORIENTED_EDGE('',*,*,#14314,.T.);
#19144=ORIENTED_EDGE('',*,*,#14312,.T.);
#19145=ORIENTED_EDGE('',*,*,#14309,.T.);
#19146=ORIENTED_EDGE('',*,*,#14307,.T.);
#19147=ORIENTED_EDGE('',*,*,#14313,.T.);
#19148=ORIENTED_EDGE('',*,*,#14304,.T.);
#19149=ORIENTED_EDGE('',*,*,#14302,.T.);
#19150=ORIENTED_EDGE('',*,*,#14300,.T.);
#19151=ORIENTED_EDGE('',*,*,#14297,.T.);
#19152=ORIENTED_EDGE('',*,*,#14295,.T.);
#19153=ORIENTED_EDGE('',*,*,#14301,.T.);
#19154=ORIENTED_EDGE('',*,*,#14292,.T.);
#19155=ORIENTED_EDGE('',*,*,#14290,.T.);
#19156=ORIENTED_EDGE('',*,*,#14288,.T.);
#19157=ORIENTED_EDGE('',*,*,#14285,.T.);
#19158=ORIENTED_EDGE('',*,*,#14283,.T.);
#19159=ORIENTED_EDGE('',*,*,#14289,.T.);
#19160=ORIENTED_EDGE('',*,*,#14280,.T.);
#19161=ORIENTED_EDGE('',*,*,#14278,.T.);
#19162=ORIENTED_EDGE('',*,*,#14183,.T.);
#19163=ORIENTED_EDGE('',*,*,#14179,.T.);
#19164=ORIENTED_EDGE('',*,*,#14176,.T.);
#19165=ORIENTED_EDGE('',*,*,#14185,.T.);
#19166=ORIENTED_EDGE('',*,*,#14171,.T.);
#19167=ORIENTED_EDGE('',*,*,#14453,.F.);
#19168=ORIENTED_EDGE('',*,*,#14170,.T.);
#19169=ORIENTED_EDGE('',*,*,#14276,.T.);
#19170=ORIENTED_EDGE('',*,*,#14454,.T.);
#19171=ORIENTED_EDGE('',*,*,#14446,.F.);
#19172=ORIENTED_EDGE('',*,*,#14454,.F.);
#19173=ORIENTED_EDGE('',*,*,#14275,.T.);
#19174=ORIENTED_EDGE('',*,*,#14455,.T.);
#19175=ORIENTED_EDGE('',*,*,#14447,.F.);
#19176=ORIENTED_EDGE('',*,*,#14273,.F.);
#19177=ORIENTED_EDGE('',*,*,#14456,.T.);
#19178=ORIENTED_EDGE('',*,*,#14449,.F.);
#19179=ORIENTED_EDGE('',*,*,#14457,.F.);
#19180=ORIENTED_EDGE('',*,*,#14274,.T.);
#19181=ORIENTED_EDGE('',*,*,#14457,.T.);
#19182=ORIENTED_EDGE('',*,*,#14448,.F.);
#19183=ORIENTED_EDGE('',*,*,#14455,.F.);
#19184=ORIENTED_EDGE('',*,*,#14458,.F.);
#19185=ORIENTED_EDGE('',*,*,#14451,.F.);
#19186=ORIENTED_EDGE('',*,*,#14459,.F.);
#19187=ORIENTED_EDGE('',*,*,#14271,.T.);
#19188=ORIENTED_EDGE('',*,*,#14272,.F.);
#19189=ORIENTED_EDGE('',*,*,#14459,.T.);
#19190=ORIENTED_EDGE('',*,*,#14450,.F.);
#19191=ORIENTED_EDGE('',*,*,#14456,.F.);
#19192=ORIENTED_EDGE('',*,*,#14436,.T.);
#19193=ORIENTED_EDGE('',*,*,#14452,.F.);
#19194=ORIENTED_EDGE('',*,*,#14458,.T.);
#19195=ORIENTED_EDGE('',*,*,#14270,.T.);
#19196=ORIENTED_EDGE('',*,*,#14460,.T.);
#19197=ORIENTED_EDGE('',*,*,#14461,.F.);
#19198=ORIENTED_EDGE('',*,*,#14462,.F.);
#19199=ORIENTED_EDGE('',*,*,#14463,.T.);
#19200=ORIENTED_EDGE('',*,*,#14461,.T.);
#19201=ORIENTED_EDGE('',*,*,#14463,.F.);
#19202=ORIENTED_EDGE('',*,*,#14464,.F.);
#19203=ORIENTED_EDGE('',*,*,#14462,.T.);
#19204=ORIENTED_EDGE('',*,*,#14277,.F.);
#19205=ORIENTED_EDGE('',*,*,#14465,.T.);
#19206=ORIENTED_EDGE('',*,*,#14464,.T.);
#19207=ORIENTED_EDGE('',*,*,#14465,.F.);
#19208=ORIENTED_EDGE('',*,*,#14460,.F.);
#19209=ORIENTED_EDGE('',*,*,#14466,.T.);
#19210=ORIENTED_EDGE('',*,*,#14453,.T.);
#19211=ORIENTED_EDGE('',*,*,#14466,.F.);
#19212=ORIENTED_EDGE('',*,*,#14467,.F.);
#19213=ORIENTED_EDGE('',*,*,#14468,.F.);
#19214=ORIENTED_EDGE('',*,*,#14469,.F.);
#19215=ORIENTED_EDGE('',*,*,#14470,.T.);
#19216=ORIENTED_EDGE('',*,*,#14471,.F.);
#19217=ORIENTED_EDGE('',*,*,#14472,.F.);
#19218=ORIENTED_EDGE('',*,*,#14473,.F.);
#19219=ORIENTED_EDGE('',*,*,#14467,.T.);
#19220=ORIENTED_EDGE('',*,*,#14474,.T.);
#19221=ORIENTED_EDGE('',*,*,#14475,.T.);
#19222=ORIENTED_EDGE('',*,*,#14476,.F.);
#19223=ORIENTED_EDGE('',*,*,#14477,.F.);
#19224=ORIENTED_EDGE('',*,*,#14478,.F.);
#19225=ORIENTED_EDGE('',*,*,#14471,.T.);
#19226=ORIENTED_EDGE('',*,*,#14479,.T.);
#19227=ORIENTED_EDGE('',*,*,#14480,.F.);
#19228=ORIENTED_EDGE('',*,*,#14481,.F.);
#19229=ORIENTED_EDGE('',*,*,#14482,.F.);
#19230=ORIENTED_EDGE('',*,*,#14476,.T.);
#19231=ORIENTED_EDGE('',*,*,#14483,.T.);
#19232=ORIENTED_EDGE('',*,*,#14484,.T.);
#19233=ORIENTED_EDGE('',*,*,#14485,.F.);
#19234=ORIENTED_EDGE('',*,*,#14486,.F.);
#19235=ORIENTED_EDGE('',*,*,#14480,.T.);
#19236=ORIENTED_EDGE('',*,*,#14487,.T.);
#19237=ORIENTED_EDGE('',*,*,#14488,.F.);
#19238=ORIENTED_EDGE('',*,*,#14489,.F.);
#19239=ORIENTED_EDGE('',*,*,#14490,.F.);
#19240=ORIENTED_EDGE('',*,*,#14485,.T.);
#19241=ORIENTED_EDGE('',*,*,#14491,.T.);
#19242=ORIENTED_EDGE('',*,*,#14492,.T.);
#19243=ORIENTED_EDGE('',*,*,#14493,.F.);
#19244=ORIENTED_EDGE('',*,*,#14494,.F.);
#19245=ORIENTED_EDGE('',*,*,#14488,.T.);
#19246=ORIENTED_EDGE('',*,*,#14495,.T.);
#19247=ORIENTED_EDGE('',*,*,#14496,.F.);
#19248=ORIENTED_EDGE('',*,*,#14497,.F.);
#19249=ORIENTED_EDGE('',*,*,#14498,.F.);
#19250=ORIENTED_EDGE('',*,*,#14493,.T.);
#19251=ORIENTED_EDGE('',*,*,#14499,.T.);
#19252=ORIENTED_EDGE('',*,*,#14500,.T.);
#19253=ORIENTED_EDGE('',*,*,#14501,.F.);
#19254=ORIENTED_EDGE('',*,*,#14502,.F.);
#19255=ORIENTED_EDGE('',*,*,#14503,.F.);
#19256=ORIENTED_EDGE('',*,*,#14496,.T.);
#19257=ORIENTED_EDGE('',*,*,#14504,.T.);
#19258=ORIENTED_EDGE('',*,*,#14505,.F.);
#19259=ORIENTED_EDGE('',*,*,#14506,.F.);
#19260=ORIENTED_EDGE('',*,*,#14501,.T.);
#19261=ORIENTED_EDGE('',*,*,#14507,.T.);
#19262=ORIENTED_EDGE('',*,*,#14508,.T.);
#19263=ORIENTED_EDGE('',*,*,#14509,.F.);
#19264=ORIENTED_EDGE('',*,*,#14510,.F.);
#19265=ORIENTED_EDGE('',*,*,#14511,.F.);
#19266=ORIENTED_EDGE('',*,*,#14505,.T.);
#19267=ORIENTED_EDGE('',*,*,#14512,.T.);
#19268=ORIENTED_EDGE('',*,*,#14513,.T.);
#19269=ORIENTED_EDGE('',*,*,#14514,.F.);
#19270=ORIENTED_EDGE('',*,*,#14515,.T.);
#19271=ORIENTED_EDGE('',*,*,#14516,.F.);
#19272=ORIENTED_EDGE('',*,*,#14517,.T.);
#19273=ORIENTED_EDGE('',*,*,#14518,.F.);
#19274=ORIENTED_EDGE('',*,*,#14519,.T.);
#19275=ORIENTED_EDGE('',*,*,#14514,.T.);
#19276=ORIENTED_EDGE('',*,*,#14520,.T.);
#19277=ORIENTED_EDGE('',*,*,#14521,.F.);
#19278=ORIENTED_EDGE('',*,*,#14522,.T.);
#19279=ORIENTED_EDGE('',*,*,#14518,.T.);
#19280=ORIENTED_EDGE('',*,*,#14523,.T.);
#19281=ORIENTED_EDGE('',*,*,#14524,.F.);
#19282=ORIENTED_EDGE('',*,*,#14525,.T.);
#19283=ORIENTED_EDGE('',*,*,#14521,.T.);
#19284=ORIENTED_EDGE('',*,*,#14526,.T.);
#19285=ORIENTED_EDGE('',*,*,#14527,.F.);
#19286=ORIENTED_EDGE('',*,*,#14528,.T.);
#19287=ORIENTED_EDGE('',*,*,#14524,.T.);
#19288=ORIENTED_EDGE('',*,*,#14529,.T.);
#19289=ORIENTED_EDGE('',*,*,#14530,.F.);
#19290=ORIENTED_EDGE('',*,*,#14531,.T.);
#19291=ORIENTED_EDGE('',*,*,#14527,.T.);
#19292=ORIENTED_EDGE('',*,*,#14532,.T.);
#19293=ORIENTED_EDGE('',*,*,#14533,.F.);
#19294=ORIENTED_EDGE('',*,*,#14534,.T.);
#19295=ORIENTED_EDGE('',*,*,#14530,.T.);
#19296=ORIENTED_EDGE('',*,*,#14535,.T.);
#19297=ORIENTED_EDGE('',*,*,#14536,.F.);
#19298=ORIENTED_EDGE('',*,*,#14537,.T.);
#19299=ORIENTED_EDGE('',*,*,#14533,.T.);
#19300=ORIENTED_EDGE('',*,*,#14538,.T.);
#19301=ORIENTED_EDGE('',*,*,#14539,.F.);
#19302=ORIENTED_EDGE('',*,*,#14540,.T.);
#19303=ORIENTED_EDGE('',*,*,#14536,.T.);
#19304=ORIENTED_EDGE('',*,*,#14541,.T.);
#19305=ORIENTED_EDGE('',*,*,#14542,.F.);
#19306=ORIENTED_EDGE('',*,*,#14543,.T.);
#19307=ORIENTED_EDGE('',*,*,#14539,.T.);
#19308=ORIENTED_EDGE('',*,*,#14544,.T.);
#19309=ORIENTED_EDGE('',*,*,#14545,.F.);
#19310=ORIENTED_EDGE('',*,*,#14546,.T.);
#19311=ORIENTED_EDGE('',*,*,#14542,.T.);
#19312=ORIENTED_EDGE('',*,*,#14547,.T.);
#19313=ORIENTED_EDGE('',*,*,#14545,.T.);
#19314=ORIENTED_EDGE('',*,*,#14548,.T.);
#19315=ORIENTED_EDGE('',*,*,#14549,.F.);
#19316=ORIENTED_EDGE('',*,*,#14550,.T.);
#19317=ORIENTED_EDGE('',*,*,#14509,.T.);
#19318=ORIENTED_EDGE('',*,*,#14551,.T.);
#19319=ORIENTED_EDGE('',*,*,#14552,.T.);
#19320=ORIENTED_EDGE('',*,*,#14553,.F.);
#19321=ORIENTED_EDGE('',*,*,#14554,.F.);
#19322=ORIENTED_EDGE('',*,*,#14555,.F.);
#19323=ORIENTED_EDGE('',*,*,#14556,.F.);
#19324=ORIENTED_EDGE('',*,*,#14557,.T.);
#19325=ORIENTED_EDGE('',*,*,#14553,.T.);
#19326=ORIENTED_EDGE('',*,*,#14558,.T.);
#19327=ORIENTED_EDGE('',*,*,#14559,.F.);
#19328=ORIENTED_EDGE('',*,*,#14557,.F.);
#19329=ORIENTED_EDGE('',*,*,#14560,.F.);
#19330=ORIENTED_EDGE('',*,*,#14548,.F.);
#19331=ORIENTED_EDGE('',*,*,#14547,.F.);
#19332=ORIENTED_EDGE('',*,*,#14544,.F.);
#19333=ORIENTED_EDGE('',*,*,#14541,.F.);
#19334=ORIENTED_EDGE('',*,*,#14538,.F.);
#19335=ORIENTED_EDGE('',*,*,#14535,.F.);
#19336=ORIENTED_EDGE('',*,*,#14532,.F.);
#19337=ORIENTED_EDGE('',*,*,#14529,.F.);
#19338=ORIENTED_EDGE('',*,*,#14526,.F.);
#19339=ORIENTED_EDGE('',*,*,#14523,.F.);
#19340=ORIENTED_EDGE('',*,*,#14520,.F.);
#19341=ORIENTED_EDGE('',*,*,#14517,.F.);
#19342=ORIENTED_EDGE('',*,*,#14561,.F.);
#19343=ORIENTED_EDGE('',*,*,#14468,.T.);
#19344=ORIENTED_EDGE('',*,*,#14473,.T.);
#19345=ORIENTED_EDGE('',*,*,#14472,.T.);
#19346=ORIENTED_EDGE('',*,*,#14478,.T.);
#19347=ORIENTED_EDGE('',*,*,#14477,.T.);
#19348=ORIENTED_EDGE('',*,*,#14482,.T.);
#19349=ORIENTED_EDGE('',*,*,#14481,.T.);
#19350=ORIENTED_EDGE('',*,*,#14486,.T.);
#19351=ORIENTED_EDGE('',*,*,#14490,.T.);
#19352=ORIENTED_EDGE('',*,*,#14489,.T.);
#19353=ORIENTED_EDGE('',*,*,#14494,.T.);
#19354=ORIENTED_EDGE('',*,*,#14498,.T.);
#19355=ORIENTED_EDGE('',*,*,#14497,.T.);
#19356=ORIENTED_EDGE('',*,*,#14503,.T.);
#19357=ORIENTED_EDGE('',*,*,#14502,.T.);
#19358=ORIENTED_EDGE('',*,*,#14506,.T.);
#19359=ORIENTED_EDGE('',*,*,#14511,.T.);
#19360=ORIENTED_EDGE('',*,*,#14510,.T.);
#19361=ORIENTED_EDGE('',*,*,#14555,.T.);
#19362=ORIENTED_EDGE('',*,*,#14554,.T.);
#19363=ORIENTED_EDGE('',*,*,#14562,.F.);
#19364=ORIENTED_EDGE('',*,*,#14563,.T.);
#19365=ORIENTED_EDGE('',*,*,#14469,.T.);
#19366=ORIENTED_EDGE('',*,*,#14561,.T.);
#19367=ORIENTED_EDGE('',*,*,#14564,.F.);
#19368=ORIENTED_EDGE('',*,*,#14558,.F.);
#19369=ORIENTED_EDGE('',*,*,#14552,.F.);
#19370=ORIENTED_EDGE('',*,*,#14551,.F.);
#19371=ORIENTED_EDGE('',*,*,#14513,.F.);
#19372=ORIENTED_EDGE('',*,*,#14512,.F.);
#19373=ORIENTED_EDGE('',*,*,#14508,.F.);
#19374=ORIENTED_EDGE('',*,*,#14507,.F.);
#19375=ORIENTED_EDGE('',*,*,#14504,.F.);
#19376=ORIENTED_EDGE('',*,*,#14500,.F.);
#19377=ORIENTED_EDGE('',*,*,#14499,.F.);
#19378=ORIENTED_EDGE('',*,*,#14495,.F.);
#19379=ORIENTED_EDGE('',*,*,#14492,.F.);
#19380=ORIENTED_EDGE('',*,*,#14491,.F.);
#19381=ORIENTED_EDGE('',*,*,#14487,.F.);
#19382=ORIENTED_EDGE('',*,*,#14484,.F.);
#19383=ORIENTED_EDGE('',*,*,#14483,.F.);
#19384=ORIENTED_EDGE('',*,*,#14479,.F.);
#19385=ORIENTED_EDGE('',*,*,#14475,.F.);
#19386=ORIENTED_EDGE('',*,*,#14474,.F.);
#19387=ORIENTED_EDGE('',*,*,#14470,.F.);
#19388=ORIENTED_EDGE('',*,*,#14563,.F.);
#19389=ORIENTED_EDGE('',*,*,#14565,.F.);
#19390=ORIENTED_EDGE('',*,*,#14515,.F.);
#19391=ORIENTED_EDGE('',*,*,#14519,.F.);
#19392=ORIENTED_EDGE('',*,*,#14522,.F.);
#19393=ORIENTED_EDGE('',*,*,#14525,.F.);
#19394=ORIENTED_EDGE('',*,*,#14528,.F.);
#19395=ORIENTED_EDGE('',*,*,#14531,.F.);
#19396=ORIENTED_EDGE('',*,*,#14534,.F.);
#19397=ORIENTED_EDGE('',*,*,#14537,.F.);
#19398=ORIENTED_EDGE('',*,*,#14540,.F.);
#19399=ORIENTED_EDGE('',*,*,#14543,.F.);
#19400=ORIENTED_EDGE('',*,*,#14546,.F.);
#19401=ORIENTED_EDGE('',*,*,#14550,.F.);
#19402=ORIENTED_EDGE('',*,*,#14566,.T.);
#19403=ORIENTED_EDGE('',*,*,#14567,.T.);
#19404=ORIENTED_EDGE('',*,*,#14564,.T.);
#19405=ORIENTED_EDGE('',*,*,#14516,.T.);
#19406=ORIENTED_EDGE('',*,*,#14565,.T.);
#19407=ORIENTED_EDGE('',*,*,#14562,.T.);
#19408=ORIENTED_EDGE('',*,*,#14567,.F.);
#19409=ORIENTED_EDGE('',*,*,#14568,.F.);
#19410=ORIENTED_EDGE('',*,*,#14566,.F.);
#19411=ORIENTED_EDGE('',*,*,#14556,.T.);
#19412=ORIENTED_EDGE('',*,*,#14569,.T.);
#19413=ORIENTED_EDGE('',*,*,#14570,.T.);
#19414=ORIENTED_EDGE('',*,*,#14569,.F.);
#19415=ORIENTED_EDGE('',*,*,#14559,.T.);
#19416=ORIENTED_EDGE('',*,*,#14549,.T.);
#19417=ORIENTED_EDGE('',*,*,#14560,.T.);
#19418=ORIENTED_EDGE('',*,*,#14570,.F.);
#19419=ORIENTED_EDGE('',*,*,#14571,.F.);
#19420=ORIENTED_EDGE('',*,*,#14572,.T.);
#19421=ORIENTED_EDGE('',*,*,#14573,.T.);
#19422=ORIENTED_EDGE('',*,*,#14574,.F.);
#19423=ORIENTED_EDGE('',*,*,#14575,.F.);
#19424=ORIENTED_EDGE('',*,*,#14573,.F.);
#19425=ORIENTED_EDGE('',*,*,#14576,.F.);
#19426=ORIENTED_EDGE('',*,*,#14577,.F.);
#19427=ORIENTED_EDGE('',*,*,#14578,.F.);
#19428=ORIENTED_EDGE('',*,*,#14576,.T.);
#19429=ORIENTED_EDGE('',*,*,#14572,.F.);
#19430=ORIENTED_EDGE('',*,*,#14579,.T.);
#19431=ORIENTED_EDGE('',*,*,#14580,.T.);
#19432=ORIENTED_EDGE('',*,*,#14581,.F.);
#19433=ORIENTED_EDGE('',*,*,#14582,.F.);
#19434=ORIENTED_EDGE('',*,*,#14580,.F.);
#19435=ORIENTED_EDGE('',*,*,#14583,.T.);
#19436=ORIENTED_EDGE('',*,*,#14584,.T.);
#19437=ORIENTED_EDGE('',*,*,#14585,.F.);
#19438=ORIENTED_EDGE('',*,*,#14586,.T.);
#19439=ORIENTED_EDGE('',*,*,#14587,.T.);
#19440=ORIENTED_EDGE('',*,*,#14588,.T.);
#19441=ORIENTED_EDGE('',*,*,#14589,.F.);
#19442=ORIENTED_EDGE('',*,*,#14590,.T.);
#19443=ORIENTED_EDGE('',*,*,#14591,.T.);
#19444=ORIENTED_EDGE('',*,*,#14592,.T.);
#19445=ORIENTED_EDGE('',*,*,#14593,.F.);
#19446=ORIENTED_EDGE('',*,*,#14594,.T.);
#19447=ORIENTED_EDGE('',*,*,#14595,.T.);
#19448=ORIENTED_EDGE('',*,*,#14596,.T.);
#19449=ORIENTED_EDGE('',*,*,#14597,.F.);
#19450=ORIENTED_EDGE('',*,*,#14598,.T.);
#19451=ORIENTED_EDGE('',*,*,#14599,.T.);
#19452=ORIENTED_EDGE('',*,*,#14600,.T.);
#19453=ORIENTED_EDGE('',*,*,#14601,.F.);
#19454=ORIENTED_EDGE('',*,*,#14602,.T.);
#19455=ORIENTED_EDGE('',*,*,#14603,.T.);
#19456=ORIENTED_EDGE('',*,*,#14604,.T.);
#19457=ORIENTED_EDGE('',*,*,#14605,.F.);
#19458=ORIENTED_EDGE('',*,*,#14606,.T.);
#19459=ORIENTED_EDGE('',*,*,#14607,.T.);
#19460=ORIENTED_EDGE('',*,*,#14608,.T.);
#19461=ORIENTED_EDGE('',*,*,#14609,.F.);
#19462=ORIENTED_EDGE('',*,*,#14610,.T.);
#19463=ORIENTED_EDGE('',*,*,#14611,.T.);
#19464=ORIENTED_EDGE('',*,*,#14612,.T.);
#19465=ORIENTED_EDGE('',*,*,#14613,.F.);
#19466=ORIENTED_EDGE('',*,*,#14614,.T.);
#19467=ORIENTED_EDGE('',*,*,#14615,.T.);
#19468=ORIENTED_EDGE('',*,*,#14616,.T.);
#19469=ORIENTED_EDGE('',*,*,#14617,.F.);
#19470=ORIENTED_EDGE('',*,*,#14618,.T.);
#19471=ORIENTED_EDGE('',*,*,#14619,.T.);
#19472=ORIENTED_EDGE('',*,*,#14620,.T.);
#19473=ORIENTED_EDGE('',*,*,#14621,.F.);
#19474=ORIENTED_EDGE('',*,*,#14622,.T.);
#19475=ORIENTED_EDGE('',*,*,#14623,.T.);
#19476=ORIENTED_EDGE('',*,*,#14624,.T.);
#19477=ORIENTED_EDGE('',*,*,#14625,.F.);
#19478=ORIENTED_EDGE('',*,*,#14626,.T.);
#19479=ORIENTED_EDGE('',*,*,#14627,.T.);
#19480=ORIENTED_EDGE('',*,*,#14628,.T.);
#19481=ORIENTED_EDGE('',*,*,#14629,.F.);
#19482=ORIENTED_EDGE('',*,*,#14630,.T.);
#19483=ORIENTED_EDGE('',*,*,#14631,.T.);
#19484=ORIENTED_EDGE('',*,*,#14632,.T.);
#19485=ORIENTED_EDGE('',*,*,#14633,.F.);
#19486=ORIENTED_EDGE('',*,*,#14634,.T.);
#19487=ORIENTED_EDGE('',*,*,#14635,.T.);
#19488=ORIENTED_EDGE('',*,*,#14636,.T.);
#19489=ORIENTED_EDGE('',*,*,#14637,.F.);
#19490=ORIENTED_EDGE('',*,*,#14638,.T.);
#19491=ORIENTED_EDGE('',*,*,#14639,.T.);
#19492=ORIENTED_EDGE('',*,*,#14640,.T.);
#19493=ORIENTED_EDGE('',*,*,#14641,.F.);
#19494=ORIENTED_EDGE('',*,*,#14642,.T.);
#19495=ORIENTED_EDGE('',*,*,#14643,.T.);
#19496=ORIENTED_EDGE('',*,*,#14644,.T.);
#19497=ORIENTED_EDGE('',*,*,#14645,.F.);
#19498=ORIENTED_EDGE('',*,*,#14646,.T.);
#19499=ORIENTED_EDGE('',*,*,#14647,.T.);
#19500=ORIENTED_EDGE('',*,*,#14648,.T.);
#19501=ORIENTED_EDGE('',*,*,#14649,.F.);
#19502=ORIENTED_EDGE('',*,*,#14574,.T.);
#19503=ORIENTED_EDGE('',*,*,#14575,.T.);
#19504=ORIENTED_EDGE('',*,*,#14578,.T.);
#19505=ORIENTED_EDGE('',*,*,#14650,.F.);
#19506=ORIENTED_EDGE('',*,*,#14651,.T.);
#19507=ORIENTED_EDGE('',*,*,#14652,.T.);
#19508=ORIENTED_EDGE('',*,*,#14653,.T.);
#19509=ORIENTED_EDGE('',*,*,#14654,.F.);
#19510=ORIENTED_EDGE('',*,*,#14655,.T.);
#19511=ORIENTED_EDGE('',*,*,#14656,.T.);
#19512=ORIENTED_EDGE('',*,*,#14657,.T.);
#19513=ORIENTED_EDGE('',*,*,#14658,.F.);
#19514=ORIENTED_EDGE('',*,*,#14659,.T.);
#19515=ORIENTED_EDGE('',*,*,#14660,.T.);
#19516=ORIENTED_EDGE('',*,*,#14661,.T.);
#19517=ORIENTED_EDGE('',*,*,#14662,.F.);
#19518=ORIENTED_EDGE('',*,*,#14663,.T.);
#19519=ORIENTED_EDGE('',*,*,#14664,.T.);
#19520=ORIENTED_EDGE('',*,*,#14665,.T.);
#19521=ORIENTED_EDGE('',*,*,#14666,.F.);
#19522=ORIENTED_EDGE('',*,*,#14667,.T.);
#19523=ORIENTED_EDGE('',*,*,#14668,.T.);
#19524=ORIENTED_EDGE('',*,*,#14669,.T.);
#19525=ORIENTED_EDGE('',*,*,#14670,.F.);
#19526=ORIENTED_EDGE('',*,*,#14671,.T.);
#19527=ORIENTED_EDGE('',*,*,#14672,.T.);
#19528=ORIENTED_EDGE('',*,*,#14673,.T.);
#19529=ORIENTED_EDGE('',*,*,#14674,.F.);
#19530=ORIENTED_EDGE('',*,*,#14675,.T.);
#19531=ORIENTED_EDGE('',*,*,#14676,.T.);
#19532=ORIENTED_EDGE('',*,*,#14677,.T.);
#19533=ORIENTED_EDGE('',*,*,#14678,.F.);
#19534=ORIENTED_EDGE('',*,*,#14679,.T.);
#19535=ORIENTED_EDGE('',*,*,#14680,.T.);
#19536=ORIENTED_EDGE('',*,*,#14681,.T.);
#19537=ORIENTED_EDGE('',*,*,#14682,.F.);
#19538=ORIENTED_EDGE('',*,*,#14683,.T.);
#19539=ORIENTED_EDGE('',*,*,#14684,.T.);
#19540=ORIENTED_EDGE('',*,*,#14685,.T.);
#19541=ORIENTED_EDGE('',*,*,#14686,.F.);
#19542=ORIENTED_EDGE('',*,*,#14687,.T.);
#19543=ORIENTED_EDGE('',*,*,#14688,.T.);
#19544=ORIENTED_EDGE('',*,*,#14689,.T.);
#19545=ORIENTED_EDGE('',*,*,#14690,.F.);
#19546=ORIENTED_EDGE('',*,*,#14691,.T.);
#19547=ORIENTED_EDGE('',*,*,#14692,.T.);
#19548=ORIENTED_EDGE('',*,*,#14693,.T.);
#19549=ORIENTED_EDGE('',*,*,#14694,.F.);
#19550=ORIENTED_EDGE('',*,*,#14695,.T.);
#19551=ORIENTED_EDGE('',*,*,#14696,.T.);
#19552=ORIENTED_EDGE('',*,*,#14697,.T.);
#19553=ORIENTED_EDGE('',*,*,#14698,.F.);
#19554=ORIENTED_EDGE('',*,*,#14699,.T.);
#19555=ORIENTED_EDGE('',*,*,#14700,.T.);
#19556=ORIENTED_EDGE('',*,*,#14701,.T.);
#19557=ORIENTED_EDGE('',*,*,#14702,.F.);
#19558=ORIENTED_EDGE('',*,*,#14703,.T.);
#19559=ORIENTED_EDGE('',*,*,#14704,.T.);
#19560=ORIENTED_EDGE('',*,*,#14705,.T.);
#19561=ORIENTED_EDGE('',*,*,#14706,.F.);
#19562=ORIENTED_EDGE('',*,*,#14707,.T.);
#19563=ORIENTED_EDGE('',*,*,#14708,.T.);
#19564=ORIENTED_EDGE('',*,*,#14709,.T.);
#19565=ORIENTED_EDGE('',*,*,#14710,.F.);
#19566=ORIENTED_EDGE('',*,*,#14711,.T.);
#19567=ORIENTED_EDGE('',*,*,#14712,.T.);
#19568=ORIENTED_EDGE('',*,*,#14713,.T.);
#19569=ORIENTED_EDGE('',*,*,#14714,.F.);
#19570=ORIENTED_EDGE('',*,*,#14715,.T.);
#19571=ORIENTED_EDGE('',*,*,#14716,.T.);
#19572=ORIENTED_EDGE('',*,*,#14717,.T.);
#19573=ORIENTED_EDGE('',*,*,#14718,.F.);
#19574=ORIENTED_EDGE('',*,*,#14719,.T.);
#19575=ORIENTED_EDGE('',*,*,#14720,.T.);
#19576=ORIENTED_EDGE('',*,*,#14721,.T.);
#19577=ORIENTED_EDGE('',*,*,#14722,.F.);
#19578=ORIENTED_EDGE('',*,*,#14723,.T.);
#19579=ORIENTED_EDGE('',*,*,#14724,.F.);
#19580=ORIENTED_EDGE('',*,*,#14725,.T.);
#19581=ORIENTED_EDGE('',*,*,#14726,.T.);
#19582=ORIENTED_EDGE('',*,*,#14646,.F.);
#19583=ORIENTED_EDGE('',*,*,#14647,.F.);
#19584=ORIENTED_EDGE('',*,*,#14726,.F.);
#19585=ORIENTED_EDGE('',*,*,#14727,.F.);
#19586=ORIENTED_EDGE('',*,*,#14728,.F.);
#19587=ORIENTED_EDGE('',*,*,#14648,.F.);
#19588=ORIENTED_EDGE('',*,*,#14727,.T.);
#19589=ORIENTED_EDGE('',*,*,#14725,.F.);
#19590=ORIENTED_EDGE('',*,*,#14729,.F.);
#19591=ORIENTED_EDGE('',*,*,#14730,.T.);
#19592=ORIENTED_EDGE('',*,*,#14731,.T.);
#19593=ORIENTED_EDGE('',*,*,#14642,.F.);
#19594=ORIENTED_EDGE('',*,*,#14643,.F.);
#19595=ORIENTED_EDGE('',*,*,#14731,.F.);
#19596=ORIENTED_EDGE('',*,*,#14732,.F.);
#19597=ORIENTED_EDGE('',*,*,#14733,.F.);
#19598=ORIENTED_EDGE('',*,*,#14644,.F.);
#19599=ORIENTED_EDGE('',*,*,#14732,.T.);
#19600=ORIENTED_EDGE('',*,*,#14730,.F.);
#19601=ORIENTED_EDGE('',*,*,#14734,.F.);
#19602=ORIENTED_EDGE('',*,*,#14735,.T.);
#19603=ORIENTED_EDGE('',*,*,#14736,.T.);
#19604=ORIENTED_EDGE('',*,*,#14638,.F.);
#19605=ORIENTED_EDGE('',*,*,#14639,.F.);
#19606=ORIENTED_EDGE('',*,*,#14736,.F.);
#19607=ORIENTED_EDGE('',*,*,#14737,.F.);
#19608=ORIENTED_EDGE('',*,*,#14738,.F.);
#19609=ORIENTED_EDGE('',*,*,#14640,.F.);
#19610=ORIENTED_EDGE('',*,*,#14737,.T.);
#19611=ORIENTED_EDGE('',*,*,#14735,.F.);
#19612=ORIENTED_EDGE('',*,*,#14739,.F.);
#19613=ORIENTED_EDGE('',*,*,#14740,.T.);
#19614=ORIENTED_EDGE('',*,*,#14741,.T.);
#19615=ORIENTED_EDGE('',*,*,#14634,.F.);
#19616=ORIENTED_EDGE('',*,*,#14635,.F.);
#19617=ORIENTED_EDGE('',*,*,#14741,.F.);
#19618=ORIENTED_EDGE('',*,*,#14742,.F.);
#19619=ORIENTED_EDGE('',*,*,#14743,.F.);
#19620=ORIENTED_EDGE('',*,*,#14636,.F.);
#19621=ORIENTED_EDGE('',*,*,#14742,.T.);
#19622=ORIENTED_EDGE('',*,*,#14740,.F.);
#19623=ORIENTED_EDGE('',*,*,#14744,.F.);
#19624=ORIENTED_EDGE('',*,*,#14745,.T.);
#19625=ORIENTED_EDGE('',*,*,#14746,.T.);
#19626=ORIENTED_EDGE('',*,*,#14630,.F.);
#19627=ORIENTED_EDGE('',*,*,#14631,.F.);
#19628=ORIENTED_EDGE('',*,*,#14746,.F.);
#19629=ORIENTED_EDGE('',*,*,#14747,.F.);
#19630=ORIENTED_EDGE('',*,*,#14748,.F.);
#19631=ORIENTED_EDGE('',*,*,#14632,.F.);
#19632=ORIENTED_EDGE('',*,*,#14747,.T.);
#19633=ORIENTED_EDGE('',*,*,#14745,.F.);
#19634=ORIENTED_EDGE('',*,*,#14749,.F.);
#19635=ORIENTED_EDGE('',*,*,#14750,.T.);
#19636=ORIENTED_EDGE('',*,*,#14751,.T.);
#19637=ORIENTED_EDGE('',*,*,#14626,.F.);
#19638=ORIENTED_EDGE('',*,*,#14627,.F.);
#19639=ORIENTED_EDGE('',*,*,#14751,.F.);
#19640=ORIENTED_EDGE('',*,*,#14752,.F.);
#19641=ORIENTED_EDGE('',*,*,#14753,.F.);
#19642=ORIENTED_EDGE('',*,*,#14628,.F.);
#19643=ORIENTED_EDGE('',*,*,#14752,.T.);
#19644=ORIENTED_EDGE('',*,*,#14750,.F.);
#19645=ORIENTED_EDGE('',*,*,#14754,.F.);
#19646=ORIENTED_EDGE('',*,*,#14755,.T.);
#19647=ORIENTED_EDGE('',*,*,#14756,.T.);
#19648=ORIENTED_EDGE('',*,*,#14622,.F.);
#19649=ORIENTED_EDGE('',*,*,#14623,.F.);
#19650=ORIENTED_EDGE('',*,*,#14756,.F.);
#19651=ORIENTED_EDGE('',*,*,#14757,.F.);
#19652=ORIENTED_EDGE('',*,*,#14758,.F.);
#19653=ORIENTED_EDGE('',*,*,#14624,.F.);
#19654=ORIENTED_EDGE('',*,*,#14757,.T.);
#19655=ORIENTED_EDGE('',*,*,#14755,.F.);
#19656=ORIENTED_EDGE('',*,*,#14759,.F.);
#19657=ORIENTED_EDGE('',*,*,#14760,.T.);
#19658=ORIENTED_EDGE('',*,*,#14761,.T.);
#19659=ORIENTED_EDGE('',*,*,#14618,.F.);
#19660=ORIENTED_EDGE('',*,*,#14619,.F.);
#19661=ORIENTED_EDGE('',*,*,#14761,.F.);
#19662=ORIENTED_EDGE('',*,*,#14762,.F.);
#19663=ORIENTED_EDGE('',*,*,#14763,.F.);
#19664=ORIENTED_EDGE('',*,*,#14620,.F.);
#19665=ORIENTED_EDGE('',*,*,#14762,.T.);
#19666=ORIENTED_EDGE('',*,*,#14760,.F.);
#19667=ORIENTED_EDGE('',*,*,#14764,.F.);
#19668=ORIENTED_EDGE('',*,*,#14765,.T.);
#19669=ORIENTED_EDGE('',*,*,#14766,.T.);
#19670=ORIENTED_EDGE('',*,*,#14614,.F.);
#19671=ORIENTED_EDGE('',*,*,#14615,.F.);
#19672=ORIENTED_EDGE('',*,*,#14766,.F.);
#19673=ORIENTED_EDGE('',*,*,#14767,.F.);
#19674=ORIENTED_EDGE('',*,*,#14768,.F.);
#19675=ORIENTED_EDGE('',*,*,#14616,.F.);
#19676=ORIENTED_EDGE('',*,*,#14767,.T.);
#19677=ORIENTED_EDGE('',*,*,#14765,.F.);
#19678=ORIENTED_EDGE('',*,*,#14769,.F.);
#19679=ORIENTED_EDGE('',*,*,#14770,.T.);
#19680=ORIENTED_EDGE('',*,*,#14771,.T.);
#19681=ORIENTED_EDGE('',*,*,#14610,.F.);
#19682=ORIENTED_EDGE('',*,*,#14611,.F.);
#19683=ORIENTED_EDGE('',*,*,#14771,.F.);
#19684=ORIENTED_EDGE('',*,*,#14772,.F.);
#19685=ORIENTED_EDGE('',*,*,#14773,.F.);
#19686=ORIENTED_EDGE('',*,*,#14612,.F.);
#19687=ORIENTED_EDGE('',*,*,#14772,.T.);
#19688=ORIENTED_EDGE('',*,*,#14770,.F.);
#19689=ORIENTED_EDGE('',*,*,#14774,.F.);
#19690=ORIENTED_EDGE('',*,*,#14775,.T.);
#19691=ORIENTED_EDGE('',*,*,#14776,.T.);
#19692=ORIENTED_EDGE('',*,*,#14606,.F.);
#19693=ORIENTED_EDGE('',*,*,#14607,.F.);
#19694=ORIENTED_EDGE('',*,*,#14776,.F.);
#19695=ORIENTED_EDGE('',*,*,#14777,.F.);
#19696=ORIENTED_EDGE('',*,*,#14778,.F.);
#19697=ORIENTED_EDGE('',*,*,#14608,.F.);
#19698=ORIENTED_EDGE('',*,*,#14777,.T.);
#19699=ORIENTED_EDGE('',*,*,#14775,.F.);
#19700=ORIENTED_EDGE('',*,*,#14779,.F.);
#19701=ORIENTED_EDGE('',*,*,#14780,.T.);
#19702=ORIENTED_EDGE('',*,*,#14781,.T.);
#19703=ORIENTED_EDGE('',*,*,#14602,.F.);
#19704=ORIENTED_EDGE('',*,*,#14603,.F.);
#19705=ORIENTED_EDGE('',*,*,#14781,.F.);
#19706=ORIENTED_EDGE('',*,*,#14782,.F.);
#19707=ORIENTED_EDGE('',*,*,#14783,.F.);
#19708=ORIENTED_EDGE('',*,*,#14604,.F.);
#19709=ORIENTED_EDGE('',*,*,#14782,.T.);
#19710=ORIENTED_EDGE('',*,*,#14780,.F.);
#19711=ORIENTED_EDGE('',*,*,#14784,.F.);
#19712=ORIENTED_EDGE('',*,*,#14785,.T.);
#19713=ORIENTED_EDGE('',*,*,#14786,.T.);
#19714=ORIENTED_EDGE('',*,*,#14598,.F.);
#19715=ORIENTED_EDGE('',*,*,#14599,.F.);
#19716=ORIENTED_EDGE('',*,*,#14786,.F.);
#19717=ORIENTED_EDGE('',*,*,#14787,.F.);
#19718=ORIENTED_EDGE('',*,*,#14788,.F.);
#19719=ORIENTED_EDGE('',*,*,#14600,.F.);
#19720=ORIENTED_EDGE('',*,*,#14787,.T.);
#19721=ORIENTED_EDGE('',*,*,#14785,.F.);
#19722=ORIENTED_EDGE('',*,*,#14789,.F.);
#19723=ORIENTED_EDGE('',*,*,#14790,.T.);
#19724=ORIENTED_EDGE('',*,*,#14791,.T.);
#19725=ORIENTED_EDGE('',*,*,#14594,.F.);
#19726=ORIENTED_EDGE('',*,*,#14595,.F.);
#19727=ORIENTED_EDGE('',*,*,#14791,.F.);
#19728=ORIENTED_EDGE('',*,*,#14792,.F.);
#19729=ORIENTED_EDGE('',*,*,#14793,.F.);
#19730=ORIENTED_EDGE('',*,*,#14596,.F.);
#19731=ORIENTED_EDGE('',*,*,#14792,.T.);
#19732=ORIENTED_EDGE('',*,*,#14790,.F.);
#19733=ORIENTED_EDGE('',*,*,#14794,.F.);
#19734=ORIENTED_EDGE('',*,*,#14795,.T.);
#19735=ORIENTED_EDGE('',*,*,#14796,.T.);
#19736=ORIENTED_EDGE('',*,*,#14590,.F.);
#19737=ORIENTED_EDGE('',*,*,#14591,.F.);
#19738=ORIENTED_EDGE('',*,*,#14796,.F.);
#19739=ORIENTED_EDGE('',*,*,#14797,.F.);
#19740=ORIENTED_EDGE('',*,*,#14798,.F.);
#19741=ORIENTED_EDGE('',*,*,#14592,.F.);
#19742=ORIENTED_EDGE('',*,*,#14797,.T.);
#19743=ORIENTED_EDGE('',*,*,#14795,.F.);
#19744=ORIENTED_EDGE('',*,*,#14799,.F.);
#19745=ORIENTED_EDGE('',*,*,#14800,.T.);
#19746=ORIENTED_EDGE('',*,*,#14801,.T.);
#19747=ORIENTED_EDGE('',*,*,#14586,.F.);
#19748=ORIENTED_EDGE('',*,*,#14587,.F.);
#19749=ORIENTED_EDGE('',*,*,#14801,.F.);
#19750=ORIENTED_EDGE('',*,*,#14802,.F.);
#19751=ORIENTED_EDGE('',*,*,#14803,.F.);
#19752=ORIENTED_EDGE('',*,*,#14588,.F.);
#19753=ORIENTED_EDGE('',*,*,#14802,.T.);
#19754=ORIENTED_EDGE('',*,*,#14800,.F.);
#19755=ORIENTED_EDGE('',*,*,#14804,.F.);
#19756=ORIENTED_EDGE('',*,*,#14805,.T.);
#19757=ORIENTED_EDGE('',*,*,#14806,.T.);
#19758=ORIENTED_EDGE('',*,*,#14723,.F.);
#19759=ORIENTED_EDGE('',*,*,#14579,.F.);
#19760=ORIENTED_EDGE('',*,*,#14806,.F.);
#19761=ORIENTED_EDGE('',*,*,#14807,.F.);
#19762=ORIENTED_EDGE('',*,*,#14583,.F.);
#19763=ORIENTED_EDGE('',*,*,#14808,.F.);
#19764=ORIENTED_EDGE('',*,*,#14584,.F.);
#19765=ORIENTED_EDGE('',*,*,#14807,.T.);
#19766=ORIENTED_EDGE('',*,*,#14805,.F.);
#19767=ORIENTED_EDGE('',*,*,#14809,.F.);
#19768=ORIENTED_EDGE('',*,*,#14810,.T.);
#19769=ORIENTED_EDGE('',*,*,#14811,.T.);
#19770=ORIENTED_EDGE('',*,*,#14719,.F.);
#19771=ORIENTED_EDGE('',*,*,#14720,.F.);
#19772=ORIENTED_EDGE('',*,*,#14811,.F.);
#19773=ORIENTED_EDGE('',*,*,#14812,.F.);
#19774=ORIENTED_EDGE('',*,*,#14813,.F.);
#19775=ORIENTED_EDGE('',*,*,#14721,.F.);
#19776=ORIENTED_EDGE('',*,*,#14812,.T.);
#19777=ORIENTED_EDGE('',*,*,#14810,.F.);
#19778=ORIENTED_EDGE('',*,*,#14814,.F.);
#19779=ORIENTED_EDGE('',*,*,#14815,.T.);
#19780=ORIENTED_EDGE('',*,*,#14816,.T.);
#19781=ORIENTED_EDGE('',*,*,#14715,.F.);
#19782=ORIENTED_EDGE('',*,*,#14716,.F.);
#19783=ORIENTED_EDGE('',*,*,#14816,.F.);
#19784=ORIENTED_EDGE('',*,*,#14817,.F.);
#19785=ORIENTED_EDGE('',*,*,#14818,.F.);
#19786=ORIENTED_EDGE('',*,*,#14717,.F.);
#19787=ORIENTED_EDGE('',*,*,#14817,.T.);
#19788=ORIENTED_EDGE('',*,*,#14815,.F.);
#19789=ORIENTED_EDGE('',*,*,#14819,.F.);
#19790=ORIENTED_EDGE('',*,*,#14820,.T.);
#19791=ORIENTED_EDGE('',*,*,#14821,.T.);
#19792=ORIENTED_EDGE('',*,*,#14711,.F.);
#19793=ORIENTED_EDGE('',*,*,#14712,.F.);
#19794=ORIENTED_EDGE('',*,*,#14821,.F.);
#19795=ORIENTED_EDGE('',*,*,#14822,.F.);
#19796=ORIENTED_EDGE('',*,*,#14823,.F.);
#19797=ORIENTED_EDGE('',*,*,#14713,.F.);
#19798=ORIENTED_EDGE('',*,*,#14822,.T.);
#19799=ORIENTED_EDGE('',*,*,#14820,.F.);
#19800=ORIENTED_EDGE('',*,*,#14824,.F.);
#19801=ORIENTED_EDGE('',*,*,#14825,.T.);
#19802=ORIENTED_EDGE('',*,*,#14826,.T.);
#19803=ORIENTED_EDGE('',*,*,#14707,.F.);
#19804=ORIENTED_EDGE('',*,*,#14708,.F.);
#19805=ORIENTED_EDGE('',*,*,#14826,.F.);
#19806=ORIENTED_EDGE('',*,*,#14827,.F.);
#19807=ORIENTED_EDGE('',*,*,#14828,.F.);
#19808=ORIENTED_EDGE('',*,*,#14709,.F.);
#19809=ORIENTED_EDGE('',*,*,#14827,.T.);
#19810=ORIENTED_EDGE('',*,*,#14825,.F.);
#19811=ORIENTED_EDGE('',*,*,#14829,.F.);
#19812=ORIENTED_EDGE('',*,*,#14830,.T.);
#19813=ORIENTED_EDGE('',*,*,#14831,.T.);
#19814=ORIENTED_EDGE('',*,*,#14703,.F.);
#19815=ORIENTED_EDGE('',*,*,#14704,.F.);
#19816=ORIENTED_EDGE('',*,*,#14831,.F.);
#19817=ORIENTED_EDGE('',*,*,#14832,.F.);
#19818=ORIENTED_EDGE('',*,*,#14833,.F.);
#19819=ORIENTED_EDGE('',*,*,#14705,.F.);
#19820=ORIENTED_EDGE('',*,*,#14832,.T.);
#19821=ORIENTED_EDGE('',*,*,#14830,.F.);
#19822=ORIENTED_EDGE('',*,*,#14834,.F.);
#19823=ORIENTED_EDGE('',*,*,#14835,.T.);
#19824=ORIENTED_EDGE('',*,*,#14836,.T.);
#19825=ORIENTED_EDGE('',*,*,#14699,.F.);
#19826=ORIENTED_EDGE('',*,*,#14700,.F.);
#19827=ORIENTED_EDGE('',*,*,#14836,.F.);
#19828=ORIENTED_EDGE('',*,*,#14837,.F.);
#19829=ORIENTED_EDGE('',*,*,#14838,.F.);
#19830=ORIENTED_EDGE('',*,*,#14701,.F.);
#19831=ORIENTED_EDGE('',*,*,#14837,.T.);
#19832=ORIENTED_EDGE('',*,*,#14835,.F.);
#19833=ORIENTED_EDGE('',*,*,#14839,.F.);
#19834=ORIENTED_EDGE('',*,*,#14840,.T.);
#19835=ORIENTED_EDGE('',*,*,#14841,.T.);
#19836=ORIENTED_EDGE('',*,*,#14695,.F.);
#19837=ORIENTED_EDGE('',*,*,#14696,.F.);
#19838=ORIENTED_EDGE('',*,*,#14841,.F.);
#19839=ORIENTED_EDGE('',*,*,#14842,.F.);
#19840=ORIENTED_EDGE('',*,*,#14843,.F.);
#19841=ORIENTED_EDGE('',*,*,#14697,.F.);
#19842=ORIENTED_EDGE('',*,*,#14842,.T.);
#19843=ORIENTED_EDGE('',*,*,#14840,.F.);
#19844=ORIENTED_EDGE('',*,*,#14844,.F.);
#19845=ORIENTED_EDGE('',*,*,#14845,.T.);
#19846=ORIENTED_EDGE('',*,*,#14846,.T.);
#19847=ORIENTED_EDGE('',*,*,#14691,.F.);
#19848=ORIENTED_EDGE('',*,*,#14692,.F.);
#19849=ORIENTED_EDGE('',*,*,#14846,.F.);
#19850=ORIENTED_EDGE('',*,*,#14847,.F.);
#19851=ORIENTED_EDGE('',*,*,#14848,.F.);
#19852=ORIENTED_EDGE('',*,*,#14693,.F.);
#19853=ORIENTED_EDGE('',*,*,#14847,.T.);
#19854=ORIENTED_EDGE('',*,*,#14845,.F.);
#19855=ORIENTED_EDGE('',*,*,#14849,.F.);
#19856=ORIENTED_EDGE('',*,*,#14850,.T.);
#19857=ORIENTED_EDGE('',*,*,#14851,.T.);
#19858=ORIENTED_EDGE('',*,*,#14687,.F.);
#19859=ORIENTED_EDGE('',*,*,#14688,.F.);
#19860=ORIENTED_EDGE('',*,*,#14851,.F.);
#19861=ORIENTED_EDGE('',*,*,#14852,.F.);
#19862=ORIENTED_EDGE('',*,*,#14853,.F.);
#19863=ORIENTED_EDGE('',*,*,#14689,.F.);
#19864=ORIENTED_EDGE('',*,*,#14852,.T.);
#19865=ORIENTED_EDGE('',*,*,#14850,.F.);
#19866=ORIENTED_EDGE('',*,*,#14854,.F.);
#19867=ORIENTED_EDGE('',*,*,#14855,.T.);
#19868=ORIENTED_EDGE('',*,*,#14856,.T.);
#19869=ORIENTED_EDGE('',*,*,#14683,.F.);
#19870=ORIENTED_EDGE('',*,*,#14684,.F.);
#19871=ORIENTED_EDGE('',*,*,#14856,.F.);
#19872=ORIENTED_EDGE('',*,*,#14857,.F.);
#19873=ORIENTED_EDGE('',*,*,#14858,.F.);
#19874=ORIENTED_EDGE('',*,*,#14685,.F.);
#19875=ORIENTED_EDGE('',*,*,#14857,.T.);
#19876=ORIENTED_EDGE('',*,*,#14855,.F.);
#19877=ORIENTED_EDGE('',*,*,#14859,.F.);
#19878=ORIENTED_EDGE('',*,*,#14860,.T.);
#19879=ORIENTED_EDGE('',*,*,#14861,.T.);
#19880=ORIENTED_EDGE('',*,*,#14679,.F.);
#19881=ORIENTED_EDGE('',*,*,#14680,.F.);
#19882=ORIENTED_EDGE('',*,*,#14861,.F.);
#19883=ORIENTED_EDGE('',*,*,#14862,.F.);
#19884=ORIENTED_EDGE('',*,*,#14863,.F.);
#19885=ORIENTED_EDGE('',*,*,#14681,.F.);
#19886=ORIENTED_EDGE('',*,*,#14862,.T.);
#19887=ORIENTED_EDGE('',*,*,#14860,.F.);
#19888=ORIENTED_EDGE('',*,*,#14864,.F.);
#19889=ORIENTED_EDGE('',*,*,#14865,.T.);
#19890=ORIENTED_EDGE('',*,*,#14866,.T.);
#19891=ORIENTED_EDGE('',*,*,#14675,.F.);
#19892=ORIENTED_EDGE('',*,*,#14676,.F.);
#19893=ORIENTED_EDGE('',*,*,#14866,.F.);
#19894=ORIENTED_EDGE('',*,*,#14867,.F.);
#19895=ORIENTED_EDGE('',*,*,#14868,.F.);
#19896=ORIENTED_EDGE('',*,*,#14677,.F.);
#19897=ORIENTED_EDGE('',*,*,#14867,.T.);
#19898=ORIENTED_EDGE('',*,*,#14865,.F.);
#19899=ORIENTED_EDGE('',*,*,#14869,.F.);
#19900=ORIENTED_EDGE('',*,*,#14870,.T.);
#19901=ORIENTED_EDGE('',*,*,#14871,.T.);
#19902=ORIENTED_EDGE('',*,*,#14671,.F.);
#19903=ORIENTED_EDGE('',*,*,#14672,.F.);
#19904=ORIENTED_EDGE('',*,*,#14871,.F.);
#19905=ORIENTED_EDGE('',*,*,#14872,.F.);
#19906=ORIENTED_EDGE('',*,*,#14873,.F.);
#19907=ORIENTED_EDGE('',*,*,#14673,.F.);
#19908=ORIENTED_EDGE('',*,*,#14872,.T.);
#19909=ORIENTED_EDGE('',*,*,#14870,.F.);
#19910=ORIENTED_EDGE('',*,*,#14874,.F.);
#19911=ORIENTED_EDGE('',*,*,#14875,.T.);
#19912=ORIENTED_EDGE('',*,*,#14876,.T.);
#19913=ORIENTED_EDGE('',*,*,#14667,.F.);
#19914=ORIENTED_EDGE('',*,*,#14668,.F.);
#19915=ORIENTED_EDGE('',*,*,#14876,.F.);
#19916=ORIENTED_EDGE('',*,*,#14877,.F.);
#19917=ORIENTED_EDGE('',*,*,#14878,.F.);
#19918=ORIENTED_EDGE('',*,*,#14669,.F.);
#19919=ORIENTED_EDGE('',*,*,#14877,.T.);
#19920=ORIENTED_EDGE('',*,*,#14875,.F.);
#19921=ORIENTED_EDGE('',*,*,#14879,.F.);
#19922=ORIENTED_EDGE('',*,*,#14880,.T.);
#19923=ORIENTED_EDGE('',*,*,#14881,.T.);
#19924=ORIENTED_EDGE('',*,*,#14663,.F.);
#19925=ORIENTED_EDGE('',*,*,#14664,.F.);
#19926=ORIENTED_EDGE('',*,*,#14881,.F.);
#19927=ORIENTED_EDGE('',*,*,#14882,.F.);
#19928=ORIENTED_EDGE('',*,*,#14883,.F.);
#19929=ORIENTED_EDGE('',*,*,#14665,.F.);
#19930=ORIENTED_EDGE('',*,*,#14882,.T.);
#19931=ORIENTED_EDGE('',*,*,#14880,.F.);
#19932=ORIENTED_EDGE('',*,*,#14884,.F.);
#19933=ORIENTED_EDGE('',*,*,#14885,.T.);
#19934=ORIENTED_EDGE('',*,*,#14886,.T.);
#19935=ORIENTED_EDGE('',*,*,#14659,.F.);
#19936=ORIENTED_EDGE('',*,*,#14660,.F.);
#19937=ORIENTED_EDGE('',*,*,#14886,.F.);
#19938=ORIENTED_EDGE('',*,*,#14887,.F.);
#19939=ORIENTED_EDGE('',*,*,#14888,.F.);
#19940=ORIENTED_EDGE('',*,*,#14661,.F.);
#19941=ORIENTED_EDGE('',*,*,#14887,.T.);
#19942=ORIENTED_EDGE('',*,*,#14885,.F.);
#19943=ORIENTED_EDGE('',*,*,#14889,.F.);
#19944=ORIENTED_EDGE('',*,*,#14890,.T.);
#19945=ORIENTED_EDGE('',*,*,#14891,.T.);
#19946=ORIENTED_EDGE('',*,*,#14655,.F.);
#19947=ORIENTED_EDGE('',*,*,#14656,.F.);
#19948=ORIENTED_EDGE('',*,*,#14891,.F.);
#19949=ORIENTED_EDGE('',*,*,#14892,.F.);
#19950=ORIENTED_EDGE('',*,*,#14893,.F.);
#19951=ORIENTED_EDGE('',*,*,#14657,.F.);
#19952=ORIENTED_EDGE('',*,*,#14892,.T.);
#19953=ORIENTED_EDGE('',*,*,#14890,.F.);
#19954=ORIENTED_EDGE('',*,*,#14894,.F.);
#19955=ORIENTED_EDGE('',*,*,#14895,.T.);
#19956=ORIENTED_EDGE('',*,*,#14896,.T.);
#19957=ORIENTED_EDGE('',*,*,#14651,.F.);
#19958=ORIENTED_EDGE('',*,*,#14652,.F.);
#19959=ORIENTED_EDGE('',*,*,#14896,.F.);
#19960=ORIENTED_EDGE('',*,*,#14897,.F.);
#19961=ORIENTED_EDGE('',*,*,#14898,.F.);
#19962=ORIENTED_EDGE('',*,*,#14653,.F.);
#19963=ORIENTED_EDGE('',*,*,#14897,.T.);
#19964=ORIENTED_EDGE('',*,*,#14895,.F.);
#19965=ORIENTED_EDGE('',*,*,#14581,.T.);
#19966=ORIENTED_EDGE('',*,*,#14582,.T.);
#19967=ORIENTED_EDGE('',*,*,#14899,.T.);
#19968=ORIENTED_EDGE('',*,*,#14568,.T.);
#19969=ORIENTED_EDGE('',*,*,#14899,.F.);
#19970=ORIENTED_EDGE('',*,*,#14804,.T.);
#19971=ORIENTED_EDGE('',*,*,#14722,.T.);
#19972=ORIENTED_EDGE('',*,*,#14813,.T.);
#19973=ORIENTED_EDGE('',*,*,#14809,.T.);
#19974=ORIENTED_EDGE('',*,*,#14718,.T.);
#19975=ORIENTED_EDGE('',*,*,#14818,.T.);
#19976=ORIENTED_EDGE('',*,*,#14814,.T.);
#19977=ORIENTED_EDGE('',*,*,#14714,.T.);
#19978=ORIENTED_EDGE('',*,*,#14823,.T.);
#19979=ORIENTED_EDGE('',*,*,#14819,.T.);
#19980=ORIENTED_EDGE('',*,*,#14710,.T.);
#19981=ORIENTED_EDGE('',*,*,#14828,.T.);
#19982=ORIENTED_EDGE('',*,*,#14824,.T.);
#19983=ORIENTED_EDGE('',*,*,#14706,.T.);
#19984=ORIENTED_EDGE('',*,*,#14833,.T.);
#19985=ORIENTED_EDGE('',*,*,#14829,.T.);
#19986=ORIENTED_EDGE('',*,*,#14702,.T.);
#19987=ORIENTED_EDGE('',*,*,#14838,.T.);
#19988=ORIENTED_EDGE('',*,*,#14834,.T.);
#19989=ORIENTED_EDGE('',*,*,#14698,.T.);
#19990=ORIENTED_EDGE('',*,*,#14843,.T.);
#19991=ORIENTED_EDGE('',*,*,#14839,.T.);
#19992=ORIENTED_EDGE('',*,*,#14694,.T.);
#19993=ORIENTED_EDGE('',*,*,#14848,.T.);
#19994=ORIENTED_EDGE('',*,*,#14844,.T.);
#19995=ORIENTED_EDGE('',*,*,#14690,.T.);
#19996=ORIENTED_EDGE('',*,*,#14853,.T.);
#19997=ORIENTED_EDGE('',*,*,#14849,.T.);
#19998=ORIENTED_EDGE('',*,*,#14686,.T.);
#19999=ORIENTED_EDGE('',*,*,#14858,.T.);
#20000=ORIENTED_EDGE('',*,*,#14854,.T.);
#20001=ORIENTED_EDGE('',*,*,#14682,.T.);
#20002=ORIENTED_EDGE('',*,*,#14863,.T.);
#20003=ORIENTED_EDGE('',*,*,#14859,.T.);
#20004=ORIENTED_EDGE('',*,*,#14678,.T.);
#20005=ORIENTED_EDGE('',*,*,#14868,.T.);
#20006=ORIENTED_EDGE('',*,*,#14864,.T.);
#20007=ORIENTED_EDGE('',*,*,#14674,.T.);
#20008=ORIENTED_EDGE('',*,*,#14873,.T.);
#20009=ORIENTED_EDGE('',*,*,#14869,.T.);
#20010=ORIENTED_EDGE('',*,*,#14670,.T.);
#20011=ORIENTED_EDGE('',*,*,#14878,.T.);
#20012=ORIENTED_EDGE('',*,*,#14874,.T.);
#20013=ORIENTED_EDGE('',*,*,#14666,.T.);
#20014=ORIENTED_EDGE('',*,*,#14883,.T.);
#20015=ORIENTED_EDGE('',*,*,#14879,.T.);
#20016=ORIENTED_EDGE('',*,*,#14662,.T.);
#20017=ORIENTED_EDGE('',*,*,#14888,.T.);
#20018=ORIENTED_EDGE('',*,*,#14884,.T.);
#20019=ORIENTED_EDGE('',*,*,#14658,.T.);
#20020=ORIENTED_EDGE('',*,*,#14893,.T.);
#20021=ORIENTED_EDGE('',*,*,#14889,.T.);
#20022=ORIENTED_EDGE('',*,*,#14654,.T.);
#20023=ORIENTED_EDGE('',*,*,#14898,.T.);
#20024=ORIENTED_EDGE('',*,*,#14894,.T.);
#20025=ORIENTED_EDGE('',*,*,#14650,.T.);
#20026=ORIENTED_EDGE('',*,*,#14577,.T.);
#20027=ORIENTED_EDGE('',*,*,#14571,.T.);
#20028=ORIENTED_EDGE('',*,*,#14649,.T.);
#20029=ORIENTED_EDGE('',*,*,#14728,.T.);
#20030=ORIENTED_EDGE('',*,*,#14724,.T.);
#20031=ORIENTED_EDGE('',*,*,#14645,.T.);
#20032=ORIENTED_EDGE('',*,*,#14733,.T.);
#20033=ORIENTED_EDGE('',*,*,#14729,.T.);
#20034=ORIENTED_EDGE('',*,*,#14641,.T.);
#20035=ORIENTED_EDGE('',*,*,#14738,.T.);
#20036=ORIENTED_EDGE('',*,*,#14734,.T.);
#20037=ORIENTED_EDGE('',*,*,#14637,.T.);
#20038=ORIENTED_EDGE('',*,*,#14743,.T.);
#20039=ORIENTED_EDGE('',*,*,#14739,.T.);
#20040=ORIENTED_EDGE('',*,*,#14633,.T.);
#20041=ORIENTED_EDGE('',*,*,#14748,.T.);
#20042=ORIENTED_EDGE('',*,*,#14744,.T.);
#20043=ORIENTED_EDGE('',*,*,#14629,.T.);
#20044=ORIENTED_EDGE('',*,*,#14753,.T.);
#20045=ORIENTED_EDGE('',*,*,#14749,.T.);
#20046=ORIENTED_EDGE('',*,*,#14625,.T.);
#20047=ORIENTED_EDGE('',*,*,#14758,.T.);
#20048=ORIENTED_EDGE('',*,*,#14754,.T.);
#20049=ORIENTED_EDGE('',*,*,#14621,.T.);
#20050=ORIENTED_EDGE('',*,*,#14763,.T.);
#20051=ORIENTED_EDGE('',*,*,#14759,.T.);
#20052=ORIENTED_EDGE('',*,*,#14617,.T.);
#20053=ORIENTED_EDGE('',*,*,#14768,.T.);
#20054=ORIENTED_EDGE('',*,*,#14764,.T.);
#20055=ORIENTED_EDGE('',*,*,#14613,.T.);
#20056=ORIENTED_EDGE('',*,*,#14773,.T.);
#20057=ORIENTED_EDGE('',*,*,#14769,.T.);
#20058=ORIENTED_EDGE('',*,*,#14609,.T.);
#20059=ORIENTED_EDGE('',*,*,#14778,.T.);
#20060=ORIENTED_EDGE('',*,*,#14774,.T.);
#20061=ORIENTED_EDGE('',*,*,#14605,.T.);
#20062=ORIENTED_EDGE('',*,*,#14783,.T.);
#20063=ORIENTED_EDGE('',*,*,#14779,.T.);
#20064=ORIENTED_EDGE('',*,*,#14601,.T.);
#20065=ORIENTED_EDGE('',*,*,#14788,.T.);
#20066=ORIENTED_EDGE('',*,*,#14784,.T.);
#20067=ORIENTED_EDGE('',*,*,#14597,.T.);
#20068=ORIENTED_EDGE('',*,*,#14793,.T.);
#20069=ORIENTED_EDGE('',*,*,#14789,.T.);
#20070=ORIENTED_EDGE('',*,*,#14593,.T.);
#20071=ORIENTED_EDGE('',*,*,#14798,.T.);
#20072=ORIENTED_EDGE('',*,*,#14794,.T.);
#20073=ORIENTED_EDGE('',*,*,#14589,.T.);
#20074=ORIENTED_EDGE('',*,*,#14803,.T.);
#20075=ORIENTED_EDGE('',*,*,#14799,.T.);
#20076=ORIENTED_EDGE('',*,*,#14585,.T.);
#20077=ORIENTED_EDGE('',*,*,#14808,.T.);
#20078=ORIENTED_EDGE('',*,*,#14900,.T.);
#20079=ORIENTED_EDGE('',*,*,#14901,.T.);
#20080=ORIENTED_EDGE('',*,*,#14900,.F.);
#20081=ORIENTED_EDGE('',*,*,#14901,.F.);
#20082=ORIENTED_EDGE('',*,*,#14902,.T.);
#20083=ORIENTED_EDGE('',*,*,#14903,.F.);
#20084=ORIENTED_EDGE('',*,*,#14904,.T.);
#20085=ORIENTED_EDGE('',*,*,#14905,.F.);
#20086=ORIENTED_EDGE('',*,*,#14906,.F.);
#20087=ORIENTED_EDGE('',*,*,#14907,.T.);
#20088=ORIENTED_EDGE('',*,*,#14908,.F.);
#20089=ORIENTED_EDGE('',*,*,#14909,.F.);
#20090=ORIENTED_EDGE('',*,*,#14910,.T.);
#20091=ORIENTED_EDGE('',*,*,#14911,.F.);
#20092=ORIENTED_EDGE('',*,*,#14912,.F.);
#20093=ORIENTED_EDGE('',*,*,#14913,.T.);
#20094=ORIENTED_EDGE('',*,*,#14914,.F.);
#20095=ORIENTED_EDGE('',*,*,#14915,.F.);
#20096=ORIENTED_EDGE('',*,*,#14916,.T.);
#20097=ORIENTED_EDGE('',*,*,#14917,.F.);
#20098=ORIENTED_EDGE('',*,*,#14918,.F.);
#20099=ORIENTED_EDGE('',*,*,#14919,.T.);
#20100=ORIENTED_EDGE('',*,*,#14920,.F.);
#20101=ORIENTED_EDGE('',*,*,#14921,.T.);
#20102=ORIENTED_EDGE('',*,*,#14902,.F.);
#20103=ORIENTED_EDGE('',*,*,#14921,.F.);
#20104=ORIENTED_EDGE('',*,*,#14922,.F.);
#20105=ORIENTED_EDGE('',*,*,#14907,.F.);
#20106=ORIENTED_EDGE('',*,*,#14923,.F.);
#20107=ORIENTED_EDGE('',*,*,#14924,.F.);
#20108=ORIENTED_EDGE('',*,*,#14925,.F.);
#20109=ORIENTED_EDGE('',*,*,#14910,.F.);
#20110=ORIENTED_EDGE('',*,*,#14926,.F.);
#20111=ORIENTED_EDGE('',*,*,#14927,.F.);
#20112=ORIENTED_EDGE('',*,*,#14928,.F.);
#20113=ORIENTED_EDGE('',*,*,#14929,.F.);
#20114=ORIENTED_EDGE('',*,*,#14930,.F.);
#20115=ORIENTED_EDGE('',*,*,#14904,.F.);
#20116=ORIENTED_EDGE('',*,*,#14931,.F.);
#20117=ORIENTED_EDGE('',*,*,#14913,.F.);
#20118=ORIENTED_EDGE('',*,*,#14932,.F.);
#20119=ORIENTED_EDGE('',*,*,#14933,.F.);
#20120=ORIENTED_EDGE('',*,*,#14934,.F.);
#20121=ORIENTED_EDGE('',*,*,#14935,.F.);
#20122=ORIENTED_EDGE('',*,*,#14936,.F.);
#20123=ORIENTED_EDGE('',*,*,#14919,.F.);
#20124=ORIENTED_EDGE('',*,*,#14937,.F.);
#20125=ORIENTED_EDGE('',*,*,#14938,.F.);
#20126=ORIENTED_EDGE('',*,*,#14939,.F.);
#20127=ORIENTED_EDGE('',*,*,#14916,.F.);
#20128=ORIENTED_EDGE('',*,*,#14914,.T.);
#20129=ORIENTED_EDGE('',*,*,#14931,.T.);
#20130=ORIENTED_EDGE('',*,*,#14940,.F.);
#20131=ORIENTED_EDGE('',*,*,#14932,.T.);
#20132=ORIENTED_EDGE('',*,*,#14912,.T.);
#20133=ORIENTED_EDGE('',*,*,#14941,.T.);
#20134=ORIENTED_EDGE('',*,*,#14942,.T.);
#20135=ORIENTED_EDGE('',*,*,#14943,.F.);
#20136=ORIENTED_EDGE('',*,*,#14911,.T.);
#20137=ORIENTED_EDGE('',*,*,#14925,.T.);
#20138=ORIENTED_EDGE('',*,*,#14944,.F.);
#20139=ORIENTED_EDGE('',*,*,#14926,.T.);
#20140=ORIENTED_EDGE('',*,*,#14909,.T.);
#20141=ORIENTED_EDGE('',*,*,#14945,.T.);
#20142=ORIENTED_EDGE('',*,*,#14946,.T.);
#20143=ORIENTED_EDGE('',*,*,#14941,.F.);
#20144=ORIENTED_EDGE('',*,*,#14908,.T.);
#20145=ORIENTED_EDGE('',*,*,#14922,.T.);
#20146=ORIENTED_EDGE('',*,*,#14947,.F.);
#20147=ORIENTED_EDGE('',*,*,#14923,.T.);
#20148=ORIENTED_EDGE('',*,*,#14906,.T.);
#20149=ORIENTED_EDGE('',*,*,#14948,.T.);
#20150=ORIENTED_EDGE('',*,*,#14949,.T.);
#20151=ORIENTED_EDGE('',*,*,#14945,.F.);
#20152=ORIENTED_EDGE('',*,*,#14924,.T.);
#20153=ORIENTED_EDGE('',*,*,#14947,.T.);
#20154=ORIENTED_EDGE('',*,*,#14927,.T.);
#20155=ORIENTED_EDGE('',*,*,#14944,.T.);
#20156=ORIENTED_EDGE('',*,*,#14929,.T.);
#20157=ORIENTED_EDGE('',*,*,#14950,.T.);
#20158=ORIENTED_EDGE('',*,*,#14933,.T.);
#20159=ORIENTED_EDGE('',*,*,#14940,.T.);
#20160=ORIENTED_EDGE('',*,*,#14935,.T.);
#20161=ORIENTED_EDGE('',*,*,#14951,.T.);
#20162=ORIENTED_EDGE('',*,*,#14938,.T.);
#20163=ORIENTED_EDGE('',*,*,#14952,.T.);
#20164=ORIENTED_EDGE('',*,*,#14953,.F.);
#20165=ORIENTED_EDGE('',*,*,#14954,.T.);
#20166=ORIENTED_EDGE('',*,*,#14949,.F.);
#20167=ORIENTED_EDGE('',*,*,#14955,.T.);
#20168=ORIENTED_EDGE('',*,*,#14946,.F.);
#20169=ORIENTED_EDGE('',*,*,#14956,.T.);
#20170=ORIENTED_EDGE('',*,*,#14942,.F.);
#20171=ORIENTED_EDGE('',*,*,#14957,.T.);
#20172=ORIENTED_EDGE('',*,*,#14958,.F.);
#20173=ORIENTED_EDGE('',*,*,#14959,.T.);
#20174=ORIENTED_EDGE('',*,*,#14960,.F.);
#20175=ORIENTED_EDGE('',*,*,#14961,.T.);
#20176=ORIENTED_EDGE('',*,*,#14962,.T.);
#20177=ORIENTED_EDGE('',*,*,#14961,.F.);
#20178=ORIENTED_EDGE('',*,*,#14959,.F.);
#20179=ORIENTED_EDGE('',*,*,#14957,.F.);
#20180=ORIENTED_EDGE('',*,*,#14956,.F.);
#20181=ORIENTED_EDGE('',*,*,#14955,.F.);
#20182=ORIENTED_EDGE('',*,*,#14954,.F.);
#20183=ORIENTED_EDGE('',*,*,#14962,.F.);
#20184=ORIENTED_EDGE('',*,*,#14903,.T.);
#20185=ORIENTED_EDGE('',*,*,#14963,.T.);
#20186=ORIENTED_EDGE('',*,*,#14953,.T.);
#20187=ORIENTED_EDGE('',*,*,#14948,.F.);
#20188=ORIENTED_EDGE('',*,*,#14905,.T.);
#20189=ORIENTED_EDGE('',*,*,#14930,.T.);
#20190=ORIENTED_EDGE('',*,*,#14950,.F.);
#20191=ORIENTED_EDGE('',*,*,#14928,.T.);
#20192=ORIENTED_EDGE('',*,*,#14918,.T.);
#20193=ORIENTED_EDGE('',*,*,#14964,.T.);
#20194=ORIENTED_EDGE('',*,*,#14960,.T.);
#20195=ORIENTED_EDGE('',*,*,#14963,.F.);
#20196=ORIENTED_EDGE('',*,*,#14920,.T.);
#20197=ORIENTED_EDGE('',*,*,#14936,.T.);
#20198=ORIENTED_EDGE('',*,*,#14951,.F.);
#20199=ORIENTED_EDGE('',*,*,#14934,.T.);
#20200=ORIENTED_EDGE('',*,*,#14915,.T.);
#20201=ORIENTED_EDGE('',*,*,#14943,.T.);
#20202=ORIENTED_EDGE('',*,*,#14958,.T.);
#20203=ORIENTED_EDGE('',*,*,#14964,.F.);
#20204=ORIENTED_EDGE('',*,*,#14917,.T.);
#20205=ORIENTED_EDGE('',*,*,#14939,.T.);
#20206=ORIENTED_EDGE('',*,*,#14952,.F.);
#20207=ORIENTED_EDGE('',*,*,#14937,.T.);
#20208=ORIENTED_EDGE('',*,*,#14965,.T.);
#20209=ORIENTED_EDGE('',*,*,#14966,.T.);
#20210=ORIENTED_EDGE('',*,*,#14967,.T.);
#20211=ORIENTED_EDGE('',*,*,#14966,.F.);
#20212=ORIENTED_EDGE('',*,*,#14968,.F.);
#20213=ORIENTED_EDGE('',*,*,#14969,.F.);
#20214=ORIENTED_EDGE('',*,*,#14970,.F.);
#20215=ORIENTED_EDGE('',*,*,#14971,.F.);
#20216=ORIENTED_EDGE('',*,*,#14972,.F.);
#20217=ORIENTED_EDGE('',*,*,#14973,.F.);
#20218=ORIENTED_EDGE('',*,*,#14974,.F.);
#20219=ORIENTED_EDGE('',*,*,#14975,.F.);
#20220=ORIENTED_EDGE('',*,*,#14976,.F.);
#20221=ORIENTED_EDGE('',*,*,#14977,.F.);
#20222=ORIENTED_EDGE('',*,*,#14978,.F.);
#20223=ORIENTED_EDGE('',*,*,#14979,.F.);
#20224=ORIENTED_EDGE('',*,*,#14980,.F.);
#20225=ORIENTED_EDGE('',*,*,#14981,.F.);
#20226=ORIENTED_EDGE('',*,*,#14982,.F.);
#20227=ORIENTED_EDGE('',*,*,#14983,.F.);
#20228=ORIENTED_EDGE('',*,*,#14984,.F.);
#20229=ORIENTED_EDGE('',*,*,#14985,.F.);
#20230=ORIENTED_EDGE('',*,*,#14986,.F.);
#20231=ORIENTED_EDGE('',*,*,#14987,.F.);
#20232=ORIENTED_EDGE('',*,*,#14988,.F.);
#20233=ORIENTED_EDGE('',*,*,#14989,.F.);
#20234=ORIENTED_EDGE('',*,*,#14990,.F.);
#20235=ORIENTED_EDGE('',*,*,#14991,.F.);
#20236=ORIENTED_EDGE('',*,*,#14967,.F.);
#20237=ORIENTED_EDGE('',*,*,#14965,.F.);
#20238=ORIENTED_EDGE('',*,*,#14992,.T.);
#20239=ORIENTED_EDGE('',*,*,#14993,.F.);
#20240=ORIENTED_EDGE('',*,*,#14992,.F.);
#20241=ORIENTED_EDGE('',*,*,#14994,.T.);
#20242=ORIENTED_EDGE('',*,*,#14995,.T.);
#20243=ORIENTED_EDGE('',*,*,#14972,.T.);
#20244=ORIENTED_EDGE('',*,*,#14995,.F.);
#20245=ORIENTED_EDGE('',*,*,#14994,.F.);
#20246=ORIENTED_EDGE('',*,*,#14996,.T.);
#20247=ORIENTED_EDGE('',*,*,#14997,.F.);
#20248=ORIENTED_EDGE('',*,*,#14996,.F.);
#20249=ORIENTED_EDGE('',*,*,#14998,.T.);
#20250=ORIENTED_EDGE('',*,*,#14999,.T.);
#20251=ORIENTED_EDGE('',*,*,#14991,.T.);
#20252=ORIENTED_EDGE('',*,*,#14999,.F.);
#20253=ORIENTED_EDGE('',*,*,#14998,.F.);
#20254=ORIENTED_EDGE('',*,*,#15000,.T.);
#20255=ORIENTED_EDGE('',*,*,#15001,.F.);
#20256=ORIENTED_EDGE('',*,*,#15000,.F.);
#20257=ORIENTED_EDGE('',*,*,#15002,.T.);
#20258=ORIENTED_EDGE('',*,*,#15003,.T.);
#20259=ORIENTED_EDGE('',*,*,#14973,.T.);
#20260=ORIENTED_EDGE('',*,*,#15003,.F.);
#20261=ORIENTED_EDGE('',*,*,#15002,.F.);
#20262=ORIENTED_EDGE('',*,*,#15004,.T.);
#20263=ORIENTED_EDGE('',*,*,#15005,.F.);
#20264=ORIENTED_EDGE('',*,*,#15004,.F.);
#20265=ORIENTED_EDGE('',*,*,#15006,.T.);
#20266=ORIENTED_EDGE('',*,*,#15007,.T.);
#20267=ORIENTED_EDGE('',*,*,#14990,.T.);
#20268=ORIENTED_EDGE('',*,*,#15007,.F.);
#20269=ORIENTED_EDGE('',*,*,#15006,.F.);
#20270=ORIENTED_EDGE('',*,*,#15008,.T.);
#20271=ORIENTED_EDGE('',*,*,#15009,.F.);
#20272=ORIENTED_EDGE('',*,*,#15008,.F.);
#20273=ORIENTED_EDGE('',*,*,#15010,.T.);
#20274=ORIENTED_EDGE('',*,*,#15011,.T.);
#20275=ORIENTED_EDGE('',*,*,#14974,.T.);
#20276=ORIENTED_EDGE('',*,*,#15011,.F.);
#20277=ORIENTED_EDGE('',*,*,#15010,.F.);
#20278=ORIENTED_EDGE('',*,*,#15012,.T.);
#20279=ORIENTED_EDGE('',*,*,#15013,.F.);
#20280=ORIENTED_EDGE('',*,*,#15012,.F.);
#20281=ORIENTED_EDGE('',*,*,#15014,.T.);
#20282=ORIENTED_EDGE('',*,*,#15015,.T.);
#20283=ORIENTED_EDGE('',*,*,#14989,.T.);
#20284=ORIENTED_EDGE('',*,*,#15015,.F.);
#20285=ORIENTED_EDGE('',*,*,#15014,.F.);
#20286=ORIENTED_EDGE('',*,*,#15016,.T.);
#20287=ORIENTED_EDGE('',*,*,#15017,.F.);
#20288=ORIENTED_EDGE('',*,*,#15016,.F.);
#20289=ORIENTED_EDGE('',*,*,#15018,.T.);
#20290=ORIENTED_EDGE('',*,*,#15019,.T.);
#20291=ORIENTED_EDGE('',*,*,#14975,.T.);
#20292=ORIENTED_EDGE('',*,*,#15019,.F.);
#20293=ORIENTED_EDGE('',*,*,#15018,.F.);
#20294=ORIENTED_EDGE('',*,*,#15020,.T.);
#20295=ORIENTED_EDGE('',*,*,#15021,.F.);
#20296=ORIENTED_EDGE('',*,*,#15020,.F.);
#20297=ORIENTED_EDGE('',*,*,#15022,.T.);
#20298=ORIENTED_EDGE('',*,*,#15023,.T.);
#20299=ORIENTED_EDGE('',*,*,#14988,.T.);
#20300=ORIENTED_EDGE('',*,*,#15023,.F.);
#20301=ORIENTED_EDGE('',*,*,#15022,.F.);
#20302=ORIENTED_EDGE('',*,*,#15024,.T.);
#20303=ORIENTED_EDGE('',*,*,#15025,.F.);
#20304=ORIENTED_EDGE('',*,*,#15024,.F.);
#20305=ORIENTED_EDGE('',*,*,#15026,.T.);
#20306=ORIENTED_EDGE('',*,*,#15027,.T.);
#20307=ORIENTED_EDGE('',*,*,#14976,.T.);
#20308=ORIENTED_EDGE('',*,*,#15027,.F.);
#20309=ORIENTED_EDGE('',*,*,#15026,.F.);
#20310=ORIENTED_EDGE('',*,*,#15028,.T.);
#20311=ORIENTED_EDGE('',*,*,#15029,.F.);
#20312=ORIENTED_EDGE('',*,*,#15028,.F.);
#20313=ORIENTED_EDGE('',*,*,#15030,.T.);
#20314=ORIENTED_EDGE('',*,*,#15031,.T.);
#20315=ORIENTED_EDGE('',*,*,#14987,.T.);
#20316=ORIENTED_EDGE('',*,*,#15031,.F.);
#20317=ORIENTED_EDGE('',*,*,#15030,.F.);
#20318=ORIENTED_EDGE('',*,*,#15032,.T.);
#20319=ORIENTED_EDGE('',*,*,#15033,.F.);
#20320=ORIENTED_EDGE('',*,*,#15032,.F.);
#20321=ORIENTED_EDGE('',*,*,#15034,.T.);
#20322=ORIENTED_EDGE('',*,*,#15035,.T.);
#20323=ORIENTED_EDGE('',*,*,#14977,.T.);
#20324=ORIENTED_EDGE('',*,*,#15035,.F.);
#20325=ORIENTED_EDGE('',*,*,#15034,.F.);
#20326=ORIENTED_EDGE('',*,*,#15036,.T.);
#20327=ORIENTED_EDGE('',*,*,#15037,.F.);
#20328=ORIENTED_EDGE('',*,*,#15036,.F.);
#20329=ORIENTED_EDGE('',*,*,#15038,.T.);
#20330=ORIENTED_EDGE('',*,*,#15039,.T.);
#20331=ORIENTED_EDGE('',*,*,#14986,.T.);
#20332=ORIENTED_EDGE('',*,*,#15039,.F.);
#20333=ORIENTED_EDGE('',*,*,#15038,.F.);
#20334=ORIENTED_EDGE('',*,*,#15040,.T.);
#20335=ORIENTED_EDGE('',*,*,#15041,.F.);
#20336=ORIENTED_EDGE('',*,*,#15040,.F.);
#20337=ORIENTED_EDGE('',*,*,#15042,.T.);
#20338=ORIENTED_EDGE('',*,*,#15043,.T.);
#20339=ORIENTED_EDGE('',*,*,#14978,.T.);
#20340=ORIENTED_EDGE('',*,*,#15043,.F.);
#20341=ORIENTED_EDGE('',*,*,#15042,.F.);
#20342=ORIENTED_EDGE('',*,*,#15044,.T.);
#20343=ORIENTED_EDGE('',*,*,#15045,.F.);
#20344=ORIENTED_EDGE('',*,*,#15044,.F.);
#20345=ORIENTED_EDGE('',*,*,#15046,.T.);
#20346=ORIENTED_EDGE('',*,*,#15047,.T.);
#20347=ORIENTED_EDGE('',*,*,#14985,.T.);
#20348=ORIENTED_EDGE('',*,*,#15047,.F.);
#20349=ORIENTED_EDGE('',*,*,#15046,.F.);
#20350=ORIENTED_EDGE('',*,*,#15048,.T.);
#20351=ORIENTED_EDGE('',*,*,#15049,.F.);
#20352=ORIENTED_EDGE('',*,*,#15048,.F.);
#20353=ORIENTED_EDGE('',*,*,#15050,.T.);
#20354=ORIENTED_EDGE('',*,*,#15051,.T.);
#20355=ORIENTED_EDGE('',*,*,#14979,.T.);
#20356=ORIENTED_EDGE('',*,*,#15051,.F.);
#20357=ORIENTED_EDGE('',*,*,#15050,.F.);
#20358=ORIENTED_EDGE('',*,*,#15052,.T.);
#20359=ORIENTED_EDGE('',*,*,#15053,.F.);
#20360=ORIENTED_EDGE('',*,*,#15052,.F.);
#20361=ORIENTED_EDGE('',*,*,#15054,.T.);
#20362=ORIENTED_EDGE('',*,*,#15055,.T.);
#20363=ORIENTED_EDGE('',*,*,#14984,.T.);
#20364=ORIENTED_EDGE('',*,*,#15055,.F.);
#20365=ORIENTED_EDGE('',*,*,#15054,.F.);
#20366=ORIENTED_EDGE('',*,*,#15056,.T.);
#20367=ORIENTED_EDGE('',*,*,#15057,.F.);
#20368=ORIENTED_EDGE('',*,*,#15056,.F.);
#20369=ORIENTED_EDGE('',*,*,#15058,.T.);
#20370=ORIENTED_EDGE('',*,*,#15059,.T.);
#20371=ORIENTED_EDGE('',*,*,#14980,.T.);
#20372=ORIENTED_EDGE('',*,*,#15059,.F.);
#20373=ORIENTED_EDGE('',*,*,#15058,.F.);
#20374=ORIENTED_EDGE('',*,*,#15060,.T.);
#20375=ORIENTED_EDGE('',*,*,#15061,.F.);
#20376=ORIENTED_EDGE('',*,*,#15060,.F.);
#20377=ORIENTED_EDGE('',*,*,#15062,.T.);
#20378=ORIENTED_EDGE('',*,*,#15063,.T.);
#20379=ORIENTED_EDGE('',*,*,#14983,.T.);
#20380=ORIENTED_EDGE('',*,*,#15063,.F.);
#20381=ORIENTED_EDGE('',*,*,#15062,.F.);
#20382=ORIENTED_EDGE('',*,*,#15064,.T.);
#20383=ORIENTED_EDGE('',*,*,#15065,.F.);
#20384=ORIENTED_EDGE('',*,*,#15064,.F.);
#20385=ORIENTED_EDGE('',*,*,#15066,.T.);
#20386=ORIENTED_EDGE('',*,*,#15067,.T.);
#20387=ORIENTED_EDGE('',*,*,#14981,.T.);
#20388=ORIENTED_EDGE('',*,*,#15067,.F.);
#20389=ORIENTED_EDGE('',*,*,#15066,.F.);
#20390=ORIENTED_EDGE('',*,*,#15068,.T.);
#20391=ORIENTED_EDGE('',*,*,#15069,.F.);
#20392=ORIENTED_EDGE('',*,*,#15068,.F.);
#20393=ORIENTED_EDGE('',*,*,#15070,.T.);
#20394=ORIENTED_EDGE('',*,*,#15071,.T.);
#20395=ORIENTED_EDGE('',*,*,#14982,.T.);
#20396=ORIENTED_EDGE('',*,*,#15071,.F.);
#20397=ORIENTED_EDGE('',*,*,#15070,.F.);
#20398=ORIENTED_EDGE('',*,*,#15072,.T.);
#20399=ORIENTED_EDGE('',*,*,#15073,.F.);
#20400=ORIENTED_EDGE('',*,*,#15072,.F.);
#20401=ORIENTED_EDGE('',*,*,#15074,.T.);
#20402=ORIENTED_EDGE('',*,*,#14968,.T.);
#20403=ORIENTED_EDGE('',*,*,#15075,.T.);
#20404=ORIENTED_EDGE('',*,*,#15076,.T.);
#20405=ORIENTED_EDGE('',*,*,#15077,.T.);
#20406=ORIENTED_EDGE('',*,*,#14969,.T.);
#20407=ORIENTED_EDGE('',*,*,#15074,.F.);
#20408=ORIENTED_EDGE('',*,*,#15078,.T.);
#20409=ORIENTED_EDGE('',*,*,#15079,.T.);
#20410=ORIENTED_EDGE('',*,*,#14970,.T.);
#20411=ORIENTED_EDGE('',*,*,#15077,.F.);
#20412=ORIENTED_EDGE('',*,*,#15080,.T.);
#20413=ORIENTED_EDGE('',*,*,#15075,.F.);
#20414=ORIENTED_EDGE('',*,*,#14971,.T.);
#20415=ORIENTED_EDGE('',*,*,#15079,.F.);
#20416=ORIENTED_EDGE('',*,*,#15081,.T.);
#20417=ORIENTED_EDGE('',*,*,#15078,.F.);
#20418=ORIENTED_EDGE('',*,*,#15082,.F.);
#20419=ORIENTED_EDGE('',*,*,#15083,.F.);
#20420=ORIENTED_EDGE('',*,*,#15084,.T.);
#20421=ORIENTED_EDGE('',*,*,#15076,.F.);
#20422=ORIENTED_EDGE('',*,*,#15085,.F.);
#20423=ORIENTED_EDGE('',*,*,#15086,.F.);
#20424=ORIENTED_EDGE('',*,*,#15082,.T.);
#20425=ORIENTED_EDGE('',*,*,#15087,.T.);
#20426=ORIENTED_EDGE('',*,*,#15088,.T.);
#20427=ORIENTED_EDGE('',*,*,#15089,.T.);
#20428=ORIENTED_EDGE('',*,*,#15086,.T.);
#20429=ORIENTED_EDGE('',*,*,#15087,.F.);
#20430=ORIENTED_EDGE('',*,*,#15090,.T.);
#20431=ORIENTED_EDGE('',*,*,#15091,.T.);
#20432=ORIENTED_EDGE('',*,*,#15092,.T.);
#20433=ORIENTED_EDGE('',*,*,#15093,.T.);
#20434=ORIENTED_EDGE('',*,*,#15094,.T.);
#20435=ORIENTED_EDGE('',*,*,#15091,.F.);
#20436=ORIENTED_EDGE('',*,*,#15095,.T.);
#20437=ORIENTED_EDGE('',*,*,#15093,.F.);
#20438=ORIENTED_EDGE('',*,*,#15083,.T.);
#20439=ORIENTED_EDGE('',*,*,#15089,.F.);
#20440=ORIENTED_EDGE('',*,*,#15096,.T.);
#20441=ORIENTED_EDGE('',*,*,#15081,.F.);
#20442=ORIENTED_EDGE('',*,*,#15097,.F.);
#20443=ORIENTED_EDGE('',*,*,#15090,.F.);
#20444=ORIENTED_EDGE('',*,*,#15085,.T.);
#20445=ORIENTED_EDGE('',*,*,#15088,.F.);
#20446=ORIENTED_EDGE('',*,*,#15092,.F.);
#20447=ORIENTED_EDGE('',*,*,#15094,.F.);
#20448=ORIENTED_EDGE('',*,*,#15096,.F.);
#20449=ORIENTED_EDGE('',*,*,#14993,.T.);
#20450=ORIENTED_EDGE('',*,*,#14997,.T.);
#20451=ORIENTED_EDGE('',*,*,#15001,.T.);
#20452=ORIENTED_EDGE('',*,*,#15005,.T.);
#20453=ORIENTED_EDGE('',*,*,#15009,.T.);
#20454=ORIENTED_EDGE('',*,*,#15013,.T.);
#20455=ORIENTED_EDGE('',*,*,#15017,.T.);
#20456=ORIENTED_EDGE('',*,*,#15021,.T.);
#20457=ORIENTED_EDGE('',*,*,#15025,.T.);
#20458=ORIENTED_EDGE('',*,*,#15029,.T.);
#20459=ORIENTED_EDGE('',*,*,#15033,.T.);
#20460=ORIENTED_EDGE('',*,*,#15037,.T.);
#20461=ORIENTED_EDGE('',*,*,#15041,.T.);
#20462=ORIENTED_EDGE('',*,*,#15045,.T.);
#20463=ORIENTED_EDGE('',*,*,#15049,.T.);
#20464=ORIENTED_EDGE('',*,*,#15053,.T.);
#20465=ORIENTED_EDGE('',*,*,#15057,.T.);
#20466=ORIENTED_EDGE('',*,*,#15061,.T.);
#20467=ORIENTED_EDGE('',*,*,#15065,.T.);
#20468=ORIENTED_EDGE('',*,*,#15069,.T.);
#20469=ORIENTED_EDGE('',*,*,#15073,.T.);
#20470=ORIENTED_EDGE('',*,*,#15080,.F.);
#20471=ORIENTED_EDGE('',*,*,#15084,.F.);
#20472=ORIENTED_EDGE('',*,*,#15095,.F.);
#20473=ORIENTED_EDGE('',*,*,#15097,.T.);
#20474=ORIENTED_EDGE('',*,*,#15098,.T.);
#20475=ORIENTED_EDGE('',*,*,#15099,.T.);
#20476=ORIENTED_EDGE('',*,*,#15100,.T.);
#20477=ORIENTED_EDGE('',*,*,#15101,.T.);
#20478=ORIENTED_EDGE('',*,*,#15102,.T.);
#20479=ORIENTED_EDGE('',*,*,#15103,.T.);
#20480=ORIENTED_EDGE('',*,*,#15100,.F.);
#20481=ORIENTED_EDGE('',*,*,#15104,.T.);
#20482=ORIENTED_EDGE('',*,*,#15105,.T.);
#20483=ORIENTED_EDGE('',*,*,#15106,.T.);
#20484=ORIENTED_EDGE('',*,*,#15102,.F.);
#20485=ORIENTED_EDGE('',*,*,#15107,.T.);
#20486=ORIENTED_EDGE('',*,*,#15108,.T.);
#20487=ORIENTED_EDGE('',*,*,#15109,.T.);
#20488=ORIENTED_EDGE('',*,*,#15105,.F.);
#20489=ORIENTED_EDGE('',*,*,#15110,.T.);
#20490=ORIENTED_EDGE('',*,*,#15111,.T.);
#20491=ORIENTED_EDGE('',*,*,#15112,.T.);
#20492=ORIENTED_EDGE('',*,*,#15108,.F.);
#20493=ORIENTED_EDGE('',*,*,#15113,.T.);
#20494=ORIENTED_EDGE('',*,*,#15113,.F.);
#20495=ORIENTED_EDGE('',*,*,#15114,.F.);
#20496=ORIENTED_EDGE('',*,*,#15115,.F.);
#20497=ORIENTED_EDGE('',*,*,#15116,.T.);
#20498=ORIENTED_EDGE('',*,*,#15110,.F.);
#20499=ORIENTED_EDGE('',*,*,#15117,.F.);
#20500=ORIENTED_EDGE('',*,*,#15118,.F.);
#20501=ORIENTED_EDGE('',*,*,#15114,.T.);
#20502=ORIENTED_EDGE('',*,*,#15107,.F.);
#20503=ORIENTED_EDGE('',*,*,#15119,.F.);
#20504=ORIENTED_EDGE('',*,*,#15120,.F.);
#20505=ORIENTED_EDGE('',*,*,#15117,.T.);
#20506=ORIENTED_EDGE('',*,*,#15104,.F.);
#20507=ORIENTED_EDGE('',*,*,#15121,.F.);
#20508=ORIENTED_EDGE('',*,*,#15122,.F.);
#20509=ORIENTED_EDGE('',*,*,#15119,.T.);
#20510=ORIENTED_EDGE('',*,*,#15099,.F.);
#20511=ORIENTED_EDGE('',*,*,#15123,.F.);
#20512=ORIENTED_EDGE('',*,*,#15124,.F.);
#20513=ORIENTED_EDGE('',*,*,#15121,.T.);
#20514=ORIENTED_EDGE('',*,*,#15125,.T.);
#20515=ORIENTED_EDGE('',*,*,#15115,.T.);
#20516=ORIENTED_EDGE('',*,*,#15126,.T.);
#20517=ORIENTED_EDGE('',*,*,#15127,.T.);
#20518=ORIENTED_EDGE('',*,*,#15126,.F.);
#20519=ORIENTED_EDGE('',*,*,#15118,.T.);
#20520=ORIENTED_EDGE('',*,*,#15128,.T.);
#20521=ORIENTED_EDGE('',*,*,#15129,.T.);
#20522=ORIENTED_EDGE('',*,*,#15130,.T.);
#20523=ORIENTED_EDGE('',*,*,#15131,.T.);
#20524=ORIENTED_EDGE('',*,*,#15128,.F.);
#20525=ORIENTED_EDGE('',*,*,#15120,.T.);
#20526=ORIENTED_EDGE('',*,*,#15130,.F.);
#20527=ORIENTED_EDGE('',*,*,#15122,.T.);
#20528=ORIENTED_EDGE('',*,*,#15132,.T.);
#20529=ORIENTED_EDGE('',*,*,#15133,.T.);
#20530=ORIENTED_EDGE('',*,*,#15134,.T.);
#20531=ORIENTED_EDGE('',*,*,#15135,.T.);
#20532=ORIENTED_EDGE('',*,*,#15132,.F.);
#20533=ORIENTED_EDGE('',*,*,#15124,.T.);
#20534=ORIENTED_EDGE('',*,*,#15136,.F.);
#20535=ORIENTED_EDGE('',*,*,#15137,.T.);
#20536=ORIENTED_EDGE('',*,*,#15138,.F.);
#20537=ORIENTED_EDGE('',*,*,#15137,.F.);
#20538=ORIENTED_EDGE('',*,*,#15139,.F.);
#20539=ORIENTED_EDGE('',*,*,#15140,.T.);
#20540=ORIENTED_EDGE('',*,*,#15141,.F.);
#20541=ORIENTED_EDGE('',*,*,#15140,.F.);
#20542=ORIENTED_EDGE('',*,*,#15142,.F.);
#20543=ORIENTED_EDGE('',*,*,#15143,.T.);
#20544=ORIENTED_EDGE('',*,*,#15144,.F.);
#20545=ORIENTED_EDGE('',*,*,#15143,.F.);
#20546=ORIENTED_EDGE('',*,*,#15145,.F.);
#20547=ORIENTED_EDGE('',*,*,#15146,.T.);
#20548=ORIENTED_EDGE('',*,*,#15147,.F.);
#20549=ORIENTED_EDGE('',*,*,#15146,.F.);
#20550=ORIENTED_EDGE('',*,*,#15148,.F.);
#20551=ORIENTED_EDGE('',*,*,#15149,.T.);
#20552=ORIENTED_EDGE('',*,*,#15150,.F.);
#20553=ORIENTED_EDGE('',*,*,#15149,.F.);
#20554=ORIENTED_EDGE('',*,*,#15151,.F.);
#20555=ORIENTED_EDGE('',*,*,#15152,.T.);
#20556=ORIENTED_EDGE('',*,*,#15153,.F.);
#20557=ORIENTED_EDGE('',*,*,#15152,.F.);
#20558=ORIENTED_EDGE('',*,*,#15154,.F.);
#20559=ORIENTED_EDGE('',*,*,#15155,.T.);
#20560=ORIENTED_EDGE('',*,*,#15156,.F.);
#20561=ORIENTED_EDGE('',*,*,#15155,.F.);
#20562=ORIENTED_EDGE('',*,*,#15157,.F.);
#20563=ORIENTED_EDGE('',*,*,#15158,.T.);
#20564=ORIENTED_EDGE('',*,*,#15159,.F.);
#20565=ORIENTED_EDGE('',*,*,#15158,.F.);
#20566=ORIENTED_EDGE('',*,*,#15160,.F.);
#20567=ORIENTED_EDGE('',*,*,#15161,.T.);
#20568=ORIENTED_EDGE('',*,*,#15162,.F.);
#20569=ORIENTED_EDGE('',*,*,#15161,.F.);
#20570=ORIENTED_EDGE('',*,*,#15163,.F.);
#20571=ORIENTED_EDGE('',*,*,#15164,.T.);
#20572=ORIENTED_EDGE('',*,*,#15165,.F.);
#20573=ORIENTED_EDGE('',*,*,#15164,.F.);
#20574=ORIENTED_EDGE('',*,*,#15166,.F.);
#20575=ORIENTED_EDGE('',*,*,#15134,.F.);
#20576=ORIENTED_EDGE('',*,*,#15123,.T.);
#20577=ORIENTED_EDGE('',*,*,#15098,.F.);
#20578=ORIENTED_EDGE('',*,*,#15167,.F.);
#20579=ORIENTED_EDGE('',*,*,#15168,.F.);
#20580=ORIENTED_EDGE('',*,*,#15169,.F.);
#20581=ORIENTED_EDGE('',*,*,#15168,.T.);
#20582=ORIENTED_EDGE('',*,*,#15170,.F.);
#20583=ORIENTED_EDGE('',*,*,#15171,.F.);
#20584=ORIENTED_EDGE('',*,*,#15172,.F.);
#20585=ORIENTED_EDGE('',*,*,#15171,.T.);
#20586=ORIENTED_EDGE('',*,*,#15173,.F.);
#20587=ORIENTED_EDGE('',*,*,#15174,.F.);
#20588=ORIENTED_EDGE('',*,*,#15175,.F.);
#20589=ORIENTED_EDGE('',*,*,#15174,.T.);
#20590=ORIENTED_EDGE('',*,*,#15176,.F.);
#20591=ORIENTED_EDGE('',*,*,#15177,.F.);
#20592=ORIENTED_EDGE('',*,*,#15178,.F.);
#20593=ORIENTED_EDGE('',*,*,#15177,.T.);
#20594=ORIENTED_EDGE('',*,*,#15179,.F.);
#20595=ORIENTED_EDGE('',*,*,#15180,.F.);
#20596=ORIENTED_EDGE('',*,*,#15181,.F.);
#20597=ORIENTED_EDGE('',*,*,#15180,.T.);
#20598=ORIENTED_EDGE('',*,*,#15182,.F.);
#20599=ORIENTED_EDGE('',*,*,#15183,.F.);
#20600=ORIENTED_EDGE('',*,*,#15184,.F.);
#20601=ORIENTED_EDGE('',*,*,#15183,.T.);
#20602=ORIENTED_EDGE('',*,*,#15185,.F.);
#20603=ORIENTED_EDGE('',*,*,#15186,.F.);
#20604=ORIENTED_EDGE('',*,*,#15187,.F.);
#20605=ORIENTED_EDGE('',*,*,#15186,.T.);
#20606=ORIENTED_EDGE('',*,*,#15188,.F.);
#20607=ORIENTED_EDGE('',*,*,#15189,.F.);
#20608=ORIENTED_EDGE('',*,*,#15190,.F.);
#20609=ORIENTED_EDGE('',*,*,#15189,.T.);
#20610=ORIENTED_EDGE('',*,*,#15191,.F.);
#20611=ORIENTED_EDGE('',*,*,#15192,.F.);
#20612=ORIENTED_EDGE('',*,*,#15193,.F.);
#20613=ORIENTED_EDGE('',*,*,#15192,.T.);
#20614=ORIENTED_EDGE('',*,*,#15194,.F.);
#20615=ORIENTED_EDGE('',*,*,#15195,.F.);
#20616=ORIENTED_EDGE('',*,*,#15196,.F.);
#20617=ORIENTED_EDGE('',*,*,#15195,.T.);
#20618=ORIENTED_EDGE('',*,*,#15197,.F.);
#20619=ORIENTED_EDGE('',*,*,#15198,.F.);
#20620=ORIENTED_EDGE('',*,*,#15199,.F.);
#20621=ORIENTED_EDGE('',*,*,#15198,.T.);
#20622=ORIENTED_EDGE('',*,*,#15200,.F.);
#20623=ORIENTED_EDGE('',*,*,#15201,.F.);
#20624=ORIENTED_EDGE('',*,*,#15202,.F.);
#20625=ORIENTED_EDGE('',*,*,#15201,.T.);
#20626=ORIENTED_EDGE('',*,*,#15203,.F.);
#20627=ORIENTED_EDGE('',*,*,#15204,.F.);
#20628=ORIENTED_EDGE('',*,*,#15205,.F.);
#20629=ORIENTED_EDGE('',*,*,#15204,.T.);
#20630=ORIENTED_EDGE('',*,*,#15206,.F.);
#20631=ORIENTED_EDGE('',*,*,#15207,.F.);
#20632=ORIENTED_EDGE('',*,*,#15208,.F.);
#20633=ORIENTED_EDGE('',*,*,#15207,.T.);
#20634=ORIENTED_EDGE('',*,*,#15209,.F.);
#20635=ORIENTED_EDGE('',*,*,#15210,.F.);
#20636=ORIENTED_EDGE('',*,*,#15211,.F.);
#20637=ORIENTED_EDGE('',*,*,#15210,.T.);
#20638=ORIENTED_EDGE('',*,*,#15212,.F.);
#20639=ORIENTED_EDGE('',*,*,#15213,.F.);
#20640=ORIENTED_EDGE('',*,*,#15214,.F.);
#20641=ORIENTED_EDGE('',*,*,#15213,.T.);
#20642=ORIENTED_EDGE('',*,*,#15215,.F.);
#20643=ORIENTED_EDGE('',*,*,#15216,.F.);
#20644=ORIENTED_EDGE('',*,*,#15217,.F.);
#20645=ORIENTED_EDGE('',*,*,#15216,.T.);
#20646=ORIENTED_EDGE('',*,*,#15218,.F.);
#20647=ORIENTED_EDGE('',*,*,#15219,.F.);
#20648=ORIENTED_EDGE('',*,*,#15220,.F.);
#20649=ORIENTED_EDGE('',*,*,#15219,.T.);
#20650=ORIENTED_EDGE('',*,*,#15221,.F.);
#20651=ORIENTED_EDGE('',*,*,#15222,.F.);
#20652=ORIENTED_EDGE('',*,*,#15223,.F.);
#20653=ORIENTED_EDGE('',*,*,#15222,.T.);
#20654=ORIENTED_EDGE('',*,*,#15224,.F.);
#20655=ORIENTED_EDGE('',*,*,#15225,.F.);
#20656=ORIENTED_EDGE('',*,*,#15226,.F.);
#20657=ORIENTED_EDGE('',*,*,#15225,.T.);
#20658=ORIENTED_EDGE('',*,*,#15227,.F.);
#20659=ORIENTED_EDGE('',*,*,#15228,.F.);
#20660=ORIENTED_EDGE('',*,*,#15229,.F.);
#20661=ORIENTED_EDGE('',*,*,#15228,.T.);
#20662=ORIENTED_EDGE('',*,*,#15230,.F.);
#20663=ORIENTED_EDGE('',*,*,#15231,.F.);
#20664=ORIENTED_EDGE('',*,*,#15232,.F.);
#20665=ORIENTED_EDGE('',*,*,#15231,.T.);
#20666=ORIENTED_EDGE('',*,*,#15233,.F.);
#20667=ORIENTED_EDGE('',*,*,#15234,.F.);
#20668=ORIENTED_EDGE('',*,*,#15235,.F.);
#20669=ORIENTED_EDGE('',*,*,#15234,.T.);
#20670=ORIENTED_EDGE('',*,*,#15236,.F.);
#20671=ORIENTED_EDGE('',*,*,#15237,.F.);
#20672=ORIENTED_EDGE('',*,*,#15238,.F.);
#20673=ORIENTED_EDGE('',*,*,#15237,.T.);
#20674=ORIENTED_EDGE('',*,*,#15239,.F.);
#20675=ORIENTED_EDGE('',*,*,#15240,.F.);
#20676=ORIENTED_EDGE('',*,*,#15241,.F.);
#20677=ORIENTED_EDGE('',*,*,#15240,.T.);
#20678=ORIENTED_EDGE('',*,*,#15242,.F.);
#20679=ORIENTED_EDGE('',*,*,#15243,.F.);
#20680=ORIENTED_EDGE('',*,*,#15244,.F.);
#20681=ORIENTED_EDGE('',*,*,#15243,.T.);
#20682=ORIENTED_EDGE('',*,*,#15245,.F.);
#20683=ORIENTED_EDGE('',*,*,#15246,.F.);
#20684=ORIENTED_EDGE('',*,*,#15247,.F.);
#20685=ORIENTED_EDGE('',*,*,#15246,.T.);
#20686=ORIENTED_EDGE('',*,*,#15248,.F.);
#20687=ORIENTED_EDGE('',*,*,#15249,.F.);
#20688=ORIENTED_EDGE('',*,*,#15250,.F.);
#20689=ORIENTED_EDGE('',*,*,#15249,.T.);
#20690=ORIENTED_EDGE('',*,*,#15251,.F.);
#20691=ORIENTED_EDGE('',*,*,#15252,.F.);
#20692=ORIENTED_EDGE('',*,*,#15253,.F.);
#20693=ORIENTED_EDGE('',*,*,#15252,.T.);
#20694=ORIENTED_EDGE('',*,*,#15254,.F.);
#20695=ORIENTED_EDGE('',*,*,#15255,.F.);
#20696=ORIENTED_EDGE('',*,*,#15256,.F.);
#20697=ORIENTED_EDGE('',*,*,#15255,.T.);
#20698=ORIENTED_EDGE('',*,*,#15257,.F.);
#20699=ORIENTED_EDGE('',*,*,#15258,.F.);
#20700=ORIENTED_EDGE('',*,*,#15259,.F.);
#20701=ORIENTED_EDGE('',*,*,#15258,.T.);
#20702=ORIENTED_EDGE('',*,*,#15260,.F.);
#20703=ORIENTED_EDGE('',*,*,#15261,.F.);
#20704=ORIENTED_EDGE('',*,*,#15262,.F.);
#20705=ORIENTED_EDGE('',*,*,#15261,.T.);
#20706=ORIENTED_EDGE('',*,*,#15263,.F.);
#20707=ORIENTED_EDGE('',*,*,#15264,.F.);
#20708=ORIENTED_EDGE('',*,*,#15265,.F.);
#20709=ORIENTED_EDGE('',*,*,#15264,.T.);
#20710=ORIENTED_EDGE('',*,*,#15266,.F.);
#20711=ORIENTED_EDGE('',*,*,#15267,.F.);
#20712=ORIENTED_EDGE('',*,*,#15268,.F.);
#20713=ORIENTED_EDGE('',*,*,#15267,.T.);
#20714=ORIENTED_EDGE('',*,*,#15269,.F.);
#20715=ORIENTED_EDGE('',*,*,#15270,.F.);
#20716=ORIENTED_EDGE('',*,*,#15271,.F.);
#20717=ORIENTED_EDGE('',*,*,#15270,.T.);
#20718=ORIENTED_EDGE('',*,*,#15272,.F.);
#20719=ORIENTED_EDGE('',*,*,#15273,.F.);
#20720=ORIENTED_EDGE('',*,*,#15274,.F.);
#20721=ORIENTED_EDGE('',*,*,#15273,.T.);
#20722=ORIENTED_EDGE('',*,*,#15275,.F.);
#20723=ORIENTED_EDGE('',*,*,#15276,.F.);
#20724=ORIENTED_EDGE('',*,*,#15277,.F.);
#20725=ORIENTED_EDGE('',*,*,#15276,.T.);
#20726=ORIENTED_EDGE('',*,*,#15278,.F.);
#20727=ORIENTED_EDGE('',*,*,#15279,.F.);
#20728=ORIENTED_EDGE('',*,*,#15280,.F.);
#20729=ORIENTED_EDGE('',*,*,#15279,.T.);
#20730=ORIENTED_EDGE('',*,*,#15281,.F.);
#20731=ORIENTED_EDGE('',*,*,#15282,.F.);
#20732=ORIENTED_EDGE('',*,*,#15283,.F.);
#20733=ORIENTED_EDGE('',*,*,#15282,.T.);
#20734=ORIENTED_EDGE('',*,*,#15284,.F.);
#20735=ORIENTED_EDGE('',*,*,#15285,.F.);
#20736=ORIENTED_EDGE('',*,*,#15286,.F.);
#20737=ORIENTED_EDGE('',*,*,#15285,.T.);
#20738=ORIENTED_EDGE('',*,*,#15287,.F.);
#20739=ORIENTED_EDGE('',*,*,#15288,.F.);
#20740=ORIENTED_EDGE('',*,*,#15289,.F.);
#20741=ORIENTED_EDGE('',*,*,#15288,.T.);
#20742=ORIENTED_EDGE('',*,*,#15290,.F.);
#20743=ORIENTED_EDGE('',*,*,#15291,.F.);
#20744=ORIENTED_EDGE('',*,*,#15292,.F.);
#20745=ORIENTED_EDGE('',*,*,#15291,.T.);
#20746=ORIENTED_EDGE('',*,*,#15293,.F.);
#20747=ORIENTED_EDGE('',*,*,#15294,.F.);
#20748=ORIENTED_EDGE('',*,*,#15295,.F.);
#20749=ORIENTED_EDGE('',*,*,#15294,.T.);
#20750=ORIENTED_EDGE('',*,*,#15296,.F.);
#20751=ORIENTED_EDGE('',*,*,#15297,.F.);
#20752=ORIENTED_EDGE('',*,*,#15298,.F.);
#20753=ORIENTED_EDGE('',*,*,#15297,.T.);
#20754=ORIENTED_EDGE('',*,*,#15299,.F.);
#20755=ORIENTED_EDGE('',*,*,#15300,.F.);
#20756=ORIENTED_EDGE('',*,*,#15301,.F.);
#20757=ORIENTED_EDGE('',*,*,#15300,.T.);
#20758=ORIENTED_EDGE('',*,*,#15302,.F.);
#20759=ORIENTED_EDGE('',*,*,#15303,.F.);
#20760=ORIENTED_EDGE('',*,*,#15304,.F.);
#20761=ORIENTED_EDGE('',*,*,#15303,.T.);
#20762=ORIENTED_EDGE('',*,*,#15305,.F.);
#20763=ORIENTED_EDGE('',*,*,#15306,.F.);
#20764=ORIENTED_EDGE('',*,*,#15307,.F.);
#20765=ORIENTED_EDGE('',*,*,#15306,.T.);
#20766=ORIENTED_EDGE('',*,*,#15308,.F.);
#20767=ORIENTED_EDGE('',*,*,#15309,.F.);
#20768=ORIENTED_EDGE('',*,*,#15310,.F.);
#20769=ORIENTED_EDGE('',*,*,#15309,.T.);
#20770=ORIENTED_EDGE('',*,*,#15311,.F.);
#20771=ORIENTED_EDGE('',*,*,#15312,.F.);
#20772=ORIENTED_EDGE('',*,*,#15313,.F.);
#20773=ORIENTED_EDGE('',*,*,#15312,.T.);
#20774=ORIENTED_EDGE('',*,*,#15314,.F.);
#20775=ORIENTED_EDGE('',*,*,#15315,.F.);
#20776=ORIENTED_EDGE('',*,*,#15316,.F.);
#20777=ORIENTED_EDGE('',*,*,#15315,.T.);
#20778=ORIENTED_EDGE('',*,*,#15317,.F.);
#20779=ORIENTED_EDGE('',*,*,#15318,.F.);
#20780=ORIENTED_EDGE('',*,*,#15319,.F.);
#20781=ORIENTED_EDGE('',*,*,#15318,.T.);
#20782=ORIENTED_EDGE('',*,*,#15320,.F.);
#20783=ORIENTED_EDGE('',*,*,#15321,.F.);
#20784=ORIENTED_EDGE('',*,*,#15322,.F.);
#20785=ORIENTED_EDGE('',*,*,#15321,.T.);
#20786=ORIENTED_EDGE('',*,*,#15323,.F.);
#20787=ORIENTED_EDGE('',*,*,#15324,.F.);
#20788=ORIENTED_EDGE('',*,*,#15325,.F.);
#20789=ORIENTED_EDGE('',*,*,#15324,.T.);
#20790=ORIENTED_EDGE('',*,*,#15326,.F.);
#20791=ORIENTED_EDGE('',*,*,#15327,.F.);
#20792=ORIENTED_EDGE('',*,*,#15328,.F.);
#20793=ORIENTED_EDGE('',*,*,#15327,.T.);
#20794=ORIENTED_EDGE('',*,*,#15329,.F.);
#20795=ORIENTED_EDGE('',*,*,#15330,.F.);
#20796=ORIENTED_EDGE('',*,*,#15331,.F.);
#20797=ORIENTED_EDGE('',*,*,#15330,.T.);
#20798=ORIENTED_EDGE('',*,*,#15332,.F.);
#20799=ORIENTED_EDGE('',*,*,#15333,.F.);
#20800=ORIENTED_EDGE('',*,*,#15334,.F.);
#20801=ORIENTED_EDGE('',*,*,#15333,.T.);
#20802=ORIENTED_EDGE('',*,*,#15335,.F.);
#20803=ORIENTED_EDGE('',*,*,#15336,.F.);
#20804=ORIENTED_EDGE('',*,*,#15337,.F.);
#20805=ORIENTED_EDGE('',*,*,#15336,.T.);
#20806=ORIENTED_EDGE('',*,*,#15338,.F.);
#20807=ORIENTED_EDGE('',*,*,#15339,.F.);
#20808=ORIENTED_EDGE('',*,*,#15340,.F.);
#20809=ORIENTED_EDGE('',*,*,#15339,.T.);
#20810=ORIENTED_EDGE('',*,*,#15341,.F.);
#20811=ORIENTED_EDGE('',*,*,#15342,.F.);
#20812=ORIENTED_EDGE('',*,*,#15343,.F.);
#20813=ORIENTED_EDGE('',*,*,#15342,.T.);
#20814=ORIENTED_EDGE('',*,*,#15344,.F.);
#20815=ORIENTED_EDGE('',*,*,#15345,.F.);
#20816=ORIENTED_EDGE('',*,*,#15346,.F.);
#20817=ORIENTED_EDGE('',*,*,#15345,.T.);
#20818=ORIENTED_EDGE('',*,*,#15347,.F.);
#20819=ORIENTED_EDGE('',*,*,#15348,.F.);
#20820=ORIENTED_EDGE('',*,*,#15349,.F.);
#20821=ORIENTED_EDGE('',*,*,#15348,.T.);
#20822=ORIENTED_EDGE('',*,*,#15350,.F.);
#20823=ORIENTED_EDGE('',*,*,#15351,.F.);
#20824=ORIENTED_EDGE('',*,*,#15352,.F.);
#20825=ORIENTED_EDGE('',*,*,#15351,.T.);
#20826=ORIENTED_EDGE('',*,*,#15353,.F.);
#20827=ORIENTED_EDGE('',*,*,#15354,.F.);
#20828=ORIENTED_EDGE('',*,*,#15355,.F.);
#20829=ORIENTED_EDGE('',*,*,#15354,.T.);
#20830=ORIENTED_EDGE('',*,*,#15356,.F.);
#20831=ORIENTED_EDGE('',*,*,#15357,.F.);
#20832=ORIENTED_EDGE('',*,*,#15358,.F.);
#20833=ORIENTED_EDGE('',*,*,#15357,.T.);
#20834=ORIENTED_EDGE('',*,*,#15359,.F.);
#20835=ORIENTED_EDGE('',*,*,#15360,.F.);
#20836=ORIENTED_EDGE('',*,*,#15361,.F.);
#20837=ORIENTED_EDGE('',*,*,#15360,.T.);
#20838=ORIENTED_EDGE('',*,*,#15362,.F.);
#20839=ORIENTED_EDGE('',*,*,#15363,.F.);
#20840=ORIENTED_EDGE('',*,*,#15364,.F.);
#20841=ORIENTED_EDGE('',*,*,#15363,.T.);
#20842=ORIENTED_EDGE('',*,*,#15365,.F.);
#20843=ORIENTED_EDGE('',*,*,#15366,.F.);
#20844=ORIENTED_EDGE('',*,*,#15367,.F.);
#20845=ORIENTED_EDGE('',*,*,#15366,.T.);
#20846=ORIENTED_EDGE('',*,*,#15368,.F.);
#20847=ORIENTED_EDGE('',*,*,#15369,.F.);
#20848=ORIENTED_EDGE('',*,*,#15370,.F.);
#20849=ORIENTED_EDGE('',*,*,#15369,.T.);
#20850=ORIENTED_EDGE('',*,*,#15371,.F.);
#20851=ORIENTED_EDGE('',*,*,#15372,.F.);
#20852=ORIENTED_EDGE('',*,*,#15373,.F.);
#20853=ORIENTED_EDGE('',*,*,#15372,.T.);
#20854=ORIENTED_EDGE('',*,*,#15374,.F.);
#20855=ORIENTED_EDGE('',*,*,#15375,.F.);
#20856=ORIENTED_EDGE('',*,*,#15376,.F.);
#20857=ORIENTED_EDGE('',*,*,#15375,.T.);
#20858=ORIENTED_EDGE('',*,*,#15377,.F.);
#20859=ORIENTED_EDGE('',*,*,#15378,.F.);
#20860=ORIENTED_EDGE('',*,*,#15379,.F.);
#20861=ORIENTED_EDGE('',*,*,#15378,.T.);
#20862=ORIENTED_EDGE('',*,*,#15380,.F.);
#20863=ORIENTED_EDGE('',*,*,#15381,.F.);
#20864=ORIENTED_EDGE('',*,*,#15382,.F.);
#20865=ORIENTED_EDGE('',*,*,#15381,.T.);
#20866=ORIENTED_EDGE('',*,*,#15383,.F.);
#20867=ORIENTED_EDGE('',*,*,#15384,.F.);
#20868=ORIENTED_EDGE('',*,*,#15385,.F.);
#20869=ORIENTED_EDGE('',*,*,#15384,.T.);
#20870=ORIENTED_EDGE('',*,*,#15386,.F.);
#20871=ORIENTED_EDGE('',*,*,#15387,.F.);
#20872=ORIENTED_EDGE('',*,*,#15388,.F.);
#20873=ORIENTED_EDGE('',*,*,#15387,.T.);
#20874=ORIENTED_EDGE('',*,*,#15389,.F.);
#20875=ORIENTED_EDGE('',*,*,#15390,.F.);
#20876=ORIENTED_EDGE('',*,*,#15391,.F.);
#20877=ORIENTED_EDGE('',*,*,#15390,.T.);
#20878=ORIENTED_EDGE('',*,*,#15392,.F.);
#20879=ORIENTED_EDGE('',*,*,#15393,.F.);
#20880=ORIENTED_EDGE('',*,*,#15394,.F.);
#20881=ORIENTED_EDGE('',*,*,#15393,.T.);
#20882=ORIENTED_EDGE('',*,*,#15395,.F.);
#20883=ORIENTED_EDGE('',*,*,#15396,.F.);
#20884=ORIENTED_EDGE('',*,*,#15397,.F.);
#20885=ORIENTED_EDGE('',*,*,#15396,.T.);
#20886=ORIENTED_EDGE('',*,*,#15398,.F.);
#20887=ORIENTED_EDGE('',*,*,#15399,.F.);
#20888=ORIENTED_EDGE('',*,*,#15400,.F.);
#20889=ORIENTED_EDGE('',*,*,#15399,.T.);
#20890=ORIENTED_EDGE('',*,*,#15401,.F.);
#20891=ORIENTED_EDGE('',*,*,#15402,.F.);
#20892=ORIENTED_EDGE('',*,*,#15403,.F.);
#20893=ORIENTED_EDGE('',*,*,#15402,.T.);
#20894=ORIENTED_EDGE('',*,*,#15404,.F.);
#20895=ORIENTED_EDGE('',*,*,#15405,.F.);
#20896=ORIENTED_EDGE('',*,*,#15406,.F.);
#20897=ORIENTED_EDGE('',*,*,#15405,.T.);
#20898=ORIENTED_EDGE('',*,*,#15407,.F.);
#20899=ORIENTED_EDGE('',*,*,#15408,.F.);
#20900=ORIENTED_EDGE('',*,*,#15409,.F.);
#20901=ORIENTED_EDGE('',*,*,#15408,.T.);
#20902=ORIENTED_EDGE('',*,*,#15410,.F.);
#20903=ORIENTED_EDGE('',*,*,#15411,.F.);
#20904=ORIENTED_EDGE('',*,*,#15412,.F.);
#20905=ORIENTED_EDGE('',*,*,#15411,.T.);
#20906=ORIENTED_EDGE('',*,*,#15413,.F.);
#20907=ORIENTED_EDGE('',*,*,#15414,.F.);
#20908=ORIENTED_EDGE('',*,*,#15415,.F.);
#20909=ORIENTED_EDGE('',*,*,#15414,.T.);
#20910=ORIENTED_EDGE('',*,*,#15416,.F.);
#20911=ORIENTED_EDGE('',*,*,#15417,.F.);
#20912=ORIENTED_EDGE('',*,*,#15418,.F.);
#20913=ORIENTED_EDGE('',*,*,#15417,.T.);
#20914=ORIENTED_EDGE('',*,*,#15419,.F.);
#20915=ORIENTED_EDGE('',*,*,#15420,.F.);
#20916=ORIENTED_EDGE('',*,*,#15421,.F.);
#20917=ORIENTED_EDGE('',*,*,#15420,.T.);
#20918=ORIENTED_EDGE('',*,*,#15422,.F.);
#20919=ORIENTED_EDGE('',*,*,#15423,.F.);
#20920=ORIENTED_EDGE('',*,*,#15424,.F.);
#20921=ORIENTED_EDGE('',*,*,#15423,.T.);
#20922=ORIENTED_EDGE('',*,*,#15425,.F.);
#20923=ORIENTED_EDGE('',*,*,#15426,.F.);
#20924=ORIENTED_EDGE('',*,*,#15427,.F.);
#20925=ORIENTED_EDGE('',*,*,#15426,.T.);
#20926=ORIENTED_EDGE('',*,*,#15428,.F.);
#20927=ORIENTED_EDGE('',*,*,#15429,.F.);
#20928=ORIENTED_EDGE('',*,*,#15430,.F.);
#20929=ORIENTED_EDGE('',*,*,#15429,.T.);
#20930=ORIENTED_EDGE('',*,*,#15431,.F.);
#20931=ORIENTED_EDGE('',*,*,#15432,.F.);
#20932=ORIENTED_EDGE('',*,*,#15433,.F.);
#20933=ORIENTED_EDGE('',*,*,#15432,.T.);
#20934=ORIENTED_EDGE('',*,*,#15434,.F.);
#20935=ORIENTED_EDGE('',*,*,#15435,.F.);
#20936=ORIENTED_EDGE('',*,*,#15436,.F.);
#20937=ORIENTED_EDGE('',*,*,#15435,.T.);
#20938=ORIENTED_EDGE('',*,*,#15437,.F.);
#20939=ORIENTED_EDGE('',*,*,#15438,.F.);
#20940=ORIENTED_EDGE('',*,*,#15439,.F.);
#20941=ORIENTED_EDGE('',*,*,#15438,.T.);
#20942=ORIENTED_EDGE('',*,*,#15440,.F.);
#20943=ORIENTED_EDGE('',*,*,#15441,.F.);
#20944=ORIENTED_EDGE('',*,*,#15442,.F.);
#20945=ORIENTED_EDGE('',*,*,#15441,.T.);
#20946=ORIENTED_EDGE('',*,*,#15443,.F.);
#20947=ORIENTED_EDGE('',*,*,#15444,.F.);
#20948=ORIENTED_EDGE('',*,*,#15445,.F.);
#20949=ORIENTED_EDGE('',*,*,#15444,.T.);
#20950=ORIENTED_EDGE('',*,*,#15446,.F.);
#20951=ORIENTED_EDGE('',*,*,#15447,.F.);
#20952=ORIENTED_EDGE('',*,*,#15448,.F.);
#20953=ORIENTED_EDGE('',*,*,#15447,.T.);
#20954=ORIENTED_EDGE('',*,*,#15449,.F.);
#20955=ORIENTED_EDGE('',*,*,#15450,.F.);
#20956=ORIENTED_EDGE('',*,*,#15451,.F.);
#20957=ORIENTED_EDGE('',*,*,#15450,.T.);
#20958=ORIENTED_EDGE('',*,*,#15452,.F.);
#20959=ORIENTED_EDGE('',*,*,#15453,.F.);
#20960=ORIENTED_EDGE('',*,*,#15454,.F.);
#20961=ORIENTED_EDGE('',*,*,#15453,.T.);
#20962=ORIENTED_EDGE('',*,*,#15455,.F.);
#20963=ORIENTED_EDGE('',*,*,#15456,.F.);
#20964=ORIENTED_EDGE('',*,*,#15457,.F.);
#20965=ORIENTED_EDGE('',*,*,#15456,.T.);
#20966=ORIENTED_EDGE('',*,*,#15458,.F.);
#20967=ORIENTED_EDGE('',*,*,#15459,.F.);
#20968=ORIENTED_EDGE('',*,*,#15460,.F.);
#20969=ORIENTED_EDGE('',*,*,#15459,.T.);
#20970=ORIENTED_EDGE('',*,*,#15461,.F.);
#20971=ORIENTED_EDGE('',*,*,#15462,.F.);
#20972=ORIENTED_EDGE('',*,*,#15463,.F.);
#20973=ORIENTED_EDGE('',*,*,#15462,.T.);
#20974=ORIENTED_EDGE('',*,*,#15464,.F.);
#20975=ORIENTED_EDGE('',*,*,#15465,.F.);
#20976=ORIENTED_EDGE('',*,*,#15466,.F.);
#20977=ORIENTED_EDGE('',*,*,#15465,.T.);
#20978=ORIENTED_EDGE('',*,*,#15467,.F.);
#20979=ORIENTED_EDGE('',*,*,#15468,.F.);
#20980=ORIENTED_EDGE('',*,*,#15469,.F.);
#20981=ORIENTED_EDGE('',*,*,#15468,.T.);
#20982=ORIENTED_EDGE('',*,*,#15470,.F.);
#20983=ORIENTED_EDGE('',*,*,#15471,.F.);
#20984=ORIENTED_EDGE('',*,*,#15472,.F.);
#20985=ORIENTED_EDGE('',*,*,#15471,.T.);
#20986=ORIENTED_EDGE('',*,*,#15473,.F.);
#20987=ORIENTED_EDGE('',*,*,#15474,.F.);
#20988=ORIENTED_EDGE('',*,*,#15475,.F.);
#20989=ORIENTED_EDGE('',*,*,#15474,.T.);
#20990=ORIENTED_EDGE('',*,*,#15476,.F.);
#20991=ORIENTED_EDGE('',*,*,#15477,.F.);
#20992=ORIENTED_EDGE('',*,*,#15478,.F.);
#20993=ORIENTED_EDGE('',*,*,#15477,.T.);
#20994=ORIENTED_EDGE('',*,*,#15479,.F.);
#20995=ORIENTED_EDGE('',*,*,#15480,.F.);
#20996=ORIENTED_EDGE('',*,*,#15481,.F.);
#20997=ORIENTED_EDGE('',*,*,#15480,.T.);
#20998=ORIENTED_EDGE('',*,*,#15482,.F.);
#20999=ORIENTED_EDGE('',*,*,#15483,.F.);
#21000=ORIENTED_EDGE('',*,*,#15484,.F.);
#21001=ORIENTED_EDGE('',*,*,#15483,.T.);
#21002=ORIENTED_EDGE('',*,*,#15485,.F.);
#21003=ORIENTED_EDGE('',*,*,#15486,.F.);
#21004=ORIENTED_EDGE('',*,*,#15487,.F.);
#21005=ORIENTED_EDGE('',*,*,#15486,.T.);
#21006=ORIENTED_EDGE('',*,*,#15488,.F.);
#21007=ORIENTED_EDGE('',*,*,#15489,.F.);
#21008=ORIENTED_EDGE('',*,*,#15490,.F.);
#21009=ORIENTED_EDGE('',*,*,#15489,.T.);
#21010=ORIENTED_EDGE('',*,*,#15491,.F.);
#21011=ORIENTED_EDGE('',*,*,#15492,.F.);
#21012=ORIENTED_EDGE('',*,*,#15493,.F.);
#21013=ORIENTED_EDGE('',*,*,#15492,.T.);
#21014=ORIENTED_EDGE('',*,*,#15494,.F.);
#21015=ORIENTED_EDGE('',*,*,#15495,.F.);
#21016=ORIENTED_EDGE('',*,*,#15496,.F.);
#21017=ORIENTED_EDGE('',*,*,#15495,.T.);
#21018=ORIENTED_EDGE('',*,*,#15497,.F.);
#21019=ORIENTED_EDGE('',*,*,#15498,.F.);
#21020=ORIENTED_EDGE('',*,*,#15499,.F.);
#21021=ORIENTED_EDGE('',*,*,#15498,.T.);
#21022=ORIENTED_EDGE('',*,*,#15500,.F.);
#21023=ORIENTED_EDGE('',*,*,#15501,.F.);
#21024=ORIENTED_EDGE('',*,*,#15502,.F.);
#21025=ORIENTED_EDGE('',*,*,#15501,.T.);
#21026=ORIENTED_EDGE('',*,*,#15503,.F.);
#21027=ORIENTED_EDGE('',*,*,#15504,.F.);
#21028=ORIENTED_EDGE('',*,*,#15505,.F.);
#21029=ORIENTED_EDGE('',*,*,#15504,.T.);
#21030=ORIENTED_EDGE('',*,*,#15506,.F.);
#21031=ORIENTED_EDGE('',*,*,#15507,.F.);
#21032=ORIENTED_EDGE('',*,*,#15508,.F.);
#21033=ORIENTED_EDGE('',*,*,#15507,.T.);
#21034=ORIENTED_EDGE('',*,*,#15509,.F.);
#21035=ORIENTED_EDGE('',*,*,#15510,.F.);
#21036=ORIENTED_EDGE('',*,*,#15511,.F.);
#21037=ORIENTED_EDGE('',*,*,#15510,.T.);
#21038=ORIENTED_EDGE('',*,*,#15512,.F.);
#21039=ORIENTED_EDGE('',*,*,#15513,.F.);
#21040=ORIENTED_EDGE('',*,*,#15514,.F.);
#21041=ORIENTED_EDGE('',*,*,#15513,.T.);
#21042=ORIENTED_EDGE('',*,*,#15515,.F.);
#21043=ORIENTED_EDGE('',*,*,#15516,.F.);
#21044=ORIENTED_EDGE('',*,*,#15517,.F.);
#21045=ORIENTED_EDGE('',*,*,#15516,.T.);
#21046=ORIENTED_EDGE('',*,*,#15518,.F.);
#21047=ORIENTED_EDGE('',*,*,#15519,.F.);
#21048=ORIENTED_EDGE('',*,*,#15520,.F.);
#21049=ORIENTED_EDGE('',*,*,#15519,.T.);
#21050=ORIENTED_EDGE('',*,*,#15521,.F.);
#21051=ORIENTED_EDGE('',*,*,#15522,.F.);
#21052=ORIENTED_EDGE('',*,*,#15523,.F.);
#21053=ORIENTED_EDGE('',*,*,#15522,.T.);
#21054=ORIENTED_EDGE('',*,*,#15524,.F.);
#21055=ORIENTED_EDGE('',*,*,#15525,.F.);
#21056=ORIENTED_EDGE('',*,*,#15526,.F.);
#21057=ORIENTED_EDGE('',*,*,#15525,.T.);
#21058=ORIENTED_EDGE('',*,*,#15527,.F.);
#21059=ORIENTED_EDGE('',*,*,#15528,.F.);
#21060=ORIENTED_EDGE('',*,*,#15529,.F.);
#21061=ORIENTED_EDGE('',*,*,#15528,.T.);
#21062=ORIENTED_EDGE('',*,*,#15530,.F.);
#21063=ORIENTED_EDGE('',*,*,#15531,.F.);
#21064=ORIENTED_EDGE('',*,*,#15532,.F.);
#21065=ORIENTED_EDGE('',*,*,#15531,.T.);
#21066=ORIENTED_EDGE('',*,*,#15533,.F.);
#21067=ORIENTED_EDGE('',*,*,#15534,.F.);
#21068=ORIENTED_EDGE('',*,*,#15535,.F.);
#21069=ORIENTED_EDGE('',*,*,#15534,.T.);
#21070=ORIENTED_EDGE('',*,*,#15536,.F.);
#21071=ORIENTED_EDGE('',*,*,#15537,.F.);
#21072=ORIENTED_EDGE('',*,*,#15538,.F.);
#21073=ORIENTED_EDGE('',*,*,#15537,.T.);
#21074=ORIENTED_EDGE('',*,*,#15539,.F.);
#21075=ORIENTED_EDGE('',*,*,#15540,.F.);
#21076=ORIENTED_EDGE('',*,*,#15541,.F.);
#21077=ORIENTED_EDGE('',*,*,#15540,.T.);
#21078=ORIENTED_EDGE('',*,*,#15542,.F.);
#21079=ORIENTED_EDGE('',*,*,#15543,.F.);
#21080=ORIENTED_EDGE('',*,*,#15544,.F.);
#21081=ORIENTED_EDGE('',*,*,#15543,.T.);
#21082=ORIENTED_EDGE('',*,*,#15545,.F.);
#21083=ORIENTED_EDGE('',*,*,#15546,.F.);
#21084=ORIENTED_EDGE('',*,*,#15547,.F.);
#21085=ORIENTED_EDGE('',*,*,#15546,.T.);
#21086=ORIENTED_EDGE('',*,*,#15548,.F.);
#21087=ORIENTED_EDGE('',*,*,#15549,.F.);
#21088=ORIENTED_EDGE('',*,*,#15550,.F.);
#21089=ORIENTED_EDGE('',*,*,#15549,.T.);
#21090=ORIENTED_EDGE('',*,*,#15551,.F.);
#21091=ORIENTED_EDGE('',*,*,#15552,.F.);
#21092=ORIENTED_EDGE('',*,*,#15553,.F.);
#21093=ORIENTED_EDGE('',*,*,#15552,.T.);
#21094=ORIENTED_EDGE('',*,*,#15554,.F.);
#21095=ORIENTED_EDGE('',*,*,#15555,.F.);
#21096=ORIENTED_EDGE('',*,*,#15556,.F.);
#21097=ORIENTED_EDGE('',*,*,#15555,.T.);
#21098=ORIENTED_EDGE('',*,*,#15557,.F.);
#21099=ORIENTED_EDGE('',*,*,#15558,.F.);
#21100=ORIENTED_EDGE('',*,*,#15559,.F.);
#21101=ORIENTED_EDGE('',*,*,#15558,.T.);
#21102=ORIENTED_EDGE('',*,*,#15560,.F.);
#21103=ORIENTED_EDGE('',*,*,#15561,.F.);
#21104=ORIENTED_EDGE('',*,*,#15562,.F.);
#21105=ORIENTED_EDGE('',*,*,#15561,.T.);
#21106=ORIENTED_EDGE('',*,*,#15563,.F.);
#21107=ORIENTED_EDGE('',*,*,#15564,.F.);
#21108=ORIENTED_EDGE('',*,*,#15565,.F.);
#21109=ORIENTED_EDGE('',*,*,#15564,.T.);
#21110=ORIENTED_EDGE('',*,*,#15566,.F.);
#21111=ORIENTED_EDGE('',*,*,#15567,.F.);
#21112=ORIENTED_EDGE('',*,*,#15568,.F.);
#21113=ORIENTED_EDGE('',*,*,#15567,.T.);
#21114=ORIENTED_EDGE('',*,*,#15569,.F.);
#21115=ORIENTED_EDGE('',*,*,#15570,.F.);
#21116=ORIENTED_EDGE('',*,*,#15571,.F.);
#21117=ORIENTED_EDGE('',*,*,#15570,.T.);
#21118=ORIENTED_EDGE('',*,*,#15572,.F.);
#21119=ORIENTED_EDGE('',*,*,#15573,.F.);
#21120=ORIENTED_EDGE('',*,*,#15574,.F.);
#21121=ORIENTED_EDGE('',*,*,#15573,.T.);
#21122=ORIENTED_EDGE('',*,*,#15575,.F.);
#21123=ORIENTED_EDGE('',*,*,#15576,.F.);
#21124=ORIENTED_EDGE('',*,*,#15577,.F.);
#21125=ORIENTED_EDGE('',*,*,#15576,.T.);
#21126=ORIENTED_EDGE('',*,*,#15578,.F.);
#21127=ORIENTED_EDGE('',*,*,#15579,.F.);
#21128=ORIENTED_EDGE('',*,*,#15580,.F.);
#21129=ORIENTED_EDGE('',*,*,#15579,.T.);
#21130=ORIENTED_EDGE('',*,*,#15581,.F.);
#21131=ORIENTED_EDGE('',*,*,#15582,.F.);
#21132=ORIENTED_EDGE('',*,*,#15583,.F.);
#21133=ORIENTED_EDGE('',*,*,#15582,.T.);
#21134=ORIENTED_EDGE('',*,*,#15584,.F.);
#21135=ORIENTED_EDGE('',*,*,#15585,.F.);
#21136=ORIENTED_EDGE('',*,*,#15586,.F.);
#21137=ORIENTED_EDGE('',*,*,#15585,.T.);
#21138=ORIENTED_EDGE('',*,*,#15587,.F.);
#21139=ORIENTED_EDGE('',*,*,#15588,.F.);
#21140=ORIENTED_EDGE('',*,*,#15589,.F.);
#21141=ORIENTED_EDGE('',*,*,#15588,.T.);
#21142=ORIENTED_EDGE('',*,*,#15590,.F.);
#21143=ORIENTED_EDGE('',*,*,#15591,.F.);
#21144=ORIENTED_EDGE('',*,*,#15592,.F.);
#21145=ORIENTED_EDGE('',*,*,#15591,.T.);
#21146=ORIENTED_EDGE('',*,*,#15593,.F.);
#21147=ORIENTED_EDGE('',*,*,#15594,.F.);
#21148=ORIENTED_EDGE('',*,*,#15595,.F.);
#21149=ORIENTED_EDGE('',*,*,#15594,.T.);
#21150=ORIENTED_EDGE('',*,*,#15596,.F.);
#21151=ORIENTED_EDGE('',*,*,#15597,.F.);
#21152=ORIENTED_EDGE('',*,*,#15598,.F.);
#21153=ORIENTED_EDGE('',*,*,#15597,.T.);
#21154=ORIENTED_EDGE('',*,*,#15599,.F.);
#21155=ORIENTED_EDGE('',*,*,#15600,.F.);
#21156=ORIENTED_EDGE('',*,*,#15601,.F.);
#21157=ORIENTED_EDGE('',*,*,#15600,.T.);
#21158=ORIENTED_EDGE('',*,*,#15602,.F.);
#21159=ORIENTED_EDGE('',*,*,#15603,.F.);
#21160=ORIENTED_EDGE('',*,*,#15604,.F.);
#21161=ORIENTED_EDGE('',*,*,#15603,.T.);
#21162=ORIENTED_EDGE('',*,*,#15605,.F.);
#21163=ORIENTED_EDGE('',*,*,#15606,.F.);
#21164=ORIENTED_EDGE('',*,*,#15607,.F.);
#21165=ORIENTED_EDGE('',*,*,#15606,.T.);
#21166=ORIENTED_EDGE('',*,*,#15608,.F.);
#21167=ORIENTED_EDGE('',*,*,#15609,.F.);
#21168=ORIENTED_EDGE('',*,*,#15610,.F.);
#21169=ORIENTED_EDGE('',*,*,#15609,.T.);
#21170=ORIENTED_EDGE('',*,*,#15611,.F.);
#21171=ORIENTED_EDGE('',*,*,#15612,.F.);
#21172=ORIENTED_EDGE('',*,*,#15613,.F.);
#21173=ORIENTED_EDGE('',*,*,#15612,.T.);
#21174=ORIENTED_EDGE('',*,*,#15614,.F.);
#21175=ORIENTED_EDGE('',*,*,#15615,.F.);
#21176=ORIENTED_EDGE('',*,*,#15616,.F.);
#21177=ORIENTED_EDGE('',*,*,#15615,.T.);
#21178=ORIENTED_EDGE('',*,*,#15617,.F.);
#21179=ORIENTED_EDGE('',*,*,#15618,.F.);
#21180=ORIENTED_EDGE('',*,*,#15619,.F.);
#21181=ORIENTED_EDGE('',*,*,#15618,.T.);
#21182=ORIENTED_EDGE('',*,*,#15620,.F.);
#21183=ORIENTED_EDGE('',*,*,#15621,.F.);
#21184=ORIENTED_EDGE('',*,*,#15622,.F.);
#21185=ORIENTED_EDGE('',*,*,#15621,.T.);
#21186=ORIENTED_EDGE('',*,*,#15623,.F.);
#21187=ORIENTED_EDGE('',*,*,#15624,.F.);
#21188=ORIENTED_EDGE('',*,*,#15625,.F.);
#21189=ORIENTED_EDGE('',*,*,#15624,.T.);
#21190=ORIENTED_EDGE('',*,*,#15626,.F.);
#21191=ORIENTED_EDGE('',*,*,#15627,.F.);
#21192=ORIENTED_EDGE('',*,*,#15628,.F.);
#21193=ORIENTED_EDGE('',*,*,#15627,.T.);
#21194=ORIENTED_EDGE('',*,*,#15629,.F.);
#21195=ORIENTED_EDGE('',*,*,#15630,.F.);
#21196=ORIENTED_EDGE('',*,*,#15631,.F.);
#21197=ORIENTED_EDGE('',*,*,#15630,.T.);
#21198=ORIENTED_EDGE('',*,*,#15632,.F.);
#21199=ORIENTED_EDGE('',*,*,#15633,.F.);
#21200=ORIENTED_EDGE('',*,*,#15634,.F.);
#21201=ORIENTED_EDGE('',*,*,#15633,.T.);
#21202=ORIENTED_EDGE('',*,*,#15635,.F.);
#21203=ORIENTED_EDGE('',*,*,#15636,.F.);
#21204=ORIENTED_EDGE('',*,*,#15637,.F.);
#21205=ORIENTED_EDGE('',*,*,#15636,.T.);
#21206=ORIENTED_EDGE('',*,*,#15638,.F.);
#21207=ORIENTED_EDGE('',*,*,#15639,.F.);
#21208=ORIENTED_EDGE('',*,*,#15640,.F.);
#21209=ORIENTED_EDGE('',*,*,#15639,.T.);
#21210=ORIENTED_EDGE('',*,*,#15641,.F.);
#21211=ORIENTED_EDGE('',*,*,#15642,.F.);
#21212=ORIENTED_EDGE('',*,*,#15643,.F.);
#21213=ORIENTED_EDGE('',*,*,#15642,.T.);
#21214=ORIENTED_EDGE('',*,*,#15644,.F.);
#21215=ORIENTED_EDGE('',*,*,#15645,.F.);
#21216=ORIENTED_EDGE('',*,*,#15646,.F.);
#21217=ORIENTED_EDGE('',*,*,#15645,.T.);
#21218=ORIENTED_EDGE('',*,*,#15647,.F.);
#21219=ORIENTED_EDGE('',*,*,#15648,.F.);
#21220=ORIENTED_EDGE('',*,*,#15649,.F.);
#21221=ORIENTED_EDGE('',*,*,#15648,.T.);
#21222=ORIENTED_EDGE('',*,*,#15650,.F.);
#21223=ORIENTED_EDGE('',*,*,#15651,.F.);
#21224=ORIENTED_EDGE('',*,*,#15652,.F.);
#21225=ORIENTED_EDGE('',*,*,#15651,.T.);
#21226=ORIENTED_EDGE('',*,*,#15653,.F.);
#21227=ORIENTED_EDGE('',*,*,#15654,.F.);
#21228=ORIENTED_EDGE('',*,*,#15655,.F.);
#21229=ORIENTED_EDGE('',*,*,#15654,.T.);
#21230=ORIENTED_EDGE('',*,*,#15656,.F.);
#21231=ORIENTED_EDGE('',*,*,#15657,.F.);
#21232=ORIENTED_EDGE('',*,*,#15658,.F.);
#21233=ORIENTED_EDGE('',*,*,#15657,.T.);
#21234=ORIENTED_EDGE('',*,*,#15659,.F.);
#21235=ORIENTED_EDGE('',*,*,#15660,.F.);
#21236=ORIENTED_EDGE('',*,*,#15661,.F.);
#21237=ORIENTED_EDGE('',*,*,#15660,.T.);
#21238=ORIENTED_EDGE('',*,*,#15662,.F.);
#21239=ORIENTED_EDGE('',*,*,#15663,.F.);
#21240=ORIENTED_EDGE('',*,*,#15664,.F.);
#21241=ORIENTED_EDGE('',*,*,#15663,.T.);
#21242=ORIENTED_EDGE('',*,*,#15665,.F.);
#21243=ORIENTED_EDGE('',*,*,#15666,.F.);
#21244=ORIENTED_EDGE('',*,*,#15667,.F.);
#21245=ORIENTED_EDGE('',*,*,#15666,.T.);
#21246=ORIENTED_EDGE('',*,*,#15668,.F.);
#21247=ORIENTED_EDGE('',*,*,#15669,.F.);
#21248=ORIENTED_EDGE('',*,*,#15670,.F.);
#21249=ORIENTED_EDGE('',*,*,#15669,.T.);
#21250=ORIENTED_EDGE('',*,*,#15671,.F.);
#21251=ORIENTED_EDGE('',*,*,#15672,.F.);
#21252=ORIENTED_EDGE('',*,*,#15673,.F.);
#21253=ORIENTED_EDGE('',*,*,#15672,.T.);
#21254=ORIENTED_EDGE('',*,*,#15674,.F.);
#21255=ORIENTED_EDGE('',*,*,#15675,.F.);
#21256=ORIENTED_EDGE('',*,*,#15676,.F.);
#21257=ORIENTED_EDGE('',*,*,#15675,.T.);
#21258=ORIENTED_EDGE('',*,*,#15677,.F.);
#21259=ORIENTED_EDGE('',*,*,#15678,.F.);
#21260=ORIENTED_EDGE('',*,*,#15679,.F.);
#21261=ORIENTED_EDGE('',*,*,#15678,.T.);
#21262=ORIENTED_EDGE('',*,*,#15680,.F.);
#21263=ORIENTED_EDGE('',*,*,#15681,.F.);
#21264=ORIENTED_EDGE('',*,*,#15682,.F.);
#21265=ORIENTED_EDGE('',*,*,#15681,.T.);
#21266=ORIENTED_EDGE('',*,*,#15683,.F.);
#21267=ORIENTED_EDGE('',*,*,#15684,.F.);
#21268=ORIENTED_EDGE('',*,*,#15685,.F.);
#21269=ORIENTED_EDGE('',*,*,#15684,.T.);
#21270=ORIENTED_EDGE('',*,*,#15686,.F.);
#21271=ORIENTED_EDGE('',*,*,#15687,.F.);
#21272=ORIENTED_EDGE('',*,*,#15688,.F.);
#21273=ORIENTED_EDGE('',*,*,#15687,.T.);
#21274=ORIENTED_EDGE('',*,*,#15689,.F.);
#21275=ORIENTED_EDGE('',*,*,#15690,.F.);
#21276=ORIENTED_EDGE('',*,*,#15691,.F.);
#21277=ORIENTED_EDGE('',*,*,#15690,.T.);
#21278=ORIENTED_EDGE('',*,*,#15692,.F.);
#21279=ORIENTED_EDGE('',*,*,#15693,.F.);
#21280=ORIENTED_EDGE('',*,*,#15694,.F.);
#21281=ORIENTED_EDGE('',*,*,#15693,.T.);
#21282=ORIENTED_EDGE('',*,*,#15695,.F.);
#21283=ORIENTED_EDGE('',*,*,#15696,.F.);
#21284=ORIENTED_EDGE('',*,*,#15697,.F.);
#21285=ORIENTED_EDGE('',*,*,#15696,.T.);
#21286=ORIENTED_EDGE('',*,*,#15698,.F.);
#21287=ORIENTED_EDGE('',*,*,#15699,.F.);
#21288=ORIENTED_EDGE('',*,*,#15700,.F.);
#21289=ORIENTED_EDGE('',*,*,#15699,.T.);
#21290=ORIENTED_EDGE('',*,*,#15701,.F.);
#21291=ORIENTED_EDGE('',*,*,#15702,.F.);
#21292=ORIENTED_EDGE('',*,*,#15703,.F.);
#21293=ORIENTED_EDGE('',*,*,#15702,.T.);
#21294=ORIENTED_EDGE('',*,*,#15704,.F.);
#21295=ORIENTED_EDGE('',*,*,#15705,.F.);
#21296=ORIENTED_EDGE('',*,*,#15706,.F.);
#21297=ORIENTED_EDGE('',*,*,#15705,.T.);
#21298=ORIENTED_EDGE('',*,*,#15707,.F.);
#21299=ORIENTED_EDGE('',*,*,#15708,.F.);
#21300=ORIENTED_EDGE('',*,*,#15709,.F.);
#21301=ORIENTED_EDGE('',*,*,#15708,.T.);
#21302=ORIENTED_EDGE('',*,*,#15710,.F.);
#21303=ORIENTED_EDGE('',*,*,#15711,.F.);
#21304=ORIENTED_EDGE('',*,*,#15712,.F.);
#21305=ORIENTED_EDGE('',*,*,#15711,.T.);
#21306=ORIENTED_EDGE('',*,*,#15713,.F.);
#21307=ORIENTED_EDGE('',*,*,#15714,.F.);
#21308=ORIENTED_EDGE('',*,*,#15715,.F.);
#21309=ORIENTED_EDGE('',*,*,#15714,.T.);
#21310=ORIENTED_EDGE('',*,*,#15716,.F.);
#21311=ORIENTED_EDGE('',*,*,#15717,.F.);
#21312=ORIENTED_EDGE('',*,*,#15718,.F.);
#21313=ORIENTED_EDGE('',*,*,#15717,.T.);
#21314=ORIENTED_EDGE('',*,*,#15719,.F.);
#21315=ORIENTED_EDGE('',*,*,#15720,.F.);
#21316=ORIENTED_EDGE('',*,*,#15721,.F.);
#21317=ORIENTED_EDGE('',*,*,#15720,.T.);
#21318=ORIENTED_EDGE('',*,*,#15722,.F.);
#21319=ORIENTED_EDGE('',*,*,#15723,.F.);
#21320=ORIENTED_EDGE('',*,*,#15724,.F.);
#21321=ORIENTED_EDGE('',*,*,#15723,.T.);
#21322=ORIENTED_EDGE('',*,*,#15725,.F.);
#21323=ORIENTED_EDGE('',*,*,#15726,.F.);
#21324=ORIENTED_EDGE('',*,*,#15727,.F.);
#21325=ORIENTED_EDGE('',*,*,#15726,.T.);
#21326=ORIENTED_EDGE('',*,*,#15728,.F.);
#21327=ORIENTED_EDGE('',*,*,#15729,.F.);
#21328=ORIENTED_EDGE('',*,*,#15730,.F.);
#21329=ORIENTED_EDGE('',*,*,#15729,.T.);
#21330=ORIENTED_EDGE('',*,*,#15731,.F.);
#21331=ORIENTED_EDGE('',*,*,#15732,.F.);
#21332=ORIENTED_EDGE('',*,*,#15733,.F.);
#21333=ORIENTED_EDGE('',*,*,#15732,.T.);
#21334=ORIENTED_EDGE('',*,*,#15734,.F.);
#21335=ORIENTED_EDGE('',*,*,#15735,.F.);
#21336=ORIENTED_EDGE('',*,*,#15736,.F.);
#21337=ORIENTED_EDGE('',*,*,#15735,.T.);
#21338=ORIENTED_EDGE('',*,*,#15737,.F.);
#21339=ORIENTED_EDGE('',*,*,#15738,.F.);
#21340=ORIENTED_EDGE('',*,*,#15739,.F.);
#21341=ORIENTED_EDGE('',*,*,#15738,.T.);
#21342=ORIENTED_EDGE('',*,*,#15740,.F.);
#21343=ORIENTED_EDGE('',*,*,#15741,.F.);
#21344=ORIENTED_EDGE('',*,*,#15742,.F.);
#21345=ORIENTED_EDGE('',*,*,#15741,.T.);
#21346=ORIENTED_EDGE('',*,*,#15743,.F.);
#21347=ORIENTED_EDGE('',*,*,#15744,.F.);
#21348=ORIENTED_EDGE('',*,*,#15745,.F.);
#21349=ORIENTED_EDGE('',*,*,#15744,.T.);
#21350=ORIENTED_EDGE('',*,*,#15746,.F.);
#21351=ORIENTED_EDGE('',*,*,#15747,.F.);
#21352=ORIENTED_EDGE('',*,*,#15748,.F.);
#21353=ORIENTED_EDGE('',*,*,#15747,.T.);
#21354=ORIENTED_EDGE('',*,*,#15749,.F.);
#21355=ORIENTED_EDGE('',*,*,#15750,.F.);
#21356=ORIENTED_EDGE('',*,*,#15751,.F.);
#21357=ORIENTED_EDGE('',*,*,#15750,.T.);
#21358=ORIENTED_EDGE('',*,*,#15752,.F.);
#21359=ORIENTED_EDGE('',*,*,#15753,.F.);
#21360=ORIENTED_EDGE('',*,*,#15754,.F.);
#21361=ORIENTED_EDGE('',*,*,#15753,.T.);
#21362=ORIENTED_EDGE('',*,*,#15755,.F.);
#21363=ORIENTED_EDGE('',*,*,#15756,.F.);
#21364=ORIENTED_EDGE('',*,*,#15757,.F.);
#21365=ORIENTED_EDGE('',*,*,#15756,.T.);
#21366=ORIENTED_EDGE('',*,*,#15758,.F.);
#21367=ORIENTED_EDGE('',*,*,#15759,.F.);
#21368=ORIENTED_EDGE('',*,*,#15760,.F.);
#21369=ORIENTED_EDGE('',*,*,#15759,.T.);
#21370=ORIENTED_EDGE('',*,*,#15761,.F.);
#21371=ORIENTED_EDGE('',*,*,#15762,.F.);
#21372=ORIENTED_EDGE('',*,*,#15763,.F.);
#21373=ORIENTED_EDGE('',*,*,#15762,.T.);
#21374=ORIENTED_EDGE('',*,*,#15764,.F.);
#21375=ORIENTED_EDGE('',*,*,#15765,.F.);
#21376=ORIENTED_EDGE('',*,*,#15766,.F.);
#21377=ORIENTED_EDGE('',*,*,#15765,.T.);
#21378=ORIENTED_EDGE('',*,*,#15767,.F.);
#21379=ORIENTED_EDGE('',*,*,#15768,.F.);
#21380=ORIENTED_EDGE('',*,*,#15769,.F.);
#21381=ORIENTED_EDGE('',*,*,#15768,.T.);
#21382=ORIENTED_EDGE('',*,*,#15770,.F.);
#21383=ORIENTED_EDGE('',*,*,#15771,.F.);
#21384=ORIENTED_EDGE('',*,*,#15772,.F.);
#21385=ORIENTED_EDGE('',*,*,#15771,.T.);
#21386=ORIENTED_EDGE('',*,*,#15773,.F.);
#21387=ORIENTED_EDGE('',*,*,#15774,.F.);
#21388=ORIENTED_EDGE('',*,*,#15775,.F.);
#21389=ORIENTED_EDGE('',*,*,#15774,.T.);
#21390=ORIENTED_EDGE('',*,*,#15776,.F.);
#21391=ORIENTED_EDGE('',*,*,#15777,.F.);
#21392=ORIENTED_EDGE('',*,*,#15778,.F.);
#21393=ORIENTED_EDGE('',*,*,#15777,.T.);
#21394=ORIENTED_EDGE('',*,*,#15779,.F.);
#21395=ORIENTED_EDGE('',*,*,#15780,.F.);
#21396=ORIENTED_EDGE('',*,*,#15781,.F.);
#21397=ORIENTED_EDGE('',*,*,#15780,.T.);
#21398=ORIENTED_EDGE('',*,*,#15782,.F.);
#21399=ORIENTED_EDGE('',*,*,#15783,.F.);
#21400=ORIENTED_EDGE('',*,*,#15784,.F.);
#21401=ORIENTED_EDGE('',*,*,#15783,.T.);
#21402=ORIENTED_EDGE('',*,*,#15785,.F.);
#21403=ORIENTED_EDGE('',*,*,#15786,.F.);
#21404=ORIENTED_EDGE('',*,*,#15787,.F.);
#21405=ORIENTED_EDGE('',*,*,#15786,.T.);
#21406=ORIENTED_EDGE('',*,*,#15788,.F.);
#21407=ORIENTED_EDGE('',*,*,#15789,.F.);
#21408=ORIENTED_EDGE('',*,*,#15790,.F.);
#21409=ORIENTED_EDGE('',*,*,#15789,.T.);
#21410=ORIENTED_EDGE('',*,*,#15791,.F.);
#21411=ORIENTED_EDGE('',*,*,#15792,.F.);
#21412=ORIENTED_EDGE('',*,*,#15793,.F.);
#21413=ORIENTED_EDGE('',*,*,#15792,.T.);
#21414=ORIENTED_EDGE('',*,*,#15794,.F.);
#21415=ORIENTED_EDGE('',*,*,#15795,.F.);
#21416=ORIENTED_EDGE('',*,*,#15796,.F.);
#21417=ORIENTED_EDGE('',*,*,#15795,.T.);
#21418=ORIENTED_EDGE('',*,*,#15797,.F.);
#21419=ORIENTED_EDGE('',*,*,#15798,.F.);
#21420=ORIENTED_EDGE('',*,*,#15799,.F.);
#21421=ORIENTED_EDGE('',*,*,#15798,.T.);
#21422=ORIENTED_EDGE('',*,*,#15800,.F.);
#21423=ORIENTED_EDGE('',*,*,#15801,.F.);
#21424=ORIENTED_EDGE('',*,*,#15802,.F.);
#21425=ORIENTED_EDGE('',*,*,#15801,.T.);
#21426=ORIENTED_EDGE('',*,*,#15803,.F.);
#21427=ORIENTED_EDGE('',*,*,#15804,.F.);
#21428=ORIENTED_EDGE('',*,*,#15805,.F.);
#21429=ORIENTED_EDGE('',*,*,#15804,.T.);
#21430=ORIENTED_EDGE('',*,*,#15806,.F.);
#21431=ORIENTED_EDGE('',*,*,#15807,.F.);
#21432=ORIENTED_EDGE('',*,*,#15808,.F.);
#21433=ORIENTED_EDGE('',*,*,#15807,.T.);
#21434=ORIENTED_EDGE('',*,*,#15809,.F.);
#21435=ORIENTED_EDGE('',*,*,#15810,.F.);
#21436=ORIENTED_EDGE('',*,*,#15811,.F.);
#21437=ORIENTED_EDGE('',*,*,#15810,.T.);
#21438=ORIENTED_EDGE('',*,*,#15812,.F.);
#21439=ORIENTED_EDGE('',*,*,#15813,.F.);
#21440=ORIENTED_EDGE('',*,*,#15814,.F.);
#21441=ORIENTED_EDGE('',*,*,#15813,.T.);
#21442=ORIENTED_EDGE('',*,*,#15815,.F.);
#21443=ORIENTED_EDGE('',*,*,#15816,.F.);
#21444=ORIENTED_EDGE('',*,*,#15817,.F.);
#21445=ORIENTED_EDGE('',*,*,#15816,.T.);
#21446=ORIENTED_EDGE('',*,*,#15818,.F.);
#21447=ORIENTED_EDGE('',*,*,#15819,.F.);
#21448=ORIENTED_EDGE('',*,*,#15820,.F.);
#21449=ORIENTED_EDGE('',*,*,#15819,.T.);
#21450=ORIENTED_EDGE('',*,*,#15821,.F.);
#21451=ORIENTED_EDGE('',*,*,#15822,.F.);
#21452=ORIENTED_EDGE('',*,*,#15823,.F.);
#21453=ORIENTED_EDGE('',*,*,#15822,.T.);
#21454=ORIENTED_EDGE('',*,*,#15824,.F.);
#21455=ORIENTED_EDGE('',*,*,#15825,.F.);
#21456=ORIENTED_EDGE('',*,*,#15826,.F.);
#21457=ORIENTED_EDGE('',*,*,#15825,.T.);
#21458=ORIENTED_EDGE('',*,*,#15827,.F.);
#21459=ORIENTED_EDGE('',*,*,#15828,.F.);
#21460=ORIENTED_EDGE('',*,*,#15829,.F.);
#21461=ORIENTED_EDGE('',*,*,#15828,.T.);
#21462=ORIENTED_EDGE('',*,*,#15830,.F.);
#21463=ORIENTED_EDGE('',*,*,#15831,.F.);
#21464=ORIENTED_EDGE('',*,*,#15832,.F.);
#21465=ORIENTED_EDGE('',*,*,#15831,.T.);
#21466=ORIENTED_EDGE('',*,*,#15833,.F.);
#21467=ORIENTED_EDGE('',*,*,#15834,.F.);
#21468=ORIENTED_EDGE('',*,*,#15835,.F.);
#21469=ORIENTED_EDGE('',*,*,#15834,.T.);
#21470=ORIENTED_EDGE('',*,*,#15836,.F.);
#21471=ORIENTED_EDGE('',*,*,#15837,.F.);
#21472=ORIENTED_EDGE('',*,*,#15838,.F.);
#21473=ORIENTED_EDGE('',*,*,#15837,.T.);
#21474=ORIENTED_EDGE('',*,*,#15839,.F.);
#21475=ORIENTED_EDGE('',*,*,#15840,.F.);
#21476=ORIENTED_EDGE('',*,*,#15841,.F.);
#21477=ORIENTED_EDGE('',*,*,#15840,.T.);
#21478=ORIENTED_EDGE('',*,*,#15842,.F.);
#21479=ORIENTED_EDGE('',*,*,#15843,.F.);
#21480=ORIENTED_EDGE('',*,*,#15844,.F.);
#21481=ORIENTED_EDGE('',*,*,#15843,.T.);
#21482=ORIENTED_EDGE('',*,*,#15845,.F.);
#21483=ORIENTED_EDGE('',*,*,#15846,.F.);
#21484=ORIENTED_EDGE('',*,*,#15847,.F.);
#21485=ORIENTED_EDGE('',*,*,#15846,.T.);
#21486=ORIENTED_EDGE('',*,*,#15848,.F.);
#21487=ORIENTED_EDGE('',*,*,#15849,.F.);
#21488=ORIENTED_EDGE('',*,*,#15850,.F.);
#21489=ORIENTED_EDGE('',*,*,#15849,.T.);
#21490=ORIENTED_EDGE('',*,*,#15851,.F.);
#21491=ORIENTED_EDGE('',*,*,#15852,.F.);
#21492=ORIENTED_EDGE('',*,*,#15853,.F.);
#21493=ORIENTED_EDGE('',*,*,#15852,.T.);
#21494=ORIENTED_EDGE('',*,*,#15854,.F.);
#21495=ORIENTED_EDGE('',*,*,#15855,.F.);
#21496=ORIENTED_EDGE('',*,*,#15856,.F.);
#21497=ORIENTED_EDGE('',*,*,#15855,.T.);
#21498=ORIENTED_EDGE('',*,*,#15857,.F.);
#21499=ORIENTED_EDGE('',*,*,#15858,.F.);
#21500=ORIENTED_EDGE('',*,*,#15859,.F.);
#21501=ORIENTED_EDGE('',*,*,#15858,.T.);
#21502=ORIENTED_EDGE('',*,*,#15860,.F.);
#21503=ORIENTED_EDGE('',*,*,#15861,.F.);
#21504=ORIENTED_EDGE('',*,*,#15862,.F.);
#21505=ORIENTED_EDGE('',*,*,#15861,.T.);
#21506=ORIENTED_EDGE('',*,*,#15863,.F.);
#21507=ORIENTED_EDGE('',*,*,#15864,.F.);
#21508=ORIENTED_EDGE('',*,*,#15865,.F.);
#21509=ORIENTED_EDGE('',*,*,#15864,.T.);
#21510=ORIENTED_EDGE('',*,*,#15866,.F.);
#21511=ORIENTED_EDGE('',*,*,#15867,.F.);
#21512=ORIENTED_EDGE('',*,*,#15868,.F.);
#21513=ORIENTED_EDGE('',*,*,#15867,.T.);
#21514=ORIENTED_EDGE('',*,*,#15869,.F.);
#21515=ORIENTED_EDGE('',*,*,#15870,.F.);
#21516=ORIENTED_EDGE('',*,*,#15871,.F.);
#21517=ORIENTED_EDGE('',*,*,#15870,.T.);
#21518=ORIENTED_EDGE('',*,*,#15872,.F.);
#21519=ORIENTED_EDGE('',*,*,#15873,.F.);
#21520=ORIENTED_EDGE('',*,*,#15874,.F.);
#21521=ORIENTED_EDGE('',*,*,#15873,.T.);
#21522=ORIENTED_EDGE('',*,*,#15875,.F.);
#21523=ORIENTED_EDGE('',*,*,#15876,.F.);
#21524=ORIENTED_EDGE('',*,*,#15877,.F.);
#21525=ORIENTED_EDGE('',*,*,#15876,.T.);
#21526=ORIENTED_EDGE('',*,*,#15878,.F.);
#21527=ORIENTED_EDGE('',*,*,#15879,.F.);
#21528=ORIENTED_EDGE('',*,*,#15880,.F.);
#21529=ORIENTED_EDGE('',*,*,#15879,.T.);
#21530=ORIENTED_EDGE('',*,*,#15881,.F.);
#21531=ORIENTED_EDGE('',*,*,#15882,.F.);
#21532=ORIENTED_EDGE('',*,*,#15883,.F.);
#21533=ORIENTED_EDGE('',*,*,#15882,.T.);
#21534=ORIENTED_EDGE('',*,*,#15884,.F.);
#21535=ORIENTED_EDGE('',*,*,#15885,.F.);
#21536=ORIENTED_EDGE('',*,*,#15886,.F.);
#21537=ORIENTED_EDGE('',*,*,#15885,.T.);
#21538=ORIENTED_EDGE('',*,*,#15887,.F.);
#21539=ORIENTED_EDGE('',*,*,#15888,.F.);
#21540=ORIENTED_EDGE('',*,*,#15889,.F.);
#21541=ORIENTED_EDGE('',*,*,#15888,.T.);
#21542=ORIENTED_EDGE('',*,*,#15890,.F.);
#21543=ORIENTED_EDGE('',*,*,#15891,.F.);
#21544=ORIENTED_EDGE('',*,*,#15892,.F.);
#21545=ORIENTED_EDGE('',*,*,#15891,.T.);
#21546=ORIENTED_EDGE('',*,*,#15893,.F.);
#21547=ORIENTED_EDGE('',*,*,#15894,.F.);
#21548=ORIENTED_EDGE('',*,*,#15895,.F.);
#21549=ORIENTED_EDGE('',*,*,#15894,.T.);
#21550=ORIENTED_EDGE('',*,*,#15896,.F.);
#21551=ORIENTED_EDGE('',*,*,#15897,.F.);
#21552=ORIENTED_EDGE('',*,*,#15898,.F.);
#21553=ORIENTED_EDGE('',*,*,#15897,.T.);
#21554=ORIENTED_EDGE('',*,*,#15899,.F.);
#21555=ORIENTED_EDGE('',*,*,#15900,.F.);
#21556=ORIENTED_EDGE('',*,*,#15901,.F.);
#21557=ORIENTED_EDGE('',*,*,#15900,.T.);
#21558=ORIENTED_EDGE('',*,*,#15902,.F.);
#21559=ORIENTED_EDGE('',*,*,#15903,.F.);
#21560=ORIENTED_EDGE('',*,*,#15904,.F.);
#21561=ORIENTED_EDGE('',*,*,#15903,.T.);
#21562=ORIENTED_EDGE('',*,*,#15905,.F.);
#21563=ORIENTED_EDGE('',*,*,#15906,.F.);
#21564=ORIENTED_EDGE('',*,*,#15907,.F.);
#21565=ORIENTED_EDGE('',*,*,#15906,.T.);
#21566=ORIENTED_EDGE('',*,*,#15908,.F.);
#21567=ORIENTED_EDGE('',*,*,#15909,.F.);
#21568=ORIENTED_EDGE('',*,*,#15910,.F.);
#21569=ORIENTED_EDGE('',*,*,#15909,.T.);
#21570=ORIENTED_EDGE('',*,*,#15911,.F.);
#21571=ORIENTED_EDGE('',*,*,#15912,.F.);
#21572=ORIENTED_EDGE('',*,*,#15913,.F.);
#21573=ORIENTED_EDGE('',*,*,#15912,.T.);
#21574=ORIENTED_EDGE('',*,*,#15914,.F.);
#21575=ORIENTED_EDGE('',*,*,#15915,.F.);
#21576=ORIENTED_EDGE('',*,*,#15916,.F.);
#21577=ORIENTED_EDGE('',*,*,#15915,.T.);
#21578=ORIENTED_EDGE('',*,*,#15917,.F.);
#21579=ORIENTED_EDGE('',*,*,#15918,.F.);
#21580=ORIENTED_EDGE('',*,*,#15919,.F.);
#21581=ORIENTED_EDGE('',*,*,#15918,.T.);
#21582=ORIENTED_EDGE('',*,*,#15920,.F.);
#21583=ORIENTED_EDGE('',*,*,#15921,.F.);
#21584=ORIENTED_EDGE('',*,*,#15922,.F.);
#21585=ORIENTED_EDGE('',*,*,#15921,.T.);
#21586=ORIENTED_EDGE('',*,*,#15923,.F.);
#21587=ORIENTED_EDGE('',*,*,#15924,.F.);
#21588=ORIENTED_EDGE('',*,*,#15925,.F.);
#21589=ORIENTED_EDGE('',*,*,#15924,.T.);
#21590=ORIENTED_EDGE('',*,*,#15926,.F.);
#21591=ORIENTED_EDGE('',*,*,#15927,.F.);
#21592=ORIENTED_EDGE('',*,*,#15928,.F.);
#21593=ORIENTED_EDGE('',*,*,#15927,.T.);
#21594=ORIENTED_EDGE('',*,*,#15929,.F.);
#21595=ORIENTED_EDGE('',*,*,#15930,.F.);
#21596=ORIENTED_EDGE('',*,*,#15931,.F.);
#21597=ORIENTED_EDGE('',*,*,#15930,.T.);
#21598=ORIENTED_EDGE('',*,*,#15932,.F.);
#21599=ORIENTED_EDGE('',*,*,#15933,.F.);
#21600=ORIENTED_EDGE('',*,*,#15934,.F.);
#21601=ORIENTED_EDGE('',*,*,#15933,.T.);
#21602=ORIENTED_EDGE('',*,*,#15935,.F.);
#21603=ORIENTED_EDGE('',*,*,#15936,.F.);
#21604=ORIENTED_EDGE('',*,*,#15937,.F.);
#21605=ORIENTED_EDGE('',*,*,#15936,.T.);
#21606=ORIENTED_EDGE('',*,*,#15938,.F.);
#21607=ORIENTED_EDGE('',*,*,#15939,.F.);
#21608=ORIENTED_EDGE('',*,*,#15940,.F.);
#21609=ORIENTED_EDGE('',*,*,#15939,.T.);
#21610=ORIENTED_EDGE('',*,*,#15941,.F.);
#21611=ORIENTED_EDGE('',*,*,#15942,.F.);
#21612=ORIENTED_EDGE('',*,*,#15943,.F.);
#21613=ORIENTED_EDGE('',*,*,#15942,.T.);
#21614=ORIENTED_EDGE('',*,*,#15944,.F.);
#21615=ORIENTED_EDGE('',*,*,#15945,.F.);
#21616=ORIENTED_EDGE('',*,*,#15946,.F.);
#21617=ORIENTED_EDGE('',*,*,#15945,.T.);
#21618=ORIENTED_EDGE('',*,*,#15947,.F.);
#21619=ORIENTED_EDGE('',*,*,#15948,.F.);
#21620=ORIENTED_EDGE('',*,*,#15949,.F.);
#21621=ORIENTED_EDGE('',*,*,#15948,.T.);
#21622=ORIENTED_EDGE('',*,*,#15950,.F.);
#21623=ORIENTED_EDGE('',*,*,#15951,.F.);
#21624=ORIENTED_EDGE('',*,*,#15952,.F.);
#21625=ORIENTED_EDGE('',*,*,#15951,.T.);
#21626=ORIENTED_EDGE('',*,*,#15953,.F.);
#21627=ORIENTED_EDGE('',*,*,#15954,.F.);
#21628=ORIENTED_EDGE('',*,*,#15955,.F.);
#21629=ORIENTED_EDGE('',*,*,#15954,.T.);
#21630=ORIENTED_EDGE('',*,*,#15956,.F.);
#21631=ORIENTED_EDGE('',*,*,#15957,.F.);
#21632=ORIENTED_EDGE('',*,*,#15958,.F.);
#21633=ORIENTED_EDGE('',*,*,#15957,.T.);
#21634=ORIENTED_EDGE('',*,*,#15959,.F.);
#21635=ORIENTED_EDGE('',*,*,#15960,.F.);
#21636=ORIENTED_EDGE('',*,*,#15961,.F.);
#21637=ORIENTED_EDGE('',*,*,#15960,.T.);
#21638=ORIENTED_EDGE('',*,*,#15962,.F.);
#21639=ORIENTED_EDGE('',*,*,#15963,.F.);
#21640=ORIENTED_EDGE('',*,*,#15964,.F.);
#21641=ORIENTED_EDGE('',*,*,#15963,.T.);
#21642=ORIENTED_EDGE('',*,*,#15965,.F.);
#21643=ORIENTED_EDGE('',*,*,#15966,.F.);
#21644=ORIENTED_EDGE('',*,*,#15967,.F.);
#21645=ORIENTED_EDGE('',*,*,#15966,.T.);
#21646=ORIENTED_EDGE('',*,*,#15968,.F.);
#21647=ORIENTED_EDGE('',*,*,#15969,.F.);
#21648=ORIENTED_EDGE('',*,*,#15970,.F.);
#21649=ORIENTED_EDGE('',*,*,#15969,.T.);
#21650=ORIENTED_EDGE('',*,*,#15971,.F.);
#21651=ORIENTED_EDGE('',*,*,#15972,.F.);
#21652=ORIENTED_EDGE('',*,*,#15973,.F.);
#21653=ORIENTED_EDGE('',*,*,#15972,.T.);
#21654=ORIENTED_EDGE('',*,*,#15974,.F.);
#21655=ORIENTED_EDGE('',*,*,#15975,.F.);
#21656=ORIENTED_EDGE('',*,*,#15976,.F.);
#21657=ORIENTED_EDGE('',*,*,#15975,.T.);
#21658=ORIENTED_EDGE('',*,*,#15977,.F.);
#21659=ORIENTED_EDGE('',*,*,#15978,.F.);
#21660=ORIENTED_EDGE('',*,*,#15979,.F.);
#21661=ORIENTED_EDGE('',*,*,#15978,.T.);
#21662=ORIENTED_EDGE('',*,*,#15980,.F.);
#21663=ORIENTED_EDGE('',*,*,#15981,.F.);
#21664=ORIENTED_EDGE('',*,*,#15982,.F.);
#21665=ORIENTED_EDGE('',*,*,#15981,.T.);
#21666=ORIENTED_EDGE('',*,*,#15983,.F.);
#21667=ORIENTED_EDGE('',*,*,#15984,.F.);
#21668=ORIENTED_EDGE('',*,*,#15985,.F.);
#21669=ORIENTED_EDGE('',*,*,#15984,.T.);
#21670=ORIENTED_EDGE('',*,*,#15986,.F.);
#21671=ORIENTED_EDGE('',*,*,#15987,.F.);
#21672=ORIENTED_EDGE('',*,*,#15988,.F.);
#21673=ORIENTED_EDGE('',*,*,#15987,.T.);
#21674=ORIENTED_EDGE('',*,*,#15989,.F.);
#21675=ORIENTED_EDGE('',*,*,#15990,.F.);
#21676=ORIENTED_EDGE('',*,*,#15991,.F.);
#21677=ORIENTED_EDGE('',*,*,#15990,.T.);
#21678=ORIENTED_EDGE('',*,*,#15992,.F.);
#21679=ORIENTED_EDGE('',*,*,#15993,.F.);
#21680=ORIENTED_EDGE('',*,*,#15994,.F.);
#21681=ORIENTED_EDGE('',*,*,#15993,.T.);
#21682=ORIENTED_EDGE('',*,*,#15995,.F.);
#21683=ORIENTED_EDGE('',*,*,#15996,.F.);
#21684=ORIENTED_EDGE('',*,*,#15997,.F.);
#21685=ORIENTED_EDGE('',*,*,#15996,.T.);
#21686=ORIENTED_EDGE('',*,*,#15998,.F.);
#21687=ORIENTED_EDGE('',*,*,#15999,.F.);
#21688=ORIENTED_EDGE('',*,*,#16000,.F.);
#21689=ORIENTED_EDGE('',*,*,#15999,.T.);
#21690=ORIENTED_EDGE('',*,*,#16001,.F.);
#21691=ORIENTED_EDGE('',*,*,#15111,.F.);
#21692=ORIENTED_EDGE('',*,*,#15116,.F.);
#21693=ORIENTED_EDGE('',*,*,#15125,.F.);
#21694=ORIENTED_EDGE('',*,*,#16001,.T.);
#21695=ORIENTED_EDGE('',*,*,#15998,.T.);
#21696=ORIENTED_EDGE('',*,*,#15995,.T.);
#21697=ORIENTED_EDGE('',*,*,#15992,.T.);
#21698=ORIENTED_EDGE('',*,*,#15989,.T.);
#21699=ORIENTED_EDGE('',*,*,#15986,.T.);
#21700=ORIENTED_EDGE('',*,*,#15983,.T.);
#21701=ORIENTED_EDGE('',*,*,#15980,.T.);
#21702=ORIENTED_EDGE('',*,*,#15977,.T.);
#21703=ORIENTED_EDGE('',*,*,#15974,.T.);
#21704=ORIENTED_EDGE('',*,*,#15971,.T.);
#21705=ORIENTED_EDGE('',*,*,#15968,.T.);
#21706=ORIENTED_EDGE('',*,*,#15965,.T.);
#21707=ORIENTED_EDGE('',*,*,#15962,.T.);
#21708=ORIENTED_EDGE('',*,*,#15959,.T.);
#21709=ORIENTED_EDGE('',*,*,#15956,.T.);
#21710=ORIENTED_EDGE('',*,*,#15953,.T.);
#21711=ORIENTED_EDGE('',*,*,#15950,.T.);
#21712=ORIENTED_EDGE('',*,*,#15947,.T.);
#21713=ORIENTED_EDGE('',*,*,#15944,.T.);
#21714=ORIENTED_EDGE('',*,*,#15941,.T.);
#21715=ORIENTED_EDGE('',*,*,#15938,.T.);
#21716=ORIENTED_EDGE('',*,*,#15935,.T.);
#21717=ORIENTED_EDGE('',*,*,#15932,.T.);
#21718=ORIENTED_EDGE('',*,*,#15929,.T.);
#21719=ORIENTED_EDGE('',*,*,#15926,.T.);
#21720=ORIENTED_EDGE('',*,*,#15923,.T.);
#21721=ORIENTED_EDGE('',*,*,#15920,.T.);
#21722=ORIENTED_EDGE('',*,*,#15917,.T.);
#21723=ORIENTED_EDGE('',*,*,#15914,.T.);
#21724=ORIENTED_EDGE('',*,*,#15911,.T.);
#21725=ORIENTED_EDGE('',*,*,#15908,.T.);
#21726=ORIENTED_EDGE('',*,*,#15905,.T.);
#21727=ORIENTED_EDGE('',*,*,#15902,.T.);
#21728=ORIENTED_EDGE('',*,*,#15899,.T.);
#21729=ORIENTED_EDGE('',*,*,#15896,.T.);
#21730=ORIENTED_EDGE('',*,*,#15893,.T.);
#21731=ORIENTED_EDGE('',*,*,#15890,.T.);
#21732=ORIENTED_EDGE('',*,*,#15887,.T.);
#21733=ORIENTED_EDGE('',*,*,#15884,.T.);
#21734=ORIENTED_EDGE('',*,*,#15881,.T.);
#21735=ORIENTED_EDGE('',*,*,#15878,.T.);
#21736=ORIENTED_EDGE('',*,*,#15875,.T.);
#21737=ORIENTED_EDGE('',*,*,#15872,.T.);
#21738=ORIENTED_EDGE('',*,*,#15869,.T.);
#21739=ORIENTED_EDGE('',*,*,#15866,.T.);
#21740=ORIENTED_EDGE('',*,*,#15863,.T.);
#21741=ORIENTED_EDGE('',*,*,#15860,.T.);
#21742=ORIENTED_EDGE('',*,*,#15857,.T.);
#21743=ORIENTED_EDGE('',*,*,#15854,.T.);
#21744=ORIENTED_EDGE('',*,*,#15851,.T.);
#21745=ORIENTED_EDGE('',*,*,#15848,.T.);
#21746=ORIENTED_EDGE('',*,*,#15845,.T.);
#21747=ORIENTED_EDGE('',*,*,#15842,.T.);
#21748=ORIENTED_EDGE('',*,*,#15839,.T.);
#21749=ORIENTED_EDGE('',*,*,#15836,.T.);
#21750=ORIENTED_EDGE('',*,*,#15833,.T.);
#21751=ORIENTED_EDGE('',*,*,#15830,.T.);
#21752=ORIENTED_EDGE('',*,*,#15827,.T.);
#21753=ORIENTED_EDGE('',*,*,#15824,.T.);
#21754=ORIENTED_EDGE('',*,*,#15821,.T.);
#21755=ORIENTED_EDGE('',*,*,#15818,.T.);
#21756=ORIENTED_EDGE('',*,*,#15815,.T.);
#21757=ORIENTED_EDGE('',*,*,#15812,.T.);
#21758=ORIENTED_EDGE('',*,*,#15809,.T.);
#21759=ORIENTED_EDGE('',*,*,#15806,.T.);
#21760=ORIENTED_EDGE('',*,*,#15803,.T.);
#21761=ORIENTED_EDGE('',*,*,#15800,.T.);
#21762=ORIENTED_EDGE('',*,*,#15797,.T.);
#21763=ORIENTED_EDGE('',*,*,#15794,.T.);
#21764=ORIENTED_EDGE('',*,*,#15791,.T.);
#21765=ORIENTED_EDGE('',*,*,#15788,.T.);
#21766=ORIENTED_EDGE('',*,*,#15785,.T.);
#21767=ORIENTED_EDGE('',*,*,#15782,.T.);
#21768=ORIENTED_EDGE('',*,*,#15779,.T.);
#21769=ORIENTED_EDGE('',*,*,#15776,.T.);
#21770=ORIENTED_EDGE('',*,*,#15773,.T.);
#21771=ORIENTED_EDGE('',*,*,#15770,.T.);
#21772=ORIENTED_EDGE('',*,*,#15767,.T.);
#21773=ORIENTED_EDGE('',*,*,#15764,.T.);
#21774=ORIENTED_EDGE('',*,*,#15761,.T.);
#21775=ORIENTED_EDGE('',*,*,#15758,.T.);
#21776=ORIENTED_EDGE('',*,*,#15755,.T.);
#21777=ORIENTED_EDGE('',*,*,#15752,.T.);
#21778=ORIENTED_EDGE('',*,*,#15749,.T.);
#21779=ORIENTED_EDGE('',*,*,#15746,.T.);
#21780=ORIENTED_EDGE('',*,*,#15743,.T.);
#21781=ORIENTED_EDGE('',*,*,#15740,.T.);
#21782=ORIENTED_EDGE('',*,*,#15737,.T.);
#21783=ORIENTED_EDGE('',*,*,#15734,.T.);
#21784=ORIENTED_EDGE('',*,*,#15731,.T.);
#21785=ORIENTED_EDGE('',*,*,#15728,.T.);
#21786=ORIENTED_EDGE('',*,*,#15725,.T.);
#21787=ORIENTED_EDGE('',*,*,#15722,.T.);
#21788=ORIENTED_EDGE('',*,*,#15719,.T.);
#21789=ORIENTED_EDGE('',*,*,#15716,.T.);
#21790=ORIENTED_EDGE('',*,*,#15713,.T.);
#21791=ORIENTED_EDGE('',*,*,#15710,.T.);
#21792=ORIENTED_EDGE('',*,*,#15707,.T.);
#21793=ORIENTED_EDGE('',*,*,#15704,.T.);
#21794=ORIENTED_EDGE('',*,*,#15701,.T.);
#21795=ORIENTED_EDGE('',*,*,#15698,.T.);
#21796=ORIENTED_EDGE('',*,*,#15695,.T.);
#21797=ORIENTED_EDGE('',*,*,#15692,.T.);
#21798=ORIENTED_EDGE('',*,*,#15689,.T.);
#21799=ORIENTED_EDGE('',*,*,#15686,.T.);
#21800=ORIENTED_EDGE('',*,*,#15683,.T.);
#21801=ORIENTED_EDGE('',*,*,#15680,.T.);
#21802=ORIENTED_EDGE('',*,*,#15677,.T.);
#21803=ORIENTED_EDGE('',*,*,#15674,.T.);
#21804=ORIENTED_EDGE('',*,*,#15671,.T.);
#21805=ORIENTED_EDGE('',*,*,#15668,.T.);
#21806=ORIENTED_EDGE('',*,*,#15665,.T.);
#21807=ORIENTED_EDGE('',*,*,#15662,.T.);
#21808=ORIENTED_EDGE('',*,*,#15659,.T.);
#21809=ORIENTED_EDGE('',*,*,#15656,.T.);
#21810=ORIENTED_EDGE('',*,*,#15653,.T.);
#21811=ORIENTED_EDGE('',*,*,#15650,.T.);
#21812=ORIENTED_EDGE('',*,*,#15647,.T.);
#21813=ORIENTED_EDGE('',*,*,#15644,.T.);
#21814=ORIENTED_EDGE('',*,*,#15641,.T.);
#21815=ORIENTED_EDGE('',*,*,#15638,.T.);
#21816=ORIENTED_EDGE('',*,*,#15635,.T.);
#21817=ORIENTED_EDGE('',*,*,#15632,.T.);
#21818=ORIENTED_EDGE('',*,*,#15629,.T.);
#21819=ORIENTED_EDGE('',*,*,#15626,.T.);
#21820=ORIENTED_EDGE('',*,*,#15623,.T.);
#21821=ORIENTED_EDGE('',*,*,#15620,.T.);
#21822=ORIENTED_EDGE('',*,*,#15617,.T.);
#21823=ORIENTED_EDGE('',*,*,#15614,.T.);
#21824=ORIENTED_EDGE('',*,*,#15611,.T.);
#21825=ORIENTED_EDGE('',*,*,#15608,.T.);
#21826=ORIENTED_EDGE('',*,*,#15605,.T.);
#21827=ORIENTED_EDGE('',*,*,#15602,.T.);
#21828=ORIENTED_EDGE('',*,*,#15599,.T.);
#21829=ORIENTED_EDGE('',*,*,#15596,.T.);
#21830=ORIENTED_EDGE('',*,*,#15593,.T.);
#21831=ORIENTED_EDGE('',*,*,#15590,.T.);
#21832=ORIENTED_EDGE('',*,*,#15587,.T.);
#21833=ORIENTED_EDGE('',*,*,#15584,.T.);
#21834=ORIENTED_EDGE('',*,*,#15581,.T.);
#21835=ORIENTED_EDGE('',*,*,#15578,.T.);
#21836=ORIENTED_EDGE('',*,*,#15575,.T.);
#21837=ORIENTED_EDGE('',*,*,#15572,.T.);
#21838=ORIENTED_EDGE('',*,*,#15569,.T.);
#21839=ORIENTED_EDGE('',*,*,#15566,.T.);
#21840=ORIENTED_EDGE('',*,*,#15563,.T.);
#21841=ORIENTED_EDGE('',*,*,#15560,.T.);
#21842=ORIENTED_EDGE('',*,*,#15557,.T.);
#21843=ORIENTED_EDGE('',*,*,#15554,.T.);
#21844=ORIENTED_EDGE('',*,*,#15551,.T.);
#21845=ORIENTED_EDGE('',*,*,#15548,.T.);
#21846=ORIENTED_EDGE('',*,*,#15545,.T.);
#21847=ORIENTED_EDGE('',*,*,#15542,.T.);
#21848=ORIENTED_EDGE('',*,*,#15539,.T.);
#21849=ORIENTED_EDGE('',*,*,#15536,.T.);
#21850=ORIENTED_EDGE('',*,*,#15533,.T.);
#21851=ORIENTED_EDGE('',*,*,#15530,.T.);
#21852=ORIENTED_EDGE('',*,*,#15527,.T.);
#21853=ORIENTED_EDGE('',*,*,#15524,.T.);
#21854=ORIENTED_EDGE('',*,*,#15521,.T.);
#21855=ORIENTED_EDGE('',*,*,#15518,.T.);
#21856=ORIENTED_EDGE('',*,*,#15515,.T.);
#21857=ORIENTED_EDGE('',*,*,#15512,.T.);
#21858=ORIENTED_EDGE('',*,*,#15509,.T.);
#21859=ORIENTED_EDGE('',*,*,#15506,.T.);
#21860=ORIENTED_EDGE('',*,*,#15503,.T.);
#21861=ORIENTED_EDGE('',*,*,#15500,.T.);
#21862=ORIENTED_EDGE('',*,*,#15497,.T.);
#21863=ORIENTED_EDGE('',*,*,#15494,.T.);
#21864=ORIENTED_EDGE('',*,*,#15491,.T.);
#21865=ORIENTED_EDGE('',*,*,#15488,.T.);
#21866=ORIENTED_EDGE('',*,*,#15485,.T.);
#21867=ORIENTED_EDGE('',*,*,#15482,.T.);
#21868=ORIENTED_EDGE('',*,*,#15479,.T.);
#21869=ORIENTED_EDGE('',*,*,#15476,.T.);
#21870=ORIENTED_EDGE('',*,*,#15473,.T.);
#21871=ORIENTED_EDGE('',*,*,#15470,.T.);
#21872=ORIENTED_EDGE('',*,*,#15467,.T.);
#21873=ORIENTED_EDGE('',*,*,#15464,.T.);
#21874=ORIENTED_EDGE('',*,*,#15461,.T.);
#21875=ORIENTED_EDGE('',*,*,#15458,.T.);
#21876=ORIENTED_EDGE('',*,*,#15455,.T.);
#21877=ORIENTED_EDGE('',*,*,#15452,.T.);
#21878=ORIENTED_EDGE('',*,*,#15449,.T.);
#21879=ORIENTED_EDGE('',*,*,#15446,.T.);
#21880=ORIENTED_EDGE('',*,*,#15443,.T.);
#21881=ORIENTED_EDGE('',*,*,#15440,.T.);
#21882=ORIENTED_EDGE('',*,*,#15437,.T.);
#21883=ORIENTED_EDGE('',*,*,#15434,.T.);
#21884=ORIENTED_EDGE('',*,*,#15431,.T.);
#21885=ORIENTED_EDGE('',*,*,#15428,.T.);
#21886=ORIENTED_EDGE('',*,*,#15425,.T.);
#21887=ORIENTED_EDGE('',*,*,#15422,.T.);
#21888=ORIENTED_EDGE('',*,*,#15419,.T.);
#21889=ORIENTED_EDGE('',*,*,#15416,.T.);
#21890=ORIENTED_EDGE('',*,*,#15413,.T.);
#21891=ORIENTED_EDGE('',*,*,#15410,.T.);
#21892=ORIENTED_EDGE('',*,*,#15407,.T.);
#21893=ORIENTED_EDGE('',*,*,#15404,.T.);
#21894=ORIENTED_EDGE('',*,*,#15401,.T.);
#21895=ORIENTED_EDGE('',*,*,#15398,.T.);
#21896=ORIENTED_EDGE('',*,*,#15395,.T.);
#21897=ORIENTED_EDGE('',*,*,#15392,.T.);
#21898=ORIENTED_EDGE('',*,*,#15389,.T.);
#21899=ORIENTED_EDGE('',*,*,#15386,.T.);
#21900=ORIENTED_EDGE('',*,*,#15383,.T.);
#21901=ORIENTED_EDGE('',*,*,#15380,.T.);
#21902=ORIENTED_EDGE('',*,*,#15377,.T.);
#21903=ORIENTED_EDGE('',*,*,#15374,.T.);
#21904=ORIENTED_EDGE('',*,*,#15371,.T.);
#21905=ORIENTED_EDGE('',*,*,#15368,.T.);
#21906=ORIENTED_EDGE('',*,*,#15365,.T.);
#21907=ORIENTED_EDGE('',*,*,#15362,.T.);
#21908=ORIENTED_EDGE('',*,*,#15359,.T.);
#21909=ORIENTED_EDGE('',*,*,#15356,.T.);
#21910=ORIENTED_EDGE('',*,*,#15353,.T.);
#21911=ORIENTED_EDGE('',*,*,#15350,.T.);
#21912=ORIENTED_EDGE('',*,*,#15347,.T.);
#21913=ORIENTED_EDGE('',*,*,#15344,.T.);
#21914=ORIENTED_EDGE('',*,*,#15341,.T.);
#21915=ORIENTED_EDGE('',*,*,#15338,.T.);
#21916=ORIENTED_EDGE('',*,*,#15335,.T.);
#21917=ORIENTED_EDGE('',*,*,#15332,.T.);
#21918=ORIENTED_EDGE('',*,*,#15329,.T.);
#21919=ORIENTED_EDGE('',*,*,#15326,.T.);
#21920=ORIENTED_EDGE('',*,*,#15323,.T.);
#21921=ORIENTED_EDGE('',*,*,#15320,.T.);
#21922=ORIENTED_EDGE('',*,*,#15317,.T.);
#21923=ORIENTED_EDGE('',*,*,#15314,.T.);
#21924=ORIENTED_EDGE('',*,*,#15311,.T.);
#21925=ORIENTED_EDGE('',*,*,#15308,.T.);
#21926=ORIENTED_EDGE('',*,*,#15305,.T.);
#21927=ORIENTED_EDGE('',*,*,#15302,.T.);
#21928=ORIENTED_EDGE('',*,*,#15299,.T.);
#21929=ORIENTED_EDGE('',*,*,#15296,.T.);
#21930=ORIENTED_EDGE('',*,*,#15293,.T.);
#21931=ORIENTED_EDGE('',*,*,#15290,.T.);
#21932=ORIENTED_EDGE('',*,*,#15287,.T.);
#21933=ORIENTED_EDGE('',*,*,#15284,.T.);
#21934=ORIENTED_EDGE('',*,*,#15281,.T.);
#21935=ORIENTED_EDGE('',*,*,#15278,.T.);
#21936=ORIENTED_EDGE('',*,*,#15275,.T.);
#21937=ORIENTED_EDGE('',*,*,#15272,.T.);
#21938=ORIENTED_EDGE('',*,*,#15269,.T.);
#21939=ORIENTED_EDGE('',*,*,#15266,.T.);
#21940=ORIENTED_EDGE('',*,*,#15263,.T.);
#21941=ORIENTED_EDGE('',*,*,#15260,.T.);
#21942=ORIENTED_EDGE('',*,*,#15257,.T.);
#21943=ORIENTED_EDGE('',*,*,#15254,.T.);
#21944=ORIENTED_EDGE('',*,*,#15251,.T.);
#21945=ORIENTED_EDGE('',*,*,#15248,.T.);
#21946=ORIENTED_EDGE('',*,*,#15245,.T.);
#21947=ORIENTED_EDGE('',*,*,#15242,.T.);
#21948=ORIENTED_EDGE('',*,*,#15239,.T.);
#21949=ORIENTED_EDGE('',*,*,#15236,.T.);
#21950=ORIENTED_EDGE('',*,*,#15233,.T.);
#21951=ORIENTED_EDGE('',*,*,#15230,.T.);
#21952=ORIENTED_EDGE('',*,*,#15227,.T.);
#21953=ORIENTED_EDGE('',*,*,#15224,.T.);
#21954=ORIENTED_EDGE('',*,*,#15221,.T.);
#21955=ORIENTED_EDGE('',*,*,#15218,.T.);
#21956=ORIENTED_EDGE('',*,*,#15215,.T.);
#21957=ORIENTED_EDGE('',*,*,#15212,.T.);
#21958=ORIENTED_EDGE('',*,*,#15209,.T.);
#21959=ORIENTED_EDGE('',*,*,#15206,.T.);
#21960=ORIENTED_EDGE('',*,*,#15203,.T.);
#21961=ORIENTED_EDGE('',*,*,#15200,.T.);
#21962=ORIENTED_EDGE('',*,*,#15197,.T.);
#21963=ORIENTED_EDGE('',*,*,#15194,.T.);
#21964=ORIENTED_EDGE('',*,*,#15191,.T.);
#21965=ORIENTED_EDGE('',*,*,#15188,.T.);
#21966=ORIENTED_EDGE('',*,*,#15185,.T.);
#21967=ORIENTED_EDGE('',*,*,#15182,.T.);
#21968=ORIENTED_EDGE('',*,*,#15179,.T.);
#21969=ORIENTED_EDGE('',*,*,#15176,.T.);
#21970=ORIENTED_EDGE('',*,*,#15173,.T.);
#21971=ORIENTED_EDGE('',*,*,#15170,.T.);
#21972=ORIENTED_EDGE('',*,*,#15167,.T.);
#21973=ORIENTED_EDGE('',*,*,#15101,.F.);
#21974=ORIENTED_EDGE('',*,*,#15103,.F.);
#21975=ORIENTED_EDGE('',*,*,#15106,.F.);
#21976=ORIENTED_EDGE('',*,*,#15109,.F.);
#21977=ORIENTED_EDGE('',*,*,#15112,.F.);
#21978=ORIENTED_EDGE('',*,*,#15163,.T.);
#21979=ORIENTED_EDGE('',*,*,#15160,.T.);
#21980=ORIENTED_EDGE('',*,*,#15157,.T.);
#21981=ORIENTED_EDGE('',*,*,#15154,.T.);
#21982=ORIENTED_EDGE('',*,*,#15151,.T.);
#21983=ORIENTED_EDGE('',*,*,#15148,.T.);
#21984=ORIENTED_EDGE('',*,*,#15145,.T.);
#21985=ORIENTED_EDGE('',*,*,#15142,.T.);
#21986=ORIENTED_EDGE('',*,*,#15139,.T.);
#21987=ORIENTED_EDGE('',*,*,#15136,.T.);
#21988=ORIENTED_EDGE('',*,*,#15166,.T.);
#21989=ORIENTED_EDGE('',*,*,#15169,.T.);
#21990=ORIENTED_EDGE('',*,*,#15172,.T.);
#21991=ORIENTED_EDGE('',*,*,#15175,.T.);
#21992=ORIENTED_EDGE('',*,*,#15178,.T.);
#21993=ORIENTED_EDGE('',*,*,#15181,.T.);
#21994=ORIENTED_EDGE('',*,*,#15184,.T.);
#21995=ORIENTED_EDGE('',*,*,#15187,.T.);
#21996=ORIENTED_EDGE('',*,*,#15190,.T.);
#21997=ORIENTED_EDGE('',*,*,#15193,.T.);
#21998=ORIENTED_EDGE('',*,*,#15196,.T.);
#21999=ORIENTED_EDGE('',*,*,#15199,.T.);
#22000=ORIENTED_EDGE('',*,*,#15202,.T.);
#22001=ORIENTED_EDGE('',*,*,#15205,.T.);
#22002=ORIENTED_EDGE('',*,*,#15208,.T.);
#22003=ORIENTED_EDGE('',*,*,#15211,.T.);
#22004=ORIENTED_EDGE('',*,*,#15214,.T.);
#22005=ORIENTED_EDGE('',*,*,#15217,.T.);
#22006=ORIENTED_EDGE('',*,*,#15220,.T.);
#22007=ORIENTED_EDGE('',*,*,#15223,.T.);
#22008=ORIENTED_EDGE('',*,*,#15226,.T.);
#22009=ORIENTED_EDGE('',*,*,#15229,.T.);
#22010=ORIENTED_EDGE('',*,*,#15232,.T.);
#22011=ORIENTED_EDGE('',*,*,#15235,.T.);
#22012=ORIENTED_EDGE('',*,*,#15238,.T.);
#22013=ORIENTED_EDGE('',*,*,#15241,.T.);
#22014=ORIENTED_EDGE('',*,*,#15244,.T.);
#22015=ORIENTED_EDGE('',*,*,#15247,.T.);
#22016=ORIENTED_EDGE('',*,*,#15250,.T.);
#22017=ORIENTED_EDGE('',*,*,#15253,.T.);
#22018=ORIENTED_EDGE('',*,*,#15256,.T.);
#22019=ORIENTED_EDGE('',*,*,#15259,.T.);
#22020=ORIENTED_EDGE('',*,*,#15262,.T.);
#22021=ORIENTED_EDGE('',*,*,#15265,.T.);
#22022=ORIENTED_EDGE('',*,*,#15268,.T.);
#22023=ORIENTED_EDGE('',*,*,#15271,.T.);
#22024=ORIENTED_EDGE('',*,*,#15274,.T.);
#22025=ORIENTED_EDGE('',*,*,#15277,.T.);
#22026=ORIENTED_EDGE('',*,*,#15280,.T.);
#22027=ORIENTED_EDGE('',*,*,#15283,.T.);
#22028=ORIENTED_EDGE('',*,*,#15286,.T.);
#22029=ORIENTED_EDGE('',*,*,#15289,.T.);
#22030=ORIENTED_EDGE('',*,*,#15292,.T.);
#22031=ORIENTED_EDGE('',*,*,#15295,.T.);
#22032=ORIENTED_EDGE('',*,*,#15298,.T.);
#22033=ORIENTED_EDGE('',*,*,#15301,.T.);
#22034=ORIENTED_EDGE('',*,*,#15304,.T.);
#22035=ORIENTED_EDGE('',*,*,#15307,.T.);
#22036=ORIENTED_EDGE('',*,*,#15310,.T.);
#22037=ORIENTED_EDGE('',*,*,#15313,.T.);
#22038=ORIENTED_EDGE('',*,*,#15316,.T.);
#22039=ORIENTED_EDGE('',*,*,#15319,.T.);
#22040=ORIENTED_EDGE('',*,*,#15322,.T.);
#22041=ORIENTED_EDGE('',*,*,#15325,.T.);
#22042=ORIENTED_EDGE('',*,*,#15328,.T.);
#22043=ORIENTED_EDGE('',*,*,#15331,.T.);
#22044=ORIENTED_EDGE('',*,*,#15334,.T.);
#22045=ORIENTED_EDGE('',*,*,#15337,.T.);
#22046=ORIENTED_EDGE('',*,*,#15340,.T.);
#22047=ORIENTED_EDGE('',*,*,#15343,.T.);
#22048=ORIENTED_EDGE('',*,*,#15346,.T.);
#22049=ORIENTED_EDGE('',*,*,#15349,.T.);
#22050=ORIENTED_EDGE('',*,*,#15352,.T.);
#22051=ORIENTED_EDGE('',*,*,#15355,.T.);
#22052=ORIENTED_EDGE('',*,*,#15358,.T.);
#22053=ORIENTED_EDGE('',*,*,#15361,.T.);
#22054=ORIENTED_EDGE('',*,*,#15364,.T.);
#22055=ORIENTED_EDGE('',*,*,#15367,.T.);
#22056=ORIENTED_EDGE('',*,*,#15370,.T.);
#22057=ORIENTED_EDGE('',*,*,#15373,.T.);
#22058=ORIENTED_EDGE('',*,*,#15376,.T.);
#22059=ORIENTED_EDGE('',*,*,#15379,.T.);
#22060=ORIENTED_EDGE('',*,*,#15382,.T.);
#22061=ORIENTED_EDGE('',*,*,#15385,.T.);
#22062=ORIENTED_EDGE('',*,*,#15388,.T.);
#22063=ORIENTED_EDGE('',*,*,#15391,.T.);
#22064=ORIENTED_EDGE('',*,*,#15394,.T.);
#22065=ORIENTED_EDGE('',*,*,#15397,.T.);
#22066=ORIENTED_EDGE('',*,*,#15400,.T.);
#22067=ORIENTED_EDGE('',*,*,#15403,.T.);
#22068=ORIENTED_EDGE('',*,*,#15406,.T.);
#22069=ORIENTED_EDGE('',*,*,#15409,.T.);
#22070=ORIENTED_EDGE('',*,*,#15412,.T.);
#22071=ORIENTED_EDGE('',*,*,#15415,.T.);
#22072=ORIENTED_EDGE('',*,*,#15418,.T.);
#22073=ORIENTED_EDGE('',*,*,#15421,.T.);
#22074=ORIENTED_EDGE('',*,*,#15424,.T.);
#22075=ORIENTED_EDGE('',*,*,#15427,.T.);
#22076=ORIENTED_EDGE('',*,*,#15430,.T.);
#22077=ORIENTED_EDGE('',*,*,#15433,.T.);
#22078=ORIENTED_EDGE('',*,*,#15436,.T.);
#22079=ORIENTED_EDGE('',*,*,#15439,.T.);
#22080=ORIENTED_EDGE('',*,*,#15442,.T.);
#22081=ORIENTED_EDGE('',*,*,#15445,.T.);
#22082=ORIENTED_EDGE('',*,*,#15448,.T.);
#22083=ORIENTED_EDGE('',*,*,#15451,.T.);
#22084=ORIENTED_EDGE('',*,*,#15454,.T.);
#22085=ORIENTED_EDGE('',*,*,#15457,.T.);
#22086=ORIENTED_EDGE('',*,*,#15460,.T.);
#22087=ORIENTED_EDGE('',*,*,#15463,.T.);
#22088=ORIENTED_EDGE('',*,*,#15466,.T.);
#22089=ORIENTED_EDGE('',*,*,#15469,.T.);
#22090=ORIENTED_EDGE('',*,*,#15472,.T.);
#22091=ORIENTED_EDGE('',*,*,#15475,.T.);
#22092=ORIENTED_EDGE('',*,*,#15478,.T.);
#22093=ORIENTED_EDGE('',*,*,#15481,.T.);
#22094=ORIENTED_EDGE('',*,*,#15484,.T.);
#22095=ORIENTED_EDGE('',*,*,#15487,.T.);
#22096=ORIENTED_EDGE('',*,*,#15490,.T.);
#22097=ORIENTED_EDGE('',*,*,#15493,.T.);
#22098=ORIENTED_EDGE('',*,*,#15496,.T.);
#22099=ORIENTED_EDGE('',*,*,#15499,.T.);
#22100=ORIENTED_EDGE('',*,*,#15502,.T.);
#22101=ORIENTED_EDGE('',*,*,#15505,.T.);
#22102=ORIENTED_EDGE('',*,*,#15508,.T.);
#22103=ORIENTED_EDGE('',*,*,#15511,.T.);
#22104=ORIENTED_EDGE('',*,*,#15514,.T.);
#22105=ORIENTED_EDGE('',*,*,#15517,.T.);
#22106=ORIENTED_EDGE('',*,*,#15520,.T.);
#22107=ORIENTED_EDGE('',*,*,#15523,.T.);
#22108=ORIENTED_EDGE('',*,*,#15526,.T.);
#22109=ORIENTED_EDGE('',*,*,#15529,.T.);
#22110=ORIENTED_EDGE('',*,*,#15532,.T.);
#22111=ORIENTED_EDGE('',*,*,#15535,.T.);
#22112=ORIENTED_EDGE('',*,*,#15538,.T.);
#22113=ORIENTED_EDGE('',*,*,#15541,.T.);
#22114=ORIENTED_EDGE('',*,*,#15544,.T.);
#22115=ORIENTED_EDGE('',*,*,#15547,.T.);
#22116=ORIENTED_EDGE('',*,*,#15550,.T.);
#22117=ORIENTED_EDGE('',*,*,#15553,.T.);
#22118=ORIENTED_EDGE('',*,*,#15556,.T.);
#22119=ORIENTED_EDGE('',*,*,#15559,.T.);
#22120=ORIENTED_EDGE('',*,*,#15562,.T.);
#22121=ORIENTED_EDGE('',*,*,#15565,.T.);
#22122=ORIENTED_EDGE('',*,*,#15568,.T.);
#22123=ORIENTED_EDGE('',*,*,#15571,.T.);
#22124=ORIENTED_EDGE('',*,*,#15574,.T.);
#22125=ORIENTED_EDGE('',*,*,#15577,.T.);
#22126=ORIENTED_EDGE('',*,*,#15580,.T.);
#22127=ORIENTED_EDGE('',*,*,#15583,.T.);
#22128=ORIENTED_EDGE('',*,*,#15586,.T.);
#22129=ORIENTED_EDGE('',*,*,#15589,.T.);
#22130=ORIENTED_EDGE('',*,*,#15592,.T.);
#22131=ORIENTED_EDGE('',*,*,#15595,.T.);
#22132=ORIENTED_EDGE('',*,*,#15598,.T.);
#22133=ORIENTED_EDGE('',*,*,#15601,.T.);
#22134=ORIENTED_EDGE('',*,*,#15604,.T.);
#22135=ORIENTED_EDGE('',*,*,#15607,.T.);
#22136=ORIENTED_EDGE('',*,*,#15610,.T.);
#22137=ORIENTED_EDGE('',*,*,#15613,.T.);
#22138=ORIENTED_EDGE('',*,*,#15616,.T.);
#22139=ORIENTED_EDGE('',*,*,#15619,.T.);
#22140=ORIENTED_EDGE('',*,*,#15622,.T.);
#22141=ORIENTED_EDGE('',*,*,#15625,.T.);
#22142=ORIENTED_EDGE('',*,*,#15628,.T.);
#22143=ORIENTED_EDGE('',*,*,#15631,.T.);
#22144=ORIENTED_EDGE('',*,*,#15634,.T.);
#22145=ORIENTED_EDGE('',*,*,#15637,.T.);
#22146=ORIENTED_EDGE('',*,*,#15640,.T.);
#22147=ORIENTED_EDGE('',*,*,#15643,.T.);
#22148=ORIENTED_EDGE('',*,*,#15646,.T.);
#22149=ORIENTED_EDGE('',*,*,#15649,.T.);
#22150=ORIENTED_EDGE('',*,*,#15652,.T.);
#22151=ORIENTED_EDGE('',*,*,#15655,.T.);
#22152=ORIENTED_EDGE('',*,*,#15658,.T.);
#22153=ORIENTED_EDGE('',*,*,#15661,.T.);
#22154=ORIENTED_EDGE('',*,*,#15664,.T.);
#22155=ORIENTED_EDGE('',*,*,#15667,.T.);
#22156=ORIENTED_EDGE('',*,*,#15670,.T.);
#22157=ORIENTED_EDGE('',*,*,#15673,.T.);
#22158=ORIENTED_EDGE('',*,*,#15676,.T.);
#22159=ORIENTED_EDGE('',*,*,#15679,.T.);
#22160=ORIENTED_EDGE('',*,*,#15682,.T.);
#22161=ORIENTED_EDGE('',*,*,#15685,.T.);
#22162=ORIENTED_EDGE('',*,*,#15688,.T.);
#22163=ORIENTED_EDGE('',*,*,#15691,.T.);
#22164=ORIENTED_EDGE('',*,*,#15694,.T.);
#22165=ORIENTED_EDGE('',*,*,#15697,.T.);
#22166=ORIENTED_EDGE('',*,*,#15700,.T.);
#22167=ORIENTED_EDGE('',*,*,#15703,.T.);
#22168=ORIENTED_EDGE('',*,*,#15706,.T.);
#22169=ORIENTED_EDGE('',*,*,#15709,.T.);
#22170=ORIENTED_EDGE('',*,*,#15712,.T.);
#22171=ORIENTED_EDGE('',*,*,#15715,.T.);
#22172=ORIENTED_EDGE('',*,*,#15718,.T.);
#22173=ORIENTED_EDGE('',*,*,#15721,.T.);
#22174=ORIENTED_EDGE('',*,*,#15724,.T.);
#22175=ORIENTED_EDGE('',*,*,#15727,.T.);
#22176=ORIENTED_EDGE('',*,*,#15730,.T.);
#22177=ORIENTED_EDGE('',*,*,#15733,.T.);
#22178=ORIENTED_EDGE('',*,*,#15736,.T.);
#22179=ORIENTED_EDGE('',*,*,#15739,.T.);
#22180=ORIENTED_EDGE('',*,*,#15742,.T.);
#22181=ORIENTED_EDGE('',*,*,#15745,.T.);
#22182=ORIENTED_EDGE('',*,*,#15748,.T.);
#22183=ORIENTED_EDGE('',*,*,#15751,.T.);
#22184=ORIENTED_EDGE('',*,*,#15754,.T.);
#22185=ORIENTED_EDGE('',*,*,#15757,.T.);
#22186=ORIENTED_EDGE('',*,*,#15760,.T.);
#22187=ORIENTED_EDGE('',*,*,#15763,.T.);
#22188=ORIENTED_EDGE('',*,*,#15766,.T.);
#22189=ORIENTED_EDGE('',*,*,#15769,.T.);
#22190=ORIENTED_EDGE('',*,*,#15772,.T.);
#22191=ORIENTED_EDGE('',*,*,#15775,.T.);
#22192=ORIENTED_EDGE('',*,*,#15778,.T.);
#22193=ORIENTED_EDGE('',*,*,#15781,.T.);
#22194=ORIENTED_EDGE('',*,*,#15784,.T.);
#22195=ORIENTED_EDGE('',*,*,#15787,.T.);
#22196=ORIENTED_EDGE('',*,*,#15790,.T.);
#22197=ORIENTED_EDGE('',*,*,#15793,.T.);
#22198=ORIENTED_EDGE('',*,*,#15796,.T.);
#22199=ORIENTED_EDGE('',*,*,#15799,.T.);
#22200=ORIENTED_EDGE('',*,*,#15802,.T.);
#22201=ORIENTED_EDGE('',*,*,#15805,.T.);
#22202=ORIENTED_EDGE('',*,*,#15808,.T.);
#22203=ORIENTED_EDGE('',*,*,#15811,.T.);
#22204=ORIENTED_EDGE('',*,*,#15814,.T.);
#22205=ORIENTED_EDGE('',*,*,#15817,.T.);
#22206=ORIENTED_EDGE('',*,*,#15820,.T.);
#22207=ORIENTED_EDGE('',*,*,#15823,.T.);
#22208=ORIENTED_EDGE('',*,*,#15826,.T.);
#22209=ORIENTED_EDGE('',*,*,#15829,.T.);
#22210=ORIENTED_EDGE('',*,*,#15832,.T.);
#22211=ORIENTED_EDGE('',*,*,#15835,.T.);
#22212=ORIENTED_EDGE('',*,*,#15838,.T.);
#22213=ORIENTED_EDGE('',*,*,#15841,.T.);
#22214=ORIENTED_EDGE('',*,*,#15844,.T.);
#22215=ORIENTED_EDGE('',*,*,#15847,.T.);
#22216=ORIENTED_EDGE('',*,*,#15850,.T.);
#22217=ORIENTED_EDGE('',*,*,#15853,.T.);
#22218=ORIENTED_EDGE('',*,*,#15856,.T.);
#22219=ORIENTED_EDGE('',*,*,#15859,.T.);
#22220=ORIENTED_EDGE('',*,*,#15862,.T.);
#22221=ORIENTED_EDGE('',*,*,#15865,.T.);
#22222=ORIENTED_EDGE('',*,*,#15868,.T.);
#22223=ORIENTED_EDGE('',*,*,#15871,.T.);
#22224=ORIENTED_EDGE('',*,*,#15874,.T.);
#22225=ORIENTED_EDGE('',*,*,#15877,.T.);
#22226=ORIENTED_EDGE('',*,*,#15880,.T.);
#22227=ORIENTED_EDGE('',*,*,#15883,.T.);
#22228=ORIENTED_EDGE('',*,*,#15886,.T.);
#22229=ORIENTED_EDGE('',*,*,#15889,.T.);
#22230=ORIENTED_EDGE('',*,*,#15892,.T.);
#22231=ORIENTED_EDGE('',*,*,#15895,.T.);
#22232=ORIENTED_EDGE('',*,*,#15898,.T.);
#22233=ORIENTED_EDGE('',*,*,#15901,.T.);
#22234=ORIENTED_EDGE('',*,*,#15904,.T.);
#22235=ORIENTED_EDGE('',*,*,#15907,.T.);
#22236=ORIENTED_EDGE('',*,*,#15910,.T.);
#22237=ORIENTED_EDGE('',*,*,#15913,.T.);
#22238=ORIENTED_EDGE('',*,*,#15916,.T.);
#22239=ORIENTED_EDGE('',*,*,#15919,.T.);
#22240=ORIENTED_EDGE('',*,*,#15922,.T.);
#22241=ORIENTED_EDGE('',*,*,#15925,.T.);
#22242=ORIENTED_EDGE('',*,*,#15928,.T.);
#22243=ORIENTED_EDGE('',*,*,#15931,.T.);
#22244=ORIENTED_EDGE('',*,*,#15934,.T.);
#22245=ORIENTED_EDGE('',*,*,#15937,.T.);
#22246=ORIENTED_EDGE('',*,*,#15940,.T.);
#22247=ORIENTED_EDGE('',*,*,#15943,.T.);
#22248=ORIENTED_EDGE('',*,*,#15946,.T.);
#22249=ORIENTED_EDGE('',*,*,#15949,.T.);
#22250=ORIENTED_EDGE('',*,*,#15952,.T.);
#22251=ORIENTED_EDGE('',*,*,#15955,.T.);
#22252=ORIENTED_EDGE('',*,*,#15958,.T.);
#22253=ORIENTED_EDGE('',*,*,#15961,.T.);
#22254=ORIENTED_EDGE('',*,*,#15964,.T.);
#22255=ORIENTED_EDGE('',*,*,#15967,.T.);
#22256=ORIENTED_EDGE('',*,*,#15970,.T.);
#22257=ORIENTED_EDGE('',*,*,#15973,.T.);
#22258=ORIENTED_EDGE('',*,*,#15976,.T.);
#22259=ORIENTED_EDGE('',*,*,#15979,.T.);
#22260=ORIENTED_EDGE('',*,*,#15982,.T.);
#22261=ORIENTED_EDGE('',*,*,#15985,.T.);
#22262=ORIENTED_EDGE('',*,*,#15988,.T.);
#22263=ORIENTED_EDGE('',*,*,#15991,.T.);
#22264=ORIENTED_EDGE('',*,*,#15994,.T.);
#22265=ORIENTED_EDGE('',*,*,#15997,.T.);
#22266=ORIENTED_EDGE('',*,*,#16000,.T.);
#22267=ORIENTED_EDGE('',*,*,#15127,.F.);
#22268=ORIENTED_EDGE('',*,*,#15129,.F.);
#22269=ORIENTED_EDGE('',*,*,#15131,.F.);
#22270=ORIENTED_EDGE('',*,*,#15133,.F.);
#22271=ORIENTED_EDGE('',*,*,#15135,.F.);
#22272=ORIENTED_EDGE('',*,*,#15165,.T.);
#22273=ORIENTED_EDGE('',*,*,#15162,.T.);
#22274=ORIENTED_EDGE('',*,*,#15159,.T.);
#22275=ORIENTED_EDGE('',*,*,#15156,.T.);
#22276=ORIENTED_EDGE('',*,*,#15153,.T.);
#22277=ORIENTED_EDGE('',*,*,#15150,.T.);
#22278=ORIENTED_EDGE('',*,*,#15147,.T.);
#22279=ORIENTED_EDGE('',*,*,#15144,.T.);
#22280=ORIENTED_EDGE('',*,*,#15141,.T.);
#22281=ORIENTED_EDGE('',*,*,#15138,.T.);
#22282=ORIENTED_EDGE('',*,*,#16002,.T.);
#22283=ORIENTED_EDGE('',*,*,#16003,.T.);
#22284=ORIENTED_EDGE('',*,*,#16004,.T.);
#22285=ORIENTED_EDGE('',*,*,#16003,.F.);
#22286=ORIENTED_EDGE('',*,*,#16005,.F.);
#22287=ORIENTED_EDGE('',*,*,#16006,.F.);
#22288=ORIENTED_EDGE('',*,*,#16007,.F.);
#22289=ORIENTED_EDGE('',*,*,#16008,.F.);
#22290=ORIENTED_EDGE('',*,*,#16009,.F.);
#22291=ORIENTED_EDGE('',*,*,#16010,.F.);
#22292=ORIENTED_EDGE('',*,*,#16011,.F.);
#22293=ORIENTED_EDGE('',*,*,#16012,.F.);
#22294=ORIENTED_EDGE('',*,*,#16013,.F.);
#22295=ORIENTED_EDGE('',*,*,#16014,.F.);
#22296=ORIENTED_EDGE('',*,*,#16015,.F.);
#22297=ORIENTED_EDGE('',*,*,#16016,.F.);
#22298=ORIENTED_EDGE('',*,*,#16017,.T.);
#22299=ORIENTED_EDGE('',*,*,#16018,.T.);
#22300=ORIENTED_EDGE('',*,*,#16019,.T.);
#22301=ORIENTED_EDGE('',*,*,#16020,.T.);
#22302=ORIENTED_EDGE('',*,*,#16021,.T.);
#22303=ORIENTED_EDGE('',*,*,#16022,.T.);
#22304=ORIENTED_EDGE('',*,*,#16023,.T.);
#22305=ORIENTED_EDGE('',*,*,#16024,.T.);
#22306=ORIENTED_EDGE('',*,*,#16025,.T.);
#22307=ORIENTED_EDGE('',*,*,#16026,.T.);
#22308=ORIENTED_EDGE('',*,*,#16027,.T.);
#22309=ORIENTED_EDGE('',*,*,#16028,.T.);
#22310=ORIENTED_EDGE('',*,*,#16029,.F.);
#22311=ORIENTED_EDGE('',*,*,#16030,.F.);
#22312=ORIENTED_EDGE('',*,*,#16031,.F.);
#22313=ORIENTED_EDGE('',*,*,#16004,.F.);
#22314=ORIENTED_EDGE('',*,*,#16002,.F.);
#22315=ORIENTED_EDGE('',*,*,#16032,.T.);
#22316=ORIENTED_EDGE('',*,*,#16033,.F.);
#22317=ORIENTED_EDGE('',*,*,#16032,.F.);
#22318=ORIENTED_EDGE('',*,*,#16034,.T.);
#22319=ORIENTED_EDGE('',*,*,#16035,.T.);
#22320=ORIENTED_EDGE('',*,*,#16013,.T.);
#22321=ORIENTED_EDGE('',*,*,#16035,.F.);
#22322=ORIENTED_EDGE('',*,*,#16034,.F.);
#22323=ORIENTED_EDGE('',*,*,#16036,.T.);
#22324=ORIENTED_EDGE('',*,*,#16037,.F.);
#22325=ORIENTED_EDGE('',*,*,#16036,.F.);
#22326=ORIENTED_EDGE('',*,*,#16038,.T.);
#22327=ORIENTED_EDGE('',*,*,#16039,.T.);
#22328=ORIENTED_EDGE('',*,*,#16031,.T.);
#22329=ORIENTED_EDGE('',*,*,#16039,.F.);
#22330=ORIENTED_EDGE('',*,*,#16038,.F.);
#22331=ORIENTED_EDGE('',*,*,#16040,.T.);
#22332=ORIENTED_EDGE('',*,*,#16041,.F.);
#22333=ORIENTED_EDGE('',*,*,#16040,.F.);
#22334=ORIENTED_EDGE('',*,*,#16042,.T.);
#22335=ORIENTED_EDGE('',*,*,#16043,.T.);
#22336=ORIENTED_EDGE('',*,*,#16014,.T.);
#22337=ORIENTED_EDGE('',*,*,#16043,.F.);
#22338=ORIENTED_EDGE('',*,*,#16042,.F.);
#22339=ORIENTED_EDGE('',*,*,#16044,.T.);
#22340=ORIENTED_EDGE('',*,*,#16045,.F.);
#22341=ORIENTED_EDGE('',*,*,#16044,.F.);
#22342=ORIENTED_EDGE('',*,*,#16046,.T.);
#22343=ORIENTED_EDGE('',*,*,#16047,.T.);
#22344=ORIENTED_EDGE('',*,*,#16030,.T.);
#22345=ORIENTED_EDGE('',*,*,#16047,.F.);
#22346=ORIENTED_EDGE('',*,*,#16046,.F.);
#22347=ORIENTED_EDGE('',*,*,#16048,.T.);
#22348=ORIENTED_EDGE('',*,*,#16049,.F.);
#22349=ORIENTED_EDGE('',*,*,#16048,.F.);
#22350=ORIENTED_EDGE('',*,*,#16050,.T.);
#22351=ORIENTED_EDGE('',*,*,#16051,.T.);
#22352=ORIENTED_EDGE('',*,*,#16015,.T.);
#22353=ORIENTED_EDGE('',*,*,#16051,.F.);
#22354=ORIENTED_EDGE('',*,*,#16050,.F.);
#22355=ORIENTED_EDGE('',*,*,#16052,.T.);
#22356=ORIENTED_EDGE('',*,*,#16053,.F.);
#22357=ORIENTED_EDGE('',*,*,#16052,.F.);
#22358=ORIENTED_EDGE('',*,*,#16054,.T.);
#22359=ORIENTED_EDGE('',*,*,#16055,.T.);
#22360=ORIENTED_EDGE('',*,*,#16029,.T.);
#22361=ORIENTED_EDGE('',*,*,#16055,.F.);
#22362=ORIENTED_EDGE('',*,*,#16054,.F.);
#22363=ORIENTED_EDGE('',*,*,#16056,.T.);
#22364=ORIENTED_EDGE('',*,*,#16057,.F.);
#22365=ORIENTED_EDGE('',*,*,#16056,.F.);
#22366=ORIENTED_EDGE('',*,*,#16058,.T.);
#22367=ORIENTED_EDGE('',*,*,#16059,.T.);
#22368=ORIENTED_EDGE('',*,*,#16016,.T.);
#22369=ORIENTED_EDGE('',*,*,#16059,.F.);
#22370=ORIENTED_EDGE('',*,*,#16058,.F.);
#22371=ORIENTED_EDGE('',*,*,#16060,.T.);
#22372=ORIENTED_EDGE('',*,*,#16061,.F.);
#22373=ORIENTED_EDGE('',*,*,#16060,.F.);
#22374=ORIENTED_EDGE('',*,*,#16062,.F.);
#22375=ORIENTED_EDGE('',*,*,#16063,.T.);
#22376=ORIENTED_EDGE('',*,*,#16023,.F.);
#22377=ORIENTED_EDGE('',*,*,#16064,.F.);
#22378=ORIENTED_EDGE('',*,*,#16065,.F.);
#22379=ORIENTED_EDGE('',*,*,#16066,.T.);
#22380=ORIENTED_EDGE('',*,*,#16024,.F.);
#22381=ORIENTED_EDGE('',*,*,#16063,.F.);
#22382=ORIENTED_EDGE('',*,*,#16067,.F.);
#22383=ORIENTED_EDGE('',*,*,#16068,.T.);
#22384=ORIENTED_EDGE('',*,*,#16025,.F.);
#22385=ORIENTED_EDGE('',*,*,#16066,.F.);
#22386=ORIENTED_EDGE('',*,*,#16069,.F.);
#22387=ORIENTED_EDGE('',*,*,#16070,.T.);
#22388=ORIENTED_EDGE('',*,*,#16026,.F.);
#22389=ORIENTED_EDGE('',*,*,#16068,.F.);
#22390=ORIENTED_EDGE('',*,*,#16071,.F.);
#22391=ORIENTED_EDGE('',*,*,#16072,.T.);
#22392=ORIENTED_EDGE('',*,*,#16027,.F.);
#22393=ORIENTED_EDGE('',*,*,#16070,.F.);
#22394=ORIENTED_EDGE('',*,*,#16073,.F.);
#22395=ORIENTED_EDGE('',*,*,#16064,.T.);
#22396=ORIENTED_EDGE('',*,*,#16028,.F.);
#22397=ORIENTED_EDGE('',*,*,#16072,.F.);
#22398=ORIENTED_EDGE('',*,*,#16074,.F.);
#22399=ORIENTED_EDGE('',*,*,#16075,.T.);
#22400=ORIENTED_EDGE('',*,*,#16017,.F.);
#22401=ORIENTED_EDGE('',*,*,#16076,.F.);
#22402=ORIENTED_EDGE('',*,*,#16077,.F.);
#22403=ORIENTED_EDGE('',*,*,#16078,.T.);
#22404=ORIENTED_EDGE('',*,*,#16018,.F.);
#22405=ORIENTED_EDGE('',*,*,#16075,.F.);
#22406=ORIENTED_EDGE('',*,*,#16079,.F.);
#22407=ORIENTED_EDGE('',*,*,#16080,.T.);
#22408=ORIENTED_EDGE('',*,*,#16019,.F.);
#22409=ORIENTED_EDGE('',*,*,#16078,.F.);
#22410=ORIENTED_EDGE('',*,*,#16081,.F.);
#22411=ORIENTED_EDGE('',*,*,#16082,.T.);
#22412=ORIENTED_EDGE('',*,*,#16020,.F.);
#22413=ORIENTED_EDGE('',*,*,#16080,.F.);
#22414=ORIENTED_EDGE('',*,*,#16083,.F.);
#22415=ORIENTED_EDGE('',*,*,#16084,.T.);
#22416=ORIENTED_EDGE('',*,*,#16021,.F.);
#22417=ORIENTED_EDGE('',*,*,#16082,.F.);
#22418=ORIENTED_EDGE('',*,*,#16085,.F.);
#22419=ORIENTED_EDGE('',*,*,#16076,.T.);
#22420=ORIENTED_EDGE('',*,*,#16022,.F.);
#22421=ORIENTED_EDGE('',*,*,#16084,.F.);
#22422=ORIENTED_EDGE('',*,*,#16005,.T.);
#22423=ORIENTED_EDGE('',*,*,#16086,.T.);
#22424=ORIENTED_EDGE('',*,*,#16087,.T.);
#22425=ORIENTED_EDGE('',*,*,#16088,.F.);
#22426=ORIENTED_EDGE('',*,*,#16012,.T.);
#22427=ORIENTED_EDGE('',*,*,#16089,.T.);
#22428=ORIENTED_EDGE('',*,*,#16090,.T.);
#22429=ORIENTED_EDGE('',*,*,#16086,.F.);
#22430=ORIENTED_EDGE('',*,*,#16011,.T.);
#22431=ORIENTED_EDGE('',*,*,#16091,.T.);
#22432=ORIENTED_EDGE('',*,*,#16092,.T.);
#22433=ORIENTED_EDGE('',*,*,#16089,.F.);
#22434=ORIENTED_EDGE('',*,*,#16010,.T.);
#22435=ORIENTED_EDGE('',*,*,#16093,.T.);
#22436=ORIENTED_EDGE('',*,*,#16094,.T.);
#22437=ORIENTED_EDGE('',*,*,#16091,.F.);
#22438=ORIENTED_EDGE('',*,*,#16009,.T.);
#22439=ORIENTED_EDGE('',*,*,#16095,.T.);
#22440=ORIENTED_EDGE('',*,*,#16096,.T.);
#22441=ORIENTED_EDGE('',*,*,#16093,.F.);
#22442=ORIENTED_EDGE('',*,*,#16097,.T.);
#22443=ORIENTED_EDGE('',*,*,#16095,.F.);
#22444=ORIENTED_EDGE('',*,*,#16008,.T.);
#22445=ORIENTED_EDGE('',*,*,#16098,.T.);
#22446=ORIENTED_EDGE('',*,*,#16099,.T.);
#22447=ORIENTED_EDGE('',*,*,#16098,.F.);
#22448=ORIENTED_EDGE('',*,*,#16007,.T.);
#22449=ORIENTED_EDGE('',*,*,#16100,.T.);
#22450=ORIENTED_EDGE('',*,*,#16101,.T.);
#22451=ORIENTED_EDGE('',*,*,#16100,.F.);
#22452=ORIENTED_EDGE('',*,*,#16006,.T.);
#22453=ORIENTED_EDGE('',*,*,#16088,.T.);
#22454=ORIENTED_EDGE('',*,*,#16097,.F.);
#22455=ORIENTED_EDGE('',*,*,#16102,.F.);
#22456=ORIENTED_EDGE('',*,*,#16103,.F.);
#22457=ORIENTED_EDGE('',*,*,#16104,.T.);
#22458=ORIENTED_EDGE('',*,*,#16099,.F.);
#22459=ORIENTED_EDGE('',*,*,#16105,.F.);
#22460=ORIENTED_EDGE('',*,*,#16106,.F.);
#22461=ORIENTED_EDGE('',*,*,#16102,.T.);
#22462=ORIENTED_EDGE('',*,*,#16101,.F.);
#22463=ORIENTED_EDGE('',*,*,#16107,.F.);
#22464=ORIENTED_EDGE('',*,*,#16108,.F.);
#22465=ORIENTED_EDGE('',*,*,#16105,.T.);
#22466=ORIENTED_EDGE('',*,*,#16087,.F.);
#22467=ORIENTED_EDGE('',*,*,#16109,.F.);
#22468=ORIENTED_EDGE('',*,*,#16110,.F.);
#22469=ORIENTED_EDGE('',*,*,#16107,.T.);
#22470=ORIENTED_EDGE('',*,*,#16096,.F.);
#22471=ORIENTED_EDGE('',*,*,#16104,.F.);
#22472=ORIENTED_EDGE('',*,*,#16111,.F.);
#22473=ORIENTED_EDGE('',*,*,#16112,.T.);
#22474=ORIENTED_EDGE('',*,*,#16090,.F.);
#22475=ORIENTED_EDGE('',*,*,#16113,.F.);
#22476=ORIENTED_EDGE('',*,*,#16114,.F.);
#22477=ORIENTED_EDGE('',*,*,#16109,.T.);
#22478=ORIENTED_EDGE('',*,*,#16092,.F.);
#22479=ORIENTED_EDGE('',*,*,#16115,.F.);
#22480=ORIENTED_EDGE('',*,*,#16116,.F.);
#22481=ORIENTED_EDGE('',*,*,#16113,.T.);
#22482=ORIENTED_EDGE('',*,*,#16094,.F.);
#22483=ORIENTED_EDGE('',*,*,#16112,.F.);
#22484=ORIENTED_EDGE('',*,*,#16117,.F.);
#22485=ORIENTED_EDGE('',*,*,#16115,.T.);
#22486=ORIENTED_EDGE('',*,*,#16117,.T.);
#22487=ORIENTED_EDGE('',*,*,#16111,.T.);
#22488=ORIENTED_EDGE('',*,*,#16103,.T.);
#22489=ORIENTED_EDGE('',*,*,#16106,.T.);
#22490=ORIENTED_EDGE('',*,*,#16108,.T.);
#22491=ORIENTED_EDGE('',*,*,#16110,.T.);
#22492=ORIENTED_EDGE('',*,*,#16114,.T.);
#22493=ORIENTED_EDGE('',*,*,#16116,.T.);
#22494=ORIENTED_EDGE('',*,*,#16074,.T.);
#22495=ORIENTED_EDGE('',*,*,#16085,.T.);
#22496=ORIENTED_EDGE('',*,*,#16083,.T.);
#22497=ORIENTED_EDGE('',*,*,#16081,.T.);
#22498=ORIENTED_EDGE('',*,*,#16079,.T.);
#22499=ORIENTED_EDGE('',*,*,#16077,.T.);
#22500=ORIENTED_EDGE('',*,*,#16062,.T.);
#22501=ORIENTED_EDGE('',*,*,#16073,.T.);
#22502=ORIENTED_EDGE('',*,*,#16071,.T.);
#22503=ORIENTED_EDGE('',*,*,#16069,.T.);
#22504=ORIENTED_EDGE('',*,*,#16067,.T.);
#22505=ORIENTED_EDGE('',*,*,#16065,.T.);
#22506=ORIENTED_EDGE('',*,*,#16033,.T.);
#22507=ORIENTED_EDGE('',*,*,#16037,.T.);
#22508=ORIENTED_EDGE('',*,*,#16041,.T.);
#22509=ORIENTED_EDGE('',*,*,#16045,.T.);
#22510=ORIENTED_EDGE('',*,*,#16049,.T.);
#22511=ORIENTED_EDGE('',*,*,#16053,.T.);
#22512=ORIENTED_EDGE('',*,*,#16057,.T.);
#22513=ORIENTED_EDGE('',*,*,#16061,.T.);
#22514=ORIENTED_EDGE('',*,*,#16118,.F.);
#22515=ORIENTED_EDGE('',*,*,#16119,.T.);
#22516=ORIENTED_EDGE('',*,*,#16120,.F.);
#22517=ORIENTED_EDGE('',*,*,#16119,.F.);
#22518=ORIENTED_EDGE('',*,*,#16121,.F.);
#22519=ORIENTED_EDGE('',*,*,#16122,.T.);
#22520=ORIENTED_EDGE('',*,*,#16123,.F.);
#22521=ORIENTED_EDGE('',*,*,#16122,.F.);
#22522=ORIENTED_EDGE('',*,*,#16124,.T.);
#22523=ORIENTED_EDGE('',*,*,#16125,.T.);
#22524=ORIENTED_EDGE('',*,*,#16126,.T.);
#22525=ORIENTED_EDGE('',*,*,#16125,.F.);
#22526=ORIENTED_EDGE('',*,*,#16124,.F.);
#22527=ORIENTED_EDGE('',*,*,#16127,.T.);
#22528=ORIENTED_EDGE('',*,*,#16128,.F.);
#22529=ORIENTED_EDGE('',*,*,#16129,.T.);
#22530=ORIENTED_EDGE('',*,*,#16130,.F.);
#22531=ORIENTED_EDGE('',*,*,#16131,.T.);
#22532=ORIENTED_EDGE('',*,*,#16132,.F.);
#22533=ORIENTED_EDGE('',*,*,#16127,.F.);
#22534=ORIENTED_EDGE('',*,*,#16133,.T.);
#22535=ORIENTED_EDGE('',*,*,#16134,.T.);
#22536=ORIENTED_EDGE('',*,*,#16135,.F.);
#22537=ORIENTED_EDGE('',*,*,#16136,.F.);
#22538=ORIENTED_EDGE('',*,*,#16126,.F.);
#22539=ORIENTED_EDGE('',*,*,#16137,.T.);
#22540=ORIENTED_EDGE('',*,*,#16138,.T.);
#22541=ORIENTED_EDGE('',*,*,#16139,.T.);
#22542=ORIENTED_EDGE('',*,*,#16138,.F.);
#22543=ORIENTED_EDGE('',*,*,#16137,.F.);
#22544=ORIENTED_EDGE('',*,*,#16140,.T.);
#22545=ORIENTED_EDGE('',*,*,#16141,.F.);
#22546=ORIENTED_EDGE('',*,*,#16142,.T.);
#22547=ORIENTED_EDGE('',*,*,#16143,.F.);
#22548=ORIENTED_EDGE('',*,*,#16144,.T.);
#22549=ORIENTED_EDGE('',*,*,#16145,.F.);
#22550=ORIENTED_EDGE('',*,*,#16140,.F.);
#22551=ORIENTED_EDGE('',*,*,#16146,.T.);
#22552=ORIENTED_EDGE('',*,*,#16147,.T.);
#22553=ORIENTED_EDGE('',*,*,#16148,.F.);
#22554=ORIENTED_EDGE('',*,*,#16149,.F.);
#22555=ORIENTED_EDGE('',*,*,#16139,.F.);
#22556=ORIENTED_EDGE('',*,*,#16150,.F.);
#22557=ORIENTED_EDGE('',*,*,#16129,.F.);
#22558=ORIENTED_EDGE('',*,*,#16151,.F.);
#22559=ORIENTED_EDGE('',*,*,#16131,.F.);
#22560=ORIENTED_EDGE('',*,*,#16152,.F.);
#22561=ORIENTED_EDGE('',*,*,#16153,.T.);
#22562=ORIENTED_EDGE('',*,*,#16154,.T.);
#22563=ORIENTED_EDGE('',*,*,#16155,.T.);
#22564=ORIENTED_EDGE('',*,*,#16153,.F.);
#22565=ORIENTED_EDGE('',*,*,#16151,.T.);
#22566=ORIENTED_EDGE('',*,*,#16130,.T.);
#22567=ORIENTED_EDGE('',*,*,#16150,.T.);
#22568=ORIENTED_EDGE('',*,*,#16128,.T.);
#22569=ORIENTED_EDGE('',*,*,#16132,.T.);
#22570=ORIENTED_EDGE('',*,*,#16156,.F.);
#22571=ORIENTED_EDGE('',*,*,#16144,.F.);
#22572=ORIENTED_EDGE('',*,*,#16157,.F.);
#22573=ORIENTED_EDGE('',*,*,#16142,.F.);
#22574=ORIENTED_EDGE('',*,*,#16158,.F.);
#22575=ORIENTED_EDGE('',*,*,#16159,.T.);
#22576=ORIENTED_EDGE('',*,*,#16160,.T.);
#22577=ORIENTED_EDGE('',*,*,#16161,.T.);
#22578=ORIENTED_EDGE('',*,*,#16159,.F.);
#22579=ORIENTED_EDGE('',*,*,#16157,.T.);
#22580=ORIENTED_EDGE('',*,*,#16141,.T.);
#22581=ORIENTED_EDGE('',*,*,#16145,.T.);
#22582=ORIENTED_EDGE('',*,*,#16156,.T.);
#22583=ORIENTED_EDGE('',*,*,#16143,.T.);
#22584=ORIENTED_EDGE('',*,*,#16152,.T.);
#22585=ORIENTED_EDGE('',*,*,#16162,.T.);
#22586=ORIENTED_EDGE('',*,*,#16163,.T.);
#22587=ORIENTED_EDGE('',*,*,#16162,.F.);
#22588=ORIENTED_EDGE('',*,*,#16164,.F.);
#22589=ORIENTED_EDGE('',*,*,#16165,.F.);
#22590=ORIENTED_EDGE('',*,*,#16166,.F.);
#22591=ORIENTED_EDGE('',*,*,#16167,.T.);
#22592=ORIENTED_EDGE('',*,*,#16136,.T.);
#22593=ORIENTED_EDGE('',*,*,#16168,.F.);
#22594=ORIENTED_EDGE('',*,*,#16163,.F.);
#22595=ORIENTED_EDGE('',*,*,#16169,.T.);
#22596=ORIENTED_EDGE('',*,*,#16154,.F.);
#22597=ORIENTED_EDGE('',*,*,#16155,.F.);
#22598=ORIENTED_EDGE('',*,*,#16169,.F.);
#22599=ORIENTED_EDGE('',*,*,#16158,.T.);
#22600=ORIENTED_EDGE('',*,*,#16170,.T.);
#22601=ORIENTED_EDGE('',*,*,#16171,.T.);
#22602=ORIENTED_EDGE('',*,*,#16170,.F.);
#22603=ORIENTED_EDGE('',*,*,#16172,.F.);
#22604=ORIENTED_EDGE('',*,*,#16173,.F.);
#22605=ORIENTED_EDGE('',*,*,#16147,.F.);
#22606=ORIENTED_EDGE('',*,*,#16174,.T.);
#22607=ORIENTED_EDGE('',*,*,#16175,.F.);
#22608=ORIENTED_EDGE('',*,*,#16176,.T.);
#22609=ORIENTED_EDGE('',*,*,#16171,.F.);
#22610=ORIENTED_EDGE('',*,*,#16177,.T.);
#22611=ORIENTED_EDGE('',*,*,#16160,.F.);
#22612=ORIENTED_EDGE('',*,*,#16161,.F.);
#22613=ORIENTED_EDGE('',*,*,#16177,.F.);
#22614=ORIENTED_EDGE('',*,*,#16164,.T.);
#22615=ORIENTED_EDGE('',*,*,#16178,.T.);
#22616=ORIENTED_EDGE('',*,*,#16172,.T.);
#22617=ORIENTED_EDGE('',*,*,#16179,.T.);
#22618=ORIENTED_EDGE('',*,*,#16179,.F.);
#22619=ORIENTED_EDGE('',*,*,#16176,.F.);
#22620=ORIENTED_EDGE('',*,*,#16180,.F.);
#22621=ORIENTED_EDGE('',*,*,#16165,.T.);
#22622=ORIENTED_EDGE('',*,*,#16166,.T.);
#22623=ORIENTED_EDGE('',*,*,#16180,.T.);
#22624=ORIENTED_EDGE('',*,*,#16175,.T.);
#22625=ORIENTED_EDGE('',*,*,#16181,.T.);
#22626=ORIENTED_EDGE('',*,*,#16182,.T.);
#22627=ORIENTED_EDGE('',*,*,#16149,.T.);
#22628=ORIENTED_EDGE('',*,*,#16183,.F.);
#22629=ORIENTED_EDGE('',*,*,#16184,.F.);
#22630=ORIENTED_EDGE('',*,*,#16185,.T.);
#22631=ORIENTED_EDGE('',*,*,#16184,.T.);
#22632=ORIENTED_EDGE('',*,*,#16186,.F.);
#22633=ORIENTED_EDGE('',*,*,#16187,.F.);
#22634=ORIENTED_EDGE('',*,*,#16188,.T.);
#22635=ORIENTED_EDGE('',*,*,#16187,.T.);
#22636=ORIENTED_EDGE('',*,*,#16189,.F.);
#22637=ORIENTED_EDGE('',*,*,#16134,.F.);
#22638=ORIENTED_EDGE('',*,*,#16178,.F.);
#22639=ORIENTED_EDGE('',*,*,#16168,.T.);
#22640=ORIENTED_EDGE('',*,*,#16135,.T.);
#22641=ORIENTED_EDGE('',*,*,#16189,.T.);
#22642=ORIENTED_EDGE('',*,*,#16186,.T.);
#22643=ORIENTED_EDGE('',*,*,#16183,.T.);
#22644=ORIENTED_EDGE('',*,*,#16148,.T.);
#22645=ORIENTED_EDGE('',*,*,#16173,.T.);
#22646=ORIENTED_EDGE('',*,*,#16120,.T.);
#22647=ORIENTED_EDGE('',*,*,#16123,.T.);
#22648=ORIENTED_EDGE('',*,*,#16181,.F.);
#22649=ORIENTED_EDGE('',*,*,#16174,.F.);
#22650=ORIENTED_EDGE('',*,*,#16146,.F.);
#22651=ORIENTED_EDGE('',*,*,#16182,.F.);
#22652=ORIENTED_EDGE('',*,*,#16185,.F.);
#22653=ORIENTED_EDGE('',*,*,#16188,.F.);
#22654=ORIENTED_EDGE('',*,*,#16133,.F.);
#22655=ORIENTED_EDGE('',*,*,#16167,.F.);
#22656=ORIENTED_EDGE('',*,*,#16118,.T.);
#22657=ORIENTED_EDGE('',*,*,#16121,.T.);
#22658=ORIENTED_EDGE('',*,*,#16190,.F.);
#22659=ORIENTED_EDGE('',*,*,#16191,.F.);
#22660=ORIENTED_EDGE('',*,*,#16192,.F.);
#22661=ORIENTED_EDGE('',*,*,#16193,.T.);
#22662=ORIENTED_EDGE('',*,*,#16194,.F.);
#22663=ORIENTED_EDGE('',*,*,#16195,.F.);
#22664=ORIENTED_EDGE('',*,*,#16190,.T.);
#22665=ORIENTED_EDGE('',*,*,#16196,.T.);
#22666=ORIENTED_EDGE('',*,*,#16197,.F.);
#22667=ORIENTED_EDGE('',*,*,#16198,.F.);
#22668=ORIENTED_EDGE('',*,*,#16199,.F.);
#22669=ORIENTED_EDGE('',*,*,#16194,.T.);
#22670=ORIENTED_EDGE('',*,*,#16200,.T.);
#22671=ORIENTED_EDGE('',*,*,#16201,.T.);
#22672=ORIENTED_EDGE('',*,*,#16202,.F.);
#22673=ORIENTED_EDGE('',*,*,#16203,.F.);
#22674=ORIENTED_EDGE('',*,*,#16197,.T.);
#22675=ORIENTED_EDGE('',*,*,#16204,.T.);
#22676=ORIENTED_EDGE('',*,*,#16205,.F.);
#22677=ORIENTED_EDGE('',*,*,#16206,.F.);
#22678=ORIENTED_EDGE('',*,*,#16207,.F.);
#22679=ORIENTED_EDGE('',*,*,#16202,.T.);
#22680=ORIENTED_EDGE('',*,*,#16208,.T.);
#22681=ORIENTED_EDGE('',*,*,#16209,.T.);
#22682=ORIENTED_EDGE('',*,*,#16210,.F.);
#22683=ORIENTED_EDGE('',*,*,#16211,.F.);
#22684=ORIENTED_EDGE('',*,*,#16205,.T.);
#22685=ORIENTED_EDGE('',*,*,#16212,.T.);
#22686=ORIENTED_EDGE('',*,*,#16213,.F.);
#22687=ORIENTED_EDGE('',*,*,#16214,.F.);
#22688=ORIENTED_EDGE('',*,*,#16215,.F.);
#22689=ORIENTED_EDGE('',*,*,#16210,.T.);
#22690=ORIENTED_EDGE('',*,*,#16216,.T.);
#22691=ORIENTED_EDGE('',*,*,#16217,.T.);
#22692=ORIENTED_EDGE('',*,*,#16218,.T.);
#22693=ORIENTED_EDGE('',*,*,#16219,.F.);
#22694=ORIENTED_EDGE('',*,*,#16220,.T.);
#22695=ORIENTED_EDGE('',*,*,#16221,.T.);
#22696=ORIENTED_EDGE('',*,*,#16222,.T.);
#22697=ORIENTED_EDGE('',*,*,#16223,.T.);
#22698=ORIENTED_EDGE('',*,*,#16224,.T.);
#22699=ORIENTED_EDGE('',*,*,#16225,.T.);
#22700=ORIENTED_EDGE('',*,*,#16226,.T.);
#22701=ORIENTED_EDGE('',*,*,#16227,.T.);
#22702=ORIENTED_EDGE('',*,*,#16228,.T.);
#22703=ORIENTED_EDGE('',*,*,#16229,.F.);
#22704=ORIENTED_EDGE('',*,*,#16230,.T.);
#22705=ORIENTED_EDGE('',*,*,#16231,.T.);
#22706=ORIENTED_EDGE('',*,*,#16232,.T.);
#22707=ORIENTED_EDGE('',*,*,#16233,.T.);
#22708=ORIENTED_EDGE('',*,*,#16234,.T.);
#22709=ORIENTED_EDGE('',*,*,#16235,.T.);
#22710=ORIENTED_EDGE('',*,*,#16236,.T.);
#22711=ORIENTED_EDGE('',*,*,#16237,.T.);
#22712=ORIENTED_EDGE('',*,*,#16213,.T.);
#22713=ORIENTED_EDGE('',*,*,#16238,.T.);
#22714=ORIENTED_EDGE('',*,*,#16239,.F.);
#22715=ORIENTED_EDGE('',*,*,#16240,.F.);
#22716=ORIENTED_EDGE('',*,*,#16241,.F.);
#22717=ORIENTED_EDGE('',*,*,#16242,.T.);
#22718=ORIENTED_EDGE('',*,*,#16239,.T.);
#22719=ORIENTED_EDGE('',*,*,#16243,.T.);
#22720=ORIENTED_EDGE('',*,*,#16244,.T.);
#22721=ORIENTED_EDGE('',*,*,#16245,.F.);
#22722=ORIENTED_EDGE('',*,*,#16242,.F.);
#22723=ORIENTED_EDGE('',*,*,#16246,.F.);
#22724=ORIENTED_EDGE('',*,*,#16228,.F.);
#22725=ORIENTED_EDGE('',*,*,#16227,.F.);
#22726=ORIENTED_EDGE('',*,*,#16226,.F.);
#22727=ORIENTED_EDGE('',*,*,#16225,.F.);
#22728=ORIENTED_EDGE('',*,*,#16224,.F.);
#22729=ORIENTED_EDGE('',*,*,#16223,.F.);
#22730=ORIENTED_EDGE('',*,*,#16222,.F.);
#22731=ORIENTED_EDGE('',*,*,#16221,.F.);
#22732=ORIENTED_EDGE('',*,*,#16220,.F.);
#22733=ORIENTED_EDGE('',*,*,#16247,.F.);
#22734=ORIENTED_EDGE('',*,*,#16248,.T.);
#22735=ORIENTED_EDGE('',*,*,#16191,.T.);
#22736=ORIENTED_EDGE('',*,*,#16195,.T.);
#22737=ORIENTED_EDGE('',*,*,#16199,.T.);
#22738=ORIENTED_EDGE('',*,*,#16198,.T.);
#22739=ORIENTED_EDGE('',*,*,#16203,.T.);
#22740=ORIENTED_EDGE('',*,*,#16207,.T.);
#22741=ORIENTED_EDGE('',*,*,#16206,.T.);
#22742=ORIENTED_EDGE('',*,*,#16211,.T.);
#22743=ORIENTED_EDGE('',*,*,#16215,.T.);
#22744=ORIENTED_EDGE('',*,*,#16214,.T.);
#22745=ORIENTED_EDGE('',*,*,#16240,.T.);
#22746=ORIENTED_EDGE('',*,*,#16249,.F.);
#22747=ORIENTED_EDGE('',*,*,#16250,.T.);
#22748=ORIENTED_EDGE('',*,*,#16192,.T.);
#22749=ORIENTED_EDGE('',*,*,#16248,.F.);
#22750=ORIENTED_EDGE('',*,*,#16247,.T.);
#22751=ORIENTED_EDGE('',*,*,#16251,.F.);
#22752=ORIENTED_EDGE('',*,*,#16244,.F.);
#22753=ORIENTED_EDGE('',*,*,#16243,.F.);
#22754=ORIENTED_EDGE('',*,*,#16238,.F.);
#22755=ORIENTED_EDGE('',*,*,#16217,.F.);
#22756=ORIENTED_EDGE('',*,*,#16216,.F.);
#22757=ORIENTED_EDGE('',*,*,#16212,.F.);
#22758=ORIENTED_EDGE('',*,*,#16209,.F.);
#22759=ORIENTED_EDGE('',*,*,#16208,.F.);
#22760=ORIENTED_EDGE('',*,*,#16204,.F.);
#22761=ORIENTED_EDGE('',*,*,#16201,.F.);
#22762=ORIENTED_EDGE('',*,*,#16200,.F.);
#22763=ORIENTED_EDGE('',*,*,#16196,.F.);
#22764=ORIENTED_EDGE('',*,*,#16193,.F.);
#22765=ORIENTED_EDGE('',*,*,#16250,.F.);
#22766=ORIENTED_EDGE('',*,*,#16252,.F.);
#22767=ORIENTED_EDGE('',*,*,#16218,.F.);
#22768=ORIENTED_EDGE('',*,*,#16237,.F.);
#22769=ORIENTED_EDGE('',*,*,#16236,.F.);
#22770=ORIENTED_EDGE('',*,*,#16235,.F.);
#22771=ORIENTED_EDGE('',*,*,#16234,.F.);
#22772=ORIENTED_EDGE('',*,*,#16233,.F.);
#22773=ORIENTED_EDGE('',*,*,#16232,.F.);
#22774=ORIENTED_EDGE('',*,*,#16231,.F.);
#22775=ORIENTED_EDGE('',*,*,#16230,.F.);
#22776=ORIENTED_EDGE('',*,*,#16253,.T.);
#22777=ORIENTED_EDGE('',*,*,#16254,.T.);
#22778=ORIENTED_EDGE('',*,*,#16251,.T.);
#22779=ORIENTED_EDGE('',*,*,#16219,.T.);
#22780=ORIENTED_EDGE('',*,*,#16252,.T.);
#22781=ORIENTED_EDGE('',*,*,#16249,.T.);
#22782=ORIENTED_EDGE('',*,*,#16254,.F.);
#22783=ORIENTED_EDGE('',*,*,#16255,.F.);
#22784=ORIENTED_EDGE('',*,*,#16253,.F.);
#22785=ORIENTED_EDGE('',*,*,#16241,.T.);
#22786=ORIENTED_EDGE('',*,*,#16256,.T.);
#22787=ORIENTED_EDGE('',*,*,#16257,.T.);
#22788=ORIENTED_EDGE('',*,*,#16256,.F.);
#22789=ORIENTED_EDGE('',*,*,#16245,.T.);
#22790=ORIENTED_EDGE('',*,*,#16229,.T.);
#22791=ORIENTED_EDGE('',*,*,#16246,.T.);
#22792=ORIENTED_EDGE('',*,*,#16257,.F.);
#22793=ORIENTED_EDGE('',*,*,#16258,.F.);
#22794=ORIENTED_EDGE('',*,*,#16259,.T.);
#22795=ORIENTED_EDGE('',*,*,#16260,.F.);
#22796=ORIENTED_EDGE('',*,*,#16261,.F.);
#22797=ORIENTED_EDGE('',*,*,#16262,.F.);
#22798=ORIENTED_EDGE('',*,*,#16263,.F.);
#22799=ORIENTED_EDGE('',*,*,#16260,.T.);
#22800=ORIENTED_EDGE('',*,*,#16264,.T.);
#22801=ORIENTED_EDGE('',*,*,#16265,.F.);
#22802=ORIENTED_EDGE('',*,*,#16264,.F.);
#22803=ORIENTED_EDGE('',*,*,#16259,.F.);
#22804=ORIENTED_EDGE('',*,*,#16266,.T.);
#22805=ORIENTED_EDGE('',*,*,#16267,.T.);
#22806=ORIENTED_EDGE('',*,*,#16268,.T.);
#22807=ORIENTED_EDGE('',*,*,#16269,.T.);
#22808=ORIENTED_EDGE('',*,*,#16270,.T.);
#22809=ORIENTED_EDGE('',*,*,#16271,.T.);
#22810=ORIENTED_EDGE('',*,*,#16272,.T.);
#22811=ORIENTED_EDGE('',*,*,#16273,.T.);
#22812=ORIENTED_EDGE('',*,*,#16274,.T.);
#22813=ORIENTED_EDGE('',*,*,#16275,.T.);
#22814=ORIENTED_EDGE('',*,*,#16276,.T.);
#22815=ORIENTED_EDGE('',*,*,#16277,.T.);
#22816=ORIENTED_EDGE('',*,*,#16278,.T.);
#22817=ORIENTED_EDGE('',*,*,#16279,.T.);
#22818=ORIENTED_EDGE('',*,*,#16280,.T.);
#22819=ORIENTED_EDGE('',*,*,#16281,.T.);
#22820=ORIENTED_EDGE('',*,*,#16282,.T.);
#22821=ORIENTED_EDGE('',*,*,#16283,.T.);
#22822=ORIENTED_EDGE('',*,*,#16284,.T.);
#22823=ORIENTED_EDGE('',*,*,#16285,.T.);
#22824=ORIENTED_EDGE('',*,*,#16286,.T.);
#22825=ORIENTED_EDGE('',*,*,#16287,.T.);
#22826=ORIENTED_EDGE('',*,*,#16288,.T.);
#22827=ORIENTED_EDGE('',*,*,#16289,.T.);
#22828=ORIENTED_EDGE('',*,*,#16290,.T.);
#22829=ORIENTED_EDGE('',*,*,#16291,.T.);
#22830=ORIENTED_EDGE('',*,*,#16292,.T.);
#22831=ORIENTED_EDGE('',*,*,#16293,.T.);
#22832=ORIENTED_EDGE('',*,*,#16294,.T.);
#22833=ORIENTED_EDGE('',*,*,#16295,.T.);
#22834=ORIENTED_EDGE('',*,*,#16296,.T.);
#22835=ORIENTED_EDGE('',*,*,#16297,.T.);
#22836=ORIENTED_EDGE('',*,*,#16298,.T.);
#22837=ORIENTED_EDGE('',*,*,#16299,.T.);
#22838=ORIENTED_EDGE('',*,*,#16300,.T.);
#22839=ORIENTED_EDGE('',*,*,#16301,.T.);
#22840=ORIENTED_EDGE('',*,*,#16302,.T.);
#22841=ORIENTED_EDGE('',*,*,#16303,.T.);
#22842=ORIENTED_EDGE('',*,*,#16304,.T.);
#22843=ORIENTED_EDGE('',*,*,#16305,.T.);
#22844=ORIENTED_EDGE('',*,*,#16306,.T.);
#22845=ORIENTED_EDGE('',*,*,#16307,.T.);
#22846=ORIENTED_EDGE('',*,*,#16308,.T.);
#22847=ORIENTED_EDGE('',*,*,#16309,.T.);
#22848=ORIENTED_EDGE('',*,*,#16310,.T.);
#22849=ORIENTED_EDGE('',*,*,#16311,.T.);
#22850=ORIENTED_EDGE('',*,*,#16312,.T.);
#22851=ORIENTED_EDGE('',*,*,#16313,.T.);
#22852=ORIENTED_EDGE('',*,*,#16314,.T.);
#22853=ORIENTED_EDGE('',*,*,#16315,.T.);
#22854=ORIENTED_EDGE('',*,*,#16316,.T.);
#22855=ORIENTED_EDGE('',*,*,#16317,.T.);
#22856=ORIENTED_EDGE('',*,*,#16318,.T.);
#22857=ORIENTED_EDGE('',*,*,#16319,.T.);
#22858=ORIENTED_EDGE('',*,*,#16320,.T.);
#22859=ORIENTED_EDGE('',*,*,#16321,.T.);
#22860=ORIENTED_EDGE('',*,*,#16322,.T.);
#22861=ORIENTED_EDGE('',*,*,#16323,.T.);
#22862=ORIENTED_EDGE('',*,*,#16324,.T.);
#22863=ORIENTED_EDGE('',*,*,#16325,.T.);
#22864=ORIENTED_EDGE('',*,*,#16326,.T.);
#22865=ORIENTED_EDGE('',*,*,#16327,.T.);
#22866=ORIENTED_EDGE('',*,*,#16328,.T.);
#22867=ORIENTED_EDGE('',*,*,#16329,.T.);
#22868=ORIENTED_EDGE('',*,*,#16330,.T.);
#22869=ORIENTED_EDGE('',*,*,#16331,.T.);
#22870=ORIENTED_EDGE('',*,*,#16332,.T.);
#22871=ORIENTED_EDGE('',*,*,#16333,.T.);
#22872=ORIENTED_EDGE('',*,*,#16334,.T.);
#22873=ORIENTED_EDGE('',*,*,#16335,.T.);
#22874=ORIENTED_EDGE('',*,*,#16336,.T.);
#22875=ORIENTED_EDGE('',*,*,#16337,.T.);
#22876=ORIENTED_EDGE('',*,*,#16338,.T.);
#22877=ORIENTED_EDGE('',*,*,#16339,.T.);
#22878=ORIENTED_EDGE('',*,*,#16340,.T.);
#22879=ORIENTED_EDGE('',*,*,#16341,.T.);
#22880=ORIENTED_EDGE('',*,*,#16342,.T.);
#22881=ORIENTED_EDGE('',*,*,#16343,.T.);
#22882=ORIENTED_EDGE('',*,*,#16344,.T.);
#22883=ORIENTED_EDGE('',*,*,#16345,.T.);
#22884=ORIENTED_EDGE('',*,*,#16346,.T.);
#22885=ORIENTED_EDGE('',*,*,#16347,.T.);
#22886=ORIENTED_EDGE('',*,*,#16348,.T.);
#22887=ORIENTED_EDGE('',*,*,#16261,.T.);
#22888=ORIENTED_EDGE('',*,*,#16263,.T.);
#22889=ORIENTED_EDGE('',*,*,#16349,.T.);
#22890=ORIENTED_EDGE('',*,*,#16350,.T.);
#22891=ORIENTED_EDGE('',*,*,#16351,.T.);
#22892=ORIENTED_EDGE('',*,*,#16352,.T.);
#22893=ORIENTED_EDGE('',*,*,#16353,.T.);
#22894=ORIENTED_EDGE('',*,*,#16354,.T.);
#22895=ORIENTED_EDGE('',*,*,#16355,.T.);
#22896=ORIENTED_EDGE('',*,*,#16356,.T.);
#22897=ORIENTED_EDGE('',*,*,#16357,.T.);
#22898=ORIENTED_EDGE('',*,*,#16358,.T.);
#22899=ORIENTED_EDGE('',*,*,#16359,.T.);
#22900=ORIENTED_EDGE('',*,*,#16360,.T.);
#22901=ORIENTED_EDGE('',*,*,#16361,.T.);
#22902=ORIENTED_EDGE('',*,*,#16362,.T.);
#22903=ORIENTED_EDGE('',*,*,#16363,.T.);
#22904=ORIENTED_EDGE('',*,*,#16364,.T.);
#22905=ORIENTED_EDGE('',*,*,#16365,.T.);
#22906=ORIENTED_EDGE('',*,*,#16366,.T.);
#22907=ORIENTED_EDGE('',*,*,#16367,.T.);
#22908=ORIENTED_EDGE('',*,*,#16368,.T.);
#22909=ORIENTED_EDGE('',*,*,#16369,.T.);
#22910=ORIENTED_EDGE('',*,*,#16370,.T.);
#22911=ORIENTED_EDGE('',*,*,#16371,.T.);
#22912=ORIENTED_EDGE('',*,*,#16372,.T.);
#22913=ORIENTED_EDGE('',*,*,#16373,.T.);
#22914=ORIENTED_EDGE('',*,*,#16372,.F.);
#22915=ORIENTED_EDGE('',*,*,#16374,.F.);
#22916=ORIENTED_EDGE('',*,*,#16375,.T.);
#22917=ORIENTED_EDGE('',*,*,#16376,.F.);
#22918=ORIENTED_EDGE('',*,*,#16350,.F.);
#22919=ORIENTED_EDGE('',*,*,#16377,.F.);
#22920=ORIENTED_EDGE('',*,*,#16351,.F.);
#22921=ORIENTED_EDGE('',*,*,#16376,.T.);
#22922=ORIENTED_EDGE('',*,*,#16378,.T.);
#22923=ORIENTED_EDGE('',*,*,#16379,.F.);
#22924=ORIENTED_EDGE('',*,*,#16378,.F.);
#22925=ORIENTED_EDGE('',*,*,#16375,.F.);
#22926=ORIENTED_EDGE('',*,*,#16380,.F.);
#22927=ORIENTED_EDGE('',*,*,#16381,.T.);
#22928=ORIENTED_EDGE('',*,*,#16382,.F.);
#22929=ORIENTED_EDGE('',*,*,#16353,.F.);
#22930=ORIENTED_EDGE('',*,*,#16383,.F.);
#22931=ORIENTED_EDGE('',*,*,#16354,.F.);
#22932=ORIENTED_EDGE('',*,*,#16382,.T.);
#22933=ORIENTED_EDGE('',*,*,#16384,.T.);
#22934=ORIENTED_EDGE('',*,*,#16385,.F.);
#22935=ORIENTED_EDGE('',*,*,#16384,.F.);
#22936=ORIENTED_EDGE('',*,*,#16381,.F.);
#22937=ORIENTED_EDGE('',*,*,#16386,.F.);
#22938=ORIENTED_EDGE('',*,*,#16387,.T.);
#22939=ORIENTED_EDGE('',*,*,#16388,.F.);
#22940=ORIENTED_EDGE('',*,*,#16356,.F.);
#22941=ORIENTED_EDGE('',*,*,#16389,.F.);
#22942=ORIENTED_EDGE('',*,*,#16357,.F.);
#22943=ORIENTED_EDGE('',*,*,#16388,.T.);
#22944=ORIENTED_EDGE('',*,*,#16390,.T.);
#22945=ORIENTED_EDGE('',*,*,#16391,.F.);
#22946=ORIENTED_EDGE('',*,*,#16390,.F.);
#22947=ORIENTED_EDGE('',*,*,#16387,.F.);
#22948=ORIENTED_EDGE('',*,*,#16392,.F.);
#22949=ORIENTED_EDGE('',*,*,#16393,.T.);
#22950=ORIENTED_EDGE('',*,*,#16394,.F.);
#22951=ORIENTED_EDGE('',*,*,#16359,.F.);
#22952=ORIENTED_EDGE('',*,*,#16395,.F.);
#22953=ORIENTED_EDGE('',*,*,#16360,.F.);
#22954=ORIENTED_EDGE('',*,*,#16394,.T.);
#22955=ORIENTED_EDGE('',*,*,#16396,.T.);
#22956=ORIENTED_EDGE('',*,*,#16397,.F.);
#22957=ORIENTED_EDGE('',*,*,#16396,.F.);
#22958=ORIENTED_EDGE('',*,*,#16393,.F.);
#22959=ORIENTED_EDGE('',*,*,#16398,.F.);
#22960=ORIENTED_EDGE('',*,*,#16399,.T.);
#22961=ORIENTED_EDGE('',*,*,#16400,.F.);
#22962=ORIENTED_EDGE('',*,*,#16362,.F.);
#22963=ORIENTED_EDGE('',*,*,#16401,.F.);
#22964=ORIENTED_EDGE('',*,*,#16363,.F.);
#22965=ORIENTED_EDGE('',*,*,#16400,.T.);
#22966=ORIENTED_EDGE('',*,*,#16402,.T.);
#22967=ORIENTED_EDGE('',*,*,#16403,.F.);
#22968=ORIENTED_EDGE('',*,*,#16402,.F.);
#22969=ORIENTED_EDGE('',*,*,#16399,.F.);
#22970=ORIENTED_EDGE('',*,*,#16404,.F.);
#22971=ORIENTED_EDGE('',*,*,#16405,.T.);
#22972=ORIENTED_EDGE('',*,*,#16406,.F.);
#22973=ORIENTED_EDGE('',*,*,#16365,.F.);
#22974=ORIENTED_EDGE('',*,*,#16407,.F.);
#22975=ORIENTED_EDGE('',*,*,#16366,.F.);
#22976=ORIENTED_EDGE('',*,*,#16406,.T.);
#22977=ORIENTED_EDGE('',*,*,#16408,.T.);
#22978=ORIENTED_EDGE('',*,*,#16409,.F.);
#22979=ORIENTED_EDGE('',*,*,#16408,.F.);
#22980=ORIENTED_EDGE('',*,*,#16405,.F.);
#22981=ORIENTED_EDGE('',*,*,#16410,.F.);
#22982=ORIENTED_EDGE('',*,*,#16411,.T.);
#22983=ORIENTED_EDGE('',*,*,#16412,.F.);
#22984=ORIENTED_EDGE('',*,*,#16368,.F.);
#22985=ORIENTED_EDGE('',*,*,#16413,.F.);
#22986=ORIENTED_EDGE('',*,*,#16369,.F.);
#22987=ORIENTED_EDGE('',*,*,#16412,.T.);
#22988=ORIENTED_EDGE('',*,*,#16414,.T.);
#22989=ORIENTED_EDGE('',*,*,#16415,.F.);
#22990=ORIENTED_EDGE('',*,*,#16414,.F.);
#22991=ORIENTED_EDGE('',*,*,#16411,.F.);
#22992=ORIENTED_EDGE('',*,*,#16416,.F.);
#22993=ORIENTED_EDGE('',*,*,#16417,.T.);
#22994=ORIENTED_EDGE('',*,*,#16418,.F.);
#22995=ORIENTED_EDGE('',*,*,#16371,.F.);
#22996=ORIENTED_EDGE('',*,*,#16419,.F.);
#22997=ORIENTED_EDGE('',*,*,#16266,.F.);
#22998=ORIENTED_EDGE('',*,*,#16418,.T.);
#22999=ORIENTED_EDGE('',*,*,#16420,.T.);
#23000=ORIENTED_EDGE('',*,*,#16421,.F.);
#23001=ORIENTED_EDGE('',*,*,#16420,.F.);
#23002=ORIENTED_EDGE('',*,*,#16417,.F.);
#23003=ORIENTED_EDGE('',*,*,#16422,.F.);
#23004=ORIENTED_EDGE('',*,*,#16423,.F.);
#23005=ORIENTED_EDGE('',*,*,#16424,.T.);
#23006=ORIENTED_EDGE('',*,*,#16425,.F.);
#23007=ORIENTED_EDGE('',*,*,#16268,.F.);
#23008=ORIENTED_EDGE('',*,*,#16426,.F.);
#23009=ORIENTED_EDGE('',*,*,#16269,.F.);
#23010=ORIENTED_EDGE('',*,*,#16425,.T.);
#23011=ORIENTED_EDGE('',*,*,#16427,.T.);
#23012=ORIENTED_EDGE('',*,*,#16428,.F.);
#23013=ORIENTED_EDGE('',*,*,#16427,.F.);
#23014=ORIENTED_EDGE('',*,*,#16424,.F.);
#23015=ORIENTED_EDGE('',*,*,#16429,.F.);
#23016=ORIENTED_EDGE('',*,*,#16430,.T.);
#23017=ORIENTED_EDGE('',*,*,#16431,.F.);
#23018=ORIENTED_EDGE('',*,*,#16271,.F.);
#23019=ORIENTED_EDGE('',*,*,#16432,.F.);
#23020=ORIENTED_EDGE('',*,*,#16272,.F.);
#23021=ORIENTED_EDGE('',*,*,#16431,.T.);
#23022=ORIENTED_EDGE('',*,*,#16433,.T.);
#23023=ORIENTED_EDGE('',*,*,#16434,.F.);
#23024=ORIENTED_EDGE('',*,*,#16433,.F.);
#23025=ORIENTED_EDGE('',*,*,#16430,.F.);
#23026=ORIENTED_EDGE('',*,*,#16435,.F.);
#23027=ORIENTED_EDGE('',*,*,#16436,.T.);
#23028=ORIENTED_EDGE('',*,*,#16437,.F.);
#23029=ORIENTED_EDGE('',*,*,#16274,.F.);
#23030=ORIENTED_EDGE('',*,*,#16438,.F.);
#23031=ORIENTED_EDGE('',*,*,#16275,.F.);
#23032=ORIENTED_EDGE('',*,*,#16437,.T.);
#23033=ORIENTED_EDGE('',*,*,#16439,.T.);
#23034=ORIENTED_EDGE('',*,*,#16440,.F.);
#23035=ORIENTED_EDGE('',*,*,#16439,.F.);
#23036=ORIENTED_EDGE('',*,*,#16436,.F.);
#23037=ORIENTED_EDGE('',*,*,#16441,.F.);
#23038=ORIENTED_EDGE('',*,*,#16442,.T.);
#23039=ORIENTED_EDGE('',*,*,#16443,.F.);
#23040=ORIENTED_EDGE('',*,*,#16277,.F.);
#23041=ORIENTED_EDGE('',*,*,#16444,.F.);
#23042=ORIENTED_EDGE('',*,*,#16278,.F.);
#23043=ORIENTED_EDGE('',*,*,#16443,.T.);
#23044=ORIENTED_EDGE('',*,*,#16445,.T.);
#23045=ORIENTED_EDGE('',*,*,#16446,.F.);
#23046=ORIENTED_EDGE('',*,*,#16445,.F.);
#23047=ORIENTED_EDGE('',*,*,#16442,.F.);
#23048=ORIENTED_EDGE('',*,*,#16447,.F.);
#23049=ORIENTED_EDGE('',*,*,#16448,.T.);
#23050=ORIENTED_EDGE('',*,*,#16449,.F.);
#23051=ORIENTED_EDGE('',*,*,#16280,.F.);
#23052=ORIENTED_EDGE('',*,*,#16450,.F.);
#23053=ORIENTED_EDGE('',*,*,#16281,.F.);
#23054=ORIENTED_EDGE('',*,*,#16449,.T.);
#23055=ORIENTED_EDGE('',*,*,#16451,.T.);
#23056=ORIENTED_EDGE('',*,*,#16452,.F.);
#23057=ORIENTED_EDGE('',*,*,#16451,.F.);
#23058=ORIENTED_EDGE('',*,*,#16448,.F.);
#23059=ORIENTED_EDGE('',*,*,#16453,.F.);
#23060=ORIENTED_EDGE('',*,*,#16454,.T.);
#23061=ORIENTED_EDGE('',*,*,#16455,.F.);
#23062=ORIENTED_EDGE('',*,*,#16283,.F.);
#23063=ORIENTED_EDGE('',*,*,#16456,.F.);
#23064=ORIENTED_EDGE('',*,*,#16284,.F.);
#23065=ORIENTED_EDGE('',*,*,#16455,.T.);
#23066=ORIENTED_EDGE('',*,*,#16457,.T.);
#23067=ORIENTED_EDGE('',*,*,#16458,.F.);
#23068=ORIENTED_EDGE('',*,*,#16457,.F.);
#23069=ORIENTED_EDGE('',*,*,#16454,.F.);
#23070=ORIENTED_EDGE('',*,*,#16459,.F.);
#23071=ORIENTED_EDGE('',*,*,#16460,.T.);
#23072=ORIENTED_EDGE('',*,*,#16461,.F.);
#23073=ORIENTED_EDGE('',*,*,#16286,.F.);
#23074=ORIENTED_EDGE('',*,*,#16462,.F.);
#23075=ORIENTED_EDGE('',*,*,#16287,.F.);
#23076=ORIENTED_EDGE('',*,*,#16461,.T.);
#23077=ORIENTED_EDGE('',*,*,#16463,.T.);
#23078=ORIENTED_EDGE('',*,*,#16464,.F.);
#23079=ORIENTED_EDGE('',*,*,#16463,.F.);
#23080=ORIENTED_EDGE('',*,*,#16460,.F.);
#23081=ORIENTED_EDGE('',*,*,#16465,.F.);
#23082=ORIENTED_EDGE('',*,*,#16466,.T.);
#23083=ORIENTED_EDGE('',*,*,#16467,.F.);
#23084=ORIENTED_EDGE('',*,*,#16289,.F.);
#23085=ORIENTED_EDGE('',*,*,#16468,.F.);
#23086=ORIENTED_EDGE('',*,*,#16290,.F.);
#23087=ORIENTED_EDGE('',*,*,#16467,.T.);
#23088=ORIENTED_EDGE('',*,*,#16469,.T.);
#23089=ORIENTED_EDGE('',*,*,#16470,.F.);
#23090=ORIENTED_EDGE('',*,*,#16469,.F.);
#23091=ORIENTED_EDGE('',*,*,#16466,.F.);
#23092=ORIENTED_EDGE('',*,*,#16471,.F.);
#23093=ORIENTED_EDGE('',*,*,#16472,.T.);
#23094=ORIENTED_EDGE('',*,*,#16473,.F.);
#23095=ORIENTED_EDGE('',*,*,#16292,.F.);
#23096=ORIENTED_EDGE('',*,*,#16474,.F.);
#23097=ORIENTED_EDGE('',*,*,#16293,.F.);
#23098=ORIENTED_EDGE('',*,*,#16473,.T.);
#23099=ORIENTED_EDGE('',*,*,#16475,.T.);
#23100=ORIENTED_EDGE('',*,*,#16476,.F.);
#23101=ORIENTED_EDGE('',*,*,#16475,.F.);
#23102=ORIENTED_EDGE('',*,*,#16472,.F.);
#23103=ORIENTED_EDGE('',*,*,#16477,.F.);
#23104=ORIENTED_EDGE('',*,*,#16478,.T.);
#23105=ORIENTED_EDGE('',*,*,#16479,.F.);
#23106=ORIENTED_EDGE('',*,*,#16295,.F.);
#23107=ORIENTED_EDGE('',*,*,#16480,.F.);
#23108=ORIENTED_EDGE('',*,*,#16296,.F.);
#23109=ORIENTED_EDGE('',*,*,#16479,.T.);
#23110=ORIENTED_EDGE('',*,*,#16481,.T.);
#23111=ORIENTED_EDGE('',*,*,#16482,.F.);
#23112=ORIENTED_EDGE('',*,*,#16481,.F.);
#23113=ORIENTED_EDGE('',*,*,#16478,.F.);
#23114=ORIENTED_EDGE('',*,*,#16483,.F.);
#23115=ORIENTED_EDGE('',*,*,#16484,.T.);
#23116=ORIENTED_EDGE('',*,*,#16485,.F.);
#23117=ORIENTED_EDGE('',*,*,#16298,.F.);
#23118=ORIENTED_EDGE('',*,*,#16486,.F.);
#23119=ORIENTED_EDGE('',*,*,#16299,.F.);
#23120=ORIENTED_EDGE('',*,*,#16485,.T.);
#23121=ORIENTED_EDGE('',*,*,#16487,.T.);
#23122=ORIENTED_EDGE('',*,*,#16488,.F.);
#23123=ORIENTED_EDGE('',*,*,#16487,.F.);
#23124=ORIENTED_EDGE('',*,*,#16484,.F.);
#23125=ORIENTED_EDGE('',*,*,#16489,.F.);
#23126=ORIENTED_EDGE('',*,*,#16490,.T.);
#23127=ORIENTED_EDGE('',*,*,#16491,.F.);
#23128=ORIENTED_EDGE('',*,*,#16301,.F.);
#23129=ORIENTED_EDGE('',*,*,#16492,.F.);
#23130=ORIENTED_EDGE('',*,*,#16302,.F.);
#23131=ORIENTED_EDGE('',*,*,#16491,.T.);
#23132=ORIENTED_EDGE('',*,*,#16493,.T.);
#23133=ORIENTED_EDGE('',*,*,#16494,.F.);
#23134=ORIENTED_EDGE('',*,*,#16493,.F.);
#23135=ORIENTED_EDGE('',*,*,#16490,.F.);
#23136=ORIENTED_EDGE('',*,*,#16495,.F.);
#23137=ORIENTED_EDGE('',*,*,#16496,.T.);
#23138=ORIENTED_EDGE('',*,*,#16497,.F.);
#23139=ORIENTED_EDGE('',*,*,#16304,.F.);
#23140=ORIENTED_EDGE('',*,*,#16498,.F.);
#23141=ORIENTED_EDGE('',*,*,#16305,.F.);
#23142=ORIENTED_EDGE('',*,*,#16497,.T.);
#23143=ORIENTED_EDGE('',*,*,#16499,.T.);
#23144=ORIENTED_EDGE('',*,*,#16500,.F.);
#23145=ORIENTED_EDGE('',*,*,#16499,.F.);
#23146=ORIENTED_EDGE('',*,*,#16496,.F.);
#23147=ORIENTED_EDGE('',*,*,#16501,.F.);
#23148=ORIENTED_EDGE('',*,*,#16502,.T.);
#23149=ORIENTED_EDGE('',*,*,#16503,.F.);
#23150=ORIENTED_EDGE('',*,*,#16307,.F.);
#23151=ORIENTED_EDGE('',*,*,#16504,.F.);
#23152=ORIENTED_EDGE('',*,*,#16308,.F.);
#23153=ORIENTED_EDGE('',*,*,#16503,.T.);
#23154=ORIENTED_EDGE('',*,*,#16505,.T.);
#23155=ORIENTED_EDGE('',*,*,#16506,.F.);
#23156=ORIENTED_EDGE('',*,*,#16505,.F.);
#23157=ORIENTED_EDGE('',*,*,#16502,.F.);
#23158=ORIENTED_EDGE('',*,*,#16507,.F.);
#23159=ORIENTED_EDGE('',*,*,#16508,.T.);
#23160=ORIENTED_EDGE('',*,*,#16509,.F.);
#23161=ORIENTED_EDGE('',*,*,#16310,.F.);
#23162=ORIENTED_EDGE('',*,*,#16510,.F.);
#23163=ORIENTED_EDGE('',*,*,#16311,.F.);
#23164=ORIENTED_EDGE('',*,*,#16509,.T.);
#23165=ORIENTED_EDGE('',*,*,#16511,.T.);
#23166=ORIENTED_EDGE('',*,*,#16512,.F.);
#23167=ORIENTED_EDGE('',*,*,#16511,.F.);
#23168=ORIENTED_EDGE('',*,*,#16508,.F.);
#23169=ORIENTED_EDGE('',*,*,#16513,.F.);
#23170=ORIENTED_EDGE('',*,*,#16514,.T.);
#23171=ORIENTED_EDGE('',*,*,#16515,.F.);
#23172=ORIENTED_EDGE('',*,*,#16313,.F.);
#23173=ORIENTED_EDGE('',*,*,#16516,.F.);
#23174=ORIENTED_EDGE('',*,*,#16314,.F.);
#23175=ORIENTED_EDGE('',*,*,#16515,.T.);
#23176=ORIENTED_EDGE('',*,*,#16517,.T.);
#23177=ORIENTED_EDGE('',*,*,#16518,.F.);
#23178=ORIENTED_EDGE('',*,*,#16517,.F.);
#23179=ORIENTED_EDGE('',*,*,#16514,.F.);
#23180=ORIENTED_EDGE('',*,*,#16519,.F.);
#23181=ORIENTED_EDGE('',*,*,#16520,.T.);
#23182=ORIENTED_EDGE('',*,*,#16521,.F.);
#23183=ORIENTED_EDGE('',*,*,#16316,.F.);
#23184=ORIENTED_EDGE('',*,*,#16522,.F.);
#23185=ORIENTED_EDGE('',*,*,#16317,.F.);
#23186=ORIENTED_EDGE('',*,*,#16521,.T.);
#23187=ORIENTED_EDGE('',*,*,#16523,.T.);
#23188=ORIENTED_EDGE('',*,*,#16524,.F.);
#23189=ORIENTED_EDGE('',*,*,#16523,.F.);
#23190=ORIENTED_EDGE('',*,*,#16520,.F.);
#23191=ORIENTED_EDGE('',*,*,#16525,.F.);
#23192=ORIENTED_EDGE('',*,*,#16526,.T.);
#23193=ORIENTED_EDGE('',*,*,#16527,.F.);
#23194=ORIENTED_EDGE('',*,*,#16319,.F.);
#23195=ORIENTED_EDGE('',*,*,#16528,.F.);
#23196=ORIENTED_EDGE('',*,*,#16320,.F.);
#23197=ORIENTED_EDGE('',*,*,#16527,.T.);
#23198=ORIENTED_EDGE('',*,*,#16529,.T.);
#23199=ORIENTED_EDGE('',*,*,#16530,.F.);
#23200=ORIENTED_EDGE('',*,*,#16529,.F.);
#23201=ORIENTED_EDGE('',*,*,#16526,.F.);
#23202=ORIENTED_EDGE('',*,*,#16531,.F.);
#23203=ORIENTED_EDGE('',*,*,#16532,.T.);
#23204=ORIENTED_EDGE('',*,*,#16533,.F.);
#23205=ORIENTED_EDGE('',*,*,#16322,.F.);
#23206=ORIENTED_EDGE('',*,*,#16534,.F.);
#23207=ORIENTED_EDGE('',*,*,#16323,.F.);
#23208=ORIENTED_EDGE('',*,*,#16533,.T.);
#23209=ORIENTED_EDGE('',*,*,#16535,.T.);
#23210=ORIENTED_EDGE('',*,*,#16536,.F.);
#23211=ORIENTED_EDGE('',*,*,#16535,.F.);
#23212=ORIENTED_EDGE('',*,*,#16532,.F.);
#23213=ORIENTED_EDGE('',*,*,#16537,.F.);
#23214=ORIENTED_EDGE('',*,*,#16538,.T.);
#23215=ORIENTED_EDGE('',*,*,#16539,.F.);
#23216=ORIENTED_EDGE('',*,*,#16325,.F.);
#23217=ORIENTED_EDGE('',*,*,#16540,.F.);
#23218=ORIENTED_EDGE('',*,*,#16326,.F.);
#23219=ORIENTED_EDGE('',*,*,#16539,.T.);
#23220=ORIENTED_EDGE('',*,*,#16541,.T.);
#23221=ORIENTED_EDGE('',*,*,#16542,.F.);
#23222=ORIENTED_EDGE('',*,*,#16541,.F.);
#23223=ORIENTED_EDGE('',*,*,#16538,.F.);
#23224=ORIENTED_EDGE('',*,*,#16543,.F.);
#23225=ORIENTED_EDGE('',*,*,#16544,.T.);
#23226=ORIENTED_EDGE('',*,*,#16545,.F.);
#23227=ORIENTED_EDGE('',*,*,#16328,.F.);
#23228=ORIENTED_EDGE('',*,*,#16546,.F.);
#23229=ORIENTED_EDGE('',*,*,#16329,.F.);
#23230=ORIENTED_EDGE('',*,*,#16545,.T.);
#23231=ORIENTED_EDGE('',*,*,#16547,.T.);
#23232=ORIENTED_EDGE('',*,*,#16548,.F.);
#23233=ORIENTED_EDGE('',*,*,#16547,.F.);
#23234=ORIENTED_EDGE('',*,*,#16544,.F.);
#23235=ORIENTED_EDGE('',*,*,#16549,.F.);
#23236=ORIENTED_EDGE('',*,*,#16550,.T.);
#23237=ORIENTED_EDGE('',*,*,#16551,.F.);
#23238=ORIENTED_EDGE('',*,*,#16331,.F.);
#23239=ORIENTED_EDGE('',*,*,#16552,.F.);
#23240=ORIENTED_EDGE('',*,*,#16332,.F.);
#23241=ORIENTED_EDGE('',*,*,#16551,.T.);
#23242=ORIENTED_EDGE('',*,*,#16553,.T.);
#23243=ORIENTED_EDGE('',*,*,#16554,.F.);
#23244=ORIENTED_EDGE('',*,*,#16553,.F.);
#23245=ORIENTED_EDGE('',*,*,#16550,.F.);
#23246=ORIENTED_EDGE('',*,*,#16555,.F.);
#23247=ORIENTED_EDGE('',*,*,#16556,.T.);
#23248=ORIENTED_EDGE('',*,*,#16557,.F.);
#23249=ORIENTED_EDGE('',*,*,#16334,.F.);
#23250=ORIENTED_EDGE('',*,*,#16558,.F.);
#23251=ORIENTED_EDGE('',*,*,#16335,.F.);
#23252=ORIENTED_EDGE('',*,*,#16557,.T.);
#23253=ORIENTED_EDGE('',*,*,#16559,.T.);
#23254=ORIENTED_EDGE('',*,*,#16560,.F.);
#23255=ORIENTED_EDGE('',*,*,#16559,.F.);
#23256=ORIENTED_EDGE('',*,*,#16556,.F.);
#23257=ORIENTED_EDGE('',*,*,#16561,.F.);
#23258=ORIENTED_EDGE('',*,*,#16562,.T.);
#23259=ORIENTED_EDGE('',*,*,#16563,.F.);
#23260=ORIENTED_EDGE('',*,*,#16337,.F.);
#23261=ORIENTED_EDGE('',*,*,#16564,.F.);
#23262=ORIENTED_EDGE('',*,*,#16338,.F.);
#23263=ORIENTED_EDGE('',*,*,#16563,.T.);
#23264=ORIENTED_EDGE('',*,*,#16565,.T.);
#23265=ORIENTED_EDGE('',*,*,#16566,.F.);
#23266=ORIENTED_EDGE('',*,*,#16565,.F.);
#23267=ORIENTED_EDGE('',*,*,#16562,.F.);
#23268=ORIENTED_EDGE('',*,*,#16567,.F.);
#23269=ORIENTED_EDGE('',*,*,#16568,.T.);
#23270=ORIENTED_EDGE('',*,*,#16569,.F.);
#23271=ORIENTED_EDGE('',*,*,#16340,.F.);
#23272=ORIENTED_EDGE('',*,*,#16570,.F.);
#23273=ORIENTED_EDGE('',*,*,#16341,.F.);
#23274=ORIENTED_EDGE('',*,*,#16569,.T.);
#23275=ORIENTED_EDGE('',*,*,#16571,.T.);
#23276=ORIENTED_EDGE('',*,*,#16572,.F.);
#23277=ORIENTED_EDGE('',*,*,#16571,.F.);
#23278=ORIENTED_EDGE('',*,*,#16568,.F.);
#23279=ORIENTED_EDGE('',*,*,#16573,.F.);
#23280=ORIENTED_EDGE('',*,*,#16574,.T.);
#23281=ORIENTED_EDGE('',*,*,#16575,.F.);
#23282=ORIENTED_EDGE('',*,*,#16343,.F.);
#23283=ORIENTED_EDGE('',*,*,#16576,.F.);
#23284=ORIENTED_EDGE('',*,*,#16344,.F.);
#23285=ORIENTED_EDGE('',*,*,#16575,.T.);
#23286=ORIENTED_EDGE('',*,*,#16577,.T.);
#23287=ORIENTED_EDGE('',*,*,#16578,.F.);
#23288=ORIENTED_EDGE('',*,*,#16577,.F.);
#23289=ORIENTED_EDGE('',*,*,#16574,.F.);
#23290=ORIENTED_EDGE('',*,*,#16579,.F.);
#23291=ORIENTED_EDGE('',*,*,#16580,.T.);
#23292=ORIENTED_EDGE('',*,*,#16581,.F.);
#23293=ORIENTED_EDGE('',*,*,#16346,.F.);
#23294=ORIENTED_EDGE('',*,*,#16582,.F.);
#23295=ORIENTED_EDGE('',*,*,#16347,.F.);
#23296=ORIENTED_EDGE('',*,*,#16581,.T.);
#23297=ORIENTED_EDGE('',*,*,#16583,.T.);
#23298=ORIENTED_EDGE('',*,*,#16584,.F.);
#23299=ORIENTED_EDGE('',*,*,#16583,.F.);
#23300=ORIENTED_EDGE('',*,*,#16580,.F.);
#23301=ORIENTED_EDGE('',*,*,#16421,.T.);
#23302=ORIENTED_EDGE('',*,*,#16585,.T.);
#23303=ORIENTED_EDGE('',*,*,#16255,.T.);
#23304=ORIENTED_EDGE('',*,*,#16585,.F.);
#23305=ORIENTED_EDGE('',*,*,#16422,.T.);
#23306=ORIENTED_EDGE('',*,*,#16416,.T.);
#23307=ORIENTED_EDGE('',*,*,#16370,.F.);
#23308=ORIENTED_EDGE('',*,*,#16413,.T.);
#23309=ORIENTED_EDGE('',*,*,#16415,.T.);
#23310=ORIENTED_EDGE('',*,*,#16410,.T.);
#23311=ORIENTED_EDGE('',*,*,#16367,.F.);
#23312=ORIENTED_EDGE('',*,*,#16407,.T.);
#23313=ORIENTED_EDGE('',*,*,#16409,.T.);
#23314=ORIENTED_EDGE('',*,*,#16404,.T.);
#23315=ORIENTED_EDGE('',*,*,#16364,.F.);
#23316=ORIENTED_EDGE('',*,*,#16401,.T.);
#23317=ORIENTED_EDGE('',*,*,#16403,.T.);
#23318=ORIENTED_EDGE('',*,*,#16398,.T.);
#23319=ORIENTED_EDGE('',*,*,#16361,.F.);
#23320=ORIENTED_EDGE('',*,*,#16395,.T.);
#23321=ORIENTED_EDGE('',*,*,#16397,.T.);
#23322=ORIENTED_EDGE('',*,*,#16392,.T.);
#23323=ORIENTED_EDGE('',*,*,#16358,.F.);
#23324=ORIENTED_EDGE('',*,*,#16389,.T.);
#23325=ORIENTED_EDGE('',*,*,#16391,.T.);
#23326=ORIENTED_EDGE('',*,*,#16386,.T.);
#23327=ORIENTED_EDGE('',*,*,#16355,.F.);
#23328=ORIENTED_EDGE('',*,*,#16383,.T.);
#23329=ORIENTED_EDGE('',*,*,#16385,.T.);
#23330=ORIENTED_EDGE('',*,*,#16380,.T.);
#23331=ORIENTED_EDGE('',*,*,#16352,.F.);
#23332=ORIENTED_EDGE('',*,*,#16377,.T.);
#23333=ORIENTED_EDGE('',*,*,#16379,.T.);
#23334=ORIENTED_EDGE('',*,*,#16374,.T.);
#23335=ORIENTED_EDGE('',*,*,#16349,.F.);
#23336=ORIENTED_EDGE('',*,*,#16262,.T.);
#23337=ORIENTED_EDGE('',*,*,#16265,.T.);
#23338=ORIENTED_EDGE('',*,*,#16258,.T.);
#23339=ORIENTED_EDGE('',*,*,#16348,.F.);
#23340=ORIENTED_EDGE('',*,*,#16582,.T.);
#23341=ORIENTED_EDGE('',*,*,#16584,.T.);
#23342=ORIENTED_EDGE('',*,*,#16579,.T.);
#23343=ORIENTED_EDGE('',*,*,#16345,.F.);
#23344=ORIENTED_EDGE('',*,*,#16576,.T.);
#23345=ORIENTED_EDGE('',*,*,#16578,.T.);
#23346=ORIENTED_EDGE('',*,*,#16573,.T.);
#23347=ORIENTED_EDGE('',*,*,#16342,.F.);
#23348=ORIENTED_EDGE('',*,*,#16570,.T.);
#23349=ORIENTED_EDGE('',*,*,#16572,.T.);
#23350=ORIENTED_EDGE('',*,*,#16567,.T.);
#23351=ORIENTED_EDGE('',*,*,#16339,.F.);
#23352=ORIENTED_EDGE('',*,*,#16564,.T.);
#23353=ORIENTED_EDGE('',*,*,#16566,.T.);
#23354=ORIENTED_EDGE('',*,*,#16561,.T.);
#23355=ORIENTED_EDGE('',*,*,#16336,.F.);
#23356=ORIENTED_EDGE('',*,*,#16558,.T.);
#23357=ORIENTED_EDGE('',*,*,#16560,.T.);
#23358=ORIENTED_EDGE('',*,*,#16555,.T.);
#23359=ORIENTED_EDGE('',*,*,#16333,.F.);
#23360=ORIENTED_EDGE('',*,*,#16552,.T.);
#23361=ORIENTED_EDGE('',*,*,#16554,.T.);
#23362=ORIENTED_EDGE('',*,*,#16549,.T.);
#23363=ORIENTED_EDGE('',*,*,#16330,.F.);
#23364=ORIENTED_EDGE('',*,*,#16546,.T.);
#23365=ORIENTED_EDGE('',*,*,#16548,.T.);
#23366=ORIENTED_EDGE('',*,*,#16543,.T.);
#23367=ORIENTED_EDGE('',*,*,#16327,.F.);
#23368=ORIENTED_EDGE('',*,*,#16540,.T.);
#23369=ORIENTED_EDGE('',*,*,#16542,.T.);
#23370=ORIENTED_EDGE('',*,*,#16537,.T.);
#23371=ORIENTED_EDGE('',*,*,#16324,.F.);
#23372=ORIENTED_EDGE('',*,*,#16534,.T.);
#23373=ORIENTED_EDGE('',*,*,#16536,.T.);
#23374=ORIENTED_EDGE('',*,*,#16531,.T.);
#23375=ORIENTED_EDGE('',*,*,#16321,.F.);
#23376=ORIENTED_EDGE('',*,*,#16528,.T.);
#23377=ORIENTED_EDGE('',*,*,#16530,.T.);
#23378=ORIENTED_EDGE('',*,*,#16525,.T.);
#23379=ORIENTED_EDGE('',*,*,#16318,.F.);
#23380=ORIENTED_EDGE('',*,*,#16522,.T.);
#23381=ORIENTED_EDGE('',*,*,#16524,.T.);
#23382=ORIENTED_EDGE('',*,*,#16519,.T.);
#23383=ORIENTED_EDGE('',*,*,#16315,.F.);
#23384=ORIENTED_EDGE('',*,*,#16516,.T.);
#23385=ORIENTED_EDGE('',*,*,#16518,.T.);
#23386=ORIENTED_EDGE('',*,*,#16513,.T.);
#23387=ORIENTED_EDGE('',*,*,#16312,.F.);
#23388=ORIENTED_EDGE('',*,*,#16510,.T.);
#23389=ORIENTED_EDGE('',*,*,#16512,.T.);
#23390=ORIENTED_EDGE('',*,*,#16507,.T.);
#23391=ORIENTED_EDGE('',*,*,#16309,.F.);
#23392=ORIENTED_EDGE('',*,*,#16504,.T.);
#23393=ORIENTED_EDGE('',*,*,#16506,.T.);
#23394=ORIENTED_EDGE('',*,*,#16501,.T.);
#23395=ORIENTED_EDGE('',*,*,#16306,.F.);
#23396=ORIENTED_EDGE('',*,*,#16498,.T.);
#23397=ORIENTED_EDGE('',*,*,#16500,.T.);
#23398=ORIENTED_EDGE('',*,*,#16495,.T.);
#23399=ORIENTED_EDGE('',*,*,#16303,.F.);
#23400=ORIENTED_EDGE('',*,*,#16492,.T.);
#23401=ORIENTED_EDGE('',*,*,#16494,.T.);
#23402=ORIENTED_EDGE('',*,*,#16489,.T.);
#23403=ORIENTED_EDGE('',*,*,#16300,.F.);
#23404=ORIENTED_EDGE('',*,*,#16486,.T.);
#23405=ORIENTED_EDGE('',*,*,#16488,.T.);
#23406=ORIENTED_EDGE('',*,*,#16483,.T.);
#23407=ORIENTED_EDGE('',*,*,#16297,.F.);
#23408=ORIENTED_EDGE('',*,*,#16480,.T.);
#23409=ORIENTED_EDGE('',*,*,#16482,.T.);
#23410=ORIENTED_EDGE('',*,*,#16477,.T.);
#23411=ORIENTED_EDGE('',*,*,#16294,.F.);
#23412=ORIENTED_EDGE('',*,*,#16474,.T.);
#23413=ORIENTED_EDGE('',*,*,#16476,.T.);
#23414=ORIENTED_EDGE('',*,*,#16471,.T.);
#23415=ORIENTED_EDGE('',*,*,#16291,.F.);
#23416=ORIENTED_EDGE('',*,*,#16468,.T.);
#23417=ORIENTED_EDGE('',*,*,#16470,.T.);
#23418=ORIENTED_EDGE('',*,*,#16465,.T.);
#23419=ORIENTED_EDGE('',*,*,#16288,.F.);
#23420=ORIENTED_EDGE('',*,*,#16462,.T.);
#23421=ORIENTED_EDGE('',*,*,#16464,.T.);
#23422=ORIENTED_EDGE('',*,*,#16459,.T.);
#23423=ORIENTED_EDGE('',*,*,#16285,.F.);
#23424=ORIENTED_EDGE('',*,*,#16456,.T.);
#23425=ORIENTED_EDGE('',*,*,#16458,.T.);
#23426=ORIENTED_EDGE('',*,*,#16453,.T.);
#23427=ORIENTED_EDGE('',*,*,#16282,.F.);
#23428=ORIENTED_EDGE('',*,*,#16450,.T.);
#23429=ORIENTED_EDGE('',*,*,#16452,.T.);
#23430=ORIENTED_EDGE('',*,*,#16447,.T.);
#23431=ORIENTED_EDGE('',*,*,#16279,.F.);
#23432=ORIENTED_EDGE('',*,*,#16444,.T.);
#23433=ORIENTED_EDGE('',*,*,#16446,.T.);
#23434=ORIENTED_EDGE('',*,*,#16441,.T.);
#23435=ORIENTED_EDGE('',*,*,#16276,.F.);
#23436=ORIENTED_EDGE('',*,*,#16438,.T.);
#23437=ORIENTED_EDGE('',*,*,#16440,.T.);
#23438=ORIENTED_EDGE('',*,*,#16435,.T.);
#23439=ORIENTED_EDGE('',*,*,#16273,.F.);
#23440=ORIENTED_EDGE('',*,*,#16432,.T.);
#23441=ORIENTED_EDGE('',*,*,#16434,.T.);
#23442=ORIENTED_EDGE('',*,*,#16429,.T.);
#23443=ORIENTED_EDGE('',*,*,#16270,.F.);
#23444=ORIENTED_EDGE('',*,*,#16426,.T.);
#23445=ORIENTED_EDGE('',*,*,#16428,.T.);
#23446=ORIENTED_EDGE('',*,*,#16423,.T.);
#23447=ORIENTED_EDGE('',*,*,#16267,.F.);
#23448=ORIENTED_EDGE('',*,*,#16419,.T.);
#23449=ORIENTED_EDGE('',*,*,#16373,.F.);
#23450=ORIENTED_EDGE('',*,*,#16586,.T.);
#23451=ORIENTED_EDGE('',*,*,#16587,.T.);
#23452=ORIENTED_EDGE('',*,*,#16588,.T.);
#23453=ORIENTED_EDGE('',*,*,#16589,.T.);
#23454=ORIENTED_EDGE('',*,*,#16590,.T.);
#23455=ORIENTED_EDGE('',*,*,#16591,.T.);
#23456=ORIENTED_EDGE('',*,*,#16592,.F.);
#23457=ORIENTED_EDGE('',*,*,#16593,.F.);
#23458=ORIENTED_EDGE('',*,*,#16594,.F.);
#23459=ORIENTED_EDGE('',*,*,#16595,.F.);
#23460=ORIENTED_EDGE('',*,*,#16596,.F.);
#23461=ORIENTED_EDGE('',*,*,#16597,.F.);
#23462=ORIENTED_EDGE('',*,*,#16598,.F.);
#23463=ORIENTED_EDGE('',*,*,#16599,.F.);
#23464=ORIENTED_EDGE('',*,*,#16600,.F.);
#23465=ORIENTED_EDGE('',*,*,#16601,.F.);
#23466=ORIENTED_EDGE('',*,*,#16602,.F.);
#23467=ORIENTED_EDGE('',*,*,#16603,.F.);
#23468=ORIENTED_EDGE('',*,*,#16604,.T.);
#23469=ORIENTED_EDGE('',*,*,#16599,.T.);
#23470=ORIENTED_EDGE('',*,*,#16597,.T.);
#23471=ORIENTED_EDGE('',*,*,#16595,.T.);
#23472=ORIENTED_EDGE('',*,*,#16593,.T.);
#23473=ORIENTED_EDGE('',*,*,#16603,.T.);
#23474=ORIENTED_EDGE('',*,*,#16601,.T.);
#23475=ORIENTED_EDGE('',*,*,#16604,.F.);
#23476=ORIENTED_EDGE('',*,*,#16586,.F.);
#23477=ORIENTED_EDGE('',*,*,#16605,.T.);
#23478=ORIENTED_EDGE('',*,*,#16592,.T.);
#23479=ORIENTED_EDGE('',*,*,#16606,.F.);
#23480=ORIENTED_EDGE('',*,*,#16591,.F.);
#23481=ORIENTED_EDGE('',*,*,#16607,.T.);
#23482=ORIENTED_EDGE('',*,*,#16602,.T.);
#23483=ORIENTED_EDGE('',*,*,#16605,.F.);
#23484=ORIENTED_EDGE('',*,*,#16590,.F.);
#23485=ORIENTED_EDGE('',*,*,#16608,.T.);
#23486=ORIENTED_EDGE('',*,*,#16600,.T.);
#23487=ORIENTED_EDGE('',*,*,#16607,.F.);
#23488=ORIENTED_EDGE('',*,*,#16589,.F.);
#23489=ORIENTED_EDGE('',*,*,#16609,.T.);
#23490=ORIENTED_EDGE('',*,*,#16598,.T.);
#23491=ORIENTED_EDGE('',*,*,#16608,.F.);
#23492=ORIENTED_EDGE('',*,*,#16588,.F.);
#23493=ORIENTED_EDGE('',*,*,#16610,.T.);
#23494=ORIENTED_EDGE('',*,*,#16596,.T.);
#23495=ORIENTED_EDGE('',*,*,#16609,.F.);
#23496=ORIENTED_EDGE('',*,*,#16587,.F.);
#23497=ORIENTED_EDGE('',*,*,#16606,.T.);
#23498=ORIENTED_EDGE('',*,*,#16594,.T.);
#23499=ORIENTED_EDGE('',*,*,#16610,.F.);
#23500=ORIENTED_EDGE('',*,*,#16611,.F.);
#23501=ORIENTED_EDGE('',*,*,#16612,.F.);
#23502=ORIENTED_EDGE('',*,*,#16613,.F.);
#23503=ORIENTED_EDGE('',*,*,#16614,.T.);
#23504=ORIENTED_EDGE('',*,*,#16615,.F.);
#23505=ORIENTED_EDGE('',*,*,#16616,.F.);
#23506=ORIENTED_EDGE('',*,*,#16617,.F.);
#23507=ORIENTED_EDGE('',*,*,#16611,.T.);
#23508=ORIENTED_EDGE('',*,*,#16618,.T.);
#23509=ORIENTED_EDGE('',*,*,#16619,.T.);
#23510=ORIENTED_EDGE('',*,*,#16620,.F.);
#23511=ORIENTED_EDGE('',*,*,#16621,.F.);
#23512=ORIENTED_EDGE('',*,*,#16622,.F.);
#23513=ORIENTED_EDGE('',*,*,#16615,.T.);
#23514=ORIENTED_EDGE('',*,*,#16623,.T.);
#23515=ORIENTED_EDGE('',*,*,#16624,.F.);
#23516=ORIENTED_EDGE('',*,*,#16625,.F.);
#23517=ORIENTED_EDGE('',*,*,#16626,.F.);
#23518=ORIENTED_EDGE('',*,*,#16620,.T.);
#23519=ORIENTED_EDGE('',*,*,#16627,.T.);
#23520=ORIENTED_EDGE('',*,*,#16628,.T.);
#23521=ORIENTED_EDGE('',*,*,#16629,.F.);
#23522=ORIENTED_EDGE('',*,*,#16630,.F.);
#23523=ORIENTED_EDGE('',*,*,#16631,.F.);
#23524=ORIENTED_EDGE('',*,*,#16624,.T.);
#23525=ORIENTED_EDGE('',*,*,#16632,.T.);
#23526=ORIENTED_EDGE('',*,*,#16633,.T.);
#23527=ORIENTED_EDGE('',*,*,#16634,.F.);
#23528=ORIENTED_EDGE('',*,*,#16635,.F.);
#23529=ORIENTED_EDGE('',*,*,#16636,.F.);
#23530=ORIENTED_EDGE('',*,*,#16629,.T.);
#23531=ORIENTED_EDGE('',*,*,#16637,.T.);
#23532=ORIENTED_EDGE('',*,*,#16638,.F.);
#23533=ORIENTED_EDGE('',*,*,#16639,.F.);
#23534=ORIENTED_EDGE('',*,*,#16634,.T.);
#23535=ORIENTED_EDGE('',*,*,#16640,.T.);
#23536=ORIENTED_EDGE('',*,*,#16641,.T.);
#23537=ORIENTED_EDGE('',*,*,#16642,.F.);
#23538=ORIENTED_EDGE('',*,*,#16643,.F.);
#23539=ORIENTED_EDGE('',*,*,#16644,.F.);
#23540=ORIENTED_EDGE('',*,*,#16638,.T.);
#23541=ORIENTED_EDGE('',*,*,#16645,.T.);
#23542=ORIENTED_EDGE('',*,*,#16646,.F.);
#23543=ORIENTED_EDGE('',*,*,#16647,.F.);
#23544=ORIENTED_EDGE('',*,*,#16642,.T.);
#23545=ORIENTED_EDGE('',*,*,#16648,.T.);
#23546=ORIENTED_EDGE('',*,*,#16649,.T.);
#23547=ORIENTED_EDGE('',*,*,#16650,.T.);
#23548=ORIENTED_EDGE('',*,*,#16651,.F.);
#23549=ORIENTED_EDGE('',*,*,#16652,.T.);
#23550=ORIENTED_EDGE('',*,*,#16653,.T.);
#23551=ORIENTED_EDGE('',*,*,#16654,.T.);
#23552=ORIENTED_EDGE('',*,*,#16655,.T.);
#23553=ORIENTED_EDGE('',*,*,#16656,.T.);
#23554=ORIENTED_EDGE('',*,*,#16657,.T.);
#23555=ORIENTED_EDGE('',*,*,#16658,.T.);
#23556=ORIENTED_EDGE('',*,*,#16659,.T.);
#23557=ORIENTED_EDGE('',*,*,#16660,.T.);
#23558=ORIENTED_EDGE('',*,*,#16661,.T.);
#23559=ORIENTED_EDGE('',*,*,#16662,.T.);
#23560=ORIENTED_EDGE('',*,*,#16663,.F.);
#23561=ORIENTED_EDGE('',*,*,#16664,.T.);
#23562=ORIENTED_EDGE('',*,*,#16665,.T.);
#23563=ORIENTED_EDGE('',*,*,#16666,.T.);
#23564=ORIENTED_EDGE('',*,*,#16667,.T.);
#23565=ORIENTED_EDGE('',*,*,#16668,.T.);
#23566=ORIENTED_EDGE('',*,*,#16669,.T.);
#23567=ORIENTED_EDGE('',*,*,#16670,.T.);
#23568=ORIENTED_EDGE('',*,*,#16671,.T.);
#23569=ORIENTED_EDGE('',*,*,#16672,.T.);
#23570=ORIENTED_EDGE('',*,*,#16673,.T.);
#23571=ORIENTED_EDGE('',*,*,#16646,.T.);
#23572=ORIENTED_EDGE('',*,*,#16674,.T.);
#23573=ORIENTED_EDGE('',*,*,#16675,.T.);
#23574=ORIENTED_EDGE('',*,*,#16676,.F.);
#23575=ORIENTED_EDGE('',*,*,#16677,.F.);
#23576=ORIENTED_EDGE('',*,*,#16678,.F.);
#23577=ORIENTED_EDGE('',*,*,#16679,.F.);
#23578=ORIENTED_EDGE('',*,*,#16680,.T.);
#23579=ORIENTED_EDGE('',*,*,#16676,.T.);
#23580=ORIENTED_EDGE('',*,*,#16681,.T.);
#23581=ORIENTED_EDGE('',*,*,#16682,.F.);
#23582=ORIENTED_EDGE('',*,*,#16680,.F.);
#23583=ORIENTED_EDGE('',*,*,#16683,.F.);
#23584=ORIENTED_EDGE('',*,*,#16662,.F.);
#23585=ORIENTED_EDGE('',*,*,#16661,.F.);
#23586=ORIENTED_EDGE('',*,*,#16660,.F.);
#23587=ORIENTED_EDGE('',*,*,#16659,.F.);
#23588=ORIENTED_EDGE('',*,*,#16658,.F.);
#23589=ORIENTED_EDGE('',*,*,#16657,.F.);
#23590=ORIENTED_EDGE('',*,*,#16656,.F.);
#23591=ORIENTED_EDGE('',*,*,#16655,.F.);
#23592=ORIENTED_EDGE('',*,*,#16654,.F.);
#23593=ORIENTED_EDGE('',*,*,#16653,.F.);
#23594=ORIENTED_EDGE('',*,*,#16652,.F.);
#23595=ORIENTED_EDGE('',*,*,#16684,.F.);
#23596=ORIENTED_EDGE('',*,*,#16612,.T.);
#23597=ORIENTED_EDGE('',*,*,#16617,.T.);
#23598=ORIENTED_EDGE('',*,*,#16616,.T.);
#23599=ORIENTED_EDGE('',*,*,#16622,.T.);
#23600=ORIENTED_EDGE('',*,*,#16621,.T.);
#23601=ORIENTED_EDGE('',*,*,#16626,.T.);
#23602=ORIENTED_EDGE('',*,*,#16625,.T.);
#23603=ORIENTED_EDGE('',*,*,#16631,.T.);
#23604=ORIENTED_EDGE('',*,*,#16630,.T.);
#23605=ORIENTED_EDGE('',*,*,#16636,.T.);
#23606=ORIENTED_EDGE('',*,*,#16635,.T.);
#23607=ORIENTED_EDGE('',*,*,#16639,.T.);
#23608=ORIENTED_EDGE('',*,*,#16644,.T.);
#23609=ORIENTED_EDGE('',*,*,#16643,.T.);
#23610=ORIENTED_EDGE('',*,*,#16647,.T.);
#23611=ORIENTED_EDGE('',*,*,#16678,.T.);
#23612=ORIENTED_EDGE('',*,*,#16677,.T.);
#23613=ORIENTED_EDGE('',*,*,#16685,.F.);
#23614=ORIENTED_EDGE('',*,*,#16686,.T.);
#23615=ORIENTED_EDGE('',*,*,#16613,.T.);
#23616=ORIENTED_EDGE('',*,*,#16684,.T.);
#23617=ORIENTED_EDGE('',*,*,#16687,.F.);
#23618=ORIENTED_EDGE('',*,*,#16681,.F.);
#23619=ORIENTED_EDGE('',*,*,#16675,.F.);
#23620=ORIENTED_EDGE('',*,*,#16674,.F.);
#23621=ORIENTED_EDGE('',*,*,#16649,.F.);
#23622=ORIENTED_EDGE('',*,*,#16648,.F.);
#23623=ORIENTED_EDGE('',*,*,#16645,.F.);
#23624=ORIENTED_EDGE('',*,*,#16641,.F.);
#23625=ORIENTED_EDGE('',*,*,#16640,.F.);
#23626=ORIENTED_EDGE('',*,*,#16637,.F.);
#23627=ORIENTED_EDGE('',*,*,#16633,.F.);
#23628=ORIENTED_EDGE('',*,*,#16632,.F.);
#23629=ORIENTED_EDGE('',*,*,#16628,.F.);
#23630=ORIENTED_EDGE('',*,*,#16627,.F.);
#23631=ORIENTED_EDGE('',*,*,#16623,.F.);
#23632=ORIENTED_EDGE('',*,*,#16619,.F.);
#23633=ORIENTED_EDGE('',*,*,#16618,.F.);
#23634=ORIENTED_EDGE('',*,*,#16614,.F.);
#23635=ORIENTED_EDGE('',*,*,#16686,.F.);
#23636=ORIENTED_EDGE('',*,*,#16688,.F.);
#23637=ORIENTED_EDGE('',*,*,#16650,.F.);
#23638=ORIENTED_EDGE('',*,*,#16673,.F.);
#23639=ORIENTED_EDGE('',*,*,#16672,.F.);
#23640=ORIENTED_EDGE('',*,*,#16671,.F.);
#23641=ORIENTED_EDGE('',*,*,#16670,.F.);
#23642=ORIENTED_EDGE('',*,*,#16669,.F.);
#23643=ORIENTED_EDGE('',*,*,#16668,.F.);
#23644=ORIENTED_EDGE('',*,*,#16667,.F.);
#23645=ORIENTED_EDGE('',*,*,#16666,.F.);
#23646=ORIENTED_EDGE('',*,*,#16665,.F.);
#23647=ORIENTED_EDGE('',*,*,#16664,.F.);
#23648=ORIENTED_EDGE('',*,*,#16689,.T.);
#23649=ORIENTED_EDGE('',*,*,#16690,.T.);
#23650=ORIENTED_EDGE('',*,*,#16687,.T.);
#23651=ORIENTED_EDGE('',*,*,#16651,.T.);
#23652=ORIENTED_EDGE('',*,*,#16688,.T.);
#23653=ORIENTED_EDGE('',*,*,#16685,.T.);
#23654=ORIENTED_EDGE('',*,*,#16690,.F.);
#23655=ORIENTED_EDGE('',*,*,#16691,.F.);
#23656=ORIENTED_EDGE('',*,*,#16689,.F.);
#23657=ORIENTED_EDGE('',*,*,#16679,.T.);
#23658=ORIENTED_EDGE('',*,*,#16692,.T.);
#23659=ORIENTED_EDGE('',*,*,#16693,.T.);
#23660=ORIENTED_EDGE('',*,*,#16692,.F.);
#23661=ORIENTED_EDGE('',*,*,#16682,.T.);
#23662=ORIENTED_EDGE('',*,*,#16663,.T.);
#23663=ORIENTED_EDGE('',*,*,#16683,.T.);
#23664=ORIENTED_EDGE('',*,*,#16693,.F.);
#23665=ORIENTED_EDGE('',*,*,#16694,.F.);
#23666=ORIENTED_EDGE('',*,*,#16695,.T.);
#23667=ORIENTED_EDGE('',*,*,#16696,.F.);
#23668=ORIENTED_EDGE('',*,*,#16697,.F.);
#23669=ORIENTED_EDGE('',*,*,#16698,.F.);
#23670=ORIENTED_EDGE('',*,*,#16699,.F.);
#23671=ORIENTED_EDGE('',*,*,#16696,.T.);
#23672=ORIENTED_EDGE('',*,*,#16700,.T.);
#23673=ORIENTED_EDGE('',*,*,#16701,.F.);
#23674=ORIENTED_EDGE('',*,*,#16700,.F.);
#23675=ORIENTED_EDGE('',*,*,#16695,.F.);
#23676=ORIENTED_EDGE('',*,*,#16702,.T.);
#23677=ORIENTED_EDGE('',*,*,#16703,.T.);
#23678=ORIENTED_EDGE('',*,*,#16704,.T.);
#23679=ORIENTED_EDGE('',*,*,#16705,.T.);
#23680=ORIENTED_EDGE('',*,*,#16706,.T.);
#23681=ORIENTED_EDGE('',*,*,#16707,.T.);
#23682=ORIENTED_EDGE('',*,*,#16708,.T.);
#23683=ORIENTED_EDGE('',*,*,#16709,.T.);
#23684=ORIENTED_EDGE('',*,*,#16710,.T.);
#23685=ORIENTED_EDGE('',*,*,#16711,.T.);
#23686=ORIENTED_EDGE('',*,*,#16712,.T.);
#23687=ORIENTED_EDGE('',*,*,#16713,.T.);
#23688=ORIENTED_EDGE('',*,*,#16714,.T.);
#23689=ORIENTED_EDGE('',*,*,#16715,.T.);
#23690=ORIENTED_EDGE('',*,*,#16716,.T.);
#23691=ORIENTED_EDGE('',*,*,#16717,.T.);
#23692=ORIENTED_EDGE('',*,*,#16718,.T.);
#23693=ORIENTED_EDGE('',*,*,#16719,.T.);
#23694=ORIENTED_EDGE('',*,*,#16720,.T.);
#23695=ORIENTED_EDGE('',*,*,#16721,.T.);
#23696=ORIENTED_EDGE('',*,*,#16722,.T.);
#23697=ORIENTED_EDGE('',*,*,#16723,.T.);
#23698=ORIENTED_EDGE('',*,*,#16724,.T.);
#23699=ORIENTED_EDGE('',*,*,#16725,.T.);
#23700=ORIENTED_EDGE('',*,*,#16726,.T.);
#23701=ORIENTED_EDGE('',*,*,#16727,.T.);
#23702=ORIENTED_EDGE('',*,*,#16728,.T.);
#23703=ORIENTED_EDGE('',*,*,#16729,.T.);
#23704=ORIENTED_EDGE('',*,*,#16730,.T.);
#23705=ORIENTED_EDGE('',*,*,#16731,.T.);
#23706=ORIENTED_EDGE('',*,*,#16732,.T.);
#23707=ORIENTED_EDGE('',*,*,#16733,.T.);
#23708=ORIENTED_EDGE('',*,*,#16734,.T.);
#23709=ORIENTED_EDGE('',*,*,#16735,.T.);
#23710=ORIENTED_EDGE('',*,*,#16736,.T.);
#23711=ORIENTED_EDGE('',*,*,#16737,.T.);
#23712=ORIENTED_EDGE('',*,*,#16738,.T.);
#23713=ORIENTED_EDGE('',*,*,#16739,.T.);
#23714=ORIENTED_EDGE('',*,*,#16740,.T.);
#23715=ORIENTED_EDGE('',*,*,#16741,.T.);
#23716=ORIENTED_EDGE('',*,*,#16742,.T.);
#23717=ORIENTED_EDGE('',*,*,#16743,.T.);
#23718=ORIENTED_EDGE('',*,*,#16744,.T.);
#23719=ORIENTED_EDGE('',*,*,#16745,.T.);
#23720=ORIENTED_EDGE('',*,*,#16746,.T.);
#23721=ORIENTED_EDGE('',*,*,#16747,.T.);
#23722=ORIENTED_EDGE('',*,*,#16748,.T.);
#23723=ORIENTED_EDGE('',*,*,#16749,.T.);
#23724=ORIENTED_EDGE('',*,*,#16750,.T.);
#23725=ORIENTED_EDGE('',*,*,#16751,.T.);
#23726=ORIENTED_EDGE('',*,*,#16752,.T.);
#23727=ORIENTED_EDGE('',*,*,#16753,.T.);
#23728=ORIENTED_EDGE('',*,*,#16754,.T.);
#23729=ORIENTED_EDGE('',*,*,#16755,.T.);
#23730=ORIENTED_EDGE('',*,*,#16756,.T.);
#23731=ORIENTED_EDGE('',*,*,#16757,.T.);
#23732=ORIENTED_EDGE('',*,*,#16697,.T.);
#23733=ORIENTED_EDGE('',*,*,#16699,.T.);
#23734=ORIENTED_EDGE('',*,*,#16758,.T.);
#23735=ORIENTED_EDGE('',*,*,#16759,.T.);
#23736=ORIENTED_EDGE('',*,*,#16760,.T.);
#23737=ORIENTED_EDGE('',*,*,#16761,.T.);
#23738=ORIENTED_EDGE('',*,*,#16762,.T.);
#23739=ORIENTED_EDGE('',*,*,#16763,.T.);
#23740=ORIENTED_EDGE('',*,*,#16764,.T.);
#23741=ORIENTED_EDGE('',*,*,#16765,.T.);
#23742=ORIENTED_EDGE('',*,*,#16766,.T.);
#23743=ORIENTED_EDGE('',*,*,#16767,.T.);
#23744=ORIENTED_EDGE('',*,*,#16768,.T.);
#23745=ORIENTED_EDGE('',*,*,#16769,.T.);
#23746=ORIENTED_EDGE('',*,*,#16770,.T.);
#23747=ORIENTED_EDGE('',*,*,#16771,.T.);
#23748=ORIENTED_EDGE('',*,*,#16772,.T.);
#23749=ORIENTED_EDGE('',*,*,#16773,.T.);
#23750=ORIENTED_EDGE('',*,*,#16774,.T.);
#23751=ORIENTED_EDGE('',*,*,#16775,.T.);
#23752=ORIENTED_EDGE('',*,*,#16776,.T.);
#23753=ORIENTED_EDGE('',*,*,#16777,.T.);
#23754=ORIENTED_EDGE('',*,*,#16778,.T.);
#23755=ORIENTED_EDGE('',*,*,#16779,.T.);
#23756=ORIENTED_EDGE('',*,*,#16780,.T.);
#23757=ORIENTED_EDGE('',*,*,#16781,.T.);
#23758=ORIENTED_EDGE('',*,*,#16782,.T.);
#23759=ORIENTED_EDGE('',*,*,#16783,.T.);
#23760=ORIENTED_EDGE('',*,*,#16784,.T.);
#23761=ORIENTED_EDGE('',*,*,#16785,.T.);
#23762=ORIENTED_EDGE('',*,*,#16786,.T.);
#23763=ORIENTED_EDGE('',*,*,#16787,.T.);
#23764=ORIENTED_EDGE('',*,*,#16788,.T.);
#23765=ORIENTED_EDGE('',*,*,#16789,.T.);
#23766=ORIENTED_EDGE('',*,*,#16790,.T.);
#23767=ORIENTED_EDGE('',*,*,#16791,.T.);
#23768=ORIENTED_EDGE('',*,*,#16792,.T.);
#23769=ORIENTED_EDGE('',*,*,#16793,.T.);
#23770=ORIENTED_EDGE('',*,*,#16794,.T.);
#23771=ORIENTED_EDGE('',*,*,#16795,.T.);
#23772=ORIENTED_EDGE('',*,*,#16796,.T.);
#23773=ORIENTED_EDGE('',*,*,#16797,.T.);
#23774=ORIENTED_EDGE('',*,*,#16798,.T.);
#23775=ORIENTED_EDGE('',*,*,#16799,.T.);
#23776=ORIENTED_EDGE('',*,*,#16800,.T.);
#23777=ORIENTED_EDGE('',*,*,#16801,.T.);
#23778=ORIENTED_EDGE('',*,*,#16802,.T.);
#23779=ORIENTED_EDGE('',*,*,#16803,.T.);
#23780=ORIENTED_EDGE('',*,*,#16804,.T.);
#23781=ORIENTED_EDGE('',*,*,#16805,.T.);
#23782=ORIENTED_EDGE('',*,*,#16806,.T.);
#23783=ORIENTED_EDGE('',*,*,#16807,.T.);
#23784=ORIENTED_EDGE('',*,*,#16808,.T.);
#23785=ORIENTED_EDGE('',*,*,#16809,.T.);
#23786=ORIENTED_EDGE('',*,*,#16808,.F.);
#23787=ORIENTED_EDGE('',*,*,#16810,.F.);
#23788=ORIENTED_EDGE('',*,*,#16811,.T.);
#23789=ORIENTED_EDGE('',*,*,#16812,.F.);
#23790=ORIENTED_EDGE('',*,*,#16759,.F.);
#23791=ORIENTED_EDGE('',*,*,#16813,.F.);
#23792=ORIENTED_EDGE('',*,*,#16760,.F.);
#23793=ORIENTED_EDGE('',*,*,#16812,.T.);
#23794=ORIENTED_EDGE('',*,*,#16814,.T.);
#23795=ORIENTED_EDGE('',*,*,#16815,.F.);
#23796=ORIENTED_EDGE('',*,*,#16814,.F.);
#23797=ORIENTED_EDGE('',*,*,#16811,.F.);
#23798=ORIENTED_EDGE('',*,*,#16816,.F.);
#23799=ORIENTED_EDGE('',*,*,#16817,.T.);
#23800=ORIENTED_EDGE('',*,*,#16818,.F.);
#23801=ORIENTED_EDGE('',*,*,#16762,.F.);
#23802=ORIENTED_EDGE('',*,*,#16819,.F.);
#23803=ORIENTED_EDGE('',*,*,#16763,.F.);
#23804=ORIENTED_EDGE('',*,*,#16818,.T.);
#23805=ORIENTED_EDGE('',*,*,#16820,.T.);
#23806=ORIENTED_EDGE('',*,*,#16821,.F.);
#23807=ORIENTED_EDGE('',*,*,#16820,.F.);
#23808=ORIENTED_EDGE('',*,*,#16817,.F.);
#23809=ORIENTED_EDGE('',*,*,#16822,.F.);
#23810=ORIENTED_EDGE('',*,*,#16823,.T.);
#23811=ORIENTED_EDGE('',*,*,#16824,.F.);
#23812=ORIENTED_EDGE('',*,*,#16765,.F.);
#23813=ORIENTED_EDGE('',*,*,#16825,.F.);
#23814=ORIENTED_EDGE('',*,*,#16766,.F.);
#23815=ORIENTED_EDGE('',*,*,#16824,.T.);
#23816=ORIENTED_EDGE('',*,*,#16826,.T.);
#23817=ORIENTED_EDGE('',*,*,#16827,.F.);
#23818=ORIENTED_EDGE('',*,*,#16826,.F.);
#23819=ORIENTED_EDGE('',*,*,#16823,.F.);
#23820=ORIENTED_EDGE('',*,*,#16828,.F.);
#23821=ORIENTED_EDGE('',*,*,#16829,.T.);
#23822=ORIENTED_EDGE('',*,*,#16830,.F.);
#23823=ORIENTED_EDGE('',*,*,#16768,.F.);
#23824=ORIENTED_EDGE('',*,*,#16831,.F.);
#23825=ORIENTED_EDGE('',*,*,#16769,.F.);
#23826=ORIENTED_EDGE('',*,*,#16830,.T.);
#23827=ORIENTED_EDGE('',*,*,#16832,.T.);
#23828=ORIENTED_EDGE('',*,*,#16833,.F.);
#23829=ORIENTED_EDGE('',*,*,#16832,.F.);
#23830=ORIENTED_EDGE('',*,*,#16829,.F.);
#23831=ORIENTED_EDGE('',*,*,#16834,.F.);
#23832=ORIENTED_EDGE('',*,*,#16835,.T.);
#23833=ORIENTED_EDGE('',*,*,#16836,.F.);
#23834=ORIENTED_EDGE('',*,*,#16771,.F.);
#23835=ORIENTED_EDGE('',*,*,#16837,.F.);
#23836=ORIENTED_EDGE('',*,*,#16772,.F.);
#23837=ORIENTED_EDGE('',*,*,#16836,.T.);
#23838=ORIENTED_EDGE('',*,*,#16838,.T.);
#23839=ORIENTED_EDGE('',*,*,#16839,.F.);
#23840=ORIENTED_EDGE('',*,*,#16838,.F.);
#23841=ORIENTED_EDGE('',*,*,#16835,.F.);
#23842=ORIENTED_EDGE('',*,*,#16840,.F.);
#23843=ORIENTED_EDGE('',*,*,#16841,.T.);
#23844=ORIENTED_EDGE('',*,*,#16842,.F.);
#23845=ORIENTED_EDGE('',*,*,#16774,.F.);
#23846=ORIENTED_EDGE('',*,*,#16843,.F.);
#23847=ORIENTED_EDGE('',*,*,#16775,.F.);
#23848=ORIENTED_EDGE('',*,*,#16842,.T.);
#23849=ORIENTED_EDGE('',*,*,#16844,.T.);
#23850=ORIENTED_EDGE('',*,*,#16845,.F.);
#23851=ORIENTED_EDGE('',*,*,#16844,.F.);
#23852=ORIENTED_EDGE('',*,*,#16841,.F.);
#23853=ORIENTED_EDGE('',*,*,#16846,.F.);
#23854=ORIENTED_EDGE('',*,*,#16847,.T.);
#23855=ORIENTED_EDGE('',*,*,#16848,.F.);
#23856=ORIENTED_EDGE('',*,*,#16777,.F.);
#23857=ORIENTED_EDGE('',*,*,#16849,.F.);
#23858=ORIENTED_EDGE('',*,*,#16778,.F.);
#23859=ORIENTED_EDGE('',*,*,#16848,.T.);
#23860=ORIENTED_EDGE('',*,*,#16850,.T.);
#23861=ORIENTED_EDGE('',*,*,#16851,.F.);
#23862=ORIENTED_EDGE('',*,*,#16850,.F.);
#23863=ORIENTED_EDGE('',*,*,#16847,.F.);
#23864=ORIENTED_EDGE('',*,*,#16852,.F.);
#23865=ORIENTED_EDGE('',*,*,#16853,.T.);
#23866=ORIENTED_EDGE('',*,*,#16854,.F.);
#23867=ORIENTED_EDGE('',*,*,#16780,.F.);
#23868=ORIENTED_EDGE('',*,*,#16855,.F.);
#23869=ORIENTED_EDGE('',*,*,#16781,.F.);
#23870=ORIENTED_EDGE('',*,*,#16854,.T.);
#23871=ORIENTED_EDGE('',*,*,#16856,.T.);
#23872=ORIENTED_EDGE('',*,*,#16857,.F.);
#23873=ORIENTED_EDGE('',*,*,#16856,.F.);
#23874=ORIENTED_EDGE('',*,*,#16853,.F.);
#23875=ORIENTED_EDGE('',*,*,#16858,.F.);
#23876=ORIENTED_EDGE('',*,*,#16859,.T.);
#23877=ORIENTED_EDGE('',*,*,#16860,.F.);
#23878=ORIENTED_EDGE('',*,*,#16783,.F.);
#23879=ORIENTED_EDGE('',*,*,#16861,.F.);
#23880=ORIENTED_EDGE('',*,*,#16784,.F.);
#23881=ORIENTED_EDGE('',*,*,#16860,.T.);
#23882=ORIENTED_EDGE('',*,*,#16862,.T.);
#23883=ORIENTED_EDGE('',*,*,#16863,.F.);
#23884=ORIENTED_EDGE('',*,*,#16862,.F.);
#23885=ORIENTED_EDGE('',*,*,#16859,.F.);
#23886=ORIENTED_EDGE('',*,*,#16864,.F.);
#23887=ORIENTED_EDGE('',*,*,#16865,.T.);
#23888=ORIENTED_EDGE('',*,*,#16866,.F.);
#23889=ORIENTED_EDGE('',*,*,#16786,.F.);
#23890=ORIENTED_EDGE('',*,*,#16867,.F.);
#23891=ORIENTED_EDGE('',*,*,#16787,.F.);
#23892=ORIENTED_EDGE('',*,*,#16866,.T.);
#23893=ORIENTED_EDGE('',*,*,#16868,.T.);
#23894=ORIENTED_EDGE('',*,*,#16869,.F.);
#23895=ORIENTED_EDGE('',*,*,#16868,.F.);
#23896=ORIENTED_EDGE('',*,*,#16865,.F.);
#23897=ORIENTED_EDGE('',*,*,#16870,.F.);
#23898=ORIENTED_EDGE('',*,*,#16871,.T.);
#23899=ORIENTED_EDGE('',*,*,#16872,.F.);
#23900=ORIENTED_EDGE('',*,*,#16789,.F.);
#23901=ORIENTED_EDGE('',*,*,#16873,.F.);
#23902=ORIENTED_EDGE('',*,*,#16790,.F.);
#23903=ORIENTED_EDGE('',*,*,#16872,.T.);
#23904=ORIENTED_EDGE('',*,*,#16874,.T.);
#23905=ORIENTED_EDGE('',*,*,#16875,.F.);
#23906=ORIENTED_EDGE('',*,*,#16874,.F.);
#23907=ORIENTED_EDGE('',*,*,#16871,.F.);
#23908=ORIENTED_EDGE('',*,*,#16876,.F.);
#23909=ORIENTED_EDGE('',*,*,#16877,.T.);
#23910=ORIENTED_EDGE('',*,*,#16878,.F.);
#23911=ORIENTED_EDGE('',*,*,#16792,.F.);
#23912=ORIENTED_EDGE('',*,*,#16879,.F.);
#23913=ORIENTED_EDGE('',*,*,#16793,.F.);
#23914=ORIENTED_EDGE('',*,*,#16878,.T.);
#23915=ORIENTED_EDGE('',*,*,#16880,.T.);
#23916=ORIENTED_EDGE('',*,*,#16881,.F.);
#23917=ORIENTED_EDGE('',*,*,#16880,.F.);
#23918=ORIENTED_EDGE('',*,*,#16877,.F.);
#23919=ORIENTED_EDGE('',*,*,#16882,.F.);
#23920=ORIENTED_EDGE('',*,*,#16883,.T.);
#23921=ORIENTED_EDGE('',*,*,#16884,.F.);
#23922=ORIENTED_EDGE('',*,*,#16795,.F.);
#23923=ORIENTED_EDGE('',*,*,#16885,.F.);
#23924=ORIENTED_EDGE('',*,*,#16796,.F.);
#23925=ORIENTED_EDGE('',*,*,#16884,.T.);
#23926=ORIENTED_EDGE('',*,*,#16886,.T.);
#23927=ORIENTED_EDGE('',*,*,#16887,.F.);
#23928=ORIENTED_EDGE('',*,*,#16886,.F.);
#23929=ORIENTED_EDGE('',*,*,#16883,.F.);
#23930=ORIENTED_EDGE('',*,*,#16888,.F.);
#23931=ORIENTED_EDGE('',*,*,#16889,.T.);
#23932=ORIENTED_EDGE('',*,*,#16890,.F.);
#23933=ORIENTED_EDGE('',*,*,#16798,.F.);
#23934=ORIENTED_EDGE('',*,*,#16891,.F.);
#23935=ORIENTED_EDGE('',*,*,#16799,.F.);
#23936=ORIENTED_EDGE('',*,*,#16890,.T.);
#23937=ORIENTED_EDGE('',*,*,#16892,.T.);
#23938=ORIENTED_EDGE('',*,*,#16893,.F.);
#23939=ORIENTED_EDGE('',*,*,#16892,.F.);
#23940=ORIENTED_EDGE('',*,*,#16889,.F.);
#23941=ORIENTED_EDGE('',*,*,#16894,.F.);
#23942=ORIENTED_EDGE('',*,*,#16895,.T.);
#23943=ORIENTED_EDGE('',*,*,#16896,.F.);
#23944=ORIENTED_EDGE('',*,*,#16801,.F.);
#23945=ORIENTED_EDGE('',*,*,#16897,.F.);
#23946=ORIENTED_EDGE('',*,*,#16802,.F.);
#23947=ORIENTED_EDGE('',*,*,#16896,.T.);
#23948=ORIENTED_EDGE('',*,*,#16898,.T.);
#23949=ORIENTED_EDGE('',*,*,#16899,.F.);
#23950=ORIENTED_EDGE('',*,*,#16898,.F.);
#23951=ORIENTED_EDGE('',*,*,#16895,.F.);
#23952=ORIENTED_EDGE('',*,*,#16900,.F.);
#23953=ORIENTED_EDGE('',*,*,#16901,.T.);
#23954=ORIENTED_EDGE('',*,*,#16902,.F.);
#23955=ORIENTED_EDGE('',*,*,#16804,.F.);
#23956=ORIENTED_EDGE('',*,*,#16903,.F.);
#23957=ORIENTED_EDGE('',*,*,#16805,.F.);
#23958=ORIENTED_EDGE('',*,*,#16902,.T.);
#23959=ORIENTED_EDGE('',*,*,#16904,.T.);
#23960=ORIENTED_EDGE('',*,*,#16905,.F.);
#23961=ORIENTED_EDGE('',*,*,#16904,.F.);
#23962=ORIENTED_EDGE('',*,*,#16901,.F.);
#23963=ORIENTED_EDGE('',*,*,#16906,.F.);
#23964=ORIENTED_EDGE('',*,*,#16907,.T.);
#23965=ORIENTED_EDGE('',*,*,#16908,.F.);
#23966=ORIENTED_EDGE('',*,*,#16807,.F.);
#23967=ORIENTED_EDGE('',*,*,#16909,.F.);
#23968=ORIENTED_EDGE('',*,*,#16702,.F.);
#23969=ORIENTED_EDGE('',*,*,#16908,.T.);
#23970=ORIENTED_EDGE('',*,*,#16910,.T.);
#23971=ORIENTED_EDGE('',*,*,#16911,.F.);
#23972=ORIENTED_EDGE('',*,*,#16910,.F.);
#23973=ORIENTED_EDGE('',*,*,#16907,.F.);
#23974=ORIENTED_EDGE('',*,*,#16912,.F.);
#23975=ORIENTED_EDGE('',*,*,#16913,.F.);
#23976=ORIENTED_EDGE('',*,*,#16914,.T.);
#23977=ORIENTED_EDGE('',*,*,#16915,.F.);
#23978=ORIENTED_EDGE('',*,*,#16704,.F.);
#23979=ORIENTED_EDGE('',*,*,#16916,.F.);
#23980=ORIENTED_EDGE('',*,*,#16705,.F.);
#23981=ORIENTED_EDGE('',*,*,#16915,.T.);
#23982=ORIENTED_EDGE('',*,*,#16917,.T.);
#23983=ORIENTED_EDGE('',*,*,#16918,.F.);
#23984=ORIENTED_EDGE('',*,*,#16917,.F.);
#23985=ORIENTED_EDGE('',*,*,#16914,.F.);
#23986=ORIENTED_EDGE('',*,*,#16919,.F.);
#23987=ORIENTED_EDGE('',*,*,#16920,.T.);
#23988=ORIENTED_EDGE('',*,*,#16921,.F.);
#23989=ORIENTED_EDGE('',*,*,#16707,.F.);
#23990=ORIENTED_EDGE('',*,*,#16922,.F.);
#23991=ORIENTED_EDGE('',*,*,#16708,.F.);
#23992=ORIENTED_EDGE('',*,*,#16921,.T.);
#23993=ORIENTED_EDGE('',*,*,#16923,.T.);
#23994=ORIENTED_EDGE('',*,*,#16924,.F.);
#23995=ORIENTED_EDGE('',*,*,#16923,.F.);
#23996=ORIENTED_EDGE('',*,*,#16920,.F.);
#23997=ORIENTED_EDGE('',*,*,#16925,.F.);
#23998=ORIENTED_EDGE('',*,*,#16926,.T.);
#23999=ORIENTED_EDGE('',*,*,#16927,.F.);
#24000=ORIENTED_EDGE('',*,*,#16710,.F.);
#24001=ORIENTED_EDGE('',*,*,#16928,.F.);
#24002=ORIENTED_EDGE('',*,*,#16711,.F.);
#24003=ORIENTED_EDGE('',*,*,#16927,.T.);
#24004=ORIENTED_EDGE('',*,*,#16929,.T.);
#24005=ORIENTED_EDGE('',*,*,#16930,.F.);
#24006=ORIENTED_EDGE('',*,*,#16929,.F.);
#24007=ORIENTED_EDGE('',*,*,#16926,.F.);
#24008=ORIENTED_EDGE('',*,*,#16931,.F.);
#24009=ORIENTED_EDGE('',*,*,#16932,.T.);
#24010=ORIENTED_EDGE('',*,*,#16933,.F.);
#24011=ORIENTED_EDGE('',*,*,#16713,.F.);
#24012=ORIENTED_EDGE('',*,*,#16934,.F.);
#24013=ORIENTED_EDGE('',*,*,#16714,.F.);
#24014=ORIENTED_EDGE('',*,*,#16933,.T.);
#24015=ORIENTED_EDGE('',*,*,#16935,.T.);
#24016=ORIENTED_EDGE('',*,*,#16936,.F.);
#24017=ORIENTED_EDGE('',*,*,#16935,.F.);
#24018=ORIENTED_EDGE('',*,*,#16932,.F.);
#24019=ORIENTED_EDGE('',*,*,#16937,.F.);
#24020=ORIENTED_EDGE('',*,*,#16938,.T.);
#24021=ORIENTED_EDGE('',*,*,#16939,.F.);
#24022=ORIENTED_EDGE('',*,*,#16716,.F.);
#24023=ORIENTED_EDGE('',*,*,#16940,.F.);
#24024=ORIENTED_EDGE('',*,*,#16717,.F.);
#24025=ORIENTED_EDGE('',*,*,#16939,.T.);
#24026=ORIENTED_EDGE('',*,*,#16941,.T.);
#24027=ORIENTED_EDGE('',*,*,#16942,.F.);
#24028=ORIENTED_EDGE('',*,*,#16941,.F.);
#24029=ORIENTED_EDGE('',*,*,#16938,.F.);
#24030=ORIENTED_EDGE('',*,*,#16943,.F.);
#24031=ORIENTED_EDGE('',*,*,#16944,.T.);
#24032=ORIENTED_EDGE('',*,*,#16945,.F.);
#24033=ORIENTED_EDGE('',*,*,#16719,.F.);
#24034=ORIENTED_EDGE('',*,*,#16946,.F.);
#24035=ORIENTED_EDGE('',*,*,#16720,.F.);
#24036=ORIENTED_EDGE('',*,*,#16945,.T.);
#24037=ORIENTED_EDGE('',*,*,#16947,.T.);
#24038=ORIENTED_EDGE('',*,*,#16948,.F.);
#24039=ORIENTED_EDGE('',*,*,#16947,.F.);
#24040=ORIENTED_EDGE('',*,*,#16944,.F.);
#24041=ORIENTED_EDGE('',*,*,#16949,.F.);
#24042=ORIENTED_EDGE('',*,*,#16950,.T.);
#24043=ORIENTED_EDGE('',*,*,#16951,.F.);
#24044=ORIENTED_EDGE('',*,*,#16722,.F.);
#24045=ORIENTED_EDGE('',*,*,#16952,.F.);
#24046=ORIENTED_EDGE('',*,*,#16723,.F.);
#24047=ORIENTED_EDGE('',*,*,#16951,.T.);
#24048=ORIENTED_EDGE('',*,*,#16953,.T.);
#24049=ORIENTED_EDGE('',*,*,#16954,.F.);
#24050=ORIENTED_EDGE('',*,*,#16953,.F.);
#24051=ORIENTED_EDGE('',*,*,#16950,.F.);
#24052=ORIENTED_EDGE('',*,*,#16955,.F.);
#24053=ORIENTED_EDGE('',*,*,#16956,.T.);
#24054=ORIENTED_EDGE('',*,*,#16957,.F.);
#24055=ORIENTED_EDGE('',*,*,#16725,.F.);
#24056=ORIENTED_EDGE('',*,*,#16958,.F.);
#24057=ORIENTED_EDGE('',*,*,#16726,.F.);
#24058=ORIENTED_EDGE('',*,*,#16957,.T.);
#24059=ORIENTED_EDGE('',*,*,#16959,.T.);
#24060=ORIENTED_EDGE('',*,*,#16960,.F.);
#24061=ORIENTED_EDGE('',*,*,#16959,.F.);
#24062=ORIENTED_EDGE('',*,*,#16956,.F.);
#24063=ORIENTED_EDGE('',*,*,#16961,.F.);
#24064=ORIENTED_EDGE('',*,*,#16962,.T.);
#24065=ORIENTED_EDGE('',*,*,#16963,.F.);
#24066=ORIENTED_EDGE('',*,*,#16728,.F.);
#24067=ORIENTED_EDGE('',*,*,#16964,.F.);
#24068=ORIENTED_EDGE('',*,*,#16729,.F.);
#24069=ORIENTED_EDGE('',*,*,#16963,.T.);
#24070=ORIENTED_EDGE('',*,*,#16965,.T.);
#24071=ORIENTED_EDGE('',*,*,#16966,.F.);
#24072=ORIENTED_EDGE('',*,*,#16965,.F.);
#24073=ORIENTED_EDGE('',*,*,#16962,.F.);
#24074=ORIENTED_EDGE('',*,*,#16967,.F.);
#24075=ORIENTED_EDGE('',*,*,#16968,.T.);
#24076=ORIENTED_EDGE('',*,*,#16969,.F.);
#24077=ORIENTED_EDGE('',*,*,#16731,.F.);
#24078=ORIENTED_EDGE('',*,*,#16970,.F.);
#24079=ORIENTED_EDGE('',*,*,#16732,.F.);
#24080=ORIENTED_EDGE('',*,*,#16969,.T.);
#24081=ORIENTED_EDGE('',*,*,#16971,.T.);
#24082=ORIENTED_EDGE('',*,*,#16972,.F.);
#24083=ORIENTED_EDGE('',*,*,#16971,.F.);
#24084=ORIENTED_EDGE('',*,*,#16968,.F.);
#24085=ORIENTED_EDGE('',*,*,#16973,.F.);
#24086=ORIENTED_EDGE('',*,*,#16974,.T.);
#24087=ORIENTED_EDGE('',*,*,#16975,.F.);
#24088=ORIENTED_EDGE('',*,*,#16734,.F.);
#24089=ORIENTED_EDGE('',*,*,#16976,.F.);
#24090=ORIENTED_EDGE('',*,*,#16735,.F.);
#24091=ORIENTED_EDGE('',*,*,#16975,.T.);
#24092=ORIENTED_EDGE('',*,*,#16977,.T.);
#24093=ORIENTED_EDGE('',*,*,#16978,.F.);
#24094=ORIENTED_EDGE('',*,*,#16977,.F.);
#24095=ORIENTED_EDGE('',*,*,#16974,.F.);
#24096=ORIENTED_EDGE('',*,*,#16979,.F.);
#24097=ORIENTED_EDGE('',*,*,#16980,.T.);
#24098=ORIENTED_EDGE('',*,*,#16981,.F.);
#24099=ORIENTED_EDGE('',*,*,#16737,.F.);
#24100=ORIENTED_EDGE('',*,*,#16982,.F.);
#24101=ORIENTED_EDGE('',*,*,#16738,.F.);
#24102=ORIENTED_EDGE('',*,*,#16981,.T.);
#24103=ORIENTED_EDGE('',*,*,#16983,.T.);
#24104=ORIENTED_EDGE('',*,*,#16984,.F.);
#24105=ORIENTED_EDGE('',*,*,#16983,.F.);
#24106=ORIENTED_EDGE('',*,*,#16980,.F.);
#24107=ORIENTED_EDGE('',*,*,#16985,.F.);
#24108=ORIENTED_EDGE('',*,*,#16986,.T.);
#24109=ORIENTED_EDGE('',*,*,#16987,.F.);
#24110=ORIENTED_EDGE('',*,*,#16740,.F.);
#24111=ORIENTED_EDGE('',*,*,#16988,.F.);
#24112=ORIENTED_EDGE('',*,*,#16741,.F.);
#24113=ORIENTED_EDGE('',*,*,#16987,.T.);
#24114=ORIENTED_EDGE('',*,*,#16989,.T.);
#24115=ORIENTED_EDGE('',*,*,#16990,.F.);
#24116=ORIENTED_EDGE('',*,*,#16989,.F.);
#24117=ORIENTED_EDGE('',*,*,#16986,.F.);
#24118=ORIENTED_EDGE('',*,*,#16991,.F.);
#24119=ORIENTED_EDGE('',*,*,#16992,.T.);
#24120=ORIENTED_EDGE('',*,*,#16993,.F.);
#24121=ORIENTED_EDGE('',*,*,#16743,.F.);
#24122=ORIENTED_EDGE('',*,*,#16994,.F.);
#24123=ORIENTED_EDGE('',*,*,#16744,.F.);
#24124=ORIENTED_EDGE('',*,*,#16993,.T.);
#24125=ORIENTED_EDGE('',*,*,#16995,.T.);
#24126=ORIENTED_EDGE('',*,*,#16996,.F.);
#24127=ORIENTED_EDGE('',*,*,#16995,.F.);
#24128=ORIENTED_EDGE('',*,*,#16992,.F.);
#24129=ORIENTED_EDGE('',*,*,#16997,.F.);
#24130=ORIENTED_EDGE('',*,*,#16998,.T.);
#24131=ORIENTED_EDGE('',*,*,#16999,.F.);
#24132=ORIENTED_EDGE('',*,*,#16746,.F.);
#24133=ORIENTED_EDGE('',*,*,#17000,.F.);
#24134=ORIENTED_EDGE('',*,*,#16747,.F.);
#24135=ORIENTED_EDGE('',*,*,#16999,.T.);
#24136=ORIENTED_EDGE('',*,*,#17001,.T.);
#24137=ORIENTED_EDGE('',*,*,#17002,.F.);
#24138=ORIENTED_EDGE('',*,*,#17001,.F.);
#24139=ORIENTED_EDGE('',*,*,#16998,.F.);
#24140=ORIENTED_EDGE('',*,*,#17003,.F.);
#24141=ORIENTED_EDGE('',*,*,#17004,.T.);
#24142=ORIENTED_EDGE('',*,*,#17005,.F.);
#24143=ORIENTED_EDGE('',*,*,#16749,.F.);
#24144=ORIENTED_EDGE('',*,*,#17006,.F.);
#24145=ORIENTED_EDGE('',*,*,#16750,.F.);
#24146=ORIENTED_EDGE('',*,*,#17005,.T.);
#24147=ORIENTED_EDGE('',*,*,#17007,.T.);
#24148=ORIENTED_EDGE('',*,*,#17008,.F.);
#24149=ORIENTED_EDGE('',*,*,#17007,.F.);
#24150=ORIENTED_EDGE('',*,*,#17004,.F.);
#24151=ORIENTED_EDGE('',*,*,#17009,.F.);
#24152=ORIENTED_EDGE('',*,*,#17010,.T.);
#24153=ORIENTED_EDGE('',*,*,#17011,.F.);
#24154=ORIENTED_EDGE('',*,*,#16752,.F.);
#24155=ORIENTED_EDGE('',*,*,#17012,.F.);
#24156=ORIENTED_EDGE('',*,*,#16753,.F.);
#24157=ORIENTED_EDGE('',*,*,#17011,.T.);
#24158=ORIENTED_EDGE('',*,*,#17013,.T.);
#24159=ORIENTED_EDGE('',*,*,#17014,.F.);
#24160=ORIENTED_EDGE('',*,*,#17013,.F.);
#24161=ORIENTED_EDGE('',*,*,#17010,.F.);
#24162=ORIENTED_EDGE('',*,*,#17015,.F.);
#24163=ORIENTED_EDGE('',*,*,#17016,.T.);
#24164=ORIENTED_EDGE('',*,*,#17017,.F.);
#24165=ORIENTED_EDGE('',*,*,#16755,.F.);
#24166=ORIENTED_EDGE('',*,*,#17018,.F.);
#24167=ORIENTED_EDGE('',*,*,#16756,.F.);
#24168=ORIENTED_EDGE('',*,*,#17017,.T.);
#24169=ORIENTED_EDGE('',*,*,#17019,.T.);
#24170=ORIENTED_EDGE('',*,*,#17020,.F.);
#24171=ORIENTED_EDGE('',*,*,#17019,.F.);
#24172=ORIENTED_EDGE('',*,*,#17016,.F.);
#24173=ORIENTED_EDGE('',*,*,#16911,.T.);
#24174=ORIENTED_EDGE('',*,*,#17021,.T.);
#24175=ORIENTED_EDGE('',*,*,#16691,.T.);
#24176=ORIENTED_EDGE('',*,*,#17021,.F.);
#24177=ORIENTED_EDGE('',*,*,#16912,.T.);
#24178=ORIENTED_EDGE('',*,*,#16906,.T.);
#24179=ORIENTED_EDGE('',*,*,#16806,.F.);
#24180=ORIENTED_EDGE('',*,*,#16903,.T.);
#24181=ORIENTED_EDGE('',*,*,#16905,.T.);
#24182=ORIENTED_EDGE('',*,*,#16900,.T.);
#24183=ORIENTED_EDGE('',*,*,#16803,.F.);
#24184=ORIENTED_EDGE('',*,*,#16897,.T.);
#24185=ORIENTED_EDGE('',*,*,#16899,.T.);
#24186=ORIENTED_EDGE('',*,*,#16894,.T.);
#24187=ORIENTED_EDGE('',*,*,#16800,.F.);
#24188=ORIENTED_EDGE('',*,*,#16891,.T.);
#24189=ORIENTED_EDGE('',*,*,#16893,.T.);
#24190=ORIENTED_EDGE('',*,*,#16888,.T.);
#24191=ORIENTED_EDGE('',*,*,#16797,.F.);
#24192=ORIENTED_EDGE('',*,*,#16885,.T.);
#24193=ORIENTED_EDGE('',*,*,#16887,.T.);
#24194=ORIENTED_EDGE('',*,*,#16882,.T.);
#24195=ORIENTED_EDGE('',*,*,#16794,.F.);
#24196=ORIENTED_EDGE('',*,*,#16879,.T.);
#24197=ORIENTED_EDGE('',*,*,#16881,.T.);
#24198=ORIENTED_EDGE('',*,*,#16876,.T.);
#24199=ORIENTED_EDGE('',*,*,#16791,.F.);
#24200=ORIENTED_EDGE('',*,*,#16873,.T.);
#24201=ORIENTED_EDGE('',*,*,#16875,.T.);
#24202=ORIENTED_EDGE('',*,*,#16870,.T.);
#24203=ORIENTED_EDGE('',*,*,#16788,.F.);
#24204=ORIENTED_EDGE('',*,*,#16867,.T.);
#24205=ORIENTED_EDGE('',*,*,#16869,.T.);
#24206=ORIENTED_EDGE('',*,*,#16864,.T.);
#24207=ORIENTED_EDGE('',*,*,#16785,.F.);
#24208=ORIENTED_EDGE('',*,*,#16861,.T.);
#24209=ORIENTED_EDGE('',*,*,#16863,.T.);
#24210=ORIENTED_EDGE('',*,*,#16858,.T.);
#24211=ORIENTED_EDGE('',*,*,#16782,.F.);
#24212=ORIENTED_EDGE('',*,*,#16855,.T.);
#24213=ORIENTED_EDGE('',*,*,#16857,.T.);
#24214=ORIENTED_EDGE('',*,*,#16852,.T.);
#24215=ORIENTED_EDGE('',*,*,#16779,.F.);
#24216=ORIENTED_EDGE('',*,*,#16849,.T.);
#24217=ORIENTED_EDGE('',*,*,#16851,.T.);
#24218=ORIENTED_EDGE('',*,*,#16846,.T.);
#24219=ORIENTED_EDGE('',*,*,#16776,.F.);
#24220=ORIENTED_EDGE('',*,*,#16843,.T.);
#24221=ORIENTED_EDGE('',*,*,#16845,.T.);
#24222=ORIENTED_EDGE('',*,*,#16840,.T.);
#24223=ORIENTED_EDGE('',*,*,#16773,.F.);
#24224=ORIENTED_EDGE('',*,*,#16837,.T.);
#24225=ORIENTED_EDGE('',*,*,#16839,.T.);
#24226=ORIENTED_EDGE('',*,*,#16834,.T.);
#24227=ORIENTED_EDGE('',*,*,#16770,.F.);
#24228=ORIENTED_EDGE('',*,*,#16831,.T.);
#24229=ORIENTED_EDGE('',*,*,#16833,.T.);
#24230=ORIENTED_EDGE('',*,*,#16828,.T.);
#24231=ORIENTED_EDGE('',*,*,#16767,.F.);
#24232=ORIENTED_EDGE('',*,*,#16825,.T.);
#24233=ORIENTED_EDGE('',*,*,#16827,.T.);
#24234=ORIENTED_EDGE('',*,*,#16822,.T.);
#24235=ORIENTED_EDGE('',*,*,#16764,.F.);
#24236=ORIENTED_EDGE('',*,*,#16819,.T.);
#24237=ORIENTED_EDGE('',*,*,#16821,.T.);
#24238=ORIENTED_EDGE('',*,*,#16816,.T.);
#24239=ORIENTED_EDGE('',*,*,#16761,.F.);
#24240=ORIENTED_EDGE('',*,*,#16813,.T.);
#24241=ORIENTED_EDGE('',*,*,#16815,.T.);
#24242=ORIENTED_EDGE('',*,*,#16810,.T.);
#24243=ORIENTED_EDGE('',*,*,#16758,.F.);
#24244=ORIENTED_EDGE('',*,*,#16698,.T.);
#24245=ORIENTED_EDGE('',*,*,#16701,.T.);
#24246=ORIENTED_EDGE('',*,*,#16694,.T.);
#24247=ORIENTED_EDGE('',*,*,#16757,.F.);
#24248=ORIENTED_EDGE('',*,*,#17018,.T.);
#24249=ORIENTED_EDGE('',*,*,#17020,.T.);
#24250=ORIENTED_EDGE('',*,*,#17015,.T.);
#24251=ORIENTED_EDGE('',*,*,#16754,.F.);
#24252=ORIENTED_EDGE('',*,*,#17012,.T.);
#24253=ORIENTED_EDGE('',*,*,#17014,.T.);
#24254=ORIENTED_EDGE('',*,*,#17009,.T.);
#24255=ORIENTED_EDGE('',*,*,#16751,.F.);
#24256=ORIENTED_EDGE('',*,*,#17006,.T.);
#24257=ORIENTED_EDGE('',*,*,#17008,.T.);
#24258=ORIENTED_EDGE('',*,*,#17003,.T.);
#24259=ORIENTED_EDGE('',*,*,#16748,.F.);
#24260=ORIENTED_EDGE('',*,*,#17000,.T.);
#24261=ORIENTED_EDGE('',*,*,#17002,.T.);
#24262=ORIENTED_EDGE('',*,*,#16997,.T.);
#24263=ORIENTED_EDGE('',*,*,#16745,.F.);
#24264=ORIENTED_EDGE('',*,*,#16994,.T.);
#24265=ORIENTED_EDGE('',*,*,#16996,.T.);
#24266=ORIENTED_EDGE('',*,*,#16991,.T.);
#24267=ORIENTED_EDGE('',*,*,#16742,.F.);
#24268=ORIENTED_EDGE('',*,*,#16988,.T.);
#24269=ORIENTED_EDGE('',*,*,#16990,.T.);
#24270=ORIENTED_EDGE('',*,*,#16985,.T.);
#24271=ORIENTED_EDGE('',*,*,#16739,.F.);
#24272=ORIENTED_EDGE('',*,*,#16982,.T.);
#24273=ORIENTED_EDGE('',*,*,#16984,.T.);
#24274=ORIENTED_EDGE('',*,*,#16979,.T.);
#24275=ORIENTED_EDGE('',*,*,#16736,.F.);
#24276=ORIENTED_EDGE('',*,*,#16976,.T.);
#24277=ORIENTED_EDGE('',*,*,#16978,.T.);
#24278=ORIENTED_EDGE('',*,*,#16973,.T.);
#24279=ORIENTED_EDGE('',*,*,#16733,.F.);
#24280=ORIENTED_EDGE('',*,*,#16970,.T.);
#24281=ORIENTED_EDGE('',*,*,#16972,.T.);
#24282=ORIENTED_EDGE('',*,*,#16967,.T.);
#24283=ORIENTED_EDGE('',*,*,#16730,.F.);
#24284=ORIENTED_EDGE('',*,*,#16964,.T.);
#24285=ORIENTED_EDGE('',*,*,#16966,.T.);
#24286=ORIENTED_EDGE('',*,*,#16961,.T.);
#24287=ORIENTED_EDGE('',*,*,#16727,.F.);
#24288=ORIENTED_EDGE('',*,*,#16958,.T.);
#24289=ORIENTED_EDGE('',*,*,#16960,.T.);
#24290=ORIENTED_EDGE('',*,*,#16955,.T.);
#24291=ORIENTED_EDGE('',*,*,#16724,.F.);
#24292=ORIENTED_EDGE('',*,*,#16952,.T.);
#24293=ORIENTED_EDGE('',*,*,#16954,.T.);
#24294=ORIENTED_EDGE('',*,*,#16949,.T.);
#24295=ORIENTED_EDGE('',*,*,#16721,.F.);
#24296=ORIENTED_EDGE('',*,*,#16946,.T.);
#24297=ORIENTED_EDGE('',*,*,#16948,.T.);
#24298=ORIENTED_EDGE('',*,*,#16943,.T.);
#24299=ORIENTED_EDGE('',*,*,#16718,.F.);
#24300=ORIENTED_EDGE('',*,*,#16940,.T.);
#24301=ORIENTED_EDGE('',*,*,#16942,.T.);
#24302=ORIENTED_EDGE('',*,*,#16937,.T.);
#24303=ORIENTED_EDGE('',*,*,#16715,.F.);
#24304=ORIENTED_EDGE('',*,*,#16934,.T.);
#24305=ORIENTED_EDGE('',*,*,#16936,.T.);
#24306=ORIENTED_EDGE('',*,*,#16931,.T.);
#24307=ORIENTED_EDGE('',*,*,#16712,.F.);
#24308=ORIENTED_EDGE('',*,*,#16928,.T.);
#24309=ORIENTED_EDGE('',*,*,#16930,.T.);
#24310=ORIENTED_EDGE('',*,*,#16925,.T.);
#24311=ORIENTED_EDGE('',*,*,#16709,.F.);
#24312=ORIENTED_EDGE('',*,*,#16922,.T.);
#24313=ORIENTED_EDGE('',*,*,#16924,.T.);
#24314=ORIENTED_EDGE('',*,*,#16919,.T.);
#24315=ORIENTED_EDGE('',*,*,#16706,.F.);
#24316=ORIENTED_EDGE('',*,*,#16916,.T.);
#24317=ORIENTED_EDGE('',*,*,#16918,.T.);
#24318=ORIENTED_EDGE('',*,*,#16913,.T.);
#24319=ORIENTED_EDGE('',*,*,#16703,.F.);
#24320=ORIENTED_EDGE('',*,*,#16909,.T.);
#24321=ORIENTED_EDGE('',*,*,#16809,.F.);
#24322=ORIENTED_EDGE('',*,*,#17022,.T.);
#24323=ORIENTED_EDGE('',*,*,#17023,.T.);
#24324=ORIENTED_EDGE('',*,*,#17024,.T.);
#24325=ORIENTED_EDGE('',*,*,#17025,.T.);
#24326=ORIENTED_EDGE('',*,*,#17026,.T.);
#24327=ORIENTED_EDGE('',*,*,#17027,.T.);
#24328=ORIENTED_EDGE('',*,*,#17028,.F.);
#24329=ORIENTED_EDGE('',*,*,#17029,.T.);
#24330=ORIENTED_EDGE('',*,*,#17030,.F.);
#24331=ORIENTED_EDGE('',*,*,#17031,.T.);
#24332=ORIENTED_EDGE('',*,*,#17032,.F.);
#24333=ORIENTED_EDGE('',*,*,#17033,.T.);
#24334=ORIENTED_EDGE('',*,*,#17034,.F.);
#24335=ORIENTED_EDGE('',*,*,#17035,.T.);
#24336=ORIENTED_EDGE('',*,*,#17036,.F.);
#24337=ORIENTED_EDGE('',*,*,#17037,.T.);
#24338=ORIENTED_EDGE('',*,*,#17038,.F.);
#24339=ORIENTED_EDGE('',*,*,#17039,.T.);
#24340=ORIENTED_EDGE('',*,*,#17040,.T.);
#24341=ORIENTED_EDGE('',*,*,#17039,.F.);
#24342=ORIENTED_EDGE('',*,*,#17037,.F.);
#24343=ORIENTED_EDGE('',*,*,#17035,.F.);
#24344=ORIENTED_EDGE('',*,*,#17033,.F.);
#24345=ORIENTED_EDGE('',*,*,#17031,.F.);
#24346=ORIENTED_EDGE('',*,*,#17029,.F.);
#24347=ORIENTED_EDGE('',*,*,#17040,.F.);
#24348=ORIENTED_EDGE('',*,*,#17022,.F.);
#24349=ORIENTED_EDGE('',*,*,#17041,.T.);
#24350=ORIENTED_EDGE('',*,*,#17028,.T.);
#24351=ORIENTED_EDGE('',*,*,#17042,.F.);
#24352=ORIENTED_EDGE('',*,*,#17027,.F.);
#24353=ORIENTED_EDGE('',*,*,#17043,.T.);
#24354=ORIENTED_EDGE('',*,*,#17038,.T.);
#24355=ORIENTED_EDGE('',*,*,#17041,.F.);
#24356=ORIENTED_EDGE('',*,*,#17026,.F.);
#24357=ORIENTED_EDGE('',*,*,#17044,.T.);
#24358=ORIENTED_EDGE('',*,*,#17036,.T.);
#24359=ORIENTED_EDGE('',*,*,#17043,.F.);
#24360=ORIENTED_EDGE('',*,*,#17025,.F.);
#24361=ORIENTED_EDGE('',*,*,#17045,.T.);
#24362=ORIENTED_EDGE('',*,*,#17034,.T.);
#24363=ORIENTED_EDGE('',*,*,#17044,.F.);
#24364=ORIENTED_EDGE('',*,*,#17024,.F.);
#24365=ORIENTED_EDGE('',*,*,#17046,.T.);
#24366=ORIENTED_EDGE('',*,*,#17032,.T.);
#24367=ORIENTED_EDGE('',*,*,#17045,.F.);
#24368=ORIENTED_EDGE('',*,*,#17023,.F.);
#24369=ORIENTED_EDGE('',*,*,#17042,.T.);
#24370=ORIENTED_EDGE('',*,*,#17030,.T.);
#24371=ORIENTED_EDGE('',*,*,#17046,.F.);
#24372=ORIENTED_EDGE('',*,*,#17047,.F.);
#24373=ORIENTED_EDGE('',*,*,#17048,.F.);
#24374=ORIENTED_EDGE('',*,*,#17049,.F.);
#24375=ORIENTED_EDGE('',*,*,#17050,.T.);
#24376=ORIENTED_EDGE('',*,*,#17051,.F.);
#24377=ORIENTED_EDGE('',*,*,#17052,.F.);
#24378=ORIENTED_EDGE('',*,*,#17047,.T.);
#24379=ORIENTED_EDGE('',*,*,#17053,.T.);
#24380=ORIENTED_EDGE('',*,*,#17054,.F.);
#24381=ORIENTED_EDGE('',*,*,#17055,.F.);
#24382=ORIENTED_EDGE('',*,*,#17056,.F.);
#24383=ORIENTED_EDGE('',*,*,#17051,.T.);
#24384=ORIENTED_EDGE('',*,*,#17057,.T.);
#24385=ORIENTED_EDGE('',*,*,#17058,.T.);
#24386=ORIENTED_EDGE('',*,*,#17059,.F.);
#24387=ORIENTED_EDGE('',*,*,#17060,.F.);
#24388=ORIENTED_EDGE('',*,*,#17061,.F.);
#24389=ORIENTED_EDGE('',*,*,#17054,.T.);
#24390=ORIENTED_EDGE('',*,*,#17062,.T.);
#24391=ORIENTED_EDGE('',*,*,#17063,.F.);
#24392=ORIENTED_EDGE('',*,*,#17064,.F.);
#24393=ORIENTED_EDGE('',*,*,#17065,.F.);
#24394=ORIENTED_EDGE('',*,*,#17059,.T.);
#24395=ORIENTED_EDGE('',*,*,#17066,.T.);
#24396=ORIENTED_EDGE('',*,*,#17067,.T.);
#24397=ORIENTED_EDGE('',*,*,#17068,.F.);
#24398=ORIENTED_EDGE('',*,*,#17069,.F.);
#24399=ORIENTED_EDGE('',*,*,#17063,.T.);
#24400=ORIENTED_EDGE('',*,*,#17070,.T.);
#24401=ORIENTED_EDGE('',*,*,#17071,.F.);
#24402=ORIENTED_EDGE('',*,*,#17072,.F.);
#24403=ORIENTED_EDGE('',*,*,#17073,.F.);
#24404=ORIENTED_EDGE('',*,*,#17068,.T.);
#24405=ORIENTED_EDGE('',*,*,#17074,.T.);
#24406=ORIENTED_EDGE('',*,*,#17075,.T.);
#24407=ORIENTED_EDGE('',*,*,#17076,.F.);
#24408=ORIENTED_EDGE('',*,*,#17077,.F.);
#24409=ORIENTED_EDGE('',*,*,#17071,.T.);
#24410=ORIENTED_EDGE('',*,*,#17078,.T.);
#24411=ORIENTED_EDGE('',*,*,#17079,.F.);
#24412=ORIENTED_EDGE('',*,*,#17080,.F.);
#24413=ORIENTED_EDGE('',*,*,#17081,.F.);
#24414=ORIENTED_EDGE('',*,*,#17076,.T.);
#24415=ORIENTED_EDGE('',*,*,#17082,.T.);
#24416=ORIENTED_EDGE('',*,*,#17083,.T.);
#24417=ORIENTED_EDGE('',*,*,#17084,.F.);
#24418=ORIENTED_EDGE('',*,*,#17085,.F.);
#24419=ORIENTED_EDGE('',*,*,#17086,.F.);
#24420=ORIENTED_EDGE('',*,*,#17079,.T.);
#24421=ORIENTED_EDGE('',*,*,#17087,.T.);
#24422=ORIENTED_EDGE('',*,*,#17088,.F.);
#24423=ORIENTED_EDGE('',*,*,#17089,.F.);
#24424=ORIENTED_EDGE('',*,*,#17090,.F.);
#24425=ORIENTED_EDGE('',*,*,#17084,.T.);
#24426=ORIENTED_EDGE('',*,*,#17091,.T.);
#24427=ORIENTED_EDGE('',*,*,#17092,.T.);
#24428=ORIENTED_EDGE('',*,*,#17093,.F.);
#24429=ORIENTED_EDGE('',*,*,#17094,.F.);
#24430=ORIENTED_EDGE('',*,*,#17088,.T.);
#24431=ORIENTED_EDGE('',*,*,#17095,.T.);
#24432=ORIENTED_EDGE('',*,*,#17096,.T.);
#24433=ORIENTED_EDGE('',*,*,#17097,.F.);
#24434=ORIENTED_EDGE('',*,*,#17098,.F.);
#24435=ORIENTED_EDGE('',*,*,#17099,.F.);
#24436=ORIENTED_EDGE('',*,*,#17093,.T.);
#24437=ORIENTED_EDGE('',*,*,#17100,.T.);
#24438=ORIENTED_EDGE('',*,*,#17101,.F.);
#24439=ORIENTED_EDGE('',*,*,#17102,.F.);
#24440=ORIENTED_EDGE('',*,*,#17097,.T.);
#24441=ORIENTED_EDGE('',*,*,#17103,.T.);
#24442=ORIENTED_EDGE('',*,*,#17104,.T.);
#24443=ORIENTED_EDGE('',*,*,#17105,.F.);
#24444=ORIENTED_EDGE('',*,*,#17106,.F.);
#24445=ORIENTED_EDGE('',*,*,#17107,.F.);
#24446=ORIENTED_EDGE('',*,*,#17101,.T.);
#24447=ORIENTED_EDGE('',*,*,#17108,.T.);
#24448=ORIENTED_EDGE('',*,*,#17109,.F.);
#24449=ORIENTED_EDGE('',*,*,#17110,.F.);
#24450=ORIENTED_EDGE('',*,*,#17105,.T.);
#24451=ORIENTED_EDGE('',*,*,#17111,.T.);
#24452=ORIENTED_EDGE('',*,*,#17112,.F.);
#24453=ORIENTED_EDGE('',*,*,#17113,.F.);
#24454=ORIENTED_EDGE('',*,*,#17114,.F.);
#24455=ORIENTED_EDGE('',*,*,#17109,.T.);
#24456=ORIENTED_EDGE('',*,*,#17115,.T.);
#24457=ORIENTED_EDGE('',*,*,#17116,.T.);
#24458=ORIENTED_EDGE('',*,*,#17117,.F.);
#24459=ORIENTED_EDGE('',*,*,#17118,.F.);
#24460=ORIENTED_EDGE('',*,*,#17112,.T.);
#24461=ORIENTED_EDGE('',*,*,#17119,.T.);
#24462=ORIENTED_EDGE('',*,*,#17120,.T.);
#24463=ORIENTED_EDGE('',*,*,#17121,.F.);
#24464=ORIENTED_EDGE('',*,*,#17122,.F.);
#24465=ORIENTED_EDGE('',*,*,#17123,.F.);
#24466=ORIENTED_EDGE('',*,*,#17117,.T.);
#24467=ORIENTED_EDGE('',*,*,#17124,.T.);
#24468=ORIENTED_EDGE('',*,*,#17125,.T.);
#24469=ORIENTED_EDGE('',*,*,#17126,.T.);
#24470=ORIENTED_EDGE('',*,*,#17127,.F.);
#24471=ORIENTED_EDGE('',*,*,#17128,.T.);
#24472=ORIENTED_EDGE('',*,*,#17129,.T.);
#24473=ORIENTED_EDGE('',*,*,#17130,.T.);
#24474=ORIENTED_EDGE('',*,*,#17131,.T.);
#24475=ORIENTED_EDGE('',*,*,#17132,.T.);
#24476=ORIENTED_EDGE('',*,*,#17133,.T.);
#24477=ORIENTED_EDGE('',*,*,#17134,.T.);
#24478=ORIENTED_EDGE('',*,*,#17135,.T.);
#24479=ORIENTED_EDGE('',*,*,#17136,.T.);
#24480=ORIENTED_EDGE('',*,*,#17137,.T.);
#24481=ORIENTED_EDGE('',*,*,#17138,.T.);
#24482=ORIENTED_EDGE('',*,*,#17139,.T.);
#24483=ORIENTED_EDGE('',*,*,#17140,.T.);
#24484=ORIENTED_EDGE('',*,*,#17141,.T.);
#24485=ORIENTED_EDGE('',*,*,#17142,.T.);
#24486=ORIENTED_EDGE('',*,*,#17143,.T.);
#24487=ORIENTED_EDGE('',*,*,#17144,.T.);
#24488=ORIENTED_EDGE('',*,*,#17145,.T.);
#24489=ORIENTED_EDGE('',*,*,#17146,.T.);
#24490=ORIENTED_EDGE('',*,*,#17147,.T.);
#24491=ORIENTED_EDGE('',*,*,#17148,.T.);
#24492=ORIENTED_EDGE('',*,*,#17149,.F.);
#24493=ORIENTED_EDGE('',*,*,#17150,.T.);
#24494=ORIENTED_EDGE('',*,*,#17151,.T.);
#24495=ORIENTED_EDGE('',*,*,#17152,.T.);
#24496=ORIENTED_EDGE('',*,*,#17153,.T.);
#24497=ORIENTED_EDGE('',*,*,#17154,.T.);
#24498=ORIENTED_EDGE('',*,*,#17155,.T.);
#24499=ORIENTED_EDGE('',*,*,#17156,.T.);
#24500=ORIENTED_EDGE('',*,*,#17157,.T.);
#24501=ORIENTED_EDGE('',*,*,#17158,.T.);
#24502=ORIENTED_EDGE('',*,*,#17159,.T.);
#24503=ORIENTED_EDGE('',*,*,#17160,.T.);
#24504=ORIENTED_EDGE('',*,*,#17161,.T.);
#24505=ORIENTED_EDGE('',*,*,#17162,.T.);
#24506=ORIENTED_EDGE('',*,*,#17163,.T.);
#24507=ORIENTED_EDGE('',*,*,#17164,.T.);
#24508=ORIENTED_EDGE('',*,*,#17165,.T.);
#24509=ORIENTED_EDGE('',*,*,#17166,.T.);
#24510=ORIENTED_EDGE('',*,*,#17167,.T.);
#24511=ORIENTED_EDGE('',*,*,#17168,.T.);
#24512=ORIENTED_EDGE('',*,*,#17169,.T.);
#24513=ORIENTED_EDGE('',*,*,#17121,.T.);
#24514=ORIENTED_EDGE('',*,*,#17170,.T.);
#24515=ORIENTED_EDGE('',*,*,#17171,.F.);
#24516=ORIENTED_EDGE('',*,*,#17172,.F.);
#24517=ORIENTED_EDGE('',*,*,#17173,.F.);
#24518=ORIENTED_EDGE('',*,*,#17174,.T.);
#24519=ORIENTED_EDGE('',*,*,#17171,.T.);
#24520=ORIENTED_EDGE('',*,*,#17175,.T.);
#24521=ORIENTED_EDGE('',*,*,#17176,.T.);
#24522=ORIENTED_EDGE('',*,*,#17177,.F.);
#24523=ORIENTED_EDGE('',*,*,#17174,.F.);
#24524=ORIENTED_EDGE('',*,*,#17178,.F.);
#24525=ORIENTED_EDGE('',*,*,#17148,.F.);
#24526=ORIENTED_EDGE('',*,*,#17147,.F.);
#24527=ORIENTED_EDGE('',*,*,#17146,.F.);
#24528=ORIENTED_EDGE('',*,*,#17145,.F.);
#24529=ORIENTED_EDGE('',*,*,#17144,.F.);
#24530=ORIENTED_EDGE('',*,*,#17143,.F.);
#24531=ORIENTED_EDGE('',*,*,#17142,.F.);
#24532=ORIENTED_EDGE('',*,*,#17141,.F.);
#24533=ORIENTED_EDGE('',*,*,#17140,.F.);
#24534=ORIENTED_EDGE('',*,*,#17139,.F.);
#24535=ORIENTED_EDGE('',*,*,#17138,.F.);
#24536=ORIENTED_EDGE('',*,*,#17137,.F.);
#24537=ORIENTED_EDGE('',*,*,#17136,.F.);
#24538=ORIENTED_EDGE('',*,*,#17135,.F.);
#24539=ORIENTED_EDGE('',*,*,#17134,.F.);
#24540=ORIENTED_EDGE('',*,*,#17133,.F.);
#24541=ORIENTED_EDGE('',*,*,#17132,.F.);
#24542=ORIENTED_EDGE('',*,*,#17131,.F.);
#24543=ORIENTED_EDGE('',*,*,#17130,.F.);
#24544=ORIENTED_EDGE('',*,*,#17129,.F.);
#24545=ORIENTED_EDGE('',*,*,#17128,.F.);
#24546=ORIENTED_EDGE('',*,*,#17179,.F.);
#24547=ORIENTED_EDGE('',*,*,#17180,.T.);
#24548=ORIENTED_EDGE('',*,*,#17048,.T.);
#24549=ORIENTED_EDGE('',*,*,#17052,.T.);
#24550=ORIENTED_EDGE('',*,*,#17056,.T.);
#24551=ORIENTED_EDGE('',*,*,#17055,.T.);
#24552=ORIENTED_EDGE('',*,*,#17061,.T.);
#24553=ORIENTED_EDGE('',*,*,#17060,.T.);
#24554=ORIENTED_EDGE('',*,*,#17065,.T.);
#24555=ORIENTED_EDGE('',*,*,#17064,.T.);
#24556=ORIENTED_EDGE('',*,*,#17069,.T.);
#24557=ORIENTED_EDGE('',*,*,#17073,.T.);
#24558=ORIENTED_EDGE('',*,*,#17072,.T.);
#24559=ORIENTED_EDGE('',*,*,#17077,.T.);
#24560=ORIENTED_EDGE('',*,*,#17081,.T.);
#24561=ORIENTED_EDGE('',*,*,#17080,.T.);
#24562=ORIENTED_EDGE('',*,*,#17086,.T.);
#24563=ORIENTED_EDGE('',*,*,#17085,.T.);
#24564=ORIENTED_EDGE('',*,*,#17090,.T.);
#24565=ORIENTED_EDGE('',*,*,#17089,.T.);
#24566=ORIENTED_EDGE('',*,*,#17094,.T.);
#24567=ORIENTED_EDGE('',*,*,#17099,.T.);
#24568=ORIENTED_EDGE('',*,*,#17098,.T.);
#24569=ORIENTED_EDGE('',*,*,#17102,.T.);
#24570=ORIENTED_EDGE('',*,*,#17107,.T.);
#24571=ORIENTED_EDGE('',*,*,#17106,.T.);
#24572=ORIENTED_EDGE('',*,*,#17110,.T.);
#24573=ORIENTED_EDGE('',*,*,#17114,.T.);
#24574=ORIENTED_EDGE('',*,*,#17113,.T.);
#24575=ORIENTED_EDGE('',*,*,#17118,.T.);
#24576=ORIENTED_EDGE('',*,*,#17123,.T.);
#24577=ORIENTED_EDGE('',*,*,#17122,.T.);
#24578=ORIENTED_EDGE('',*,*,#17172,.T.);
#24579=ORIENTED_EDGE('',*,*,#17181,.F.);
#24580=ORIENTED_EDGE('',*,*,#17182,.T.);
#24581=ORIENTED_EDGE('',*,*,#17049,.T.);
#24582=ORIENTED_EDGE('',*,*,#17180,.F.);
#24583=ORIENTED_EDGE('',*,*,#17179,.T.);
#24584=ORIENTED_EDGE('',*,*,#17183,.F.);
#24585=ORIENTED_EDGE('',*,*,#17176,.F.);
#24586=ORIENTED_EDGE('',*,*,#17175,.F.);
#24587=ORIENTED_EDGE('',*,*,#17170,.F.);
#24588=ORIENTED_EDGE('',*,*,#17125,.F.);
#24589=ORIENTED_EDGE('',*,*,#17124,.F.);
#24590=ORIENTED_EDGE('',*,*,#17120,.F.);
#24591=ORIENTED_EDGE('',*,*,#17119,.F.);
#24592=ORIENTED_EDGE('',*,*,#17116,.F.);
#24593=ORIENTED_EDGE('',*,*,#17115,.F.);
#24594=ORIENTED_EDGE('',*,*,#17111,.F.);
#24595=ORIENTED_EDGE('',*,*,#17108,.F.);
#24596=ORIENTED_EDGE('',*,*,#17104,.F.);
#24597=ORIENTED_EDGE('',*,*,#17103,.F.);
#24598=ORIENTED_EDGE('',*,*,#17100,.F.);
#24599=ORIENTED_EDGE('',*,*,#17096,.F.);
#24600=ORIENTED_EDGE('',*,*,#17095,.F.);
#24601=ORIENTED_EDGE('',*,*,#17092,.F.);
#24602=ORIENTED_EDGE('',*,*,#17091,.F.);
#24603=ORIENTED_EDGE('',*,*,#17087,.F.);
#24604=ORIENTED_EDGE('',*,*,#17083,.F.);
#24605=ORIENTED_EDGE('',*,*,#17082,.F.);
#24606=ORIENTED_EDGE('',*,*,#17078,.F.);
#24607=ORIENTED_EDGE('',*,*,#17075,.F.);
#24608=ORIENTED_EDGE('',*,*,#17074,.F.);
#24609=ORIENTED_EDGE('',*,*,#17070,.F.);
#24610=ORIENTED_EDGE('',*,*,#17067,.F.);
#24611=ORIENTED_EDGE('',*,*,#17066,.F.);
#24612=ORIENTED_EDGE('',*,*,#17062,.F.);
#24613=ORIENTED_EDGE('',*,*,#17058,.F.);
#24614=ORIENTED_EDGE('',*,*,#17057,.F.);
#24615=ORIENTED_EDGE('',*,*,#17053,.F.);
#24616=ORIENTED_EDGE('',*,*,#17050,.F.);
#24617=ORIENTED_EDGE('',*,*,#17182,.F.);
#24618=ORIENTED_EDGE('',*,*,#17184,.F.);
#24619=ORIENTED_EDGE('',*,*,#17126,.F.);
#24620=ORIENTED_EDGE('',*,*,#17169,.F.);
#24621=ORIENTED_EDGE('',*,*,#17168,.F.);
#24622=ORIENTED_EDGE('',*,*,#17167,.F.);
#24623=ORIENTED_EDGE('',*,*,#17166,.F.);
#24624=ORIENTED_EDGE('',*,*,#17165,.F.);
#24625=ORIENTED_EDGE('',*,*,#17164,.F.);
#24626=ORIENTED_EDGE('',*,*,#17163,.F.);
#24627=ORIENTED_EDGE('',*,*,#17162,.F.);
#24628=ORIENTED_EDGE('',*,*,#17161,.F.);
#24629=ORIENTED_EDGE('',*,*,#17160,.F.);
#24630=ORIENTED_EDGE('',*,*,#17159,.F.);
#24631=ORIENTED_EDGE('',*,*,#17158,.F.);
#24632=ORIENTED_EDGE('',*,*,#17157,.F.);
#24633=ORIENTED_EDGE('',*,*,#17156,.F.);
#24634=ORIENTED_EDGE('',*,*,#17155,.F.);
#24635=ORIENTED_EDGE('',*,*,#17154,.F.);
#24636=ORIENTED_EDGE('',*,*,#17153,.F.);
#24637=ORIENTED_EDGE('',*,*,#17152,.F.);
#24638=ORIENTED_EDGE('',*,*,#17151,.F.);
#24639=ORIENTED_EDGE('',*,*,#17150,.F.);
#24640=ORIENTED_EDGE('',*,*,#17185,.T.);
#24641=ORIENTED_EDGE('',*,*,#17186,.T.);
#24642=ORIENTED_EDGE('',*,*,#17183,.T.);
#24643=ORIENTED_EDGE('',*,*,#17127,.T.);
#24644=ORIENTED_EDGE('',*,*,#17184,.T.);
#24645=ORIENTED_EDGE('',*,*,#17181,.T.);
#24646=ORIENTED_EDGE('',*,*,#17186,.F.);
#24647=ORIENTED_EDGE('',*,*,#17187,.F.);
#24648=ORIENTED_EDGE('',*,*,#17185,.F.);
#24649=ORIENTED_EDGE('',*,*,#17173,.T.);
#24650=ORIENTED_EDGE('',*,*,#17188,.T.);
#24651=ORIENTED_EDGE('',*,*,#17189,.T.);
#24652=ORIENTED_EDGE('',*,*,#17188,.F.);
#24653=ORIENTED_EDGE('',*,*,#17177,.T.);
#24654=ORIENTED_EDGE('',*,*,#17149,.T.);
#24655=ORIENTED_EDGE('',*,*,#17178,.T.);
#24656=ORIENTED_EDGE('',*,*,#17189,.F.);
#24657=ORIENTED_EDGE('',*,*,#17190,.F.);
#24658=ORIENTED_EDGE('',*,*,#17191,.T.);
#24659=ORIENTED_EDGE('',*,*,#17192,.F.);
#24660=ORIENTED_EDGE('',*,*,#17193,.F.);
#24661=ORIENTED_EDGE('',*,*,#17194,.F.);
#24662=ORIENTED_EDGE('',*,*,#17195,.F.);
#24663=ORIENTED_EDGE('',*,*,#17192,.T.);
#24664=ORIENTED_EDGE('',*,*,#17196,.T.);
#24665=ORIENTED_EDGE('',*,*,#17197,.F.);
#24666=ORIENTED_EDGE('',*,*,#17196,.F.);
#24667=ORIENTED_EDGE('',*,*,#17191,.F.);
#24668=ORIENTED_EDGE('',*,*,#17198,.T.);
#24669=ORIENTED_EDGE('',*,*,#17199,.T.);
#24670=ORIENTED_EDGE('',*,*,#17200,.T.);
#24671=ORIENTED_EDGE('',*,*,#17201,.T.);
#24672=ORIENTED_EDGE('',*,*,#17202,.T.);
#24673=ORIENTED_EDGE('',*,*,#17203,.T.);
#24674=ORIENTED_EDGE('',*,*,#17204,.T.);
#24675=ORIENTED_EDGE('',*,*,#17205,.T.);
#24676=ORIENTED_EDGE('',*,*,#17206,.T.);
#24677=ORIENTED_EDGE('',*,*,#17207,.T.);
#24678=ORIENTED_EDGE('',*,*,#17208,.T.);
#24679=ORIENTED_EDGE('',*,*,#17209,.T.);
#24680=ORIENTED_EDGE('',*,*,#17210,.T.);
#24681=ORIENTED_EDGE('',*,*,#17211,.T.);
#24682=ORIENTED_EDGE('',*,*,#17212,.T.);
#24683=ORIENTED_EDGE('',*,*,#17213,.T.);
#24684=ORIENTED_EDGE('',*,*,#17214,.T.);
#24685=ORIENTED_EDGE('',*,*,#17215,.T.);
#24686=ORIENTED_EDGE('',*,*,#17216,.T.);
#24687=ORIENTED_EDGE('',*,*,#17217,.T.);
#24688=ORIENTED_EDGE('',*,*,#17218,.T.);
#24689=ORIENTED_EDGE('',*,*,#17219,.T.);
#24690=ORIENTED_EDGE('',*,*,#17220,.T.);
#24691=ORIENTED_EDGE('',*,*,#17221,.T.);
#24692=ORIENTED_EDGE('',*,*,#17222,.T.);
#24693=ORIENTED_EDGE('',*,*,#17223,.T.);
#24694=ORIENTED_EDGE('',*,*,#17224,.T.);
#24695=ORIENTED_EDGE('',*,*,#17225,.T.);
#24696=ORIENTED_EDGE('',*,*,#17226,.T.);
#24697=ORIENTED_EDGE('',*,*,#17227,.T.);
#24698=ORIENTED_EDGE('',*,*,#17228,.T.);
#24699=ORIENTED_EDGE('',*,*,#17229,.T.);
#24700=ORIENTED_EDGE('',*,*,#17230,.T.);
#24701=ORIENTED_EDGE('',*,*,#17231,.T.);
#24702=ORIENTED_EDGE('',*,*,#17232,.T.);
#24703=ORIENTED_EDGE('',*,*,#17233,.T.);
#24704=ORIENTED_EDGE('',*,*,#17234,.T.);
#24705=ORIENTED_EDGE('',*,*,#17235,.T.);
#24706=ORIENTED_EDGE('',*,*,#17236,.T.);
#24707=ORIENTED_EDGE('',*,*,#17237,.T.);
#24708=ORIENTED_EDGE('',*,*,#17238,.T.);
#24709=ORIENTED_EDGE('',*,*,#17239,.T.);
#24710=ORIENTED_EDGE('',*,*,#17240,.T.);
#24711=ORIENTED_EDGE('',*,*,#17241,.T.);
#24712=ORIENTED_EDGE('',*,*,#17242,.T.);
#24713=ORIENTED_EDGE('',*,*,#17243,.T.);
#24714=ORIENTED_EDGE('',*,*,#17244,.T.);
#24715=ORIENTED_EDGE('',*,*,#17245,.T.);
#24716=ORIENTED_EDGE('',*,*,#17246,.T.);
#24717=ORIENTED_EDGE('',*,*,#17247,.T.);
#24718=ORIENTED_EDGE('',*,*,#17248,.T.);
#24719=ORIENTED_EDGE('',*,*,#17249,.T.);
#24720=ORIENTED_EDGE('',*,*,#17250,.T.);
#24721=ORIENTED_EDGE('',*,*,#17251,.T.);
#24722=ORIENTED_EDGE('',*,*,#17252,.T.);
#24723=ORIENTED_EDGE('',*,*,#17253,.T.);
#24724=ORIENTED_EDGE('',*,*,#17193,.T.);
#24725=ORIENTED_EDGE('',*,*,#17195,.T.);
#24726=ORIENTED_EDGE('',*,*,#17254,.T.);
#24727=ORIENTED_EDGE('',*,*,#17255,.T.);
#24728=ORIENTED_EDGE('',*,*,#17256,.T.);
#24729=ORIENTED_EDGE('',*,*,#17257,.T.);
#24730=ORIENTED_EDGE('',*,*,#17258,.T.);
#24731=ORIENTED_EDGE('',*,*,#17259,.T.);
#24732=ORIENTED_EDGE('',*,*,#17260,.T.);
#24733=ORIENTED_EDGE('',*,*,#17261,.T.);
#24734=ORIENTED_EDGE('',*,*,#17262,.T.);
#24735=ORIENTED_EDGE('',*,*,#17263,.T.);
#24736=ORIENTED_EDGE('',*,*,#17264,.T.);
#24737=ORIENTED_EDGE('',*,*,#17265,.T.);
#24738=ORIENTED_EDGE('',*,*,#17266,.T.);
#24739=ORIENTED_EDGE('',*,*,#17267,.T.);
#24740=ORIENTED_EDGE('',*,*,#17268,.T.);
#24741=ORIENTED_EDGE('',*,*,#17269,.T.);
#24742=ORIENTED_EDGE('',*,*,#17270,.T.);
#24743=ORIENTED_EDGE('',*,*,#17271,.T.);
#24744=ORIENTED_EDGE('',*,*,#17272,.T.);
#24745=ORIENTED_EDGE('',*,*,#17273,.T.);
#24746=ORIENTED_EDGE('',*,*,#17274,.T.);
#24747=ORIENTED_EDGE('',*,*,#17275,.T.);
#24748=ORIENTED_EDGE('',*,*,#17276,.T.);
#24749=ORIENTED_EDGE('',*,*,#17277,.T.);
#24750=ORIENTED_EDGE('',*,*,#17278,.T.);
#24751=ORIENTED_EDGE('',*,*,#17279,.T.);
#24752=ORIENTED_EDGE('',*,*,#17280,.T.);
#24753=ORIENTED_EDGE('',*,*,#17281,.T.);
#24754=ORIENTED_EDGE('',*,*,#17282,.T.);
#24755=ORIENTED_EDGE('',*,*,#17283,.T.);
#24756=ORIENTED_EDGE('',*,*,#17284,.T.);
#24757=ORIENTED_EDGE('',*,*,#17285,.T.);
#24758=ORIENTED_EDGE('',*,*,#17286,.T.);
#24759=ORIENTED_EDGE('',*,*,#17287,.T.);
#24760=ORIENTED_EDGE('',*,*,#17288,.T.);
#24761=ORIENTED_EDGE('',*,*,#17289,.T.);
#24762=ORIENTED_EDGE('',*,*,#17290,.T.);
#24763=ORIENTED_EDGE('',*,*,#17291,.T.);
#24764=ORIENTED_EDGE('',*,*,#17292,.T.);
#24765=ORIENTED_EDGE('',*,*,#17293,.T.);
#24766=ORIENTED_EDGE('',*,*,#17294,.T.);
#24767=ORIENTED_EDGE('',*,*,#17295,.T.);
#24768=ORIENTED_EDGE('',*,*,#17296,.T.);
#24769=ORIENTED_EDGE('',*,*,#17297,.T.);
#24770=ORIENTED_EDGE('',*,*,#17298,.T.);
#24771=ORIENTED_EDGE('',*,*,#17299,.T.);
#24772=ORIENTED_EDGE('',*,*,#17300,.T.);
#24773=ORIENTED_EDGE('',*,*,#17301,.T.);
#24774=ORIENTED_EDGE('',*,*,#17302,.T.);
#24775=ORIENTED_EDGE('',*,*,#17303,.T.);
#24776=ORIENTED_EDGE('',*,*,#17304,.T.);
#24777=ORIENTED_EDGE('',*,*,#17305,.T.);
#24778=ORIENTED_EDGE('',*,*,#17304,.F.);
#24779=ORIENTED_EDGE('',*,*,#17306,.F.);
#24780=ORIENTED_EDGE('',*,*,#17307,.T.);
#24781=ORIENTED_EDGE('',*,*,#17308,.F.);
#24782=ORIENTED_EDGE('',*,*,#17255,.F.);
#24783=ORIENTED_EDGE('',*,*,#17309,.F.);
#24784=ORIENTED_EDGE('',*,*,#17256,.F.);
#24785=ORIENTED_EDGE('',*,*,#17308,.T.);
#24786=ORIENTED_EDGE('',*,*,#17310,.T.);
#24787=ORIENTED_EDGE('',*,*,#17311,.F.);
#24788=ORIENTED_EDGE('',*,*,#17310,.F.);
#24789=ORIENTED_EDGE('',*,*,#17307,.F.);
#24790=ORIENTED_EDGE('',*,*,#17312,.F.);
#24791=ORIENTED_EDGE('',*,*,#17313,.T.);
#24792=ORIENTED_EDGE('',*,*,#17314,.F.);
#24793=ORIENTED_EDGE('',*,*,#17258,.F.);
#24794=ORIENTED_EDGE('',*,*,#17315,.F.);
#24795=ORIENTED_EDGE('',*,*,#17259,.F.);
#24796=ORIENTED_EDGE('',*,*,#17314,.T.);
#24797=ORIENTED_EDGE('',*,*,#17316,.T.);
#24798=ORIENTED_EDGE('',*,*,#17317,.F.);
#24799=ORIENTED_EDGE('',*,*,#17316,.F.);
#24800=ORIENTED_EDGE('',*,*,#17313,.F.);
#24801=ORIENTED_EDGE('',*,*,#17318,.F.);
#24802=ORIENTED_EDGE('',*,*,#17319,.T.);
#24803=ORIENTED_EDGE('',*,*,#17320,.F.);
#24804=ORIENTED_EDGE('',*,*,#17261,.F.);
#24805=ORIENTED_EDGE('',*,*,#17321,.F.);
#24806=ORIENTED_EDGE('',*,*,#17262,.F.);
#24807=ORIENTED_EDGE('',*,*,#17320,.T.);
#24808=ORIENTED_EDGE('',*,*,#17322,.T.);
#24809=ORIENTED_EDGE('',*,*,#17323,.F.);
#24810=ORIENTED_EDGE('',*,*,#17322,.F.);
#24811=ORIENTED_EDGE('',*,*,#17319,.F.);
#24812=ORIENTED_EDGE('',*,*,#17324,.F.);
#24813=ORIENTED_EDGE('',*,*,#17325,.T.);
#24814=ORIENTED_EDGE('',*,*,#17326,.F.);
#24815=ORIENTED_EDGE('',*,*,#17264,.F.);
#24816=ORIENTED_EDGE('',*,*,#17327,.F.);
#24817=ORIENTED_EDGE('',*,*,#17265,.F.);
#24818=ORIENTED_EDGE('',*,*,#17326,.T.);
#24819=ORIENTED_EDGE('',*,*,#17328,.T.);
#24820=ORIENTED_EDGE('',*,*,#17329,.F.);
#24821=ORIENTED_EDGE('',*,*,#17328,.F.);
#24822=ORIENTED_EDGE('',*,*,#17325,.F.);
#24823=ORIENTED_EDGE('',*,*,#17330,.F.);
#24824=ORIENTED_EDGE('',*,*,#17331,.T.);
#24825=ORIENTED_EDGE('',*,*,#17332,.F.);
#24826=ORIENTED_EDGE('',*,*,#17267,.F.);
#24827=ORIENTED_EDGE('',*,*,#17333,.F.);
#24828=ORIENTED_EDGE('',*,*,#17268,.F.);
#24829=ORIENTED_EDGE('',*,*,#17332,.T.);
#24830=ORIENTED_EDGE('',*,*,#17334,.T.);
#24831=ORIENTED_EDGE('',*,*,#17335,.F.);
#24832=ORIENTED_EDGE('',*,*,#17334,.F.);
#24833=ORIENTED_EDGE('',*,*,#17331,.F.);
#24834=ORIENTED_EDGE('',*,*,#17336,.F.);
#24835=ORIENTED_EDGE('',*,*,#17337,.T.);
#24836=ORIENTED_EDGE('',*,*,#17338,.F.);
#24837=ORIENTED_EDGE('',*,*,#17270,.F.);
#24838=ORIENTED_EDGE('',*,*,#17339,.F.);
#24839=ORIENTED_EDGE('',*,*,#17271,.F.);
#24840=ORIENTED_EDGE('',*,*,#17338,.T.);
#24841=ORIENTED_EDGE('',*,*,#17340,.T.);
#24842=ORIENTED_EDGE('',*,*,#17341,.F.);
#24843=ORIENTED_EDGE('',*,*,#17340,.F.);
#24844=ORIENTED_EDGE('',*,*,#17337,.F.);
#24845=ORIENTED_EDGE('',*,*,#17342,.F.);
#24846=ORIENTED_EDGE('',*,*,#17343,.T.);
#24847=ORIENTED_EDGE('',*,*,#17344,.F.);
#24848=ORIENTED_EDGE('',*,*,#17273,.F.);
#24849=ORIENTED_EDGE('',*,*,#17345,.F.);
#24850=ORIENTED_EDGE('',*,*,#17274,.F.);
#24851=ORIENTED_EDGE('',*,*,#17344,.T.);
#24852=ORIENTED_EDGE('',*,*,#17346,.T.);
#24853=ORIENTED_EDGE('',*,*,#17347,.F.);
#24854=ORIENTED_EDGE('',*,*,#17346,.F.);
#24855=ORIENTED_EDGE('',*,*,#17343,.F.);
#24856=ORIENTED_EDGE('',*,*,#17348,.F.);
#24857=ORIENTED_EDGE('',*,*,#17349,.T.);
#24858=ORIENTED_EDGE('',*,*,#17350,.F.);
#24859=ORIENTED_EDGE('',*,*,#17276,.F.);
#24860=ORIENTED_EDGE('',*,*,#17351,.F.);
#24861=ORIENTED_EDGE('',*,*,#17277,.F.);
#24862=ORIENTED_EDGE('',*,*,#17350,.T.);
#24863=ORIENTED_EDGE('',*,*,#17352,.T.);
#24864=ORIENTED_EDGE('',*,*,#17353,.F.);
#24865=ORIENTED_EDGE('',*,*,#17352,.F.);
#24866=ORIENTED_EDGE('',*,*,#17349,.F.);
#24867=ORIENTED_EDGE('',*,*,#17354,.F.);
#24868=ORIENTED_EDGE('',*,*,#17355,.T.);
#24869=ORIENTED_EDGE('',*,*,#17356,.F.);
#24870=ORIENTED_EDGE('',*,*,#17279,.F.);
#24871=ORIENTED_EDGE('',*,*,#17357,.F.);
#24872=ORIENTED_EDGE('',*,*,#17280,.F.);
#24873=ORIENTED_EDGE('',*,*,#17356,.T.);
#24874=ORIENTED_EDGE('',*,*,#17358,.T.);
#24875=ORIENTED_EDGE('',*,*,#17359,.F.);
#24876=ORIENTED_EDGE('',*,*,#17358,.F.);
#24877=ORIENTED_EDGE('',*,*,#17355,.F.);
#24878=ORIENTED_EDGE('',*,*,#17360,.F.);
#24879=ORIENTED_EDGE('',*,*,#17361,.T.);
#24880=ORIENTED_EDGE('',*,*,#17362,.F.);
#24881=ORIENTED_EDGE('',*,*,#17282,.F.);
#24882=ORIENTED_EDGE('',*,*,#17363,.F.);
#24883=ORIENTED_EDGE('',*,*,#17283,.F.);
#24884=ORIENTED_EDGE('',*,*,#17362,.T.);
#24885=ORIENTED_EDGE('',*,*,#17364,.T.);
#24886=ORIENTED_EDGE('',*,*,#17365,.F.);
#24887=ORIENTED_EDGE('',*,*,#17364,.F.);
#24888=ORIENTED_EDGE('',*,*,#17361,.F.);
#24889=ORIENTED_EDGE('',*,*,#17366,.F.);
#24890=ORIENTED_EDGE('',*,*,#17367,.T.);
#24891=ORIENTED_EDGE('',*,*,#17368,.F.);
#24892=ORIENTED_EDGE('',*,*,#17285,.F.);
#24893=ORIENTED_EDGE('',*,*,#17369,.F.);
#24894=ORIENTED_EDGE('',*,*,#17286,.F.);
#24895=ORIENTED_EDGE('',*,*,#17368,.T.);
#24896=ORIENTED_EDGE('',*,*,#17370,.T.);
#24897=ORIENTED_EDGE('',*,*,#17371,.F.);
#24898=ORIENTED_EDGE('',*,*,#17370,.F.);
#24899=ORIENTED_EDGE('',*,*,#17367,.F.);
#24900=ORIENTED_EDGE('',*,*,#17372,.F.);
#24901=ORIENTED_EDGE('',*,*,#17373,.T.);
#24902=ORIENTED_EDGE('',*,*,#17374,.F.);
#24903=ORIENTED_EDGE('',*,*,#17288,.F.);
#24904=ORIENTED_EDGE('',*,*,#17375,.F.);
#24905=ORIENTED_EDGE('',*,*,#17289,.F.);
#24906=ORIENTED_EDGE('',*,*,#17374,.T.);
#24907=ORIENTED_EDGE('',*,*,#17376,.T.);
#24908=ORIENTED_EDGE('',*,*,#17377,.F.);
#24909=ORIENTED_EDGE('',*,*,#17376,.F.);
#24910=ORIENTED_EDGE('',*,*,#17373,.F.);
#24911=ORIENTED_EDGE('',*,*,#17378,.F.);
#24912=ORIENTED_EDGE('',*,*,#17379,.T.);
#24913=ORIENTED_EDGE('',*,*,#17380,.F.);
#24914=ORIENTED_EDGE('',*,*,#17291,.F.);
#24915=ORIENTED_EDGE('',*,*,#17381,.F.);
#24916=ORIENTED_EDGE('',*,*,#17292,.F.);
#24917=ORIENTED_EDGE('',*,*,#17380,.T.);
#24918=ORIENTED_EDGE('',*,*,#17382,.T.);
#24919=ORIENTED_EDGE('',*,*,#17383,.F.);
#24920=ORIENTED_EDGE('',*,*,#17382,.F.);
#24921=ORIENTED_EDGE('',*,*,#17379,.F.);
#24922=ORIENTED_EDGE('',*,*,#17384,.F.);
#24923=ORIENTED_EDGE('',*,*,#17385,.T.);
#24924=ORIENTED_EDGE('',*,*,#17386,.F.);
#24925=ORIENTED_EDGE('',*,*,#17294,.F.);
#24926=ORIENTED_EDGE('',*,*,#17387,.F.);
#24927=ORIENTED_EDGE('',*,*,#17295,.F.);
#24928=ORIENTED_EDGE('',*,*,#17386,.T.);
#24929=ORIENTED_EDGE('',*,*,#17388,.T.);
#24930=ORIENTED_EDGE('',*,*,#17389,.F.);
#24931=ORIENTED_EDGE('',*,*,#17388,.F.);
#24932=ORIENTED_EDGE('',*,*,#17385,.F.);
#24933=ORIENTED_EDGE('',*,*,#17390,.F.);
#24934=ORIENTED_EDGE('',*,*,#17391,.T.);
#24935=ORIENTED_EDGE('',*,*,#17392,.F.);
#24936=ORIENTED_EDGE('',*,*,#17297,.F.);
#24937=ORIENTED_EDGE('',*,*,#17393,.F.);
#24938=ORIENTED_EDGE('',*,*,#17298,.F.);
#24939=ORIENTED_EDGE('',*,*,#17392,.T.);
#24940=ORIENTED_EDGE('',*,*,#17394,.T.);
#24941=ORIENTED_EDGE('',*,*,#17395,.F.);
#24942=ORIENTED_EDGE('',*,*,#17394,.F.);
#24943=ORIENTED_EDGE('',*,*,#17391,.F.);
#24944=ORIENTED_EDGE('',*,*,#17396,.F.);
#24945=ORIENTED_EDGE('',*,*,#17397,.T.);
#24946=ORIENTED_EDGE('',*,*,#17398,.F.);
#24947=ORIENTED_EDGE('',*,*,#17300,.F.);
#24948=ORIENTED_EDGE('',*,*,#17399,.F.);
#24949=ORIENTED_EDGE('',*,*,#17301,.F.);
#24950=ORIENTED_EDGE('',*,*,#17398,.T.);
#24951=ORIENTED_EDGE('',*,*,#17400,.T.);
#24952=ORIENTED_EDGE('',*,*,#17401,.F.);
#24953=ORIENTED_EDGE('',*,*,#17400,.F.);
#24954=ORIENTED_EDGE('',*,*,#17397,.F.);
#24955=ORIENTED_EDGE('',*,*,#17402,.F.);
#24956=ORIENTED_EDGE('',*,*,#17403,.T.);
#24957=ORIENTED_EDGE('',*,*,#17404,.F.);
#24958=ORIENTED_EDGE('',*,*,#17303,.F.);
#24959=ORIENTED_EDGE('',*,*,#17405,.F.);
#24960=ORIENTED_EDGE('',*,*,#17198,.F.);
#24961=ORIENTED_EDGE('',*,*,#17404,.T.);
#24962=ORIENTED_EDGE('',*,*,#17406,.T.);
#24963=ORIENTED_EDGE('',*,*,#17407,.F.);
#24964=ORIENTED_EDGE('',*,*,#17406,.F.);
#24965=ORIENTED_EDGE('',*,*,#17403,.F.);
#24966=ORIENTED_EDGE('',*,*,#17408,.F.);
#24967=ORIENTED_EDGE('',*,*,#17409,.F.);
#24968=ORIENTED_EDGE('',*,*,#17410,.T.);
#24969=ORIENTED_EDGE('',*,*,#17411,.F.);
#24970=ORIENTED_EDGE('',*,*,#17200,.F.);
#24971=ORIENTED_EDGE('',*,*,#17412,.F.);
#24972=ORIENTED_EDGE('',*,*,#17201,.F.);
#24973=ORIENTED_EDGE('',*,*,#17411,.T.);
#24974=ORIENTED_EDGE('',*,*,#17413,.T.);
#24975=ORIENTED_EDGE('',*,*,#17414,.F.);
#24976=ORIENTED_EDGE('',*,*,#17413,.F.);
#24977=ORIENTED_EDGE('',*,*,#17410,.F.);
#24978=ORIENTED_EDGE('',*,*,#17415,.F.);
#24979=ORIENTED_EDGE('',*,*,#17416,.T.);
#24980=ORIENTED_EDGE('',*,*,#17417,.F.);
#24981=ORIENTED_EDGE('',*,*,#17203,.F.);
#24982=ORIENTED_EDGE('',*,*,#17418,.F.);
#24983=ORIENTED_EDGE('',*,*,#17204,.F.);
#24984=ORIENTED_EDGE('',*,*,#17417,.T.);
#24985=ORIENTED_EDGE('',*,*,#17419,.T.);
#24986=ORIENTED_EDGE('',*,*,#17420,.F.);
#24987=ORIENTED_EDGE('',*,*,#17419,.F.);
#24988=ORIENTED_EDGE('',*,*,#17416,.F.);
#24989=ORIENTED_EDGE('',*,*,#17421,.F.);
#24990=ORIENTED_EDGE('',*,*,#17422,.T.);
#24991=ORIENTED_EDGE('',*,*,#17423,.F.);
#24992=ORIENTED_EDGE('',*,*,#17206,.F.);
#24993=ORIENTED_EDGE('',*,*,#17424,.F.);
#24994=ORIENTED_EDGE('',*,*,#17207,.F.);
#24995=ORIENTED_EDGE('',*,*,#17423,.T.);
#24996=ORIENTED_EDGE('',*,*,#17425,.T.);
#24997=ORIENTED_EDGE('',*,*,#17426,.F.);
#24998=ORIENTED_EDGE('',*,*,#17425,.F.);
#24999=ORIENTED_EDGE('',*,*,#17422,.F.);
#25000=ORIENTED_EDGE('',*,*,#17427,.F.);
#25001=ORIENTED_EDGE('',*,*,#17428,.T.);
#25002=ORIENTED_EDGE('',*,*,#17429,.F.);
#25003=ORIENTED_EDGE('',*,*,#17209,.F.);
#25004=ORIENTED_EDGE('',*,*,#17430,.F.);
#25005=ORIENTED_EDGE('',*,*,#17210,.F.);
#25006=ORIENTED_EDGE('',*,*,#17429,.T.);
#25007=ORIENTED_EDGE('',*,*,#17431,.T.);
#25008=ORIENTED_EDGE('',*,*,#17432,.F.);
#25009=ORIENTED_EDGE('',*,*,#17431,.F.);
#25010=ORIENTED_EDGE('',*,*,#17428,.F.);
#25011=ORIENTED_EDGE('',*,*,#17433,.F.);
#25012=ORIENTED_EDGE('',*,*,#17434,.T.);
#25013=ORIENTED_EDGE('',*,*,#17435,.F.);
#25014=ORIENTED_EDGE('',*,*,#17212,.F.);
#25015=ORIENTED_EDGE('',*,*,#17436,.F.);
#25016=ORIENTED_EDGE('',*,*,#17213,.F.);
#25017=ORIENTED_EDGE('',*,*,#17435,.T.);
#25018=ORIENTED_EDGE('',*,*,#17437,.T.);
#25019=ORIENTED_EDGE('',*,*,#17438,.F.);
#25020=ORIENTED_EDGE('',*,*,#17437,.F.);
#25021=ORIENTED_EDGE('',*,*,#17434,.F.);
#25022=ORIENTED_EDGE('',*,*,#17439,.F.);
#25023=ORIENTED_EDGE('',*,*,#17440,.T.);
#25024=ORIENTED_EDGE('',*,*,#17441,.F.);
#25025=ORIENTED_EDGE('',*,*,#17215,.F.);
#25026=ORIENTED_EDGE('',*,*,#17442,.F.);
#25027=ORIENTED_EDGE('',*,*,#17216,.F.);
#25028=ORIENTED_EDGE('',*,*,#17441,.T.);
#25029=ORIENTED_EDGE('',*,*,#17443,.T.);
#25030=ORIENTED_EDGE('',*,*,#17444,.F.);
#25031=ORIENTED_EDGE('',*,*,#17443,.F.);
#25032=ORIENTED_EDGE('',*,*,#17440,.F.);
#25033=ORIENTED_EDGE('',*,*,#17445,.F.);
#25034=ORIENTED_EDGE('',*,*,#17446,.T.);
#25035=ORIENTED_EDGE('',*,*,#17447,.F.);
#25036=ORIENTED_EDGE('',*,*,#17218,.F.);
#25037=ORIENTED_EDGE('',*,*,#17448,.F.);
#25038=ORIENTED_EDGE('',*,*,#17219,.F.);
#25039=ORIENTED_EDGE('',*,*,#17447,.T.);
#25040=ORIENTED_EDGE('',*,*,#17449,.T.);
#25041=ORIENTED_EDGE('',*,*,#17450,.F.);
#25042=ORIENTED_EDGE('',*,*,#17449,.F.);
#25043=ORIENTED_EDGE('',*,*,#17446,.F.);
#25044=ORIENTED_EDGE('',*,*,#17451,.F.);
#25045=ORIENTED_EDGE('',*,*,#17452,.T.);
#25046=ORIENTED_EDGE('',*,*,#17453,.F.);
#25047=ORIENTED_EDGE('',*,*,#17221,.F.);
#25048=ORIENTED_EDGE('',*,*,#17454,.F.);
#25049=ORIENTED_EDGE('',*,*,#17222,.F.);
#25050=ORIENTED_EDGE('',*,*,#17453,.T.);
#25051=ORIENTED_EDGE('',*,*,#17455,.T.);
#25052=ORIENTED_EDGE('',*,*,#17456,.F.);
#25053=ORIENTED_EDGE('',*,*,#17455,.F.);
#25054=ORIENTED_EDGE('',*,*,#17452,.F.);
#25055=ORIENTED_EDGE('',*,*,#17457,.F.);
#25056=ORIENTED_EDGE('',*,*,#17458,.T.);
#25057=ORIENTED_EDGE('',*,*,#17459,.F.);
#25058=ORIENTED_EDGE('',*,*,#17224,.F.);
#25059=ORIENTED_EDGE('',*,*,#17460,.F.);
#25060=ORIENTED_EDGE('',*,*,#17225,.F.);
#25061=ORIENTED_EDGE('',*,*,#17459,.T.);
#25062=ORIENTED_EDGE('',*,*,#17461,.T.);
#25063=ORIENTED_EDGE('',*,*,#17462,.F.);
#25064=ORIENTED_EDGE('',*,*,#17461,.F.);
#25065=ORIENTED_EDGE('',*,*,#17458,.F.);
#25066=ORIENTED_EDGE('',*,*,#17463,.F.);
#25067=ORIENTED_EDGE('',*,*,#17464,.T.);
#25068=ORIENTED_EDGE('',*,*,#17465,.F.);
#25069=ORIENTED_EDGE('',*,*,#17227,.F.);
#25070=ORIENTED_EDGE('',*,*,#17466,.F.);
#25071=ORIENTED_EDGE('',*,*,#17228,.F.);
#25072=ORIENTED_EDGE('',*,*,#17465,.T.);
#25073=ORIENTED_EDGE('',*,*,#17467,.T.);
#25074=ORIENTED_EDGE('',*,*,#17468,.F.);
#25075=ORIENTED_EDGE('',*,*,#17467,.F.);
#25076=ORIENTED_EDGE('',*,*,#17464,.F.);
#25077=ORIENTED_EDGE('',*,*,#17469,.F.);
#25078=ORIENTED_EDGE('',*,*,#17470,.T.);
#25079=ORIENTED_EDGE('',*,*,#17471,.F.);
#25080=ORIENTED_EDGE('',*,*,#17230,.F.);
#25081=ORIENTED_EDGE('',*,*,#17472,.F.);
#25082=ORIENTED_EDGE('',*,*,#17231,.F.);
#25083=ORIENTED_EDGE('',*,*,#17471,.T.);
#25084=ORIENTED_EDGE('',*,*,#17473,.T.);
#25085=ORIENTED_EDGE('',*,*,#17474,.F.);
#25086=ORIENTED_EDGE('',*,*,#17473,.F.);
#25087=ORIENTED_EDGE('',*,*,#17470,.F.);
#25088=ORIENTED_EDGE('',*,*,#17475,.F.);
#25089=ORIENTED_EDGE('',*,*,#17476,.T.);
#25090=ORIENTED_EDGE('',*,*,#17477,.F.);
#25091=ORIENTED_EDGE('',*,*,#17233,.F.);
#25092=ORIENTED_EDGE('',*,*,#17478,.F.);
#25093=ORIENTED_EDGE('',*,*,#17234,.F.);
#25094=ORIENTED_EDGE('',*,*,#17477,.T.);
#25095=ORIENTED_EDGE('',*,*,#17479,.T.);
#25096=ORIENTED_EDGE('',*,*,#17480,.F.);
#25097=ORIENTED_EDGE('',*,*,#17479,.F.);
#25098=ORIENTED_EDGE('',*,*,#17476,.F.);
#25099=ORIENTED_EDGE('',*,*,#17481,.F.);
#25100=ORIENTED_EDGE('',*,*,#17482,.T.);
#25101=ORIENTED_EDGE('',*,*,#17483,.F.);
#25102=ORIENTED_EDGE('',*,*,#17236,.F.);
#25103=ORIENTED_EDGE('',*,*,#17484,.F.);
#25104=ORIENTED_EDGE('',*,*,#17237,.F.);
#25105=ORIENTED_EDGE('',*,*,#17483,.T.);
#25106=ORIENTED_EDGE('',*,*,#17485,.T.);
#25107=ORIENTED_EDGE('',*,*,#17486,.F.);
#25108=ORIENTED_EDGE('',*,*,#17485,.F.);
#25109=ORIENTED_EDGE('',*,*,#17482,.F.);
#25110=ORIENTED_EDGE('',*,*,#17487,.F.);
#25111=ORIENTED_EDGE('',*,*,#17488,.T.);
#25112=ORIENTED_EDGE('',*,*,#17489,.F.);
#25113=ORIENTED_EDGE('',*,*,#17239,.F.);
#25114=ORIENTED_EDGE('',*,*,#17490,.F.);
#25115=ORIENTED_EDGE('',*,*,#17240,.F.);
#25116=ORIENTED_EDGE('',*,*,#17489,.T.);
#25117=ORIENTED_EDGE('',*,*,#17491,.T.);
#25118=ORIENTED_EDGE('',*,*,#17492,.F.);
#25119=ORIENTED_EDGE('',*,*,#17491,.F.);
#25120=ORIENTED_EDGE('',*,*,#17488,.F.);
#25121=ORIENTED_EDGE('',*,*,#17493,.F.);
#25122=ORIENTED_EDGE('',*,*,#17494,.T.);
#25123=ORIENTED_EDGE('',*,*,#17495,.F.);
#25124=ORIENTED_EDGE('',*,*,#17242,.F.);
#25125=ORIENTED_EDGE('',*,*,#17496,.F.);
#25126=ORIENTED_EDGE('',*,*,#17243,.F.);
#25127=ORIENTED_EDGE('',*,*,#17495,.T.);
#25128=ORIENTED_EDGE('',*,*,#17497,.T.);
#25129=ORIENTED_EDGE('',*,*,#17498,.F.);
#25130=ORIENTED_EDGE('',*,*,#17497,.F.);
#25131=ORIENTED_EDGE('',*,*,#17494,.F.);
#25132=ORIENTED_EDGE('',*,*,#17499,.F.);
#25133=ORIENTED_EDGE('',*,*,#17500,.T.);
#25134=ORIENTED_EDGE('',*,*,#17501,.F.);
#25135=ORIENTED_EDGE('',*,*,#17245,.F.);
#25136=ORIENTED_EDGE('',*,*,#17502,.F.);
#25137=ORIENTED_EDGE('',*,*,#17246,.F.);
#25138=ORIENTED_EDGE('',*,*,#17501,.T.);
#25139=ORIENTED_EDGE('',*,*,#17503,.T.);
#25140=ORIENTED_EDGE('',*,*,#17504,.F.);
#25141=ORIENTED_EDGE('',*,*,#17503,.F.);
#25142=ORIENTED_EDGE('',*,*,#17500,.F.);
#25143=ORIENTED_EDGE('',*,*,#17505,.F.);
#25144=ORIENTED_EDGE('',*,*,#17506,.T.);
#25145=ORIENTED_EDGE('',*,*,#17507,.F.);
#25146=ORIENTED_EDGE('',*,*,#17248,.F.);
#25147=ORIENTED_EDGE('',*,*,#17508,.F.);
#25148=ORIENTED_EDGE('',*,*,#17249,.F.);
#25149=ORIENTED_EDGE('',*,*,#17507,.T.);
#25150=ORIENTED_EDGE('',*,*,#17509,.T.);
#25151=ORIENTED_EDGE('',*,*,#17510,.F.);
#25152=ORIENTED_EDGE('',*,*,#17509,.F.);
#25153=ORIENTED_EDGE('',*,*,#17506,.F.);
#25154=ORIENTED_EDGE('',*,*,#17511,.F.);
#25155=ORIENTED_EDGE('',*,*,#17512,.T.);
#25156=ORIENTED_EDGE('',*,*,#17513,.F.);
#25157=ORIENTED_EDGE('',*,*,#17251,.F.);
#25158=ORIENTED_EDGE('',*,*,#17514,.F.);
#25159=ORIENTED_EDGE('',*,*,#17252,.F.);
#25160=ORIENTED_EDGE('',*,*,#17513,.T.);
#25161=ORIENTED_EDGE('',*,*,#17515,.T.);
#25162=ORIENTED_EDGE('',*,*,#17516,.F.);
#25163=ORIENTED_EDGE('',*,*,#17515,.F.);
#25164=ORIENTED_EDGE('',*,*,#17512,.F.);
#25165=ORIENTED_EDGE('',*,*,#17407,.T.);
#25166=ORIENTED_EDGE('',*,*,#17517,.T.);
#25167=ORIENTED_EDGE('',*,*,#17187,.T.);
#25168=ORIENTED_EDGE('',*,*,#17517,.F.);
#25169=ORIENTED_EDGE('',*,*,#17408,.T.);
#25170=ORIENTED_EDGE('',*,*,#17402,.T.);
#25171=ORIENTED_EDGE('',*,*,#17302,.F.);
#25172=ORIENTED_EDGE('',*,*,#17399,.T.);
#25173=ORIENTED_EDGE('',*,*,#17401,.T.);
#25174=ORIENTED_EDGE('',*,*,#17396,.T.);
#25175=ORIENTED_EDGE('',*,*,#17299,.F.);
#25176=ORIENTED_EDGE('',*,*,#17393,.T.);
#25177=ORIENTED_EDGE('',*,*,#17395,.T.);
#25178=ORIENTED_EDGE('',*,*,#17390,.T.);
#25179=ORIENTED_EDGE('',*,*,#17296,.F.);
#25180=ORIENTED_EDGE('',*,*,#17387,.T.);
#25181=ORIENTED_EDGE('',*,*,#17389,.T.);
#25182=ORIENTED_EDGE('',*,*,#17384,.T.);
#25183=ORIENTED_EDGE('',*,*,#17293,.F.);
#25184=ORIENTED_EDGE('',*,*,#17381,.T.);
#25185=ORIENTED_EDGE('',*,*,#17383,.T.);
#25186=ORIENTED_EDGE('',*,*,#17378,.T.);
#25187=ORIENTED_EDGE('',*,*,#17290,.F.);
#25188=ORIENTED_EDGE('',*,*,#17375,.T.);
#25189=ORIENTED_EDGE('',*,*,#17377,.T.);
#25190=ORIENTED_EDGE('',*,*,#17372,.T.);
#25191=ORIENTED_EDGE('',*,*,#17287,.F.);
#25192=ORIENTED_EDGE('',*,*,#17369,.T.);
#25193=ORIENTED_EDGE('',*,*,#17371,.T.);
#25194=ORIENTED_EDGE('',*,*,#17366,.T.);
#25195=ORIENTED_EDGE('',*,*,#17284,.F.);
#25196=ORIENTED_EDGE('',*,*,#17363,.T.);
#25197=ORIENTED_EDGE('',*,*,#17365,.T.);
#25198=ORIENTED_EDGE('',*,*,#17360,.T.);
#25199=ORIENTED_EDGE('',*,*,#17281,.F.);
#25200=ORIENTED_EDGE('',*,*,#17357,.T.);
#25201=ORIENTED_EDGE('',*,*,#17359,.T.);
#25202=ORIENTED_EDGE('',*,*,#17354,.T.);
#25203=ORIENTED_EDGE('',*,*,#17278,.F.);
#25204=ORIENTED_EDGE('',*,*,#17351,.T.);
#25205=ORIENTED_EDGE('',*,*,#17353,.T.);
#25206=ORIENTED_EDGE('',*,*,#17348,.T.);
#25207=ORIENTED_EDGE('',*,*,#17275,.F.);
#25208=ORIENTED_EDGE('',*,*,#17345,.T.);
#25209=ORIENTED_EDGE('',*,*,#17347,.T.);
#25210=ORIENTED_EDGE('',*,*,#17342,.T.);
#25211=ORIENTED_EDGE('',*,*,#17272,.F.);
#25212=ORIENTED_EDGE('',*,*,#17339,.T.);
#25213=ORIENTED_EDGE('',*,*,#17341,.T.);
#25214=ORIENTED_EDGE('',*,*,#17336,.T.);
#25215=ORIENTED_EDGE('',*,*,#17269,.F.);
#25216=ORIENTED_EDGE('',*,*,#17333,.T.);
#25217=ORIENTED_EDGE('',*,*,#17335,.T.);
#25218=ORIENTED_EDGE('',*,*,#17330,.T.);
#25219=ORIENTED_EDGE('',*,*,#17266,.F.);
#25220=ORIENTED_EDGE('',*,*,#17327,.T.);
#25221=ORIENTED_EDGE('',*,*,#17329,.T.);
#25222=ORIENTED_EDGE('',*,*,#17324,.T.);
#25223=ORIENTED_EDGE('',*,*,#17263,.F.);
#25224=ORIENTED_EDGE('',*,*,#17321,.T.);
#25225=ORIENTED_EDGE('',*,*,#17323,.T.);
#25226=ORIENTED_EDGE('',*,*,#17318,.T.);
#25227=ORIENTED_EDGE('',*,*,#17260,.F.);
#25228=ORIENTED_EDGE('',*,*,#17315,.T.);
#25229=ORIENTED_EDGE('',*,*,#17317,.T.);
#25230=ORIENTED_EDGE('',*,*,#17312,.T.);
#25231=ORIENTED_EDGE('',*,*,#17257,.F.);
#25232=ORIENTED_EDGE('',*,*,#17309,.T.);
#25233=ORIENTED_EDGE('',*,*,#17311,.T.);
#25234=ORIENTED_EDGE('',*,*,#17306,.T.);
#25235=ORIENTED_EDGE('',*,*,#17254,.F.);
#25236=ORIENTED_EDGE('',*,*,#17194,.T.);
#25237=ORIENTED_EDGE('',*,*,#17197,.T.);
#25238=ORIENTED_EDGE('',*,*,#17190,.T.);
#25239=ORIENTED_EDGE('',*,*,#17253,.F.);
#25240=ORIENTED_EDGE('',*,*,#17514,.T.);
#25241=ORIENTED_EDGE('',*,*,#17516,.T.);
#25242=ORIENTED_EDGE('',*,*,#17511,.T.);
#25243=ORIENTED_EDGE('',*,*,#17250,.F.);
#25244=ORIENTED_EDGE('',*,*,#17508,.T.);
#25245=ORIENTED_EDGE('',*,*,#17510,.T.);
#25246=ORIENTED_EDGE('',*,*,#17505,.T.);
#25247=ORIENTED_EDGE('',*,*,#17247,.F.);
#25248=ORIENTED_EDGE('',*,*,#17502,.T.);
#25249=ORIENTED_EDGE('',*,*,#17504,.T.);
#25250=ORIENTED_EDGE('',*,*,#17499,.T.);
#25251=ORIENTED_EDGE('',*,*,#17244,.F.);
#25252=ORIENTED_EDGE('',*,*,#17496,.T.);
#25253=ORIENTED_EDGE('',*,*,#17498,.T.);
#25254=ORIENTED_EDGE('',*,*,#17493,.T.);
#25255=ORIENTED_EDGE('',*,*,#17241,.F.);
#25256=ORIENTED_EDGE('',*,*,#17490,.T.);
#25257=ORIENTED_EDGE('',*,*,#17492,.T.);
#25258=ORIENTED_EDGE('',*,*,#17487,.T.);
#25259=ORIENTED_EDGE('',*,*,#17238,.F.);
#25260=ORIENTED_EDGE('',*,*,#17484,.T.);
#25261=ORIENTED_EDGE('',*,*,#17486,.T.);
#25262=ORIENTED_EDGE('',*,*,#17481,.T.);
#25263=ORIENTED_EDGE('',*,*,#17235,.F.);
#25264=ORIENTED_EDGE('',*,*,#17478,.T.);
#25265=ORIENTED_EDGE('',*,*,#17480,.T.);
#25266=ORIENTED_EDGE('',*,*,#17475,.T.);
#25267=ORIENTED_EDGE('',*,*,#17232,.F.);
#25268=ORIENTED_EDGE('',*,*,#17472,.T.);
#25269=ORIENTED_EDGE('',*,*,#17474,.T.);
#25270=ORIENTED_EDGE('',*,*,#17469,.T.);
#25271=ORIENTED_EDGE('',*,*,#17229,.F.);
#25272=ORIENTED_EDGE('',*,*,#17466,.T.);
#25273=ORIENTED_EDGE('',*,*,#17468,.T.);
#25274=ORIENTED_EDGE('',*,*,#17463,.T.);
#25275=ORIENTED_EDGE('',*,*,#17226,.F.);
#25276=ORIENTED_EDGE('',*,*,#17460,.T.);
#25277=ORIENTED_EDGE('',*,*,#17462,.T.);
#25278=ORIENTED_EDGE('',*,*,#17457,.T.);
#25279=ORIENTED_EDGE('',*,*,#17223,.F.);
#25280=ORIENTED_EDGE('',*,*,#17454,.T.);
#25281=ORIENTED_EDGE('',*,*,#17456,.T.);
#25282=ORIENTED_EDGE('',*,*,#17451,.T.);
#25283=ORIENTED_EDGE('',*,*,#17220,.F.);
#25284=ORIENTED_EDGE('',*,*,#17448,.T.);
#25285=ORIENTED_EDGE('',*,*,#17450,.T.);
#25286=ORIENTED_EDGE('',*,*,#17445,.T.);
#25287=ORIENTED_EDGE('',*,*,#17217,.F.);
#25288=ORIENTED_EDGE('',*,*,#17442,.T.);
#25289=ORIENTED_EDGE('',*,*,#17444,.T.);
#25290=ORIENTED_EDGE('',*,*,#17439,.T.);
#25291=ORIENTED_EDGE('',*,*,#17214,.F.);
#25292=ORIENTED_EDGE('',*,*,#17436,.T.);
#25293=ORIENTED_EDGE('',*,*,#17438,.T.);
#25294=ORIENTED_EDGE('',*,*,#17433,.T.);
#25295=ORIENTED_EDGE('',*,*,#17211,.F.);
#25296=ORIENTED_EDGE('',*,*,#17430,.T.);
#25297=ORIENTED_EDGE('',*,*,#17432,.T.);
#25298=ORIENTED_EDGE('',*,*,#17427,.T.);
#25299=ORIENTED_EDGE('',*,*,#17208,.F.);
#25300=ORIENTED_EDGE('',*,*,#17424,.T.);
#25301=ORIENTED_EDGE('',*,*,#17426,.T.);
#25302=ORIENTED_EDGE('',*,*,#17421,.T.);
#25303=ORIENTED_EDGE('',*,*,#17205,.F.);
#25304=ORIENTED_EDGE('',*,*,#17418,.T.);
#25305=ORIENTED_EDGE('',*,*,#17420,.T.);
#25306=ORIENTED_EDGE('',*,*,#17415,.T.);
#25307=ORIENTED_EDGE('',*,*,#17202,.F.);
#25308=ORIENTED_EDGE('',*,*,#17412,.T.);
#25309=ORIENTED_EDGE('',*,*,#17414,.T.);
#25310=ORIENTED_EDGE('',*,*,#17409,.T.);
#25311=ORIENTED_EDGE('',*,*,#17199,.F.);
#25312=ORIENTED_EDGE('',*,*,#17405,.T.);
#25313=ORIENTED_EDGE('',*,*,#17305,.F.);
#25314=ORIENTED_EDGE('',*,*,#17518,.T.);
#25315=ORIENTED_EDGE('',*,*,#17519,.T.);
#25316=ORIENTED_EDGE('',*,*,#17520,.T.);
#25317=ORIENTED_EDGE('',*,*,#17521,.T.);
#25318=ORIENTED_EDGE('',*,*,#17522,.T.);
#25319=ORIENTED_EDGE('',*,*,#17523,.T.);
#25320=ORIENTED_EDGE('',*,*,#17524,.F.);
#25321=ORIENTED_EDGE('',*,*,#17525,.T.);
#25322=ORIENTED_EDGE('',*,*,#17526,.F.);
#25323=ORIENTED_EDGE('',*,*,#17527,.T.);
#25324=ORIENTED_EDGE('',*,*,#17528,.F.);
#25325=ORIENTED_EDGE('',*,*,#17529,.T.);
#25326=ORIENTED_EDGE('',*,*,#17530,.F.);
#25327=ORIENTED_EDGE('',*,*,#17531,.T.);
#25328=ORIENTED_EDGE('',*,*,#17532,.F.);
#25329=ORIENTED_EDGE('',*,*,#17533,.T.);
#25330=ORIENTED_EDGE('',*,*,#17534,.F.);
#25331=ORIENTED_EDGE('',*,*,#17535,.T.);
#25332=ORIENTED_EDGE('',*,*,#17536,.T.);
#25333=ORIENTED_EDGE('',*,*,#17535,.F.);
#25334=ORIENTED_EDGE('',*,*,#17533,.F.);
#25335=ORIENTED_EDGE('',*,*,#17531,.F.);
#25336=ORIENTED_EDGE('',*,*,#17529,.F.);
#25337=ORIENTED_EDGE('',*,*,#17527,.F.);
#25338=ORIENTED_EDGE('',*,*,#17525,.F.);
#25339=ORIENTED_EDGE('',*,*,#17536,.F.);
#25340=ORIENTED_EDGE('',*,*,#17518,.F.);
#25341=ORIENTED_EDGE('',*,*,#17537,.T.);
#25342=ORIENTED_EDGE('',*,*,#17524,.T.);
#25343=ORIENTED_EDGE('',*,*,#17538,.F.);
#25344=ORIENTED_EDGE('',*,*,#17523,.F.);
#25345=ORIENTED_EDGE('',*,*,#17539,.T.);
#25346=ORIENTED_EDGE('',*,*,#17534,.T.);
#25347=ORIENTED_EDGE('',*,*,#17537,.F.);
#25348=ORIENTED_EDGE('',*,*,#17522,.F.);
#25349=ORIENTED_EDGE('',*,*,#17540,.T.);
#25350=ORIENTED_EDGE('',*,*,#17532,.T.);
#25351=ORIENTED_EDGE('',*,*,#17539,.F.);
#25352=ORIENTED_EDGE('',*,*,#17521,.F.);
#25353=ORIENTED_EDGE('',*,*,#17541,.T.);
#25354=ORIENTED_EDGE('',*,*,#17530,.T.);
#25355=ORIENTED_EDGE('',*,*,#17540,.F.);
#25356=ORIENTED_EDGE('',*,*,#17520,.F.);
#25357=ORIENTED_EDGE('',*,*,#17542,.T.);
#25358=ORIENTED_EDGE('',*,*,#17528,.T.);
#25359=ORIENTED_EDGE('',*,*,#17541,.F.);
#25360=ORIENTED_EDGE('',*,*,#17519,.F.);
#25361=ORIENTED_EDGE('',*,*,#17538,.T.);
#25362=ORIENTED_EDGE('',*,*,#17526,.T.);
#25363=ORIENTED_EDGE('',*,*,#17542,.F.);
#25364=ORIENTED_EDGE('',*,*,#17543,.T.);
#25365=ORIENTED_EDGE('',*,*,#17544,.T.);
#25366=ORIENTED_EDGE('',*,*,#17545,.F.);
#25367=ORIENTED_EDGE('',*,*,#17544,.F.);
#25368=ORIENTED_EDGE('',*,*,#17546,.F.);
#25369=ORIENTED_EDGE('',*,*,#17545,.T.);
#25370=ORIENTED_EDGE('',*,*,#17547,.F.);
#25371=ORIENTED_EDGE('',*,*,#17548,.T.);
#25372=ORIENTED_EDGE('',*,*,#17546,.T.);
#25373=ORIENTED_EDGE('',*,*,#17548,.F.);
#25374=ORIENTED_EDGE('',*,*,#17547,.T.);
#25375=ORIENTED_EDGE('',*,*,#17549,.T.);
#25376=ORIENTED_EDGE('',*,*,#17550,.F.);
#25377=ORIENTED_EDGE('',*,*,#17549,.F.);
#25378=ORIENTED_EDGE('',*,*,#17550,.T.);
#25379=ORIENTED_EDGE('',*,*,#17551,.F.);
#25380=ORIENTED_EDGE('',*,*,#17543,.F.);
#25381=ORIENTED_EDGE('',*,*,#17552,.T.);
#25382=ORIENTED_EDGE('',*,*,#17551,.T.);
#25383=ORIENTED_EDGE('',*,*,#17552,.F.);
#25384=ORIENTED_EDGE('',*,*,#17553,.T.);
#25385=ORIENTED_EDGE('',*,*,#17554,.T.);
#25386=ORIENTED_EDGE('',*,*,#17555,.T.);
#25387=ORIENTED_EDGE('',*,*,#17554,.F.);
#25388=ORIENTED_EDGE('',*,*,#17553,.F.);
#25389=ORIENTED_EDGE('',*,*,#17556,.T.);
#25390=ORIENTED_EDGE('',*,*,#17557,.F.);
#25391=ORIENTED_EDGE('',*,*,#17556,.F.);
#25392=ORIENTED_EDGE('',*,*,#17558,.T.);
#25393=ORIENTED_EDGE('',*,*,#17555,.F.);
#25394=ORIENTED_EDGE('',*,*,#17559,.F.);
#25395=ORIENTED_EDGE('',*,*,#17560,.T.);
#25396=ORIENTED_EDGE('',*,*,#17561,.F.);
#25397=ORIENTED_EDGE('',*,*,#17560,.F.);
#25398=ORIENTED_EDGE('',*,*,#17559,.T.);
#25399=ORIENTED_EDGE('',*,*,#17562,.T.);
#25400=ORIENTED_EDGE('',*,*,#17563,.F.);
#25401=ORIENTED_EDGE('',*,*,#17562,.F.);
#25402=ORIENTED_EDGE('',*,*,#17563,.T.);
#25403=ORIENTED_EDGE('',*,*,#17564,.F.);
#25404=ORIENTED_EDGE('',*,*,#17565,.F.);
#25405=ORIENTED_EDGE('',*,*,#17566,.T.);
#25406=ORIENTED_EDGE('',*,*,#17564,.T.);
#25407=ORIENTED_EDGE('',*,*,#17566,.F.);
#25408=ORIENTED_EDGE('',*,*,#17565,.T.);
#25409=ORIENTED_EDGE('',*,*,#17557,.T.);
#25410=ORIENTED_EDGE('',*,*,#17567,.F.);
#25411=ORIENTED_EDGE('',*,*,#17568,.F.);
#25412=ORIENTED_EDGE('',*,*,#17569,.F.);
#25413=ORIENTED_EDGE('',*,*,#17570,.F.);
#25414=ORIENTED_EDGE('',*,*,#17571,.F.);
#25415=ORIENTED_EDGE('',*,*,#17572,.F.);
#25416=ORIENTED_EDGE('',*,*,#17573,.T.);
#25417=ORIENTED_EDGE('',*,*,#17558,.F.);
#25418=ORIENTED_EDGE('',*,*,#17573,.F.);
#25419=ORIENTED_EDGE('',*,*,#17567,.T.);
#25420=ORIENTED_EDGE('',*,*,#17574,.F.);
#25421=ORIENTED_EDGE('',*,*,#17575,.F.);
#25422=ORIENTED_EDGE('',*,*,#17576,.T.);
#25423=ORIENTED_EDGE('',*,*,#17572,.T.);
#25424=ORIENTED_EDGE('',*,*,#17577,.F.);
#25425=ORIENTED_EDGE('',*,*,#17578,.F.);
#25426=ORIENTED_EDGE('',*,*,#17574,.T.);
#25427=ORIENTED_EDGE('',*,*,#17571,.T.);
#25428=ORIENTED_EDGE('',*,*,#17579,.F.);
#25429=ORIENTED_EDGE('',*,*,#17580,.F.);
#25430=ORIENTED_EDGE('',*,*,#17577,.T.);
#25431=ORIENTED_EDGE('',*,*,#17570,.T.);
#25432=ORIENTED_EDGE('',*,*,#17581,.F.);
#25433=ORIENTED_EDGE('',*,*,#17582,.F.);
#25434=ORIENTED_EDGE('',*,*,#17579,.T.);
#25435=ORIENTED_EDGE('',*,*,#17569,.T.);
#25436=ORIENTED_EDGE('',*,*,#17583,.F.);
#25437=ORIENTED_EDGE('',*,*,#17584,.F.);
#25438=ORIENTED_EDGE('',*,*,#17581,.T.);
#25439=ORIENTED_EDGE('',*,*,#17568,.T.);
#25440=ORIENTED_EDGE('',*,*,#17576,.F.);
#25441=ORIENTED_EDGE('',*,*,#17585,.F.);
#25442=ORIENTED_EDGE('',*,*,#17583,.T.);
#25443=ORIENTED_EDGE('',*,*,#17580,.T.);
#25444=ORIENTED_EDGE('',*,*,#17582,.T.);
#25445=ORIENTED_EDGE('',*,*,#17584,.T.);
#25446=ORIENTED_EDGE('',*,*,#17585,.T.);
#25447=ORIENTED_EDGE('',*,*,#17575,.T.);
#25448=ORIENTED_EDGE('',*,*,#17578,.T.);
#25449=ORIENTED_EDGE('',*,*,#17561,.T.);
#25450=CONICAL_SURFACE('',#27100,1.9525,0.785398163397448);
#25451=CONICAL_SURFACE('',#27107,1.9525,0.785398163397448);
#25452=CONICAL_SURFACE('',#27114,1.80249999999999,1.02974425867665);
#25453=CONICAL_SURFACE('',#27115,1.80249999999999,1.02974425867665);
#25454=CONICAL_SURFACE('',#27116,1.9525,0.785398163397448);
#25455=CONICAL_SURFACE('',#27123,1.9525,0.785398163397448);
#25456=CONICAL_SURFACE('',#27130,0.901249999999996,1.02974425867665);
#25457=CONICAL_SURFACE('',#27131,0.901249999999996,1.02974425867665);
#25458=CONICAL_SURFACE('',#27144,1.9525,0.785398163397445);
#25459=CONICAL_SURFACE('',#27154,1.9525,0.785398163397444);
#25460=CONICAL_SURFACE('',#27158,1.9525,0.785398163397444);
#25461=CONICAL_SURFACE('',#27162,1.9525,0.785398163397445);
#25462=CONICAL_SURFACE('',#27166,6.563,0.785398163397448);
#25463=CONICAL_SURFACE('',#27208,1.903,0.785398163397448);
#25464=CONICAL_SURFACE('',#27231,1.903,0.785398163397448);
#25465=CONICAL_SURFACE('',#27235,1.903,0.785398163397448);
#25466=CONICAL_SURFACE('',#27239,1.903,0.785398163397448);
#25467=CONICAL_SURFACE('',#27243,1.9525,0.785398163397456);
#25468=CONICAL_SURFACE('',#27261,1.9525,0.785398163397452);
#25469=CONICAL_SURFACE('',#27264,1.9525,0.785398163397452);
#25470=CONICAL_SURFACE('',#27267,1.9525,0.785398163397456);
#25471=CONICAL_SURFACE('',#27283,3.04,0.785398163397456);
#25472=CONICAL_SURFACE('',#27286,3.04,0.785398163397459);
#25473=CONICAL_SURFACE('',#27289,3.04,0.785398163397448);
#25474=CONICAL_SURFACE('',#27292,3.04,0.785398163397448);
#25475=CONICAL_SURFACE('',#27313,2.625,0.785398163397456);
#25476=CONICAL_SURFACE('',#27317,0.949999999999994,0.785398163397451);
#25477=CONICAL_SURFACE('',#27320,0.949999999999994,0.785398163397459);
#25478=CONICAL_SURFACE('',#27323,0.949999999999996,0.785398163397459);
#25479=CONICAL_SURFACE('',#27326,0.949999999999994,0.785398163397451);
#25480=CONICAL_SURFACE('',#27329,2.625,0.785398163397448);
#25481=CONICAL_SURFACE('',#27377,1.65,0.785398163397459);
#25482=CONICAL_SURFACE('',#27384,1.55,1.02974425867665);
#25483=CONICAL_SURFACE('',#27388,3.105,0.785398163397459);
#25484=CONICAL_SURFACE('',#27394,5.35,0.785398163397445);
#25485=CONICAL_SURFACE('',#27635,1.2885,0.785398163397446);
#25486=CONICAL_SURFACE('',#27824,2.6,0.785398163397444);
#25487=CONICAL_SURFACE('',#27828,1.49337567297406,0.785398163397459);
#25488=CONICAL_SURFACE('',#27868,1.44337567297406,1.02974425867665);
#25489=CONICAL_SURFACE('',#27873,1.87799999999999,0.785398163397448);
#25490=CONICAL_SURFACE('',#27901,1.87799999999999,0.785398163397448);
#25491=CONICAL_SURFACE('',#27905,1.878,0.785398163397448);
#25492=CONICAL_SURFACE('',#27909,1.878,0.785398163397448);
#25493=CONICAL_SURFACE('',#27913,1.878,0.785398163397459);
#25494=CONICAL_SURFACE('',#27917,1.87799999999999,0.785398163397448);
#25495=CONICAL_SURFACE('',#27921,1.878,0.785398163397459);
#25496=CONICAL_SURFACE('',#27925,1.878,0.785398163397459);
#25497=CONICAL_SURFACE('',#27929,1.878,0.785398163397448);
#25498=CONICAL_SURFACE('',#27933,1.878,0.785398163397448);
#25499=CONICAL_SURFACE('',#27937,1.87799999999999,0.785398163397448);
#25500=CONICAL_SURFACE('',#27941,1.878,0.785398163397448);
#25501=CONICAL_SURFACE('',#27945,1.878,0.785398163397448);
#25502=CONICAL_SURFACE('',#27949,1.878,0.785398163397459);
#25503=CONICAL_SURFACE('',#27953,1.878,0.785398163397459);
#25504=CONICAL_SURFACE('',#27957,1.878,0.785398163397459);
#25505=CONICAL_SURFACE('',#27961,1.878,0.785398163397459);
#25506=CONICAL_SURFACE('',#27965,1.878,0.785398163397459);
#25507=CONICAL_SURFACE('',#27969,1.878,0.785398163397448);
#25508=CONICAL_SURFACE('',#27973,1.878,0.785398163397448);
#25509=CONICAL_SURFACE('',#27977,1.87799999999999,0.785398163397448);
#25510=CONICAL_SURFACE('',#27982,4.6375,0.785398163397448);
#25511=CONICAL_SURFACE('',#27985,4.6375,0.785398163397448);
#25512=CONICAL_SURFACE('',#27991,4.6375,0.785398163397448);
#25513=CONICAL_SURFACE('',#27995,4.6375,0.785398163397448);
#25514=CONICAL_SURFACE('',#28002,4.6625,0.785398163397448);
#25515=CONICAL_SURFACE('',#28006,4.6625,0.785398163397448);
#25516=CONICAL_SURFACE('',#28018,4.6625,0.785398163397448);
#25517=CONICAL_SURFACE('',#28021,4.6625,0.785398163397448);
#25518=CONICAL_SURFACE('',#28336,1.903,0.785398163397448);
#25519=CONICAL_SURFACE('',#28349,1.903,0.785398163397448);
#25520=CONICAL_SURFACE('',#28353,1.903,0.785398163397448);
#25521=CONICAL_SURFACE('',#28357,1.903,0.785398163397448);
#25522=CONICAL_SURFACE('',#28361,1.903,0.785398163397448);
#25523=CONICAL_SURFACE('',#28365,1.903,0.785398163397448);
#25524=CONICAL_SURFACE('',#28369,1.903,0.785398163397448);
#25525=CONICAL_SURFACE('',#28373,1.903,0.785398163397448);
#25526=CONICAL_SURFACE('',#28413,1.9525,0.785398163397452);
#25527=CONICAL_SURFACE('',#28423,1.9525,0.785398163397452);
#25528=CONICAL_SURFACE('',#28433,0.90125,1.02974425867665);
#25529=CONICAL_SURFACE('',#28434,0.90125,1.02974425867665);
#25530=CONICAL_SURFACE('',#28439,0.90125,1.02974425867665);
#25531=CONICAL_SURFACE('',#28440,0.90125,1.02974425867665);
#25532=CONICAL_SURFACE('',#28445,1.9525,0.785398163397448);
#25533=CONICAL_SURFACE('',#28448,1.8025,1.02974425867665);
#25534=CONICAL_SURFACE('',#28449,1.9525,0.785398163397448);
#25535=CONICAL_SURFACE('',#28452,0.901250000000005,1.02974425867665);
#25536=CONICAL_SURFACE('',#28486,1.52934,0.785398163397448);
#25537=CONICAL_SURFACE('',#28493,2.7202,0.785398163397452);
#25538=CONICAL_SURFACE('',#28686,0.801975608296219,1.02974425867665);
#25539=CONICAL_SURFACE('',#28720,1.52934,0.785398163397445);
#25540=CONICAL_SURFACE('',#28727,2.7202,0.785398163397445);
#25541=CONICAL_SURFACE('',#28920,1.60395121659243,1.02974425867665);
#25542=CONICAL_SURFACE('',#28964,1.52934,0.785398163397448);
#25543=CONICAL_SURFACE('',#28971,2.7202,0.785398163397434);
#25544=CONICAL_SURFACE('',#29164,1.60395121659244,1.02974425867666);
#25545=CONICAL_SURFACE('',#29172,2.0312,0.785398163397493);
#25546=CONICAL_SURFACE('',#29179,4.6875,0.785398163397478);
#25547=CONICAL_SURFACE('',#29185,1.92749999999999,0.785398163397448);
#25548=CONICAL_SURFACE('',#29195,3.5,0.785398163397426);
#25549=CONICAL_SURFACE('',#29202,4.42651513084632,1.04719755119659);
#25550=ADVANCED_FACE('',(#2357),#25450,.F.);
#25551=ADVANCED_FACE('',(#2358),#2142,.F.);
#25552=ADVANCED_FACE('',(#2359,#961),#1123,.T.);
#25553=ADVANCED_FACE('',(#2360),#25451,.F.);
#25554=ADVANCED_FACE('',(#2361),#2143,.F.);
#25555=ADVANCED_FACE('',(#2362,#962),#1124,.T.);
#25556=ADVANCED_FACE('',(#2363),#25452,.F.);
#25557=ADVANCED_FACE('',(#2364),#25453,.F.);
#25558=ADVANCED_FACE('',(#2365),#25454,.F.);
#25559=ADVANCED_FACE('',(#2366),#2144,.F.);
#25560=ADVANCED_FACE('',(#2367,#963),#1125,.T.);
#25561=ADVANCED_FACE('',(#2368),#25455,.F.);
#25562=ADVANCED_FACE('',(#2369),#2145,.F.);
#25563=ADVANCED_FACE('',(#2370,#964),#1126,.T.);
#25564=ADVANCED_FACE('',(#2371),#25456,.F.);
#25565=ADVANCED_FACE('',(#2372),#25457,.F.);
#25566=ADVANCED_FACE('',(#2373),#2146,.F.);
#25567=ADVANCED_FACE('',(#2374),#2147,.F.);
#25568=ADVANCED_FACE('',(#2375),#2148,.F.);
#25569=ADVANCED_FACE('',(#2376),#2149,.F.);
#25570=ADVANCED_FACE('',(#2377),#25458,.F.);
#25571=ADVANCED_FACE('',(#2378,#965,#966,#967,#968,#969,#970,#971,#972,
#973),#1127,.T.);
#25572=ADVANCED_FACE('',(#2379),#2150,.F.);
#25573=ADVANCED_FACE('',(#2380),#25459,.F.);
#25574=ADVANCED_FACE('',(#2381),#2151,.F.);
#25575=ADVANCED_FACE('',(#2382),#25460,.F.);
#25576=ADVANCED_FACE('',(#2383),#2152,.F.);
#25577=ADVANCED_FACE('',(#2384),#25461,.F.);
#25578=ADVANCED_FACE('',(#2385),#2153,.F.);
#25579=ADVANCED_FACE('',(#2386),#25462,.F.);
#25580=ADVANCED_FACE('',(#2387),#2154,.F.);
#25581=ADVANCED_FACE('',(#2388),#1128,.T.);
#25582=ADVANCED_FACE('',(#2389),#1129,.T.);
#25583=ADVANCED_FACE('',(#2390),#1130,.T.);
#25584=ADVANCED_FACE('',(#2391),#1131,.T.);
#25585=ADVANCED_FACE('',(#2392),#1132,.T.);
#25586=ADVANCED_FACE('',(#2393),#1133,.T.);
#25587=ADVANCED_FACE('',(#2394),#1134,.T.);
#25588=ADVANCED_FACE('',(#2395),#1135,.T.);
#25589=ADVANCED_FACE('',(#2396),#1136,.T.);
#25590=ADVANCED_FACE('',(#2397),#1137,.T.);
#25591=ADVANCED_FACE('',(#2398),#1138,.T.);
#25592=ADVANCED_FACE('',(#2399),#1139,.T.);
#25593=ADVANCED_FACE('',(#2400),#1140,.T.);
#25594=ADVANCED_FACE('',(#2401),#1141,.T.);
#25595=ADVANCED_FACE('',(#2402),#1142,.T.);
#25596=ADVANCED_FACE('',(#2403),#1143,.T.);
#25597=ADVANCED_FACE('',(#2404),#1144,.T.);
#25598=ADVANCED_FACE('',(#2405),#1145,.T.);
#25599=ADVANCED_FACE('',(#2406),#1146,.T.);
#25600=ADVANCED_FACE('',(#2407),#1147,.T.);
#25601=ADVANCED_FACE('',(#2408),#1148,.T.);
#25602=ADVANCED_FACE('',(#2409),#1149,.F.);
#25603=ADVANCED_FACE('',(#2410),#1150,.F.);
#25604=ADVANCED_FACE('',(#2411),#1151,.F.);
#25605=ADVANCED_FACE('',(#2412),#1152,.T.);
#25606=ADVANCED_FACE('',(#2413),#1153,.F.);
#25607=ADVANCED_FACE('',(#2414),#1154,.F.);
#25608=ADVANCED_FACE('',(#2415),#1155,.F.);
#25609=ADVANCED_FACE('',(#2416),#1156,.F.);
#25610=ADVANCED_FACE('',(#2417),#1157,.F.);
#25611=ADVANCED_FACE('',(#2418),#1158,.F.);
#25612=ADVANCED_FACE('',(#2419),#1159,.T.);
#25613=ADVANCED_FACE('',(#2420),#1160,.T.);
#25614=ADVANCED_FACE('',(#2421,#974,#975,#976,#977,#978,#979,#980,#981,
#982),#1161,.F.);
#25615=ADVANCED_FACE('',(#2422),#1162,.F.);
#25616=ADVANCED_FACE('',(#2423),#1163,.F.);
#25617=ADVANCED_FACE('',(#2424),#1164,.F.);
#25618=ADVANCED_FACE('',(#2425),#25463,.F.);
#25619=ADVANCED_FACE('',(#2426,#983,#984,#985,#986,#987,#988,#989,#990,
#991),#1165,.F.);
#25620=ADVANCED_FACE('',(#2427),#2155,.F.);
#25621=ADVANCED_FACE('',(#2428),#25464,.F.);
#25622=ADVANCED_FACE('',(#2429),#2156,.F.);
#25623=ADVANCED_FACE('',(#2430),#25465,.F.);
#25624=ADVANCED_FACE('',(#2431),#2157,.F.);
#25625=ADVANCED_FACE('',(#2432),#25466,.F.);
#25626=ADVANCED_FACE('',(#2433),#2158,.F.);
#25627=ADVANCED_FACE('',(#2434),#25467,.F.);
#25628=ADVANCED_FACE('',(#2435,#992,#993,#994,#995,#996,#997,#998,#999,
#1000),#1166,.T.);
#25629=ADVANCED_FACE('',(#2436),#2159,.F.);
#25630=ADVANCED_FACE('',(#2437),#25468,.F.);
#25631=ADVANCED_FACE('',(#2438),#2160,.F.);
#25632=ADVANCED_FACE('',(#2439),#25469,.F.);
#25633=ADVANCED_FACE('',(#2440),#2161,.F.);
#25634=ADVANCED_FACE('',(#2441),#25470,.F.);
#25635=ADVANCED_FACE('',(#2442),#2162,.F.);
#25636=ADVANCED_FACE('',(#2443),#1167,.T.);
#25637=ADVANCED_FACE('',(#2444),#1168,.T.);
#25638=ADVANCED_FACE('',(#2445),#1169,.T.);
#25639=ADVANCED_FACE('',(#2446),#1170,.T.);
#25640=ADVANCED_FACE('',(#2447),#1171,.T.);
#25641=ADVANCED_FACE('',(#2448),#1172,.T.);
#25642=ADVANCED_FACE('',(#2449),#1173,.T.);
#25643=ADVANCED_FACE('',(#2450),#1174,.T.);
#25644=ADVANCED_FACE('',(#2451),#1175,.T.);
#25645=ADVANCED_FACE('',(#2452),#1176,.T.);
#25646=ADVANCED_FACE('',(#2453),#1177,.T.);
#25647=ADVANCED_FACE('',(#2454),#1178,.T.);
#25648=ADVANCED_FACE('',(#2455),#1179,.T.);
#25649=ADVANCED_FACE('',(#2456),#25471,.T.);
#25650=ADVANCED_FACE('',(#2457),#1180,.T.);
#25651=ADVANCED_FACE('',(#2458),#25472,.T.);
#25652=ADVANCED_FACE('',(#2459),#1181,.T.);
#25653=ADVANCED_FACE('',(#2460),#25473,.T.);
#25654=ADVANCED_FACE('',(#2461),#1182,.T.);
#25655=ADVANCED_FACE('',(#2462),#25474,.T.);
#25656=ADVANCED_FACE('',(#2463),#1183,.T.);
#25657=ADVANCED_FACE('',(#2464),#1184,.T.);
#25658=ADVANCED_FACE('',(#2465),#1185,.T.);
#25659=ADVANCED_FACE('',(#2466),#1186,.T.);
#25660=ADVANCED_FACE('',(#2467),#1187,.T.);
#25661=ADVANCED_FACE('',(#2468),#1188,.T.);
#25662=ADVANCED_FACE('',(#2469),#1189,.T.);
#25663=ADVANCED_FACE('',(#2470),#1190,.T.);
#25664=ADVANCED_FACE('',(#2471),#1191,.T.);
#25665=ADVANCED_FACE('',(#2472),#1192,.T.);
#25666=ADVANCED_FACE('',(#2473),#1193,.T.);
#25667=ADVANCED_FACE('',(#2474),#1194,.T.);
#25668=ADVANCED_FACE('',(#2475),#2163,.T.);
#25669=ADVANCED_FACE('',(#2476),#1195,.T.);
#25670=ADVANCED_FACE('',(#2477),#2164,.T.);
#25671=ADVANCED_FACE('',(#2478),#1196,.T.);
#25672=ADVANCED_FACE('',(#2479),#1197,.T.);
#25673=ADVANCED_FACE('',(#2480),#1198,.T.);
#25674=ADVANCED_FACE('',(#2481),#1199,.T.);
#25675=ADVANCED_FACE('',(#2482),#25475,.F.);
#25676=ADVANCED_FACE('',(#2483),#1200,.T.);
#25677=ADVANCED_FACE('',(#2484),#1201,.T.);
#25678=ADVANCED_FACE('',(#2485),#25476,.F.);
#25679=ADVANCED_FACE('',(#2486),#1202,.T.);
#25680=ADVANCED_FACE('',(#2487),#25477,.F.);
#25681=ADVANCED_FACE('',(#2488),#1203,.T.);
#25682=ADVANCED_FACE('',(#2489),#25478,.F.);
#25683=ADVANCED_FACE('',(#2490),#1204,.T.);
#25684=ADVANCED_FACE('',(#2491),#25479,.F.);
#25685=ADVANCED_FACE('',(#2492),#1205,.T.);
#25686=ADVANCED_FACE('',(#2493),#25480,.F.);
#25687=ADVANCED_FACE('',(#2494),#1206,.T.);
#25688=ADVANCED_FACE('',(#2495),#1207,.F.);
#25689=ADVANCED_FACE('',(#2496),#2165,.F.);
#25690=ADVANCED_FACE('',(#2497),#1208,.F.);
#25691=ADVANCED_FACE('',(#2498),#1209,.F.);
#25692=ADVANCED_FACE('',(#2499),#2166,.F.);
#25693=ADVANCED_FACE('',(#2500),#1210,.F.);
#25694=ADVANCED_FACE('',(#2501),#2167,.F.);
#25695=ADVANCED_FACE('',(#2502),#1211,.F.);
#25696=ADVANCED_FACE('',(#2503),#1212,.F.);
#25697=ADVANCED_FACE('',(#2504),#1213,.F.);
#25698=ADVANCED_FACE('',(#2505),#2168,.F.);
#25699=ADVANCED_FACE('',(#2506),#1214,.F.);
#25700=ADVANCED_FACE('',(#2507),#1215,.F.);
#25701=ADVANCED_FACE('',(#2508),#2169,.F.);
#25702=ADVANCED_FACE('',(#2509),#1216,.F.);
#25703=ADVANCED_FACE('',(#2510),#2170,.F.);
#25704=ADVANCED_FACE('',(#2511),#1217,.T.);
#25705=ADVANCED_FACE('',(#2512),#1218,.T.);
#25706=ADVANCED_FACE('',(#2513),#1219,.T.);
#25707=ADVANCED_FACE('',(#2514),#1220,.T.);
#25708=ADVANCED_FACE('',(#2515),#1221,.T.);
#25709=ADVANCED_FACE('',(#2516),#1222,.T.);
#25710=ADVANCED_FACE('',(#2517),#1223,.T.);
#25711=ADVANCED_FACE('',(#2518),#1224,.T.);
#25712=ADVANCED_FACE('',(#2519),#2171,.T.);
#25713=ADVANCED_FACE('',(#2520),#1225,.T.);
#25714=ADVANCED_FACE('',(#2521),#2172,.T.);
#25715=ADVANCED_FACE('',(#2522),#1226,.T.);
#25716=ADVANCED_FACE('',(#2523),#2173,.T.);
#25717=ADVANCED_FACE('',(#2524),#1227,.F.);
#25718=ADVANCED_FACE('',(#2525),#2174,.F.);
#25719=ADVANCED_FACE('',(#2526),#2175,.F.);
#25720=ADVANCED_FACE('',(#2527),#2176,.F.);
#25721=ADVANCED_FACE('',(#2528),#2177,.F.);
#25722=ADVANCED_FACE('',(#2529),#25481,.F.);
#25723=ADVANCED_FACE('',(#2530),#2178,.F.);
#25724=ADVANCED_FACE('',(#2531,#1001),#1228,.T.);
#25725=ADVANCED_FACE('',(#2532),#25482,.F.);
#25726=ADVANCED_FACE('',(#2533),#2179,.T.);
#25727=ADVANCED_FACE('',(#2534),#25483,.T.);
#25728=ADVANCED_FACE('',(#2535),#2180,.T.);
#25729=ADVANCED_FACE('',(#2536,#1002),#1229,.T.);
#25730=ADVANCED_FACE('',(#2537),#25484,.T.);
#25731=ADVANCED_FACE('',(#2538),#1230,.T.);
#25732=ADVANCED_FACE('',(#2539),#2181,.T.);
#25733=ADVANCED_FACE('',(#2540),#2182,.T.);
#25734=ADVANCED_FACE('',(#2541),#1231,.T.);
#25735=ADVANCED_FACE('',(#2542),#2183,.T.);
#25736=ADVANCED_FACE('',(#2543),#2184,.T.);
#25737=ADVANCED_FACE('',(#2544,#1003),#1232,.T.);
#25738=ADVANCED_FACE('',(#2545,#1004,#1005),#1233,.T.);
#25739=ADVANCED_FACE('',(#2546,#1006,#1007),#1234,.T.);
#25740=ADVANCED_FACE('',(#2547,#1008,#1009),#1235,.F.);
#25741=ADVANCED_FACE('',(#2548),#1236,.T.);
#25742=ADVANCED_FACE('',(#2549),#2185,.T.);
#25743=ADVANCED_FACE('',(#2550),#1237,.T.);
#25744=ADVANCED_FACE('',(#2551),#2186,.T.);
#25745=ADVANCED_FACE('',(#2552),#1238,.T.);
#25746=ADVANCED_FACE('',(#2553),#2187,.T.);
#25747=ADVANCED_FACE('',(#2554),#1239,.T.);
#25748=ADVANCED_FACE('',(#2555),#2188,.T.);
#25749=ADVANCED_FACE('',(#2556,#1010,#1011),#1240,.F.);
#25750=ADVANCED_FACE('',(#2557),#1241,.T.);
#25751=ADVANCED_FACE('',(#2558),#1242,.T.);
#25752=ADVANCED_FACE('',(#2559),#2189,.T.);
#25753=ADVANCED_FACE('',(#2560),#1243,.T.);
#25754=ADVANCED_FACE('',(#2561),#2190,.T.);
#25755=ADVANCED_FACE('',(#2562,#1012),#1244,.T.);
#25756=ADVANCED_FACE('',(#2563),#2191,.T.);
#25757=ADVANCED_FACE('',(#2564),#1245,.T.);
#25758=ADVANCED_FACE('',(#2565),#2192,.T.);
#25759=ADVANCED_FACE('',(#2566),#1246,.T.);
#25760=ADVANCED_FACE('',(#2567),#1247,.F.);
#25761=ADVANCED_FACE('',(#2568),#1248,.T.);
#25762=ADVANCED_FACE('',(#2569),#2193,.T.);
#25763=ADVANCED_FACE('',(#2570),#865,.T.);
#25764=ADVANCED_FACE('',(#2571),#1249,.T.);
#25765=ADVANCED_FACE('',(#2572),#866,.T.);
#25766=ADVANCED_FACE('',(#2573,#1013),#1250,.T.);
#25767=ADVANCED_FACE('',(#2574),#2194,.T.);
#25768=ADVANCED_FACE('',(#2575),#1251,.T.);
#25769=ADVANCED_FACE('',(#2576),#2195,.T.);
#25770=ADVANCED_FACE('',(#2577),#867,.T.);
#25771=ADVANCED_FACE('',(#2578),#1252,.T.);
#25772=ADVANCED_FACE('',(#2579),#868,.T.);
#25773=ADVANCED_FACE('',(#2580),#2196,.T.);
#25774=ADVANCED_FACE('',(#2581),#1253,.T.);
#25775=ADVANCED_FACE('',(#2582),#2197,.T.);
#25776=ADVANCED_FACE('',(#2583),#869,.T.);
#25777=ADVANCED_FACE('',(#2584),#1254,.T.);
#25778=ADVANCED_FACE('',(#2585),#870,.T.);
#25779=ADVANCED_FACE('',(#2586),#2198,.T.);
#25780=ADVANCED_FACE('',(#2587),#1255,.T.);
#25781=ADVANCED_FACE('',(#2588),#2199,.T.);
#25782=ADVANCED_FACE('',(#2589),#871,.T.);
#25783=ADVANCED_FACE('',(#2590),#1256,.T.);
#25784=ADVANCED_FACE('',(#2591),#872,.T.);
#25785=ADVANCED_FACE('',(#2592),#2200,.T.);
#25786=ADVANCED_FACE('',(#2593),#1257,.T.);
#25787=ADVANCED_FACE('',(#2594),#2201,.T.);
#25788=ADVANCED_FACE('',(#2595),#873,.T.);
#25789=ADVANCED_FACE('',(#2596),#1258,.T.);
#25790=ADVANCED_FACE('',(#2597),#874,.T.);
#25791=ADVANCED_FACE('',(#2598),#2202,.T.);
#25792=ADVANCED_FACE('',(#2599),#1259,.T.);
#25793=ADVANCED_FACE('',(#2600),#2203,.T.);
#25794=ADVANCED_FACE('',(#2601),#875,.T.);
#25795=ADVANCED_FACE('',(#2602),#1260,.T.);
#25796=ADVANCED_FACE('',(#2603),#876,.T.);
#25797=ADVANCED_FACE('',(#2604),#2204,.T.);
#25798=ADVANCED_FACE('',(#2605),#1261,.T.);
#25799=ADVANCED_FACE('',(#2606),#2205,.T.);
#25800=ADVANCED_FACE('',(#2607),#877,.T.);
#25801=ADVANCED_FACE('',(#2608),#1262,.T.);
#25802=ADVANCED_FACE('',(#2609),#878,.T.);
#25803=ADVANCED_FACE('',(#2610),#2206,.T.);
#25804=ADVANCED_FACE('',(#2611),#1263,.T.);
#25805=ADVANCED_FACE('',(#2612),#2207,.T.);
#25806=ADVANCED_FACE('',(#2613),#879,.T.);
#25807=ADVANCED_FACE('',(#2614),#1264,.T.);
#25808=ADVANCED_FACE('',(#2615),#880,.T.);
#25809=ADVANCED_FACE('',(#2616),#2208,.T.);
#25810=ADVANCED_FACE('',(#2617),#1265,.T.);
#25811=ADVANCED_FACE('',(#2618),#2209,.T.);
#25812=ADVANCED_FACE('',(#2619),#881,.T.);
#25813=ADVANCED_FACE('',(#2620),#1266,.T.);
#25814=ADVANCED_FACE('',(#2621),#882,.T.);
#25815=ADVANCED_FACE('',(#2622),#2210,.T.);
#25816=ADVANCED_FACE('',(#2623),#1267,.T.);
#25817=ADVANCED_FACE('',(#2624),#2211,.T.);
#25818=ADVANCED_FACE('',(#2625),#883,.T.);
#25819=ADVANCED_FACE('',(#2626),#1268,.T.);
#25820=ADVANCED_FACE('',(#2627),#884,.T.);
#25821=ADVANCED_FACE('',(#2628),#2212,.T.);
#25822=ADVANCED_FACE('',(#2629),#1269,.T.);
#25823=ADVANCED_FACE('',(#2630),#2213,.T.);
#25824=ADVANCED_FACE('',(#2631),#885,.T.);
#25825=ADVANCED_FACE('',(#2632),#1270,.T.);
#25826=ADVANCED_FACE('',(#2633),#886,.T.);
#25827=ADVANCED_FACE('',(#2634),#2214,.T.);
#25828=ADVANCED_FACE('',(#2635),#1271,.T.);
#25829=ADVANCED_FACE('',(#2636),#2215,.T.);
#25830=ADVANCED_FACE('',(#2637),#887,.T.);
#25831=ADVANCED_FACE('',(#2638),#1272,.T.);
#25832=ADVANCED_FACE('',(#2639),#888,.T.);
#25833=ADVANCED_FACE('',(#2640),#2216,.T.);
#25834=ADVANCED_FACE('',(#2641),#1273,.T.);
#25835=ADVANCED_FACE('',(#2642),#2217,.T.);
#25836=ADVANCED_FACE('',(#2643),#889,.T.);
#25837=ADVANCED_FACE('',(#2644),#1274,.T.);
#25838=ADVANCED_FACE('',(#2645),#890,.T.);
#25839=ADVANCED_FACE('',(#2646),#2218,.T.);
#25840=ADVANCED_FACE('',(#2647),#1275,.T.);
#25841=ADVANCED_FACE('',(#2648),#2219,.T.);
#25842=ADVANCED_FACE('',(#2649),#891,.T.);
#25843=ADVANCED_FACE('',(#2650),#1276,.T.);
#25844=ADVANCED_FACE('',(#2651),#892,.T.);
#25845=ADVANCED_FACE('',(#2652),#2220,.T.);
#25846=ADVANCED_FACE('',(#2653),#1277,.T.);
#25847=ADVANCED_FACE('',(#2654),#1278,.T.);
#25848=ADVANCED_FACE('',(#2655),#2221,.T.);
#25849=ADVANCED_FACE('',(#2656),#893,.T.);
#25850=ADVANCED_FACE('',(#2657),#894,.T.);
#25851=ADVANCED_FACE('',(#2658,#1014),#1279,.T.);
#25852=ADVANCED_FACE('',(#2659),#2222,.T.);
#25853=ADVANCED_FACE('',(#2660),#1280,.T.);
#25854=ADVANCED_FACE('',(#2661),#2223,.T.);
#25855=ADVANCED_FACE('',(#2662),#895,.T.);
#25856=ADVANCED_FACE('',(#2663),#1281,.T.);
#25857=ADVANCED_FACE('',(#2664),#896,.T.);
#25858=ADVANCED_FACE('',(#2665),#2224,.T.);
#25859=ADVANCED_FACE('',(#2666,#1015),#1282,.T.);
#25860=ADVANCED_FACE('',(#2667),#2225,.F.);
#25861=ADVANCED_FACE('',(#2668,#1016),#1283,.T.);
#25862=ADVANCED_FACE('',(#2669),#2226,.F.);
#25863=ADVANCED_FACE('',(#2670),#2227,.F.);
#25864=ADVANCED_FACE('',(#2671),#2228,.T.);
#25865=ADVANCED_FACE('',(#2672),#2229,.T.);
#25866=ADVANCED_FACE('',(#2673),#2230,.T.);
#25867=ADVANCED_FACE('',(#2674),#2231,.T.);
#25868=ADVANCED_FACE('',(#2675),#2232,.T.);
#25869=ADVANCED_FACE('',(#2676),#2233,.T.);
#25870=ADVANCED_FACE('',(#2677),#2234,.T.);
#25871=ADVANCED_FACE('',(#2678),#2235,.T.);
#25872=ADVANCED_FACE('',(#2679),#2236,.T.);
#25873=ADVANCED_FACE('',(#2680),#2237,.T.);
#25874=ADVANCED_FACE('',(#2681),#2238,.T.);
#25875=ADVANCED_FACE('',(#2682),#2239,.T.);
#25876=ADVANCED_FACE('',(#2683),#2240,.T.);
#25877=ADVANCED_FACE('',(#2684),#2241,.T.);
#25878=ADVANCED_FACE('',(#2685),#2242,.T.);
#25879=ADVANCED_FACE('',(#2686),#2243,.T.);
#25880=ADVANCED_FACE('',(#2687),#2244,.T.);
#25881=ADVANCED_FACE('',(#2688),#2245,.T.);
#25882=ADVANCED_FACE('',(#2689),#2246,.T.);
#25883=ADVANCED_FACE('',(#2690),#2247,.T.);
#25884=ADVANCED_FACE('',(#2691),#2248,.T.);
#25885=ADVANCED_FACE('',(#2692),#2249,.T.);
#25886=ADVANCED_FACE('',(#2693),#2250,.T.);
#25887=ADVANCED_FACE('',(#2694),#2251,.T.);
#25888=ADVANCED_FACE('',(#2695),#1284,.T.);
#25889=ADVANCED_FACE('',(#2696),#897,.F.);
#25890=ADVANCED_FACE('',(#2697),#1285,.F.);
#25891=ADVANCED_FACE('',(#2698),#898,.F.);
#25892=ADVANCED_FACE('',(#2699),#503,.F.);
#25893=ADVANCED_FACE('',(#2700,#1017),#1286,.F.);
#25894=ADVANCED_FACE('',(#2701),#25485,.T.);
#25895=ADVANCED_FACE('',(#2702),#1287,.F.);
#25896=ADVANCED_FACE('',(#2703),#1288,.F.);
#25897=ADVANCED_FACE('',(#2704),#1289,.F.);
#25898=ADVANCED_FACE('',(#2705),#1290,.F.);
#25899=ADVANCED_FACE('',(#2706),#2252,.T.);
#25900=ADVANCED_FACE('',(#2707),#1291,.F.);
#25901=ADVANCED_FACE('',(#2708),#1292,.F.);
#25902=ADVANCED_FACE('',(#2709),#1293,.F.);
#25903=ADVANCED_FACE('',(#2710),#1294,.F.);
#25904=ADVANCED_FACE('',(#2711),#1295,.F.);
#25905=ADVANCED_FACE('',(#2712),#1296,.F.);
#25906=ADVANCED_FACE('',(#2713),#1297,.F.);
#25907=ADVANCED_FACE('',(#2714),#1298,.F.);
#25908=ADVANCED_FACE('',(#2715),#1299,.F.);
#25909=ADVANCED_FACE('',(#2716),#1300,.F.);
#25910=ADVANCED_FACE('',(#2717),#1301,.F.);
#25911=ADVANCED_FACE('',(#2718),#1302,.F.);
#25912=ADVANCED_FACE('',(#2719),#1303,.F.);
#25913=ADVANCED_FACE('',(#2720),#1304,.F.);
#25914=ADVANCED_FACE('',(#2721),#1305,.F.);
#25915=ADVANCED_FACE('',(#2722),#1306,.F.);
#25916=ADVANCED_FACE('',(#2723),#1307,.F.);
#25917=ADVANCED_FACE('',(#2724),#1308,.F.);
#25918=ADVANCED_FACE('',(#2725),#1309,.F.);
#25919=ADVANCED_FACE('',(#2726),#1310,.F.);
#25920=ADVANCED_FACE('',(#2727),#1311,.F.);
#25921=ADVANCED_FACE('',(#2728),#1312,.F.);
#25922=ADVANCED_FACE('',(#2729),#1313,.F.);
#25923=ADVANCED_FACE('',(#2730),#1314,.F.);
#25924=ADVANCED_FACE('',(#2731),#1315,.F.);
#25925=ADVANCED_FACE('',(#2732),#1316,.F.);
#25926=ADVANCED_FACE('',(#2733),#1317,.F.);
#25927=ADVANCED_FACE('',(#2734),#1318,.F.);
#25928=ADVANCED_FACE('',(#2735),#1319,.F.);
#25929=ADVANCED_FACE('',(#2736),#1320,.F.);
#25930=ADVANCED_FACE('',(#2737),#1321,.F.);
#25931=ADVANCED_FACE('',(#2738),#1322,.F.);
#25932=ADVANCED_FACE('',(#2739),#1323,.F.);
#25933=ADVANCED_FACE('',(#2740),#1324,.F.);
#25934=ADVANCED_FACE('',(#2741),#1325,.F.);
#25935=ADVANCED_FACE('',(#2742),#1326,.F.);
#25936=ADVANCED_FACE('',(#2743),#1327,.F.);
#25937=ADVANCED_FACE('',(#2744),#1328,.F.);
#25938=ADVANCED_FACE('',(#2745),#1329,.F.);
#25939=ADVANCED_FACE('',(#2746),#1330,.F.);
#25940=ADVANCED_FACE('',(#2747),#1331,.F.);
#25941=ADVANCED_FACE('',(#2748),#1332,.F.);
#25942=ADVANCED_FACE('',(#2749),#1333,.F.);
#25943=ADVANCED_FACE('',(#2750),#1334,.F.);
#25944=ADVANCED_FACE('',(#2751),#1335,.F.);
#25945=ADVANCED_FACE('',(#2752),#1336,.F.);
#25946=ADVANCED_FACE('',(#2753),#1337,.F.);
#25947=ADVANCED_FACE('',(#2754),#1338,.F.);
#25948=ADVANCED_FACE('',(#2755),#1339,.F.);
#25949=ADVANCED_FACE('',(#2756),#1340,.F.);
#25950=ADVANCED_FACE('',(#2757),#1341,.F.);
#25951=ADVANCED_FACE('',(#2758),#1342,.F.);
#25952=ADVANCED_FACE('',(#2759),#1343,.F.);
#25953=ADVANCED_FACE('',(#2760),#1344,.F.);
#25954=ADVANCED_FACE('',(#2761),#1345,.F.);
#25955=ADVANCED_FACE('',(#2762),#1346,.F.);
#25956=ADVANCED_FACE('',(#2763),#1347,.F.);
#25957=ADVANCED_FACE('',(#2764),#1348,.F.);
#25958=ADVANCED_FACE('',(#2765),#1349,.F.);
#25959=ADVANCED_FACE('',(#2766),#1350,.F.);
#25960=ADVANCED_FACE('',(#2767),#1351,.F.);
#25961=ADVANCED_FACE('',(#2768),#1352,.F.);
#25962=ADVANCED_FACE('',(#2769),#1353,.F.);
#25963=ADVANCED_FACE('',(#2770),#1354,.F.);
#25964=ADVANCED_FACE('',(#2771),#1355,.F.);
#25965=ADVANCED_FACE('',(#2772),#1356,.F.);
#25966=ADVANCED_FACE('',(#2773),#1357,.F.);
#25967=ADVANCED_FACE('',(#2774),#1358,.F.);
#25968=ADVANCED_FACE('',(#2775),#1359,.F.);
#25969=ADVANCED_FACE('',(#2776),#1360,.F.);
#25970=ADVANCED_FACE('',(#2777),#1361,.F.);
#25971=ADVANCED_FACE('',(#2778),#1362,.F.);
#25972=ADVANCED_FACE('',(#2779),#1363,.F.);
#25973=ADVANCED_FACE('',(#2780),#1364,.F.);
#25974=ADVANCED_FACE('',(#2781),#1365,.F.);
#25975=ADVANCED_FACE('',(#2782),#1366,.F.);
#25976=ADVANCED_FACE('',(#2783),#1367,.F.);
#25977=ADVANCED_FACE('',(#2784),#1368,.F.);
#25978=ADVANCED_FACE('',(#2785),#1369,.F.);
#25979=ADVANCED_FACE('',(#2786),#1370,.F.);
#25980=ADVANCED_FACE('',(#2787),#1371,.F.);
#25981=ADVANCED_FACE('',(#2788),#1372,.F.);
#25982=ADVANCED_FACE('',(#2789),#1373,.F.);
#25983=ADVANCED_FACE('',(#2790),#1374,.F.);
#25984=ADVANCED_FACE('',(#2791),#1375,.F.);
#25985=ADVANCED_FACE('',(#2792),#1376,.F.);
#25986=ADVANCED_FACE('',(#2793),#1377,.F.);
#25987=ADVANCED_FACE('',(#2794),#1378,.F.);
#25988=ADVANCED_FACE('',(#2795),#1379,.F.);
#25989=ADVANCED_FACE('',(#2796),#1380,.F.);
#25990=ADVANCED_FACE('',(#2797),#1381,.F.);
#25991=ADVANCED_FACE('',(#2798),#1382,.F.);
#25992=ADVANCED_FACE('',(#2799),#1383,.F.);
#25993=ADVANCED_FACE('',(#2800),#1384,.F.);
#25994=ADVANCED_FACE('',(#2801),#1385,.F.);
#25995=ADVANCED_FACE('',(#2802),#1386,.F.);
#25996=ADVANCED_FACE('',(#2803),#1387,.F.);
#25997=ADVANCED_FACE('',(#2804),#1388,.F.);
#25998=ADVANCED_FACE('',(#2805),#1389,.F.);
#25999=ADVANCED_FACE('',(#2806),#1390,.F.);
#26000=ADVANCED_FACE('',(#2807),#1391,.F.);
#26001=ADVANCED_FACE('',(#2808),#1392,.F.);
#26002=ADVANCED_FACE('',(#2809),#1393,.F.);
#26003=ADVANCED_FACE('',(#2810),#1394,.F.);
#26004=ADVANCED_FACE('',(#2811),#1395,.F.);
#26005=ADVANCED_FACE('',(#2812),#504,.T.);
#26006=ADVANCED_FACE('',(#2813),#25486,.T.);
#26007=ADVANCED_FACE('',(#2814,#1018),#1396,.T.);
#26008=ADVANCED_FACE('',(#2815),#25487,.F.);
#26009=ADVANCED_FACE('',(#2816),#2253,.T.);
#26010=ADVANCED_FACE('',(#2817),#2254,.T.);
#26011=ADVANCED_FACE('',(#2818),#2255,.T.);
#26012=ADVANCED_FACE('',(#2819),#2256,.T.);
#26013=ADVANCED_FACE('',(#2820),#2257,.T.);
#26014=ADVANCED_FACE('',(#2821),#2258,.T.);
#26015=ADVANCED_FACE('',(#2822),#1397,.F.);
#26016=ADVANCED_FACE('',(#2823),#1398,.F.);
#26017=ADVANCED_FACE('',(#2824),#1399,.F.);
#26018=ADVANCED_FACE('',(#2825),#1400,.T.);
#26019=ADVANCED_FACE('',(#2826),#1401,.T.);
#26020=ADVANCED_FACE('',(#2827),#1402,.T.);
#26021=ADVANCED_FACE('',(#2828),#1403,.T.);
#26022=ADVANCED_FACE('',(#2829),#1404,.T.);
#26023=ADVANCED_FACE('',(#2830),#1405,.T.);
#26024=ADVANCED_FACE('',(#2831),#1406,.F.);
#26025=ADVANCED_FACE('',(#2832),#1407,.F.);
#26026=ADVANCED_FACE('',(#2833),#1408,.F.);
#26027=ADVANCED_FACE('',(#2834),#1409,.F.);
#26028=ADVANCED_FACE('',(#2835),#1410,.F.);
#26029=ADVANCED_FACE('',(#2836),#1411,.F.);
#26030=ADVANCED_FACE('',(#2837),#25488,.F.);
#26031=ADVANCED_FACE('',(#2838),#1412,.F.);
#26032=ADVANCED_FACE('',(#2839),#1413,.F.);
#26033=ADVANCED_FACE('',(#2840),#1414,.F.);
#26034=ADVANCED_FACE('',(#2841),#25489,.F.);
#26035=ADVANCED_FACE('',(#2842,#1019,#1020,#1021,#1022,#1023,#1024,#1025,
#1026,#1027,#1028,#1029,#1030,#1031,#1032,#1033,#1034,#1035,#1036,#1037,
#1038,#1039),#1415,.T.);
#26036=ADVANCED_FACE('',(#2843),#2259,.F.);
#26037=ADVANCED_FACE('',(#2844),#25490,.F.);
#26038=ADVANCED_FACE('',(#2845),#2260,.F.);
#26039=ADVANCED_FACE('',(#2846),#25491,.F.);
#26040=ADVANCED_FACE('',(#2847),#2261,.F.);
#26041=ADVANCED_FACE('',(#2848),#25492,.F.);
#26042=ADVANCED_FACE('',(#2849),#2262,.F.);
#26043=ADVANCED_FACE('',(#2850),#25493,.F.);
#26044=ADVANCED_FACE('',(#2851),#2263,.F.);
#26045=ADVANCED_FACE('',(#2852),#25494,.F.);
#26046=ADVANCED_FACE('',(#2853),#2264,.F.);
#26047=ADVANCED_FACE('',(#2854),#25495,.F.);
#26048=ADVANCED_FACE('',(#2855),#2265,.F.);
#26049=ADVANCED_FACE('',(#2856),#25496,.F.);
#26050=ADVANCED_FACE('',(#2857),#2266,.F.);
#26051=ADVANCED_FACE('',(#2858),#25497,.F.);
#26052=ADVANCED_FACE('',(#2859),#2267,.F.);
#26053=ADVANCED_FACE('',(#2860),#25498,.F.);
#26054=ADVANCED_FACE('',(#2861),#2268,.F.);
#26055=ADVANCED_FACE('',(#2862),#25499,.F.);
#26056=ADVANCED_FACE('',(#2863),#2269,.F.);
#26057=ADVANCED_FACE('',(#2864),#25500,.F.);
#26058=ADVANCED_FACE('',(#2865),#2270,.F.);
#26059=ADVANCED_FACE('',(#2866),#25501,.F.);
#26060=ADVANCED_FACE('',(#2867),#2271,.F.);
#26061=ADVANCED_FACE('',(#2868),#25502,.F.);
#26062=ADVANCED_FACE('',(#2869),#2272,.F.);
#26063=ADVANCED_FACE('',(#2870),#25503,.F.);
#26064=ADVANCED_FACE('',(#2871),#2273,.F.);
#26065=ADVANCED_FACE('',(#2872),#25504,.F.);
#26066=ADVANCED_FACE('',(#2873),#2274,.F.);
#26067=ADVANCED_FACE('',(#2874),#25505,.F.);
#26068=ADVANCED_FACE('',(#2875),#2275,.F.);
#26069=ADVANCED_FACE('',(#2876),#25506,.F.);
#26070=ADVANCED_FACE('',(#2877),#2276,.F.);
#26071=ADVANCED_FACE('',(#2878),#25507,.F.);
#26072=ADVANCED_FACE('',(#2879),#2277,.F.);
#26073=ADVANCED_FACE('',(#2880),#25508,.F.);
#26074=ADVANCED_FACE('',(#2881),#2278,.F.);
#26075=ADVANCED_FACE('',(#2882),#25509,.F.);
#26076=ADVANCED_FACE('',(#2883),#2279,.F.);
#26077=ADVANCED_FACE('',(#2884),#1416,.T.);
#26078=ADVANCED_FACE('',(#2885),#25510,.T.);
#26079=ADVANCED_FACE('',(#2886),#1417,.T.);
#26080=ADVANCED_FACE('',(#2887),#25511,.T.);
#26081=ADVANCED_FACE('',(#2888),#2280,.T.);
#26082=ADVANCED_FACE('',(#2889),#1418,.T.);
#26083=ADVANCED_FACE('',(#2890),#1419,.T.);
#26084=ADVANCED_FACE('',(#2891),#25512,.T.);
#26085=ADVANCED_FACE('',(#2892),#1420,.T.);
#26086=ADVANCED_FACE('',(#2893),#25513,.T.);
#26087=ADVANCED_FACE('',(#2894),#2281,.T.);
#26088=ADVANCED_FACE('',(#2895,#1040,#1041,#1042,#1043,#1044,#1045,#1046,
#1047,#1048,#1049,#1050,#1051,#1052,#1053,#1054,#1055,#1056,#1057,#1058,
#1059,#1060),#1421,.F.);
#26089=ADVANCED_FACE('',(#2896),#1422,.T.);
#26090=ADVANCED_FACE('',(#2897),#1423,.T.);
#26091=ADVANCED_FACE('',(#2898),#25514,.T.);
#26092=ADVANCED_FACE('',(#2899),#1424,.T.);
#26093=ADVANCED_FACE('',(#2900),#25515,.T.);
#26094=ADVANCED_FACE('',(#2901),#1425,.T.);
#26095=ADVANCED_FACE('',(#2902),#1426,.T.);
#26096=ADVANCED_FACE('',(#2903),#2282,.T.);
#26097=ADVANCED_FACE('',(#2904),#1427,.T.);
#26098=ADVANCED_FACE('',(#2905),#2283,.T.);
#26099=ADVANCED_FACE('',(#2906),#1428,.T.);
#26100=ADVANCED_FACE('',(#2907),#1429,.T.);
#26101=ADVANCED_FACE('',(#2908),#25516,.T.);
#26102=ADVANCED_FACE('',(#2909),#1430,.T.);
#26103=ADVANCED_FACE('',(#2910),#25517,.T.);
#26104=ADVANCED_FACE('',(#2911),#1431,.T.);
#26105=ADVANCED_FACE('',(#2912),#2284,.F.);
#26106=ADVANCED_FACE('',(#2913),#2285,.F.);
#26107=ADVANCED_FACE('',(#2914),#2286,.F.);
#26108=ADVANCED_FACE('',(#2915),#2287,.F.);
#26109=ADVANCED_FACE('',(#2916),#2288,.F.);
#26110=ADVANCED_FACE('',(#2917),#2289,.F.);
#26111=ADVANCED_FACE('',(#2918),#2290,.F.);
#26112=ADVANCED_FACE('',(#2919),#2291,.F.);
#26113=ADVANCED_FACE('',(#2920),#2292,.F.);
#26114=ADVANCED_FACE('',(#2921),#2293,.F.);
#26115=ADVANCED_FACE('',(#2922),#1432,.T.);
#26116=ADVANCED_FACE('',(#2923),#1433,.T.);
#26117=ADVANCED_FACE('',(#2924),#1434,.T.);
#26118=ADVANCED_FACE('',(#2925),#1435,.T.);
#26119=ADVANCED_FACE('',(#2926),#1436,.T.);
#26120=ADVANCED_FACE('',(#2927),#1437,.T.);
#26121=ADVANCED_FACE('',(#2928),#1438,.T.);
#26122=ADVANCED_FACE('',(#2929),#1439,.T.);
#26123=ADVANCED_FACE('',(#2930),#1440,.T.);
#26124=ADVANCED_FACE('',(#2931),#1441,.T.);
#26125=ADVANCED_FACE('',(#2932),#1442,.T.);
#26126=ADVANCED_FACE('',(#2933),#1443,.T.);
#26127=ADVANCED_FACE('',(#2934),#1444,.T.);
#26128=ADVANCED_FACE('',(#2935),#1445,.T.);
#26129=ADVANCED_FACE('',(#2936),#1446,.T.);
#26130=ADVANCED_FACE('',(#2937),#1447,.T.);
#26131=ADVANCED_FACE('',(#2938),#1448,.T.);
#26132=ADVANCED_FACE('',(#2939),#1449,.T.);
#26133=ADVANCED_FACE('',(#2940),#1450,.T.);
#26134=ADVANCED_FACE('',(#2941),#1451,.T.);
#26135=ADVANCED_FACE('',(#2942),#1452,.T.);
#26136=ADVANCED_FACE('',(#2943),#1453,.T.);
#26137=ADVANCED_FACE('',(#2944),#1454,.T.);
#26138=ADVANCED_FACE('',(#2945),#1455,.T.);
#26139=ADVANCED_FACE('',(#2946),#1456,.T.);
#26140=ADVANCED_FACE('',(#2947),#1457,.T.);
#26141=ADVANCED_FACE('',(#2948),#1458,.T.);
#26142=ADVANCED_FACE('',(#2949),#1459,.T.);
#26143=ADVANCED_FACE('',(#2950),#1460,.T.);
#26144=ADVANCED_FACE('',(#2951),#1461,.T.);
#26145=ADVANCED_FACE('',(#2952),#1462,.T.);
#26146=ADVANCED_FACE('',(#2953),#1463,.T.);
#26147=ADVANCED_FACE('',(#2954),#1464,.T.);
#26148=ADVANCED_FACE('',(#2955),#1465,.T.);
#26149=ADVANCED_FACE('',(#2956),#1466,.T.);
#26150=ADVANCED_FACE('',(#2957),#1467,.T.);
#26151=ADVANCED_FACE('',(#2958),#1468,.T.);
#26152=ADVANCED_FACE('',(#2959),#1469,.T.);
#26153=ADVANCED_FACE('',(#2960),#1470,.T.);
#26154=ADVANCED_FACE('',(#2961),#1471,.T.);
#26155=ADVANCED_FACE('',(#2962),#1472,.T.);
#26156=ADVANCED_FACE('',(#2963),#1473,.T.);
#26157=ADVANCED_FACE('',(#2964),#1474,.T.);
#26158=ADVANCED_FACE('',(#2965),#1475,.T.);
#26159=ADVANCED_FACE('',(#2966),#1476,.T.);
#26160=ADVANCED_FACE('',(#2967),#1477,.T.);
#26161=ADVANCED_FACE('',(#2968),#1478,.T.);
#26162=ADVANCED_FACE('',(#2969),#1479,.T.);
#26163=ADVANCED_FACE('',(#2970),#1480,.T.);
#26164=ADVANCED_FACE('',(#2971),#1481,.T.);
#26165=ADVANCED_FACE('',(#2972),#1482,.T.);
#26166=ADVANCED_FACE('',(#2973),#1483,.T.);
#26167=ADVANCED_FACE('',(#2974),#1484,.T.);
#26168=ADVANCED_FACE('',(#2975),#1485,.T.);
#26169=ADVANCED_FACE('',(#2976),#1486,.T.);
#26170=ADVANCED_FACE('',(#2977),#1487,.T.);
#26171=ADVANCED_FACE('',(#2978),#1488,.T.);
#26172=ADVANCED_FACE('',(#2979),#1489,.T.);
#26173=ADVANCED_FACE('',(#2980),#1490,.T.);
#26174=ADVANCED_FACE('',(#2981),#1491,.T.);
#26175=ADVANCED_FACE('',(#2982),#1492,.T.);
#26176=ADVANCED_FACE('',(#2983),#1493,.T.);
#26177=ADVANCED_FACE('',(#2984),#1494,.T.);
#26178=ADVANCED_FACE('',(#2985),#1495,.T.);
#26179=ADVANCED_FACE('',(#2986),#1496,.T.);
#26180=ADVANCED_FACE('',(#2987),#1497,.T.);
#26181=ADVANCED_FACE('',(#2988),#1498,.T.);
#26182=ADVANCED_FACE('',(#2989),#1499,.T.);
#26183=ADVANCED_FACE('',(#2990),#1500,.T.);
#26184=ADVANCED_FACE('',(#2991),#1501,.T.);
#26185=ADVANCED_FACE('',(#2992),#1502,.T.);
#26186=ADVANCED_FACE('',(#2993),#1503,.T.);
#26187=ADVANCED_FACE('',(#2994),#1504,.T.);
#26188=ADVANCED_FACE('',(#2995),#1505,.T.);
#26189=ADVANCED_FACE('',(#2996),#1506,.T.);
#26190=ADVANCED_FACE('',(#2997),#1507,.T.);
#26191=ADVANCED_FACE('',(#2998),#1508,.T.);
#26192=ADVANCED_FACE('',(#2999),#1509,.T.);
#26193=ADVANCED_FACE('',(#3000),#1510,.T.);
#26194=ADVANCED_FACE('',(#3001),#1511,.T.);
#26195=ADVANCED_FACE('',(#3002),#1512,.T.);
#26196=ADVANCED_FACE('',(#3003),#1513,.T.);
#26197=ADVANCED_FACE('',(#3004),#1514,.T.);
#26198=ADVANCED_FACE('',(#3005),#1515,.T.);
#26199=ADVANCED_FACE('',(#3006),#1516,.T.);
#26200=ADVANCED_FACE('',(#3007),#1517,.T.);
#26201=ADVANCED_FACE('',(#3008),#1518,.T.);
#26202=ADVANCED_FACE('',(#3009),#1519,.T.);
#26203=ADVANCED_FACE('',(#3010),#1520,.T.);
#26204=ADVANCED_FACE('',(#3011),#1521,.T.);
#26205=ADVANCED_FACE('',(#3012),#1522,.T.);
#26206=ADVANCED_FACE('',(#3013),#1523,.T.);
#26207=ADVANCED_FACE('',(#3014),#1524,.T.);
#26208=ADVANCED_FACE('',(#3015),#1525,.T.);
#26209=ADVANCED_FACE('',(#3016),#1526,.T.);
#26210=ADVANCED_FACE('',(#3017),#1527,.T.);
#26211=ADVANCED_FACE('',(#3018),#1528,.T.);
#26212=ADVANCED_FACE('',(#3019),#1529,.T.);
#26213=ADVANCED_FACE('',(#3020),#1530,.T.);
#26214=ADVANCED_FACE('',(#3021),#1531,.T.);
#26215=ADVANCED_FACE('',(#3022),#1532,.T.);
#26216=ADVANCED_FACE('',(#3023),#1533,.T.);
#26217=ADVANCED_FACE('',(#3024),#1534,.T.);
#26218=ADVANCED_FACE('',(#3025),#1535,.T.);
#26219=ADVANCED_FACE('',(#3026),#1536,.T.);
#26220=ADVANCED_FACE('',(#3027),#1537,.T.);
#26221=ADVANCED_FACE('',(#3028),#1538,.T.);
#26222=ADVANCED_FACE('',(#3029),#1539,.T.);
#26223=ADVANCED_FACE('',(#3030),#1540,.T.);
#26224=ADVANCED_FACE('',(#3031),#1541,.T.);
#26225=ADVANCED_FACE('',(#3032),#1542,.T.);
#26226=ADVANCED_FACE('',(#3033),#1543,.T.);
#26227=ADVANCED_FACE('',(#3034),#1544,.T.);
#26228=ADVANCED_FACE('',(#3035),#1545,.T.);
#26229=ADVANCED_FACE('',(#3036),#1546,.T.);
#26230=ADVANCED_FACE('',(#3037),#1547,.T.);
#26231=ADVANCED_FACE('',(#3038),#1548,.T.);
#26232=ADVANCED_FACE('',(#3039),#1549,.T.);
#26233=ADVANCED_FACE('',(#3040),#1550,.T.);
#26234=ADVANCED_FACE('',(#3041),#1551,.T.);
#26235=ADVANCED_FACE('',(#3042),#1552,.T.);
#26236=ADVANCED_FACE('',(#3043),#1553,.T.);
#26237=ADVANCED_FACE('',(#3044),#1554,.T.);
#26238=ADVANCED_FACE('',(#3045),#1555,.T.);
#26239=ADVANCED_FACE('',(#3046),#1556,.T.);
#26240=ADVANCED_FACE('',(#3047),#1557,.T.);
#26241=ADVANCED_FACE('',(#3048),#1558,.T.);
#26242=ADVANCED_FACE('',(#3049),#1559,.T.);
#26243=ADVANCED_FACE('',(#3050),#1560,.T.);
#26244=ADVANCED_FACE('',(#3051),#1561,.T.);
#26245=ADVANCED_FACE('',(#3052),#1562,.T.);
#26246=ADVANCED_FACE('',(#3053),#1563,.T.);
#26247=ADVANCED_FACE('',(#3054),#1564,.T.);
#26248=ADVANCED_FACE('',(#3055),#1565,.T.);
#26249=ADVANCED_FACE('',(#3056),#1566,.T.);
#26250=ADVANCED_FACE('',(#3057),#1567,.T.);
#26251=ADVANCED_FACE('',(#3058),#1568,.T.);
#26252=ADVANCED_FACE('',(#3059),#1569,.T.);
#26253=ADVANCED_FACE('',(#3060),#1570,.T.);
#26254=ADVANCED_FACE('',(#3061),#1571,.T.);
#26255=ADVANCED_FACE('',(#3062),#1572,.T.);
#26256=ADVANCED_FACE('',(#3063),#1573,.T.);
#26257=ADVANCED_FACE('',(#3064),#1574,.T.);
#26258=ADVANCED_FACE('',(#3065),#1575,.T.);
#26259=ADVANCED_FACE('',(#3066),#1576,.T.);
#26260=ADVANCED_FACE('',(#3067),#1577,.T.);
#26261=ADVANCED_FACE('',(#3068),#1578,.T.);
#26262=ADVANCED_FACE('',(#3069),#1579,.T.);
#26263=ADVANCED_FACE('',(#3070),#1580,.T.);
#26264=ADVANCED_FACE('',(#3071),#1581,.T.);
#26265=ADVANCED_FACE('',(#3072),#1582,.T.);
#26266=ADVANCED_FACE('',(#3073),#1583,.T.);
#26267=ADVANCED_FACE('',(#3074),#1584,.T.);
#26268=ADVANCED_FACE('',(#3075),#1585,.T.);
#26269=ADVANCED_FACE('',(#3076),#1586,.T.);
#26270=ADVANCED_FACE('',(#3077),#1587,.T.);
#26271=ADVANCED_FACE('',(#3078),#1588,.T.);
#26272=ADVANCED_FACE('',(#3079),#1589,.T.);
#26273=ADVANCED_FACE('',(#3080),#1590,.T.);
#26274=ADVANCED_FACE('',(#3081),#1591,.T.);
#26275=ADVANCED_FACE('',(#3082),#1592,.T.);
#26276=ADVANCED_FACE('',(#3083),#1593,.T.);
#26277=ADVANCED_FACE('',(#3084),#1594,.T.);
#26278=ADVANCED_FACE('',(#3085),#1595,.T.);
#26279=ADVANCED_FACE('',(#3086),#1596,.T.);
#26280=ADVANCED_FACE('',(#3087),#1597,.T.);
#26281=ADVANCED_FACE('',(#3088),#1598,.T.);
#26282=ADVANCED_FACE('',(#3089),#1599,.T.);
#26283=ADVANCED_FACE('',(#3090),#1600,.T.);
#26284=ADVANCED_FACE('',(#3091),#1601,.T.);
#26285=ADVANCED_FACE('',(#3092),#1602,.T.);
#26286=ADVANCED_FACE('',(#3093),#1603,.T.);
#26287=ADVANCED_FACE('',(#3094),#1604,.T.);
#26288=ADVANCED_FACE('',(#3095),#1605,.T.);
#26289=ADVANCED_FACE('',(#3096),#1606,.T.);
#26290=ADVANCED_FACE('',(#3097),#1607,.T.);
#26291=ADVANCED_FACE('',(#3098),#1608,.T.);
#26292=ADVANCED_FACE('',(#3099),#1609,.T.);
#26293=ADVANCED_FACE('',(#3100),#1610,.T.);
#26294=ADVANCED_FACE('',(#3101),#1611,.T.);
#26295=ADVANCED_FACE('',(#3102),#1612,.T.);
#26296=ADVANCED_FACE('',(#3103),#1613,.T.);
#26297=ADVANCED_FACE('',(#3104),#1614,.T.);
#26298=ADVANCED_FACE('',(#3105),#1615,.T.);
#26299=ADVANCED_FACE('',(#3106),#1616,.T.);
#26300=ADVANCED_FACE('',(#3107),#1617,.T.);
#26301=ADVANCED_FACE('',(#3108),#1618,.T.);
#26302=ADVANCED_FACE('',(#3109),#1619,.T.);
#26303=ADVANCED_FACE('',(#3110),#1620,.T.);
#26304=ADVANCED_FACE('',(#3111),#1621,.T.);
#26305=ADVANCED_FACE('',(#3112),#1622,.T.);
#26306=ADVANCED_FACE('',(#3113),#1623,.T.);
#26307=ADVANCED_FACE('',(#3114),#1624,.T.);
#26308=ADVANCED_FACE('',(#3115),#1625,.T.);
#26309=ADVANCED_FACE('',(#3116),#1626,.T.);
#26310=ADVANCED_FACE('',(#3117),#1627,.T.);
#26311=ADVANCED_FACE('',(#3118),#1628,.T.);
#26312=ADVANCED_FACE('',(#3119),#1629,.T.);
#26313=ADVANCED_FACE('',(#3120),#1630,.T.);
#26314=ADVANCED_FACE('',(#3121),#1631,.T.);
#26315=ADVANCED_FACE('',(#3122),#1632,.T.);
#26316=ADVANCED_FACE('',(#3123),#1633,.T.);
#26317=ADVANCED_FACE('',(#3124),#1634,.T.);
#26318=ADVANCED_FACE('',(#3125),#1635,.T.);
#26319=ADVANCED_FACE('',(#3126),#1636,.T.);
#26320=ADVANCED_FACE('',(#3127),#1637,.T.);
#26321=ADVANCED_FACE('',(#3128),#1638,.T.);
#26322=ADVANCED_FACE('',(#3129),#1639,.T.);
#26323=ADVANCED_FACE('',(#3130),#1640,.T.);
#26324=ADVANCED_FACE('',(#3131),#1641,.T.);
#26325=ADVANCED_FACE('',(#3132),#1642,.T.);
#26326=ADVANCED_FACE('',(#3133),#1643,.T.);
#26327=ADVANCED_FACE('',(#3134),#1644,.T.);
#26328=ADVANCED_FACE('',(#3135),#1645,.T.);
#26329=ADVANCED_FACE('',(#3136),#1646,.T.);
#26330=ADVANCED_FACE('',(#3137),#1647,.T.);
#26331=ADVANCED_FACE('',(#3138),#1648,.T.);
#26332=ADVANCED_FACE('',(#3139),#1649,.T.);
#26333=ADVANCED_FACE('',(#3140),#1650,.T.);
#26334=ADVANCED_FACE('',(#3141),#1651,.T.);
#26335=ADVANCED_FACE('',(#3142),#1652,.T.);
#26336=ADVANCED_FACE('',(#3143),#1653,.T.);
#26337=ADVANCED_FACE('',(#3144),#1654,.T.);
#26338=ADVANCED_FACE('',(#3145),#1655,.T.);
#26339=ADVANCED_FACE('',(#3146),#1656,.T.);
#26340=ADVANCED_FACE('',(#3147),#1657,.T.);
#26341=ADVANCED_FACE('',(#3148),#1658,.T.);
#26342=ADVANCED_FACE('',(#3149),#1659,.T.);
#26343=ADVANCED_FACE('',(#3150),#1660,.T.);
#26344=ADVANCED_FACE('',(#3151),#1661,.T.);
#26345=ADVANCED_FACE('',(#3152),#1662,.T.);
#26346=ADVANCED_FACE('',(#3153),#1663,.T.);
#26347=ADVANCED_FACE('',(#3154),#1664,.T.);
#26348=ADVANCED_FACE('',(#3155),#1665,.T.);
#26349=ADVANCED_FACE('',(#3156),#1666,.T.);
#26350=ADVANCED_FACE('',(#3157),#1667,.T.);
#26351=ADVANCED_FACE('',(#3158),#1668,.T.);
#26352=ADVANCED_FACE('',(#3159),#1669,.T.);
#26353=ADVANCED_FACE('',(#3160),#1670,.T.);
#26354=ADVANCED_FACE('',(#3161),#1671,.T.);
#26355=ADVANCED_FACE('',(#3162),#1672,.T.);
#26356=ADVANCED_FACE('',(#3163),#1673,.T.);
#26357=ADVANCED_FACE('',(#3164),#1674,.T.);
#26358=ADVANCED_FACE('',(#3165),#1675,.T.);
#26359=ADVANCED_FACE('',(#3166),#1676,.T.);
#26360=ADVANCED_FACE('',(#3167),#1677,.T.);
#26361=ADVANCED_FACE('',(#3168),#1678,.T.);
#26362=ADVANCED_FACE('',(#3169),#1679,.T.);
#26363=ADVANCED_FACE('',(#3170),#1680,.T.);
#26364=ADVANCED_FACE('',(#3171),#1681,.T.);
#26365=ADVANCED_FACE('',(#3172),#1682,.T.);
#26366=ADVANCED_FACE('',(#3173),#1683,.T.);
#26367=ADVANCED_FACE('',(#3174),#1684,.T.);
#26368=ADVANCED_FACE('',(#3175),#1685,.T.);
#26369=ADVANCED_FACE('',(#3176),#1686,.T.);
#26370=ADVANCED_FACE('',(#3177),#1687,.T.);
#26371=ADVANCED_FACE('',(#3178),#1688,.T.);
#26372=ADVANCED_FACE('',(#3179),#1689,.T.);
#26373=ADVANCED_FACE('',(#3180),#1690,.T.);
#26374=ADVANCED_FACE('',(#3181),#1691,.T.);
#26375=ADVANCED_FACE('',(#3182),#1692,.T.);
#26376=ADVANCED_FACE('',(#3183),#1693,.T.);
#26377=ADVANCED_FACE('',(#3184),#1694,.T.);
#26378=ADVANCED_FACE('',(#3185),#1695,.T.);
#26379=ADVANCED_FACE('',(#3186),#1696,.T.);
#26380=ADVANCED_FACE('',(#3187),#1697,.T.);
#26381=ADVANCED_FACE('',(#3188),#1698,.T.);
#26382=ADVANCED_FACE('',(#3189),#1699,.T.);
#26383=ADVANCED_FACE('',(#3190),#1700,.T.);
#26384=ADVANCED_FACE('',(#3191),#1701,.T.);
#26385=ADVANCED_FACE('',(#3192),#1702,.T.);
#26386=ADVANCED_FACE('',(#3193),#1703,.T.);
#26387=ADVANCED_FACE('',(#3194),#1704,.T.);
#26388=ADVANCED_FACE('',(#3195),#1705,.T.);
#26389=ADVANCED_FACE('',(#3196),#1706,.T.);
#26390=ADVANCED_FACE('',(#3197),#1707,.T.);
#26391=ADVANCED_FACE('',(#3198),#1708,.T.);
#26392=ADVANCED_FACE('',(#3199),#1709,.T.);
#26393=ADVANCED_FACE('',(#3200),#1710,.T.);
#26394=ADVANCED_FACE('',(#3201,#1061,#1062,#1063,#1064,#1065,#1066,#1067,
#1068,#1069,#1070),#1711,.T.);
#26395=ADVANCED_FACE('',(#3202,#1071,#1072,#1073,#1074,#1075,#1076,#1077,
#1078,#1079,#1080),#1712,.F.);
#26396=ADVANCED_FACE('',(#3203),#25518,.F.);
#26397=ADVANCED_FACE('',(#3204,#1081,#1082,#1083,#1084,#1085,#1086,#1087,
#1088,#1089,#1090),#1713,.T.);
#26398=ADVANCED_FACE('',(#3205),#2294,.F.);
#26399=ADVANCED_FACE('',(#3206),#25519,.F.);
#26400=ADVANCED_FACE('',(#3207),#2295,.F.);
#26401=ADVANCED_FACE('',(#3208),#25520,.F.);
#26402=ADVANCED_FACE('',(#3209),#2296,.F.);
#26403=ADVANCED_FACE('',(#3210),#25521,.F.);
#26404=ADVANCED_FACE('',(#3211),#2297,.F.);
#26405=ADVANCED_FACE('',(#3212),#25522,.F.);
#26406=ADVANCED_FACE('',(#3213),#2298,.F.);
#26407=ADVANCED_FACE('',(#3214),#25523,.F.);
#26408=ADVANCED_FACE('',(#3215),#2299,.F.);
#26409=ADVANCED_FACE('',(#3216),#25524,.F.);
#26410=ADVANCED_FACE('',(#3217),#2300,.F.);
#26411=ADVANCED_FACE('',(#3218),#25525,.F.);
#26412=ADVANCED_FACE('',(#3219),#2301,.F.);
#26413=ADVANCED_FACE('',(#3220),#1714,.F.);
#26414=ADVANCED_FACE('',(#3221),#1715,.F.);
#26415=ADVANCED_FACE('',(#3222),#1716,.F.);
#26416=ADVANCED_FACE('',(#3223),#1717,.F.);
#26417=ADVANCED_FACE('',(#3224),#1718,.F.);
#26418=ADVANCED_FACE('',(#3225),#1719,.F.);
#26419=ADVANCED_FACE('',(#3226),#1720,.F.);
#26420=ADVANCED_FACE('',(#3227),#1721,.F.);
#26421=ADVANCED_FACE('',(#3228),#1722,.F.);
#26422=ADVANCED_FACE('',(#3229),#1723,.F.);
#26423=ADVANCED_FACE('',(#3230),#1724,.F.);
#26424=ADVANCED_FACE('',(#3231),#1725,.F.);
#26425=ADVANCED_FACE('',(#3232),#1726,.T.);
#26426=ADVANCED_FACE('',(#3233),#1727,.T.);
#26427=ADVANCED_FACE('',(#3234),#1728,.T.);
#26428=ADVANCED_FACE('',(#3235),#1729,.T.);
#26429=ADVANCED_FACE('',(#3236),#1730,.T.);
#26430=ADVANCED_FACE('',(#3237),#1731,.T.);
#26431=ADVANCED_FACE('',(#3238),#1732,.T.);
#26432=ADVANCED_FACE('',(#3239),#1733,.T.);
#26433=ADVANCED_FACE('',(#3240),#1734,.T.);
#26434=ADVANCED_FACE('',(#3241),#1735,.T.);
#26435=ADVANCED_FACE('',(#3242),#1736,.T.);
#26436=ADVANCED_FACE('',(#3243),#1737,.T.);
#26437=ADVANCED_FACE('',(#3244),#1738,.T.);
#26438=ADVANCED_FACE('',(#3245),#1739,.T.);
#26439=ADVANCED_FACE('',(#3246),#1740,.T.);
#26440=ADVANCED_FACE('',(#3247),#1741,.T.);
#26441=ADVANCED_FACE('',(#3248,#1091,#1092,#1093,#1094,#1095,#1096,#1097,
#1098,#1099,#1100),#1742,.F.);
#26442=ADVANCED_FACE('',(#3249),#2302,.F.);
#26443=ADVANCED_FACE('',(#3250),#2303,.F.);
#26444=ADVANCED_FACE('',(#3251),#25526,.F.);
#26445=ADVANCED_FACE('',(#3252),#2304,.F.);
#26446=ADVANCED_FACE('',(#3253,#1101),#1743,.T.);
#26447=ADVANCED_FACE('',(#3254),#25527,.F.);
#26448=ADVANCED_FACE('',(#3255),#2305,.F.);
#26449=ADVANCED_FACE('',(#3256,#1102),#1744,.T.);
#26450=ADVANCED_FACE('',(#3257),#25528,.F.);
#26451=ADVANCED_FACE('',(#3258),#25529,.F.);
#26452=ADVANCED_FACE('',(#3259,#1103),#2306,.F.);
#26453=ADVANCED_FACE('',(#3260),#25530,.F.);
#26454=ADVANCED_FACE('',(#3261),#25531,.F.);
#26455=ADVANCED_FACE('',(#3262,#1104),#2307,.F.);
#26456=ADVANCED_FACE('',(#3263),#25532,.F.);
#26457=ADVANCED_FACE('',(#3264,#1105),#1745,.T.);
#26458=ADVANCED_FACE('',(#3265),#25533,.F.);
#26459=ADVANCED_FACE('',(#3266),#25534,.F.);
#26460=ADVANCED_FACE('',(#3267,#1106),#1746,.T.);
#26461=ADVANCED_FACE('',(#3268),#25535,.F.);
#26462=ADVANCED_FACE('',(#3269),#1747,.T.);
#26463=ADVANCED_FACE('',(#3270),#1748,.T.);
#26464=ADVANCED_FACE('',(#3271),#1749,.T.);
#26465=ADVANCED_FACE('',(#3272),#1750,.T.);
#26466=ADVANCED_FACE('',(#3273),#1751,.T.);
#26467=ADVANCED_FACE('',(#3274),#1752,.T.);
#26468=ADVANCED_FACE('',(#3275,#1107,#1108),#1753,.T.);
#26469=ADVANCED_FACE('',(#3276,#1109,#1110),#1754,.F.);
#26470=ADVANCED_FACE('',(#3277),#2308,.T.);
#26471=ADVANCED_FACE('',(#3278),#2309,.T.);
#26472=ADVANCED_FACE('',(#3279),#2310,.T.);
#26473=ADVANCED_FACE('',(#3280),#2311,.T.);
#26474=ADVANCED_FACE('',(#3281),#2312,.T.);
#26475=ADVANCED_FACE('',(#3282),#2313,.T.);
#26476=ADVANCED_FACE('',(#3283),#2314,.T.);
#26477=ADVANCED_FACE('',(#3284),#2315,.T.);
#26478=ADVANCED_FACE('',(#3285),#2316,.T.);
#26479=ADVANCED_FACE('',(#3286),#1755,.T.);
#26480=ADVANCED_FACE('',(#3287),#899,.F.);
#26481=ADVANCED_FACE('',(#3288),#1756,.F.);
#26482=ADVANCED_FACE('',(#3289),#900,.F.);
#26483=ADVANCED_FACE('',(#3290),#505,.F.);
#26484=ADVANCED_FACE('',(#3291,#1111),#1757,.F.);
#26485=ADVANCED_FACE('',(#3292),#25536,.T.);
#26486=ADVANCED_FACE('',(#3293),#1758,.F.);
#26487=ADVANCED_FACE('',(#3294),#1759,.F.);
#26488=ADVANCED_FACE('',(#3295),#1760,.F.);
#26489=ADVANCED_FACE('',(#3296),#1761,.F.);
#26490=ADVANCED_FACE('',(#3297),#25537,.T.);
#26491=ADVANCED_FACE('',(#3298),#1762,.F.);
#26492=ADVANCED_FACE('',(#3299),#1763,.F.);
#26493=ADVANCED_FACE('',(#3300),#1764,.F.);
#26494=ADVANCED_FACE('',(#3301),#1765,.F.);
#26495=ADVANCED_FACE('',(#3302),#1766,.F.);
#26496=ADVANCED_FACE('',(#3303),#1767,.F.);
#26497=ADVANCED_FACE('',(#3304),#1768,.F.);
#26498=ADVANCED_FACE('',(#3305),#1769,.F.);
#26499=ADVANCED_FACE('',(#3306),#1770,.F.);
#26500=ADVANCED_FACE('',(#3307),#1771,.F.);
#26501=ADVANCED_FACE('',(#3308),#1772,.F.);
#26502=ADVANCED_FACE('',(#3309),#1773,.F.);
#26503=ADVANCED_FACE('',(#3310),#1774,.F.);
#26504=ADVANCED_FACE('',(#3311),#1775,.F.);
#26505=ADVANCED_FACE('',(#3312),#1776,.F.);
#26506=ADVANCED_FACE('',(#3313),#1777,.F.);
#26507=ADVANCED_FACE('',(#3314),#1778,.F.);
#26508=ADVANCED_FACE('',(#3315),#1779,.F.);
#26509=ADVANCED_FACE('',(#3316),#1780,.F.);
#26510=ADVANCED_FACE('',(#3317),#1781,.F.);
#26511=ADVANCED_FACE('',(#3318),#1782,.F.);
#26512=ADVANCED_FACE('',(#3319),#1783,.F.);
#26513=ADVANCED_FACE('',(#3320),#1784,.F.);
#26514=ADVANCED_FACE('',(#3321),#1785,.F.);
#26515=ADVANCED_FACE('',(#3322),#1786,.F.);
#26516=ADVANCED_FACE('',(#3323),#1787,.F.);
#26517=ADVANCED_FACE('',(#3324),#1788,.F.);
#26518=ADVANCED_FACE('',(#3325),#1789,.F.);
#26519=ADVANCED_FACE('',(#3326),#1790,.F.);
#26520=ADVANCED_FACE('',(#3327),#1791,.F.);
#26521=ADVANCED_FACE('',(#3328),#1792,.F.);
#26522=ADVANCED_FACE('',(#3329),#1793,.F.);
#26523=ADVANCED_FACE('',(#3330),#1794,.F.);
#26524=ADVANCED_FACE('',(#3331),#1795,.F.);
#26525=ADVANCED_FACE('',(#3332),#1796,.F.);
#26526=ADVANCED_FACE('',(#3333),#1797,.F.);
#26527=ADVANCED_FACE('',(#3334),#1798,.F.);
#26528=ADVANCED_FACE('',(#3335),#1799,.F.);
#26529=ADVANCED_FACE('',(#3336),#1800,.F.);
#26530=ADVANCED_FACE('',(#3337),#1801,.F.);
#26531=ADVANCED_FACE('',(#3338),#1802,.F.);
#26532=ADVANCED_FACE('',(#3339),#1803,.F.);
#26533=ADVANCED_FACE('',(#3340),#1804,.F.);
#26534=ADVANCED_FACE('',(#3341),#1805,.F.);
#26535=ADVANCED_FACE('',(#3342),#1806,.F.);
#26536=ADVANCED_FACE('',(#3343),#1807,.F.);
#26537=ADVANCED_FACE('',(#3344),#1808,.F.);
#26538=ADVANCED_FACE('',(#3345),#1809,.F.);
#26539=ADVANCED_FACE('',(#3346),#1810,.F.);
#26540=ADVANCED_FACE('',(#3347),#1811,.F.);
#26541=ADVANCED_FACE('',(#3348),#1812,.F.);
#26542=ADVANCED_FACE('',(#3349),#1813,.F.);
#26543=ADVANCED_FACE('',(#3350),#1814,.F.);
#26544=ADVANCED_FACE('',(#3351),#1815,.F.);
#26545=ADVANCED_FACE('',(#3352),#1816,.F.);
#26546=ADVANCED_FACE('',(#3353),#1817,.F.);
#26547=ADVANCED_FACE('',(#3354),#1818,.F.);
#26548=ADVANCED_FACE('',(#3355),#1819,.F.);
#26549=ADVANCED_FACE('',(#3356),#1820,.F.);
#26550=ADVANCED_FACE('',(#3357),#1821,.F.);
#26551=ADVANCED_FACE('',(#3358),#1822,.F.);
#26552=ADVANCED_FACE('',(#3359),#1823,.F.);
#26553=ADVANCED_FACE('',(#3360),#1824,.F.);
#26554=ADVANCED_FACE('',(#3361),#1825,.F.);
#26555=ADVANCED_FACE('',(#3362),#1826,.F.);
#26556=ADVANCED_FACE('',(#3363),#1827,.F.);
#26557=ADVANCED_FACE('',(#3364),#1828,.F.);
#26558=ADVANCED_FACE('',(#3365),#1829,.F.);
#26559=ADVANCED_FACE('',(#3366),#1830,.F.);
#26560=ADVANCED_FACE('',(#3367),#1831,.F.);
#26561=ADVANCED_FACE('',(#3368),#1832,.F.);
#26562=ADVANCED_FACE('',(#3369),#1833,.F.);
#26563=ADVANCED_FACE('',(#3370),#1834,.F.);
#26564=ADVANCED_FACE('',(#3371),#1835,.F.);
#26565=ADVANCED_FACE('',(#3372),#1836,.F.);
#26566=ADVANCED_FACE('',(#3373),#1837,.F.);
#26567=ADVANCED_FACE('',(#3374),#1838,.F.);
#26568=ADVANCED_FACE('',(#3375),#1839,.F.);
#26569=ADVANCED_FACE('',(#3376),#1840,.F.);
#26570=ADVANCED_FACE('',(#3377),#1841,.F.);
#26571=ADVANCED_FACE('',(#3378),#1842,.F.);
#26572=ADVANCED_FACE('',(#3379),#1843,.F.);
#26573=ADVANCED_FACE('',(#3380),#1844,.F.);
#26574=ADVANCED_FACE('',(#3381),#1845,.F.);
#26575=ADVANCED_FACE('',(#3382),#1846,.F.);
#26576=ADVANCED_FACE('',(#3383),#1847,.F.);
#26577=ADVANCED_FACE('',(#3384),#1848,.F.);
#26578=ADVANCED_FACE('',(#3385),#1849,.F.);
#26579=ADVANCED_FACE('',(#3386),#1850,.F.);
#26580=ADVANCED_FACE('',(#3387),#1851,.F.);
#26581=ADVANCED_FACE('',(#3388),#1852,.F.);
#26582=ADVANCED_FACE('',(#3389),#1853,.F.);
#26583=ADVANCED_FACE('',(#3390),#1854,.F.);
#26584=ADVANCED_FACE('',(#3391),#1855,.F.);
#26585=ADVANCED_FACE('',(#3392),#1856,.F.);
#26586=ADVANCED_FACE('',(#3393),#1857,.F.);
#26587=ADVANCED_FACE('',(#3394),#1858,.F.);
#26588=ADVANCED_FACE('',(#3395),#1859,.F.);
#26589=ADVANCED_FACE('',(#3396),#1860,.F.);
#26590=ADVANCED_FACE('',(#3397),#1861,.F.);
#26591=ADVANCED_FACE('',(#3398),#1862,.F.);
#26592=ADVANCED_FACE('',(#3399),#1863,.F.);
#26593=ADVANCED_FACE('',(#3400),#1864,.F.);
#26594=ADVANCED_FACE('',(#3401),#1865,.F.);
#26595=ADVANCED_FACE('',(#3402),#1866,.F.);
#26596=ADVANCED_FACE('',(#3403),#2317,.T.);
#26597=ADVANCED_FACE('',(#3404,#1112),#1867,.T.);
#26598=ADVANCED_FACE('',(#3405),#1868,.F.);
#26599=ADVANCED_FACE('',(#3406),#1869,.F.);
#26600=ADVANCED_FACE('',(#3407),#1870,.F.);
#26601=ADVANCED_FACE('',(#3408),#1871,.F.);
#26602=ADVANCED_FACE('',(#3409),#1872,.F.);
#26603=ADVANCED_FACE('',(#3410),#1873,.F.);
#26604=ADVANCED_FACE('',(#3411),#25538,.F.);
#26605=ADVANCED_FACE('',(#3412),#1874,.F.);
#26606=ADVANCED_FACE('',(#3413),#1875,.F.);
#26607=ADVANCED_FACE('',(#3414),#1876,.F.);
#26608=ADVANCED_FACE('',(#3415),#1877,.F.);
#26609=ADVANCED_FACE('',(#3416),#1878,.F.);
#26610=ADVANCED_FACE('',(#3417),#1879,.F.);
#26611=ADVANCED_FACE('',(#3418),#2318,.T.);
#26612=ADVANCED_FACE('',(#3419),#2319,.T.);
#26613=ADVANCED_FACE('',(#3420),#2320,.T.);
#26614=ADVANCED_FACE('',(#3421),#2321,.T.);
#26615=ADVANCED_FACE('',(#3422),#2322,.T.);
#26616=ADVANCED_FACE('',(#3423),#2323,.T.);
#26617=ADVANCED_FACE('',(#3424),#2324,.T.);
#26618=ADVANCED_FACE('',(#3425),#2325,.T.);
#26619=ADVANCED_FACE('',(#3426),#2326,.T.);
#26620=ADVANCED_FACE('',(#3427),#2327,.T.);
#26621=ADVANCED_FACE('',(#3428),#2328,.T.);
#26622=ADVANCED_FACE('',(#3429),#1880,.T.);
#26623=ADVANCED_FACE('',(#3430),#901,.F.);
#26624=ADVANCED_FACE('',(#3431),#1881,.F.);
#26625=ADVANCED_FACE('',(#3432),#902,.F.);
#26626=ADVANCED_FACE('',(#3433),#506,.F.);
#26627=ADVANCED_FACE('',(#3434,#1113),#1882,.F.);
#26628=ADVANCED_FACE('',(#3435),#25539,.T.);
#26629=ADVANCED_FACE('',(#3436),#1883,.F.);
#26630=ADVANCED_FACE('',(#3437),#1884,.F.);
#26631=ADVANCED_FACE('',(#3438),#1885,.F.);
#26632=ADVANCED_FACE('',(#3439),#1886,.F.);
#26633=ADVANCED_FACE('',(#3440),#25540,.T.);
#26634=ADVANCED_FACE('',(#3441),#1887,.F.);
#26635=ADVANCED_FACE('',(#3442),#1888,.F.);
#26636=ADVANCED_FACE('',(#3443),#1889,.F.);
#26637=ADVANCED_FACE('',(#3444),#1890,.F.);
#26638=ADVANCED_FACE('',(#3445),#1891,.F.);
#26639=ADVANCED_FACE('',(#3446),#1892,.F.);
#26640=ADVANCED_FACE('',(#3447),#1893,.F.);
#26641=ADVANCED_FACE('',(#3448),#1894,.F.);
#26642=ADVANCED_FACE('',(#3449),#1895,.F.);
#26643=ADVANCED_FACE('',(#3450),#1896,.F.);
#26644=ADVANCED_FACE('',(#3451),#1897,.F.);
#26645=ADVANCED_FACE('',(#3452),#1898,.F.);
#26646=ADVANCED_FACE('',(#3453),#1899,.F.);
#26647=ADVANCED_FACE('',(#3454),#1900,.F.);
#26648=ADVANCED_FACE('',(#3455),#1901,.F.);
#26649=ADVANCED_FACE('',(#3456),#1902,.F.);
#26650=ADVANCED_FACE('',(#3457),#1903,.F.);
#26651=ADVANCED_FACE('',(#3458),#1904,.F.);
#26652=ADVANCED_FACE('',(#3459),#1905,.F.);
#26653=ADVANCED_FACE('',(#3460),#1906,.F.);
#26654=ADVANCED_FACE('',(#3461),#1907,.F.);
#26655=ADVANCED_FACE('',(#3462),#1908,.F.);
#26656=ADVANCED_FACE('',(#3463),#1909,.F.);
#26657=ADVANCED_FACE('',(#3464),#1910,.F.);
#26658=ADVANCED_FACE('',(#3465),#1911,.F.);
#26659=ADVANCED_FACE('',(#3466),#1912,.F.);
#26660=ADVANCED_FACE('',(#3467),#1913,.F.);
#26661=ADVANCED_FACE('',(#3468),#1914,.F.);
#26662=ADVANCED_FACE('',(#3469),#1915,.F.);
#26663=ADVANCED_FACE('',(#3470),#1916,.F.);
#26664=ADVANCED_FACE('',(#3471),#1917,.F.);
#26665=ADVANCED_FACE('',(#3472),#1918,.F.);
#26666=ADVANCED_FACE('',(#3473),#1919,.F.);
#26667=ADVANCED_FACE('',(#3474),#1920,.F.);
#26668=ADVANCED_FACE('',(#3475),#1921,.F.);
#26669=ADVANCED_FACE('',(#3476),#1922,.F.);
#26670=ADVANCED_FACE('',(#3477),#1923,.F.);
#26671=ADVANCED_FACE('',(#3478),#1924,.F.);
#26672=ADVANCED_FACE('',(#3479),#1925,.F.);
#26673=ADVANCED_FACE('',(#3480),#1926,.F.);
#26674=ADVANCED_FACE('',(#3481),#1927,.F.);
#26675=ADVANCED_FACE('',(#3482),#1928,.F.);
#26676=ADVANCED_FACE('',(#3483),#1929,.F.);
#26677=ADVANCED_FACE('',(#3484),#1930,.F.);
#26678=ADVANCED_FACE('',(#3485),#1931,.F.);
#26679=ADVANCED_FACE('',(#3486),#1932,.F.);
#26680=ADVANCED_FACE('',(#3487),#1933,.F.);
#26681=ADVANCED_FACE('',(#3488),#1934,.F.);
#26682=ADVANCED_FACE('',(#3489),#1935,.F.);
#26683=ADVANCED_FACE('',(#3490),#1936,.F.);
#26684=ADVANCED_FACE('',(#3491),#1937,.F.);
#26685=ADVANCED_FACE('',(#3492),#1938,.F.);
#26686=ADVANCED_FACE('',(#3493),#1939,.F.);
#26687=ADVANCED_FACE('',(#3494),#1940,.F.);
#26688=ADVANCED_FACE('',(#3495),#1941,.F.);
#26689=ADVANCED_FACE('',(#3496),#1942,.F.);
#26690=ADVANCED_FACE('',(#3497),#1943,.F.);
#26691=ADVANCED_FACE('',(#3498),#1944,.F.);
#26692=ADVANCED_FACE('',(#3499),#1945,.F.);
#26693=ADVANCED_FACE('',(#3500),#1946,.F.);
#26694=ADVANCED_FACE('',(#3501),#1947,.F.);
#26695=ADVANCED_FACE('',(#3502),#1948,.F.);
#26696=ADVANCED_FACE('',(#3503),#1949,.F.);
#26697=ADVANCED_FACE('',(#3504),#1950,.F.);
#26698=ADVANCED_FACE('',(#3505),#1951,.F.);
#26699=ADVANCED_FACE('',(#3506),#1952,.F.);
#26700=ADVANCED_FACE('',(#3507),#1953,.F.);
#26701=ADVANCED_FACE('',(#3508),#1954,.F.);
#26702=ADVANCED_FACE('',(#3509),#1955,.F.);
#26703=ADVANCED_FACE('',(#3510),#1956,.F.);
#26704=ADVANCED_FACE('',(#3511),#1957,.F.);
#26705=ADVANCED_FACE('',(#3512),#1958,.F.);
#26706=ADVANCED_FACE('',(#3513),#1959,.F.);
#26707=ADVANCED_FACE('',(#3514),#1960,.F.);
#26708=ADVANCED_FACE('',(#3515),#1961,.F.);
#26709=ADVANCED_FACE('',(#3516),#1962,.F.);
#26710=ADVANCED_FACE('',(#3517),#1963,.F.);
#26711=ADVANCED_FACE('',(#3518),#1964,.F.);
#26712=ADVANCED_FACE('',(#3519),#1965,.F.);
#26713=ADVANCED_FACE('',(#3520),#1966,.F.);
#26714=ADVANCED_FACE('',(#3521),#1967,.F.);
#26715=ADVANCED_FACE('',(#3522),#1968,.F.);
#26716=ADVANCED_FACE('',(#3523),#1969,.F.);
#26717=ADVANCED_FACE('',(#3524),#1970,.F.);
#26718=ADVANCED_FACE('',(#3525),#1971,.F.);
#26719=ADVANCED_FACE('',(#3526),#1972,.F.);
#26720=ADVANCED_FACE('',(#3527),#1973,.F.);
#26721=ADVANCED_FACE('',(#3528),#1974,.F.);
#26722=ADVANCED_FACE('',(#3529),#1975,.F.);
#26723=ADVANCED_FACE('',(#3530),#1976,.F.);
#26724=ADVANCED_FACE('',(#3531),#1977,.F.);
#26725=ADVANCED_FACE('',(#3532),#1978,.F.);
#26726=ADVANCED_FACE('',(#3533),#1979,.F.);
#26727=ADVANCED_FACE('',(#3534),#1980,.F.);
#26728=ADVANCED_FACE('',(#3535),#1981,.F.);
#26729=ADVANCED_FACE('',(#3536),#1982,.F.);
#26730=ADVANCED_FACE('',(#3537),#1983,.F.);
#26731=ADVANCED_FACE('',(#3538),#1984,.F.);
#26732=ADVANCED_FACE('',(#3539),#1985,.F.);
#26733=ADVANCED_FACE('',(#3540),#1986,.F.);
#26734=ADVANCED_FACE('',(#3541),#1987,.F.);
#26735=ADVANCED_FACE('',(#3542),#1988,.F.);
#26736=ADVANCED_FACE('',(#3543),#1989,.F.);
#26737=ADVANCED_FACE('',(#3544),#1990,.F.);
#26738=ADVANCED_FACE('',(#3545),#1991,.F.);
#26739=ADVANCED_FACE('',(#3546),#2329,.T.);
#26740=ADVANCED_FACE('',(#3547,#1114),#1992,.T.);
#26741=ADVANCED_FACE('',(#3548),#1993,.F.);
#26742=ADVANCED_FACE('',(#3549),#1994,.F.);
#26743=ADVANCED_FACE('',(#3550),#1995,.F.);
#26744=ADVANCED_FACE('',(#3551),#1996,.F.);
#26745=ADVANCED_FACE('',(#3552),#1997,.F.);
#26746=ADVANCED_FACE('',(#3553),#1998,.F.);
#26747=ADVANCED_FACE('',(#3554),#25541,.F.);
#26748=ADVANCED_FACE('',(#3555),#1999,.F.);
#26749=ADVANCED_FACE('',(#3556),#2000,.F.);
#26750=ADVANCED_FACE('',(#3557),#2001,.F.);
#26751=ADVANCED_FACE('',(#3558),#2002,.F.);
#26752=ADVANCED_FACE('',(#3559),#2003,.F.);
#26753=ADVANCED_FACE('',(#3560),#2004,.F.);
#26754=ADVANCED_FACE('',(#3561),#2330,.T.);
#26755=ADVANCED_FACE('',(#3562),#2331,.T.);
#26756=ADVANCED_FACE('',(#3563),#2332,.T.);
#26757=ADVANCED_FACE('',(#3564),#2333,.T.);
#26758=ADVANCED_FACE('',(#3565),#2334,.T.);
#26759=ADVANCED_FACE('',(#3566),#2335,.T.);
#26760=ADVANCED_FACE('',(#3567),#2336,.T.);
#26761=ADVANCED_FACE('',(#3568),#2337,.T.);
#26762=ADVANCED_FACE('',(#3569),#2338,.T.);
#26763=ADVANCED_FACE('',(#3570),#2339,.T.);
#26764=ADVANCED_FACE('',(#3571),#2340,.T.);
#26765=ADVANCED_FACE('',(#3572),#2341,.T.);
#26766=ADVANCED_FACE('',(#3573),#2342,.T.);
#26767=ADVANCED_FACE('',(#3574),#2343,.T.);
#26768=ADVANCED_FACE('',(#3575),#2344,.T.);
#26769=ADVANCED_FACE('',(#3576),#2345,.T.);
#26770=ADVANCED_FACE('',(#3577),#2346,.T.);
#26771=ADVANCED_FACE('',(#3578),#2347,.T.);
#26772=ADVANCED_FACE('',(#3579),#2348,.T.);
#26773=ADVANCED_FACE('',(#3580),#2349,.T.);
#26774=ADVANCED_FACE('',(#3581),#2350,.T.);
#26775=ADVANCED_FACE('',(#3582),#2005,.T.);
#26776=ADVANCED_FACE('',(#3583),#903,.F.);
#26777=ADVANCED_FACE('',(#3584),#2006,.F.);
#26778=ADVANCED_FACE('',(#3585),#904,.F.);
#26779=ADVANCED_FACE('',(#3586),#507,.F.);
#26780=ADVANCED_FACE('',(#3587,#1115),#2007,.F.);
#26781=ADVANCED_FACE('',(#3588),#25542,.T.);
#26782=ADVANCED_FACE('',(#3589),#2008,.F.);
#26783=ADVANCED_FACE('',(#3590),#2009,.F.);
#26784=ADVANCED_FACE('',(#3591),#2010,.F.);
#26785=ADVANCED_FACE('',(#3592),#2011,.F.);
#26786=ADVANCED_FACE('',(#3593),#25543,.T.);
#26787=ADVANCED_FACE('',(#3594),#2012,.F.);
#26788=ADVANCED_FACE('',(#3595),#2013,.F.);
#26789=ADVANCED_FACE('',(#3596),#2014,.F.);
#26790=ADVANCED_FACE('',(#3597),#2015,.F.);
#26791=ADVANCED_FACE('',(#3598),#2016,.F.);
#26792=ADVANCED_FACE('',(#3599),#2017,.F.);
#26793=ADVANCED_FACE('',(#3600),#2018,.F.);
#26794=ADVANCED_FACE('',(#3601),#2019,.F.);
#26795=ADVANCED_FACE('',(#3602),#2020,.F.);
#26796=ADVANCED_FACE('',(#3603),#2021,.F.);
#26797=ADVANCED_FACE('',(#3604),#2022,.F.);
#26798=ADVANCED_FACE('',(#3605),#2023,.F.);
#26799=ADVANCED_FACE('',(#3606),#2024,.F.);
#26800=ADVANCED_FACE('',(#3607),#2025,.F.);
#26801=ADVANCED_FACE('',(#3608),#2026,.F.);
#26802=ADVANCED_FACE('',(#3609),#2027,.F.);
#26803=ADVANCED_FACE('',(#3610),#2028,.F.);
#26804=ADVANCED_FACE('',(#3611),#2029,.F.);
#26805=ADVANCED_FACE('',(#3612),#2030,.F.);
#26806=ADVANCED_FACE('',(#3613),#2031,.F.);
#26807=ADVANCED_FACE('',(#3614),#2032,.F.);
#26808=ADVANCED_FACE('',(#3615),#2033,.F.);
#26809=ADVANCED_FACE('',(#3616),#2034,.F.);
#26810=ADVANCED_FACE('',(#3617),#2035,.F.);
#26811=ADVANCED_FACE('',(#3618),#2036,.F.);
#26812=ADVANCED_FACE('',(#3619),#2037,.F.);
#26813=ADVANCED_FACE('',(#3620),#2038,.F.);
#26814=ADVANCED_FACE('',(#3621),#2039,.F.);
#26815=ADVANCED_FACE('',(#3622),#2040,.F.);
#26816=ADVANCED_FACE('',(#3623),#2041,.F.);
#26817=ADVANCED_FACE('',(#3624),#2042,.F.);
#26818=ADVANCED_FACE('',(#3625),#2043,.F.);
#26819=ADVANCED_FACE('',(#3626),#2044,.F.);
#26820=ADVANCED_FACE('',(#3627),#2045,.F.);
#26821=ADVANCED_FACE('',(#3628),#2046,.F.);
#26822=ADVANCED_FACE('',(#3629),#2047,.F.);
#26823=ADVANCED_FACE('',(#3630),#2048,.F.);
#26824=ADVANCED_FACE('',(#3631),#2049,.F.);
#26825=ADVANCED_FACE('',(#3632),#2050,.F.);
#26826=ADVANCED_FACE('',(#3633),#2051,.F.);
#26827=ADVANCED_FACE('',(#3634),#2052,.F.);
#26828=ADVANCED_FACE('',(#3635),#2053,.F.);
#26829=ADVANCED_FACE('',(#3636),#2054,.F.);
#26830=ADVANCED_FACE('',(#3637),#2055,.F.);
#26831=ADVANCED_FACE('',(#3638),#2056,.F.);
#26832=ADVANCED_FACE('',(#3639),#2057,.F.);
#26833=ADVANCED_FACE('',(#3640),#2058,.F.);
#26834=ADVANCED_FACE('',(#3641),#2059,.F.);
#26835=ADVANCED_FACE('',(#3642),#2060,.F.);
#26836=ADVANCED_FACE('',(#3643),#2061,.F.);
#26837=ADVANCED_FACE('',(#3644),#2062,.F.);
#26838=ADVANCED_FACE('',(#3645),#2063,.F.);
#26839=ADVANCED_FACE('',(#3646),#2064,.F.);
#26840=ADVANCED_FACE('',(#3647),#2065,.F.);
#26841=ADVANCED_FACE('',(#3648),#2066,.F.);
#26842=ADVANCED_FACE('',(#3649),#2067,.F.);
#26843=ADVANCED_FACE('',(#3650),#2068,.F.);
#26844=ADVANCED_FACE('',(#3651),#2069,.F.);
#26845=ADVANCED_FACE('',(#3652),#2070,.F.);
#26846=ADVANCED_FACE('',(#3653),#2071,.F.);
#26847=ADVANCED_FACE('',(#3654),#2072,.F.);
#26848=ADVANCED_FACE('',(#3655),#2073,.F.);
#26849=ADVANCED_FACE('',(#3656),#2074,.F.);
#26850=ADVANCED_FACE('',(#3657),#2075,.F.);
#26851=ADVANCED_FACE('',(#3658),#2076,.F.);
#26852=ADVANCED_FACE('',(#3659),#2077,.F.);
#26853=ADVANCED_FACE('',(#3660),#2078,.F.);
#26854=ADVANCED_FACE('',(#3661),#2079,.F.);
#26855=ADVANCED_FACE('',(#3662),#2080,.F.);
#26856=ADVANCED_FACE('',(#3663),#2081,.F.);
#26857=ADVANCED_FACE('',(#3664),#2082,.F.);
#26858=ADVANCED_FACE('',(#3665),#2083,.F.);
#26859=ADVANCED_FACE('',(#3666),#2084,.F.);
#26860=ADVANCED_FACE('',(#3667),#2085,.F.);
#26861=ADVANCED_FACE('',(#3668),#2086,.F.);
#26862=ADVANCED_FACE('',(#3669),#2087,.F.);
#26863=ADVANCED_FACE('',(#3670),#2088,.F.);
#26864=ADVANCED_FACE('',(#3671),#2089,.F.);
#26865=ADVANCED_FACE('',(#3672),#2090,.F.);
#26866=ADVANCED_FACE('',(#3673),#2091,.F.);
#26867=ADVANCED_FACE('',(#3674),#2092,.F.);
#26868=ADVANCED_FACE('',(#3675),#2093,.F.);
#26869=ADVANCED_FACE('',(#3676),#2094,.F.);
#26870=ADVANCED_FACE('',(#3677),#2095,.F.);
#26871=ADVANCED_FACE('',(#3678),#2096,.F.);
#26872=ADVANCED_FACE('',(#3679),#2097,.F.);
#26873=ADVANCED_FACE('',(#3680),#2098,.F.);
#26874=ADVANCED_FACE('',(#3681),#2099,.F.);
#26875=ADVANCED_FACE('',(#3682),#2100,.F.);
#26876=ADVANCED_FACE('',(#3683),#2101,.F.);
#26877=ADVANCED_FACE('',(#3684),#2102,.F.);
#26878=ADVANCED_FACE('',(#3685),#2103,.F.);
#26879=ADVANCED_FACE('',(#3686),#2104,.F.);
#26880=ADVANCED_FACE('',(#3687),#2105,.F.);
#26881=ADVANCED_FACE('',(#3688),#2106,.F.);
#26882=ADVANCED_FACE('',(#3689),#2107,.F.);
#26883=ADVANCED_FACE('',(#3690),#2108,.F.);
#26884=ADVANCED_FACE('',(#3691),#2109,.F.);
#26885=ADVANCED_FACE('',(#3692),#2110,.F.);
#26886=ADVANCED_FACE('',(#3693),#2111,.F.);
#26887=ADVANCED_FACE('',(#3694),#2112,.F.);
#26888=ADVANCED_FACE('',(#3695),#2113,.F.);
#26889=ADVANCED_FACE('',(#3696),#2114,.F.);
#26890=ADVANCED_FACE('',(#3697),#2115,.F.);
#26891=ADVANCED_FACE('',(#3698),#2116,.F.);
#26892=ADVANCED_FACE('',(#3699),#2351,.T.);
#26893=ADVANCED_FACE('',(#3700,#1116),#2117,.T.);
#26894=ADVANCED_FACE('',(#3701),#2118,.F.);
#26895=ADVANCED_FACE('',(#3702),#2119,.F.);
#26896=ADVANCED_FACE('',(#3703),#2120,.F.);
#26897=ADVANCED_FACE('',(#3704),#2121,.F.);
#26898=ADVANCED_FACE('',(#3705),#2122,.F.);
#26899=ADVANCED_FACE('',(#3706),#2123,.F.);
#26900=ADVANCED_FACE('',(#3707),#25544,.F.);
#26901=ADVANCED_FACE('',(#3708),#2124,.F.);
#26902=ADVANCED_FACE('',(#3709),#2125,.F.);
#26903=ADVANCED_FACE('',(#3710),#2126,.F.);
#26904=ADVANCED_FACE('',(#3711),#2127,.F.);
#26905=ADVANCED_FACE('',(#3712),#2128,.F.);
#26906=ADVANCED_FACE('',(#3713),#2129,.F.);
#26907=ADVANCED_FACE('',(#3714),#25545,.F.);
#26908=ADVANCED_FACE('',(#3715,#1117),#2130,.T.);
#26909=ADVANCED_FACE('',(#3716),#2352,.T.);
#26910=ADVANCED_FACE('',(#3717),#25546,.T.);
#26911=ADVANCED_FACE('',(#3718,#1118),#2131,.T.);
#26912=ADVANCED_FACE('',(#3719),#2353,.F.);
#26913=ADVANCED_FACE('',(#3720),#25547,.F.);
#26914=ADVANCED_FACE('',(#3721),#2354,.F.);
#26915=ADVANCED_FACE('',(#3722,#1119),#2132,.T.);
#26916=ADVANCED_FACE('',(#3723),#2355,.T.);
#26917=ADVANCED_FACE('',(#3724),#25548,.T.);
#26918=ADVANCED_FACE('',(#3725,#1120),#2133,.T.);
#26919=ADVANCED_FACE('',(#3726),#2356,.F.);
#26920=ADVANCED_FACE('',(#3727,#1121),#2134,.F.);
#26921=ADVANCED_FACE('',(#3728),#25549,.T.);
#26922=ADVANCED_FACE('',(#3729),#2135,.T.);
#26923=ADVANCED_FACE('',(#3730),#2136,.T.);
#26924=ADVANCED_FACE('',(#3731),#2137,.T.);
#26925=ADVANCED_FACE('',(#3732),#2138,.T.);
#26926=ADVANCED_FACE('',(#3733),#2139,.T.);
#26927=ADVANCED_FACE('',(#3734),#2140,.T.);
#26928=ADVANCED_FACE('',(#3735,#1122),#2141,.F.);
#26929=CLOSED_SHELL('',(#25550,#25551,#25552,#25553,#25554,#25555,#25556,
#25557,#25558,#25559,#25560,#25561,#25562,#25563,#25564,#25565,#25566,#25567,
#25568,#25569,#25570,#25571,#25572,#25573,#25574,#25575,#25576,#25577,#25578,
#25579,#25580,#25581,#25582,#25583,#25584,#25585,#25586,#25587,#25588,#25589,
#25590,#25591,#25592,#25593,#25594,#25595,#25596,#25597,#25598,#25599,#25600,
#25601,#25602,#25603,#25604,#25605,#25606,#25607,#25608,#25609,#25610,#25611,
#25612,#25613,#25614,#25615,#25616,#25617));
#26930=CLOSED_SHELL('',(#25618,#25619,#25620,#25621,#25622,#25623,#25624,
#25625,#25626,#25627,#25628,#25629,#25630,#25631,#25632,#25633,#25634,#25635,
#25636,#25637,#25638,#25639,#25640,#25641,#25642,#25643,#25644,#25645,#25646,
#25647,#25648,#25649,#25650,#25651,#25652,#25653,#25654,#25655,#25656,#25657,
#25658,#25659,#25660,#25661,#25662,#25663,#25664,#25665,#25666,#25667,#25668,
#25669,#25670,#25671,#25672,#25673,#25674,#25675,#25676,#25677,#25678,#25679,
#25680,#25681,#25682,#25683,#25684,#25685,#25686,#25687,#25688,#25689,#25690,
#25691,#25692,#25693,#25694,#25695,#25696,#25697,#25698,#25699,#25700,#25701,
#25702,#25703,#25704,#25705,#25706,#25707,#25708,#25709,#25710,#25711,#25712,
#25713,#25714,#25715));
#26931=CLOSED_SHELL('',(#25716,#25717,#25718,#25719,#25720,#25721,#25722,
#25723,#25724,#25725,#25726,#25727,#25728,#25729,#25730,#25731,#25732,#25733,
#25734,#25735,#25736,#25737,#25738,#25739,#25740,#25741,#25742,#25743,#25744,
#25745,#25746,#25747,#25748,#25749,#25750,#25751,#25752,#25753,#25754,#25755,
#25756,#25757,#25758,#25759,#25760));
#26932=CLOSED_SHELL('',(#25761,#25762,#25763,#25764,#25765,#25766,#25767,
#25768,#25769,#25770,#25771,#25772,#25773,#25774,#25775,#25776,#25777,#25778,
#25779,#25780,#25781,#25782,#25783,#25784,#25785,#25786,#25787,#25788,#25789,
#25790,#25791,#25792,#25793,#25794,#25795,#25796,#25797,#25798,#25799,#25800,
#25801,#25802,#25803,#25804,#25805,#25806,#25807,#25808,#25809,#25810,#25811,
#25812,#25813,#25814,#25815,#25816,#25817,#25818,#25819,#25820,#25821,#25822,
#25823,#25824,#25825,#25826,#25827,#25828,#25829,#25830,#25831,#25832,#25833,
#25834,#25835,#25836,#25837,#25838,#25839,#25840,#25841,#25842,#25843,#25844,
#25845,#25846,#25847,#25848,#25849,#25850,#25851,#25852,#25853,#25854,#25855,
#25856,#25857,#25858,#25859,#25860,#25861,#25862,#25863));
#26933=CLOSED_SHELL('',(#25864,#25865,#25866,#25867,#25868,#25869,#25870,
#25871,#25872,#25873,#25874,#25875,#25876,#25877,#25878,#25879,#25880,#25881,
#25882,#25883,#25884,#25885,#25886,#25887,#25888,#25889,#25890,#25891,#25892,
#25893,#25894,#25895,#25896,#25897,#25898,#25899,#25900,#25901,#25902,#25903,
#25904,#25905,#25906,#25907,#25908,#25909,#25910,#25911,#25912,#25913,#25914,
#25915,#25916,#25917,#25918,#25919,#25920,#25921,#25922,#25923,#25924,#25925,
#25926,#25927,#25928,#25929,#25930,#25931,#25932,#25933,#25934,#25935,#25936,
#25937,#25938,#25939,#25940,#25941,#25942,#25943,#25944,#25945,#25946,#25947,
#25948,#25949,#25950,#25951,#25952,#25953,#25954,#25955,#25956,#25957,#25958,
#25959,#25960,#25961,#25962,#25963,#25964,#25965,#25966,#25967,#25968,#25969,
#25970,#25971,#25972,#25973,#25974,#25975,#25976,#25977,#25978,#25979,#25980,
#25981,#25982,#25983,#25984,#25985,#25986,#25987,#25988,#25989,#25990,#25991,
#25992,#25993,#25994,#25995,#25996,#25997,#25998,#25999,#26000,#26001,#26002,
#26003,#26004,#26005,#26006,#26007,#26008,#26009,#26010,#26011,#26012,#26013,
#26014,#26015,#26016,#26017,#26018,#26019,#26020,#26021,#26022,#26023,#26024,
#26025,#26026,#26027,#26028,#26029,#26030,#26031,#26032,#26033));
#26934=CLOSED_SHELL('',(#26034,#26035,#26036,#26037,#26038,#26039,#26040,
#26041,#26042,#26043,#26044,#26045,#26046,#26047,#26048,#26049,#26050,#26051,
#26052,#26053,#26054,#26055,#26056,#26057,#26058,#26059,#26060,#26061,#26062,
#26063,#26064,#26065,#26066,#26067,#26068,#26069,#26070,#26071,#26072,#26073,
#26074,#26075,#26076,#26077,#26078,#26079,#26080,#26081,#26082,#26083,#26084,
#26085,#26086,#26087,#26088,#26089));
#26935=CLOSED_SHELL('',(#26090,#26091,#26092,#26093,#26094,#26095,#26096,
#26097,#26098,#26099,#26100,#26101,#26102,#26103,#26104,#26105,#26106,#26107,
#26108,#26109,#26110,#26111,#26112,#26113,#26114,#26115,#26116,#26117,#26118,
#26119,#26120,#26121,#26122,#26123,#26124,#26125,#26126,#26127,#26128,#26129,
#26130,#26131,#26132,#26133,#26134,#26135,#26136,#26137,#26138,#26139,#26140,
#26141,#26142,#26143,#26144,#26145,#26146,#26147,#26148,#26149,#26150,#26151,
#26152,#26153,#26154,#26155,#26156,#26157,#26158,#26159,#26160,#26161,#26162,
#26163,#26164,#26165,#26166,#26167,#26168,#26169,#26170,#26171,#26172,#26173,
#26174,#26175,#26176,#26177,#26178,#26179,#26180,#26181,#26182,#26183,#26184,
#26185,#26186,#26187,#26188,#26189,#26190,#26191,#26192,#26193,#26194,#26195,
#26196,#26197,#26198,#26199,#26200,#26201,#26202,#26203,#26204,#26205,#26206,
#26207,#26208,#26209,#26210,#26211,#26212,#26213,#26214,#26215,#26216,#26217,
#26218,#26219,#26220,#26221,#26222,#26223,#26224,#26225,#26226,#26227,#26228,
#26229,#26230,#26231,#26232,#26233,#26234,#26235,#26236,#26237,#26238,#26239,
#26240,#26241,#26242,#26243,#26244,#26245,#26246,#26247,#26248,#26249,#26250,
#26251,#26252,#26253,#26254,#26255,#26256,#26257,#26258,#26259,#26260,#26261,
#26262,#26263,#26264,#26265,#26266,#26267,#26268,#26269,#26270,#26271,#26272,
#26273,#26274,#26275,#26276,#26277,#26278,#26279,#26280,#26281,#26282,#26283,
#26284,#26285,#26286,#26287,#26288,#26289,#26290,#26291,#26292,#26293,#26294,
#26295,#26296,#26297,#26298,#26299,#26300,#26301,#26302,#26303,#26304,#26305,
#26306,#26307,#26308,#26309,#26310,#26311,#26312,#26313,#26314,#26315,#26316,
#26317,#26318,#26319,#26320,#26321,#26322,#26323,#26324,#26325,#26326,#26327,
#26328,#26329,#26330,#26331,#26332,#26333,#26334,#26335,#26336,#26337,#26338,
#26339,#26340,#26341,#26342,#26343,#26344,#26345,#26346,#26347,#26348,#26349,
#26350,#26351,#26352,#26353,#26354,#26355,#26356,#26357,#26358,#26359,#26360,
#26361,#26362,#26363,#26364,#26365,#26366,#26367,#26368,#26369,#26370,#26371,
#26372,#26373,#26374,#26375,#26376,#26377,#26378,#26379,#26380,#26381,#26382,
#26383,#26384,#26385,#26386,#26387,#26388,#26389,#26390,#26391,#26392,#26393,
#26394,#26395));
#26936=CLOSED_SHELL('',(#26396,#26397,#26398,#26399,#26400,#26401,#26402,
#26403,#26404,#26405,#26406,#26407,#26408,#26409,#26410,#26411,#26412,#26413,
#26414,#26415,#26416,#26417,#26418,#26419,#26420,#26421,#26422,#26423,#26424,
#26425,#26426,#26427,#26428,#26429,#26430,#26431,#26432,#26433,#26434,#26435,
#26436,#26437,#26438,#26439,#26440,#26441));
#26937=CLOSED_SHELL('',(#26442,#26443,#26444,#26445,#26446,#26447,#26448,
#26449,#26450,#26451,#26452,#26453,#26454,#26455,#26456,#26457,#26458,#26459,
#26460,#26461,#26462,#26463,#26464,#26465,#26466,#26467,#26468,#26469));
#26938=CLOSED_SHELL('',(#26470,#26471,#26472,#26473,#26474,#26475,#26476,
#26477,#26478,#26479,#26480,#26481,#26482,#26483,#26484,#26485,#26486,#26487,
#26488,#26489,#26490,#26491,#26492,#26493,#26494,#26495,#26496,#26497,#26498,
#26499,#26500,#26501,#26502,#26503,#26504,#26505,#26506,#26507,#26508,#26509,
#26510,#26511,#26512,#26513,#26514,#26515,#26516,#26517,#26518,#26519,#26520,
#26521,#26522,#26523,#26524,#26525,#26526,#26527,#26528,#26529,#26530,#26531,
#26532,#26533,#26534,#26535,#26536,#26537,#26538,#26539,#26540,#26541,#26542,
#26543,#26544,#26545,#26546,#26547,#26548,#26549,#26550,#26551,#26552,#26553,
#26554,#26555,#26556,#26557,#26558,#26559,#26560,#26561,#26562,#26563,#26564,
#26565,#26566,#26567,#26568,#26569,#26570,#26571,#26572,#26573,#26574,#26575,
#26576,#26577,#26578,#26579,#26580,#26581,#26582,#26583,#26584,#26585,#26586,
#26587,#26588,#26589,#26590,#26591,#26592,#26593,#26594,#26595,#26596,#26597,
#26598,#26599,#26600,#26601,#26602,#26603,#26604,#26605,#26606,#26607,#26608,
#26609,#26610));
#26939=CLOSED_SHELL('',(#26611,#26612,#26613,#26614,#26615,#26616,#26617,
#26618,#26619,#26620,#26621,#26622,#26623,#26624,#26625,#26626,#26627,#26628,
#26629,#26630,#26631,#26632,#26633,#26634,#26635,#26636,#26637,#26638,#26639,
#26640,#26641,#26642,#26643,#26644,#26645,#26646,#26647,#26648,#26649,#26650,
#26651,#26652,#26653,#26654,#26655,#26656,#26657,#26658,#26659,#26660,#26661,
#26662,#26663,#26664,#26665,#26666,#26667,#26668,#26669,#26670,#26671,#26672,
#26673,#26674,#26675,#26676,#26677,#26678,#26679,#26680,#26681,#26682,#26683,
#26684,#26685,#26686,#26687,#26688,#26689,#26690,#26691,#26692,#26693,#26694,
#26695,#26696,#26697,#26698,#26699,#26700,#26701,#26702,#26703,#26704,#26705,
#26706,#26707,#26708,#26709,#26710,#26711,#26712,#26713,#26714,#26715,#26716,
#26717,#26718,#26719,#26720,#26721,#26722,#26723,#26724,#26725,#26726,#26727,
#26728,#26729,#26730,#26731,#26732,#26733,#26734,#26735,#26736,#26737,#26738,
#26739,#26740,#26741,#26742,#26743,#26744,#26745,#26746,#26747,#26748,#26749,
#26750,#26751,#26752,#26753));
#26940=CLOSED_SHELL('',(#26754,#26755,#26756,#26757,#26758,#26759,#26760,
#26761,#26762,#26763,#26764,#26765,#26766,#26767,#26768,#26769,#26770,#26771,
#26772,#26773,#26774,#26775,#26776,#26777,#26778,#26779,#26780,#26781,#26782,
#26783,#26784,#26785,#26786,#26787,#26788,#26789,#26790,#26791,#26792,#26793,
#26794,#26795,#26796,#26797,#26798,#26799,#26800,#26801,#26802,#26803,#26804,
#26805,#26806,#26807,#26808,#26809,#26810,#26811,#26812,#26813,#26814,#26815,
#26816,#26817,#26818,#26819,#26820,#26821,#26822,#26823,#26824,#26825,#26826,
#26827,#26828,#26829,#26830,#26831,#26832,#26833,#26834,#26835,#26836,#26837,
#26838,#26839,#26840,#26841,#26842,#26843,#26844,#26845,#26846,#26847,#26848,
#26849,#26850,#26851,#26852,#26853,#26854,#26855,#26856,#26857,#26858,#26859,
#26860,#26861,#26862,#26863,#26864,#26865,#26866,#26867,#26868,#26869,#26870,
#26871,#26872,#26873,#26874,#26875,#26876,#26877,#26878,#26879,#26880,#26881,
#26882,#26883,#26884,#26885,#26886,#26887,#26888,#26889,#26890,#26891,#26892,
#26893,#26894,#26895,#26896,#26897,#26898,#26899,#26900,#26901,#26902,#26903,
#26904,#26905,#26906));
#26941=CLOSED_SHELL('',(#26907,#26908,#26909,#26910,#26911,#26912));
#26942=CLOSED_SHELL('',(#26913,#26914,#26915,#26916,#26917,#26918,#26919,
#26920,#26921,#26922,#26923,#26924,#26925,#26926,#26927,#26928));
#26943=DERIVED_UNIT_ELEMENT(#26971,1.);
#26944=DERIVED_UNIT_ELEMENT(#83221,-3.);
#26945=DERIVED_UNIT_ELEMENT(#26971,1.);
#26946=DERIVED_UNIT_ELEMENT(#83221,-3.);
#26947=DERIVED_UNIT_ELEMENT(#26971,1.);
#26948=DERIVED_UNIT_ELEMENT(#83221,-3.);
#26949=DERIVED_UNIT_ELEMENT(#26971,1.);
#26950=DERIVED_UNIT_ELEMENT(#83221,-3.);
#26951=DERIVED_UNIT_ELEMENT(#26971,1.);
#26952=DERIVED_UNIT_ELEMENT(#83221,-3.);
#26953=DERIVED_UNIT_ELEMENT(#26971,1.);
#26954=DERIVED_UNIT_ELEMENT(#83221,-3.);
#26955=DERIVED_UNIT_ELEMENT(#26971,1.);
#26956=DERIVED_UNIT_ELEMENT(#83221,-3.);
#26957=DERIVED_UNIT_ELEMENT(#26971,1.);
#26958=DERIVED_UNIT_ELEMENT(#83221,-3.);
#26959=DERIVED_UNIT_ELEMENT(#26971,1.);
#26960=DERIVED_UNIT_ELEMENT(#83221,-3.);
#26961=DERIVED_UNIT_ELEMENT(#26971,1.);
#26962=DERIVED_UNIT_ELEMENT(#83221,-3.);
#26963=DERIVED_UNIT_ELEMENT(#26971,1.);
#26964=DERIVED_UNIT_ELEMENT(#83221,-3.);
#26965=DERIVED_UNIT_ELEMENT(#26971,1.);
#26966=DERIVED_UNIT_ELEMENT(#83221,-3.);
#26967=DERIVED_UNIT_ELEMENT(#26971,1.);
#26968=DERIVED_UNIT_ELEMENT(#83221,-3.);
#26969=DERIVED_UNIT_ELEMENT(#26971,1.);
#26970=DERIVED_UNIT_ELEMENT(#83221,-3.);
#26971=(
MASS_UNIT()
NAMED_UNIT(*)
SI_UNIT(.KILO.,.GRAM.)
);
#26972=DERIVED_UNIT((#26943,#26944));
#26973=DERIVED_UNIT((#26945,#26946));
#26974=DERIVED_UNIT((#26947,#26948));
#26975=DERIVED_UNIT((#26949,#26950));
#26976=DERIVED_UNIT((#26951,#26952));
#26977=DERIVED_UNIT((#26953,#26954));
#26978=DERIVED_UNIT((#26955,#26956));
#26979=DERIVED_UNIT((#26957,#26958));
#26980=DERIVED_UNIT((#26959,#26960));
#26981=DERIVED_UNIT((#26961,#26962));
#26982=DERIVED_UNIT((#26963,#26964));
#26983=DERIVED_UNIT((#26965,#26966));
#26984=DERIVED_UNIT((#26967,#26968));
#26985=DERIVED_UNIT((#26969,#26970));
#26986=MEASURE_REPRESENTATION_ITEM('density measure',
POSITIVE_RATIO_MEASURE(7850.),#26972);
#26987=MEASURE_REPRESENTATION_ITEM('density measure',
POSITIVE_RATIO_MEASURE(7850.),#26973);
#26988=MEASURE_REPRESENTATION_ITEM('density measure',
POSITIVE_RATIO_MEASURE(7850.),#26974);
#26989=MEASURE_REPRESENTATION_ITEM('density measure',
POSITIVE_RATIO_MEASURE(7850.),#26975);
#26990=MEASURE_REPRESENTATION_ITEM('density measure',
POSITIVE_RATIO_MEASURE(7850.),#26976);
#26991=MEASURE_REPRESENTATION_ITEM('density measure',
POSITIVE_RATIO_MEASURE(7850.),#26977);
#26992=MEASURE_REPRESENTATION_ITEM('density measure',
POSITIVE_RATIO_MEASURE(7850.),#26978);
#26993=MEASURE_REPRESENTATION_ITEM('density measure',
POSITIVE_RATIO_MEASURE(7850.),#26979);
#26994=MEASURE_REPRESENTATION_ITEM('density measure',
POSITIVE_RATIO_MEASURE(7850.),#26980);
#26995=MEASURE_REPRESENTATION_ITEM('density measure',
POSITIVE_RATIO_MEASURE(7850.),#26981);
#26996=MEASURE_REPRESENTATION_ITEM('density measure',
POSITIVE_RATIO_MEASURE(7850.),#26982);
#26997=MEASURE_REPRESENTATION_ITEM('density measure',
POSITIVE_RATIO_MEASURE(7850.),#26983);
#26998=MEASURE_REPRESENTATION_ITEM('density measure',
POSITIVE_RATIO_MEASURE(7850.),#26984);
#26999=MEASURE_REPRESENTATION_ITEM('density measure',
POSITIVE_RATIO_MEASURE(7850.),#26985);
#27000=PROPERTY_DEFINITION_REPRESENTATION(#27070,#27028);
#27001=PROPERTY_DEFINITION_REPRESENTATION(#27071,#27029);
#27002=PROPERTY_DEFINITION_REPRESENTATION(#27072,#27030);
#27003=PROPERTY_DEFINITION_REPRESENTATION(#27073,#27031);
#27004=PROPERTY_DEFINITION_REPRESENTATION(#27074,#27032);
#27005=PROPERTY_DEFINITION_REPRESENTATION(#27075,#27033);
#27006=PROPERTY_DEFINITION_REPRESENTATION(#27076,#27034);
#27007=PROPERTY_DEFINITION_REPRESENTATION(#27077,#27035);
#27008=PROPERTY_DEFINITION_REPRESENTATION(#27078,#27036);
#27009=PROPERTY_DEFINITION_REPRESENTATION(#27079,#27037);
#27010=PROPERTY_DEFINITION_REPRESENTATION(#27080,#27038);
#27011=PROPERTY_DEFINITION_REPRESENTATION(#27081,#27039);
#27012=PROPERTY_DEFINITION_REPRESENTATION(#27082,#27040);
#27013=PROPERTY_DEFINITION_REPRESENTATION(#27083,#27041);
#27014=PROPERTY_DEFINITION_REPRESENTATION(#27084,#27042);
#27015=PROPERTY_DEFINITION_REPRESENTATION(#27085,#27043);
#27016=PROPERTY_DEFINITION_REPRESENTATION(#27086,#27044);
#27017=PROPERTY_DEFINITION_REPRESENTATION(#27087,#27045);
#27018=PROPERTY_DEFINITION_REPRESENTATION(#27088,#27046);
#27019=PROPERTY_DEFINITION_REPRESENTATION(#27089,#27047);
#27020=PROPERTY_DEFINITION_REPRESENTATION(#27090,#27048);
#27021=PROPERTY_DEFINITION_REPRESENTATION(#27091,#27049);
#27022=PROPERTY_DEFINITION_REPRESENTATION(#27092,#27050);
#27023=PROPERTY_DEFINITION_REPRESENTATION(#27093,#27051);
#27024=PROPERTY_DEFINITION_REPRESENTATION(#27094,#27052);
#27025=PROPERTY_DEFINITION_REPRESENTATION(#27095,#27053);
#27026=PROPERTY_DEFINITION_REPRESENTATION(#27096,#27054);
#27027=PROPERTY_DEFINITION_REPRESENTATION(#27097,#27055);
#27028=REPRESENTATION('material name',(#27056),#83205);
#27029=REPRESENTATION('density',(#26986),#83205);
#27030=REPRESENTATION('material name',(#27057),#83206);
#27031=REPRESENTATION('density',(#26987),#83206);
#27032=REPRESENTATION('material name',(#27058),#83207);
#27033=REPRESENTATION('density',(#26988),#83207);
#27034=REPRESENTATION('material name',(#27059),#83208);
#27035=REPRESENTATION('density',(#26989),#83208);
#27036=REPRESENTATION('material name',(#27060),#83209);
#27037=REPRESENTATION('density',(#26990),#83209);
#27038=REPRESENTATION('material name',(#27061),#83210);
#27039=REPRESENTATION('density',(#26991),#83210);
#27040=REPRESENTATION('material name',(#27062),#83211);
#27041=REPRESENTATION('density',(#26992),#83211);
#27042=REPRESENTATION('material name',(#27063),#83212);
#27043=REPRESENTATION('density',(#26993),#83212);
#27044=REPRESENTATION('material name',(#27064),#83213);
#27045=REPRESENTATION('density',(#26994),#83213);
#27046=REPRESENTATION('material name',(#27065),#83214);
#27047=REPRESENTATION('density',(#26995),#83214);
#27048=REPRESENTATION('material name',(#27066),#83215);
#27049=REPRESENTATION('density',(#26996),#83215);
#27050=REPRESENTATION('material name',(#27067),#83216);
#27051=REPRESENTATION('density',(#26997),#83216);
#27052=REPRESENTATION('material name',(#27068),#83217);
#27053=REPRESENTATION('density',(#26998),#83217);
#27054=REPRESENTATION('material name',(#27069),#83218);
#27055=REPRESENTATION('density',(#26999),#83218);
#27056=DESCRIPTIVE_REPRESENTATION_ITEM('Steel','Steel');
#27057=DESCRIPTIVE_REPRESENTATION_ITEM('Steel','Steel');
#27058=DESCRIPTIVE_REPRESENTATION_ITEM('Steel','Steel');
#27059=DESCRIPTIVE_REPRESENTATION_ITEM('Steel','Steel');
#27060=DESCRIPTIVE_REPRESENTATION_ITEM('Steel','Steel');
#27061=DESCRIPTIVE_REPRESENTATION_ITEM('Steel','Steel');
#27062=DESCRIPTIVE_REPRESENTATION_ITEM('Steel','Steel');
#27063=DESCRIPTIVE_REPRESENTATION_ITEM('Steel','Steel');
#27064=DESCRIPTIVE_REPRESENTATION_ITEM('Steel','Steel');
#27065=DESCRIPTIVE_REPRESENTATION_ITEM('Steel','Steel');
#27066=DESCRIPTIVE_REPRESENTATION_ITEM('Steel','Steel');
#27067=DESCRIPTIVE_REPRESENTATION_ITEM('Steel','Steel');
#27068=DESCRIPTIVE_REPRESENTATION_ITEM('Steel','Steel');
#27069=DESCRIPTIVE_REPRESENTATION_ITEM('Steel','Steel');
#27070=PROPERTY_DEFINITION('material property','material name',#83316);
#27071=PROPERTY_DEFINITION('material property','density of part',#83316);
#27072=PROPERTY_DEFINITION('material property','material name',#83317);
#27073=PROPERTY_DEFINITION('material property','density of part',#83317);
#27074=PROPERTY_DEFINITION('material property','material name',#83318);
#27075=PROPERTY_DEFINITION('material property','density of part',#83318);
#27076=PROPERTY_DEFINITION('material property','material name',#83319);
#27077=PROPERTY_DEFINITION('material property','density of part',#83319);
#27078=PROPERTY_DEFINITION('material property','material name',#83320);
#27079=PROPERTY_DEFINITION('material property','density of part',#83320);
#27080=PROPERTY_DEFINITION('material property','material name',#83321);
#27081=PROPERTY_DEFINITION('material property','density of part',#83321);
#27082=PROPERTY_DEFINITION('material property','material name',#83322);
#27083=PROPERTY_DEFINITION('material property','density of part',#83322);
#27084=PROPERTY_DEFINITION('material property','material name',#83323);
#27085=PROPERTY_DEFINITION('material property','density of part',#83323);
#27086=PROPERTY_DEFINITION('material property','material name',#83324);
#27087=PROPERTY_DEFINITION('material property','density of part',#83324);
#27088=PROPERTY_DEFINITION('material property','material name',#83325);
#27089=PROPERTY_DEFINITION('material property','density of part',#83325);
#27090=PROPERTY_DEFINITION('material property','material name',#83326);
#27091=PROPERTY_DEFINITION('material property','density of part',#83326);
#27092=PROPERTY_DEFINITION('material property','material name',#83327);
#27093=PROPERTY_DEFINITION('material property','density of part',#83327);
#27094=PROPERTY_DEFINITION('material property','material name',#83328);
#27095=PROPERTY_DEFINITION('material property','density of part',#83328);
#27096=PROPERTY_DEFINITION('material property','material name',#83329);
#27097=PROPERTY_DEFINITION('material property','density of part',#83329);
#27098=AXIS2_PLACEMENT_3D('',#36080,#29255,#29256);
#27099=AXIS2_PLACEMENT_3D('',#36081,#29257,#29258);
#27100=AXIS2_PLACEMENT_3D('',#36082,#29259,#29260);
#27101=AXIS2_PLACEMENT_3D('',#36084,#29261,#29262);
#27102=AXIS2_PLACEMENT_3D('',#36087,#29264,#29265);
#27103=AXIS2_PLACEMENT_3D('',#36088,#29266,#29267);
#27104=AXIS2_PLACEMENT_3D('',#36092,#29269,#29270);
#27105=AXIS2_PLACEMENT_3D('',#36093,#29271,#29272);
#27106=AXIS2_PLACEMENT_3D('',#36094,#29273,#29274);
#27107=AXIS2_PLACEMENT_3D('',#36103,#29279,#29280);
#27108=AXIS2_PLACEMENT_3D('',#36105,#29281,#29282);
#27109=AXIS2_PLACEMENT_3D('',#36108,#29284,#29285);
#27110=AXIS2_PLACEMENT_3D('',#36109,#29286,#29287);
#27111=AXIS2_PLACEMENT_3D('',#36113,#29289,#29290);
#27112=AXIS2_PLACEMENT_3D('',#36114,#29291,#29292);
#27113=AXIS2_PLACEMENT_3D('',#36115,#29293,#29294);
#27114=AXIS2_PLACEMENT_3D('',#36124,#29299,#29300);
#27115=AXIS2_PLACEMENT_3D('',#36127,#29302,#29303);
#27116=AXIS2_PLACEMENT_3D('',#36130,#29305,#29306);
#27117=AXIS2_PLACEMENT_3D('',#36132,#29307,#29308);
#27118=AXIS2_PLACEMENT_3D('',#36135,#29310,#29311);
#27119=AXIS2_PLACEMENT_3D('',#36136,#29312,#29313);
#27120=AXIS2_PLACEMENT_3D('',#36140,#29315,#29316);
#27121=AXIS2_PLACEMENT_3D('',#36141,#29317,#29318);
#27122=AXIS2_PLACEMENT_3D('',#36142,#29319,#29320);
#27123=AXIS2_PLACEMENT_3D('',#36151,#29325,#29326);
#27124=AXIS2_PLACEMENT_3D('',#36153,#29327,#29328);
#27125=AXIS2_PLACEMENT_3D('',#36156,#29330,#29331);
#27126=AXIS2_PLACEMENT_3D('',#36157,#29332,#29333);
#27127=AXIS2_PLACEMENT_3D('',#36161,#29335,#29336);
#27128=AXIS2_PLACEMENT_3D('',#36162,#29337,#29338);
#27129=AXIS2_PLACEMENT_3D('',#36163,#29339,#29340);
#27130=AXIS2_PLACEMENT_3D('',#36172,#29345,#29346);
#27131=AXIS2_PLACEMENT_3D('',#36175,#29348,#29349);
#27132=AXIS2_PLACEMENT_3D('',#36178,#29351,#29352);
#27133=AXIS2_PLACEMENT_3D('',#36180,#29353,#29354);
#27134=AXIS2_PLACEMENT_3D('',#36183,#29356,#29357);
#27135=AXIS2_PLACEMENT_3D('',#36184,#29358,#29359);
#27136=AXIS2_PLACEMENT_3D('',#36186,#29360,#29361);
#27137=AXIS2_PLACEMENT_3D('',#36189,#29363,#29364);
#27138=AXIS2_PLACEMENT_3D('',#36190,#29365,#29366);
#27139=AXIS2_PLACEMENT_3D('',#36192,#29367,#29368);
#27140=AXIS2_PLACEMENT_3D('',#36195,#29370,#29371);
#27141=AXIS2_PLACEMENT_3D('',#36196,#29372,#29373);
#27142=AXIS2_PLACEMENT_3D('',#36198,#29374,#29375);
#27143=AXIS2_PLACEMENT_3D('',#36201,#29377,#29378);
#27144=AXIS2_PLACEMENT_3D('',#36202,#29379,#29380);
#27145=AXIS2_PLACEMENT_3D('',#36204,#29381,#29382);
#27146=AXIS2_PLACEMENT_3D('',#36207,#29384,#29385);
#27147=AXIS2_PLACEMENT_3D('',#36208,#29386,#29387);
#27148=AXIS2_PLACEMENT_3D('',#36250,#29408,#29409);
#27149=AXIS2_PLACEMENT_3D('',#36252,#29410,#29411);
#27150=AXIS2_PLACEMENT_3D('',#36254,#29412,#29413);
#27151=AXIS2_PLACEMENT_3D('',#36256,#29414,#29415);
#27152=AXIS2_PLACEMENT_3D('',#36257,#29416,#29417);
#27153=AXIS2_PLACEMENT_3D('',#36260,#29419,#29420);
#27154=AXIS2_PLACEMENT_3D('',#36261,#29421,#29422);
#27155=AXIS2_PLACEMENT_3D('',#36263,#29423,#29424);
#27156=AXIS2_PLACEMENT_3D('',#36265,#29426,#29427);
#27157=AXIS2_PLACEMENT_3D('',#36268,#29429,#29430);
#27158=AXIS2_PLACEMENT_3D('',#36269,#29431,#29432);
#27159=AXIS2_PLACEMENT_3D('',#36271,#29433,#29434);
#27160=AXIS2_PLACEMENT_3D('',#36273,#29436,#29437);
#27161=AXIS2_PLACEMENT_3D('',#36276,#29439,#29440);
#27162=AXIS2_PLACEMENT_3D('',#36277,#29441,#29442);
#27163=AXIS2_PLACEMENT_3D('',#36279,#29443,#29444);
#27164=AXIS2_PLACEMENT_3D('',#36281,#29446,#29447);
#27165=AXIS2_PLACEMENT_3D('',#36284,#29449,#29450);
#27166=AXIS2_PLACEMENT_3D('',#36285,#29451,#29452);
#27167=AXIS2_PLACEMENT_3D('',#36287,#29453,#29454);
#27168=AXIS2_PLACEMENT_3D('',#36289,#29456,#29457);
#27169=AXIS2_PLACEMENT_3D('',#36292,#29459,#29460);
#27170=AXIS2_PLACEMENT_3D('',#36293,#29461,#29462);
#27171=AXIS2_PLACEMENT_3D('',#36299,#29466,#29467);
#27172=AXIS2_PLACEMENT_3D('',#36302,#29470,#29471);
#27173=AXIS2_PLACEMENT_3D('',#36304,#29473,#29474);
#27174=AXIS2_PLACEMENT_3D('',#36310,#29478,#29479);
#27175=AXIS2_PLACEMENT_3D('',#36314,#29482,#29483);
#27176=AXIS2_PLACEMENT_3D('',#36319,#29487,#29488);
#27177=AXIS2_PLACEMENT_3D('',#36321,#29490,#29491);
#27178=AXIS2_PLACEMENT_3D('',#36327,#29495,#29496);
#27179=AXIS2_PLACEMENT_3D('',#36331,#29499,#29500);
#27180=AXIS2_PLACEMENT_3D('',#36335,#29503,#29504);
#27181=AXIS2_PLACEMENT_3D('',#36337,#29506,#29507);
#27182=AXIS2_PLACEMENT_3D('',#36340,#29510,#29511);
#27183=AXIS2_PLACEMENT_3D('',#36342,#29513,#29514);
#27184=AXIS2_PLACEMENT_3D('',#36344,#29516,#29517);
#27185=AXIS2_PLACEMENT_3D('',#36346,#29519,#29520);
#27186=AXIS2_PLACEMENT_3D('',#36349,#29523,#29524);
#27187=AXIS2_PLACEMENT_3D('',#36351,#29526,#29527);
#27188=AXIS2_PLACEMENT_3D('',#36355,#29530,#29531);
#27189=AXIS2_PLACEMENT_3D('',#36359,#29534,#29535);
#27190=AXIS2_PLACEMENT_3D('',#36361,#29537,#29538);
#27191=AXIS2_PLACEMENT_3D('',#36365,#29541,#29542);
#27192=AXIS2_PLACEMENT_3D('',#36369,#29545,#29546);
#27193=AXIS2_PLACEMENT_3D('',#36373,#29549,#29550);
#27194=AXIS2_PLACEMENT_3D('',#36375,#29552,#29553);
#27195=AXIS2_PLACEMENT_3D('',#36379,#29556,#29557);
#27196=AXIS2_PLACEMENT_3D('',#36383,#29560,#29561);
#27197=AXIS2_PLACEMENT_3D('',#36387,#29564,#29565);
#27198=AXIS2_PLACEMENT_3D('',#36391,#29568,#29569);
#27199=AXIS2_PLACEMENT_3D('',#36397,#29573,#29574);
#27200=AXIS2_PLACEMENT_3D('',#36401,#29577,#29578);
#27201=AXIS2_PLACEMENT_3D('',#36403,#29580,#29581);
#27202=AXIS2_PLACEMENT_3D('',#36405,#29583,#29584);
#27203=AXIS2_PLACEMENT_3D('',#36407,#29586,#29587);
#27204=AXIS2_PLACEMENT_3D('',#36413,#29591,#29592);
#27205=AXIS2_PLACEMENT_3D('',#36416,#29595,#29596);
#27206=AXIS2_PLACEMENT_3D('',#36417,#29597,#29598);
#27207=AXIS2_PLACEMENT_3D('',#36418,#29599,#29600);
#27208=AXIS2_PLACEMENT_3D('',#36419,#29601,#29602);
#27209=AXIS2_PLACEMENT_3D('',#36421,#29603,#29604);
#27210=AXIS2_PLACEMENT_3D('',#36424,#29606,#29607);
#27211=AXIS2_PLACEMENT_3D('',#36425,#29608,#29609);
#27212=AXIS2_PLACEMENT_3D('',#36430,#29611,#29612);
#27213=AXIS2_PLACEMENT_3D('',#36434,#29614,#29615);
#27214=AXIS2_PLACEMENT_3D('',#36454,#29625,#29626);
#27215=AXIS2_PLACEMENT_3D('',#36458,#29628,#29629);
#27216=AXIS2_PLACEMENT_3D('',#36475,#29638,#29639);
#27217=AXIS2_PLACEMENT_3D('',#36477,#29640,#29641);
#27218=AXIS2_PLACEMENT_3D('',#36479,#29642,#29643);
#27219=AXIS2_PLACEMENT_3D('',#36481,#29644,#29645);
#27220=AXIS2_PLACEMENT_3D('',#36483,#29646,#29647);
#27221=AXIS2_PLACEMENT_3D('',#36485,#29648,#29649);
#27222=AXIS2_PLACEMENT_3D('',#36492,#29652,#29653);
#27223=AXIS2_PLACEMENT_3D('',#36496,#29655,#29656);
#27224=AXIS2_PLACEMENT_3D('',#36502,#29659,#29660);
#27225=AXIS2_PLACEMENT_3D('',#36508,#29663,#29664);
#27226=AXIS2_PLACEMENT_3D('',#36512,#29666,#29667);
#27227=AXIS2_PLACEMENT_3D('',#36517,#29670,#29671);
#27228=AXIS2_PLACEMENT_3D('',#36519,#29672,#29673);
#27229=AXIS2_PLACEMENT_3D('',#36520,#29674,#29675);
#27230=AXIS2_PLACEMENT_3D('',#36522,#29676,#29677);
#27231=AXIS2_PLACEMENT_3D('',#36524,#29679,#29680);
#27232=AXIS2_PLACEMENT_3D('',#36526,#29681,#29682);
#27233=AXIS2_PLACEMENT_3D('',#36528,#29684,#29685);
#27234=AXIS2_PLACEMENT_3D('',#36530,#29686,#29687);
#27235=AXIS2_PLACEMENT_3D('',#36532,#29689,#29690);
#27236=AXIS2_PLACEMENT_3D('',#36534,#29691,#29692);
#27237=AXIS2_PLACEMENT_3D('',#36536,#29694,#29695);
#27238=AXIS2_PLACEMENT_3D('',#36538,#29696,#29697);
#27239=AXIS2_PLACEMENT_3D('',#36540,#29699,#29700);
#27240=AXIS2_PLACEMENT_3D('',#36542,#29701,#29702);
#27241=AXIS2_PLACEMENT_3D('',#36544,#29704,#29705);
#27242=AXIS2_PLACEMENT_3D('',#36546,#29706,#29707);
#27243=AXIS2_PLACEMENT_3D('',#36548,#29709,#29710);
#27244=AXIS2_PLACEMENT_3D('',#36550,#29711,#29712);
#27245=AXIS2_PLACEMENT_3D('',#36553,#29714,#29715);
#27246=AXIS2_PLACEMENT_3D('',#36554,#29716,#29717);
#27247=AXIS2_PLACEMENT_3D('',#36559,#29719,#29720);
#27248=AXIS2_PLACEMENT_3D('',#36563,#29722,#29723);
#27249=AXIS2_PLACEMENT_3D('',#36583,#29733,#29734);
#27250=AXIS2_PLACEMENT_3D('',#36587,#29736,#29737);
#27251=AXIS2_PLACEMENT_3D('',#36604,#29746,#29747);
#27252=AXIS2_PLACEMENT_3D('',#36609,#29749,#29750);
#27253=AXIS2_PLACEMENT_3D('',#36613,#29752,#29753);
#27254=AXIS2_PLACEMENT_3D('',#36619,#29756,#29757);
#27255=AXIS2_PLACEMENT_3D('',#36625,#29760,#29761);
#27256=AXIS2_PLACEMENT_3D('',#36629,#29763,#29764);
#27257=AXIS2_PLACEMENT_3D('',#36635,#29767,#29768);
#27258=AXIS2_PLACEMENT_3D('',#36638,#29770,#29771);
#27259=AXIS2_PLACEMENT_3D('',#36640,#29772,#29773);
#27260=AXIS2_PLACEMENT_3D('',#36641,#29774,#29775);
#27261=AXIS2_PLACEMENT_3D('',#36643,#29777,#29778);
#27262=AXIS2_PLACEMENT_3D('',#36645,#29779,#29780);
#27263=AXIS2_PLACEMENT_3D('',#36647,#29782,#29783);
#27264=AXIS2_PLACEMENT_3D('',#36649,#29785,#29786);
#27265=AXIS2_PLACEMENT_3D('',#36651,#29787,#29788);
#27266=AXIS2_PLACEMENT_3D('',#36653,#29790,#29791);
#27267=AXIS2_PLACEMENT_3D('',#36655,#29793,#29794);
#27268=AXIS2_PLACEMENT_3D('',#36657,#29795,#29796);
#27269=AXIS2_PLACEMENT_3D('',#36659,#29798,#29799);
#27270=AXIS2_PLACEMENT_3D('',#36661,#29801,#29802);
#27271=AXIS2_PLACEMENT_3D('',#36667,#29806,#29807);
#27272=AXIS2_PLACEMENT_3D('',#36671,#29810,#29811);
#27273=AXIS2_PLACEMENT_3D('',#36675,#29814,#29815);
#27274=AXIS2_PLACEMENT_3D('',#36679,#29818,#29819);
#27275=AXIS2_PLACEMENT_3D('',#36685,#29823,#29824);
#27276=AXIS2_PLACEMENT_3D('',#36689,#29827,#29828);
#27277=AXIS2_PLACEMENT_3D('',#36693,#29831,#29832);
#27278=AXIS2_PLACEMENT_3D('',#36697,#29835,#29836);
#27279=AXIS2_PLACEMENT_3D('',#36701,#29839,#29840);
#27280=AXIS2_PLACEMENT_3D('',#36705,#29843,#29844);
#27281=AXIS2_PLACEMENT_3D('',#36709,#29847,#29848);
#27282=AXIS2_PLACEMENT_3D('',#36713,#29851,#29852);
#27283=AXIS2_PLACEMENT_3D('',#36719,#29856,#29857);
#27284=AXIS2_PLACEMENT_3D('',#36722,#29859,#29860);
#27285=AXIS2_PLACEMENT_3D('',#36723,#29861,#29862);
#27286=AXIS2_PLACEMENT_3D('',#36727,#29865,#29866);
#27287=AXIS2_PLACEMENT_3D('',#36730,#29868,#29869);
#27288=AXIS2_PLACEMENT_3D('',#36731,#29870,#29871);
#27289=AXIS2_PLACEMENT_3D('',#36733,#29873,#29874);
#27290=AXIS2_PLACEMENT_3D('',#36736,#29876,#29877);
#27291=AXIS2_PLACEMENT_3D('',#36737,#29878,#29879);
#27292=AXIS2_PLACEMENT_3D('',#36741,#29882,#29883);
#27293=AXIS2_PLACEMENT_3D('',#36744,#29885,#29886);
#27294=AXIS2_PLACEMENT_3D('',#36745,#29887,#29888);
#27295=AXIS2_PLACEMENT_3D('',#36747,#29890,#29891);
#27296=AXIS2_PLACEMENT_3D('',#36751,#29894,#29895);
#27297=AXIS2_PLACEMENT_3D('',#36755,#29898,#29899);
#27298=AXIS2_PLACEMENT_3D('',#36757,#29901,#29902);
#27299=AXIS2_PLACEMENT_3D('',#36760,#29905,#29906);
#27300=AXIS2_PLACEMENT_3D('',#36762,#29908,#29909);
#27301=AXIS2_PLACEMENT_3D('',#36764,#29911,#29912);
#27302=AXIS2_PLACEMENT_3D('',#36766,#29914,#29915);
#27303=AXIS2_PLACEMENT_3D('',#36768,#29917,#29918);
#27304=AXIS2_PLACEMENT_3D('',#36770,#29920,#29921);
#27305=AXIS2_PLACEMENT_3D('',#36772,#29923,#29924);
#27306=AXIS2_PLACEMENT_3D('',#36774,#29926,#29927);
#27307=AXIS2_PLACEMENT_3D('',#36776,#29929,#29930);
#27308=AXIS2_PLACEMENT_3D('',#36778,#29932,#29933);
#27309=AXIS2_PLACEMENT_3D('',#36780,#29935,#29936);
#27310=AXIS2_PLACEMENT_3D('',#36782,#29938,#29939);
#27311=AXIS2_PLACEMENT_3D('',#36788,#29943,#29944);
#27312=AXIS2_PLACEMENT_3D('',#36794,#29948,#29949);
#27313=AXIS2_PLACEMENT_3D('',#36800,#29953,#29954);
#27314=AXIS2_PLACEMENT_3D('',#36803,#29956,#29957);
#27315=AXIS2_PLACEMENT_3D('',#36804,#29958,#29959);
#27316=AXIS2_PLACEMENT_3D('',#36806,#29961,#29962);
#27317=AXIS2_PLACEMENT_3D('',#36812,#29966,#29967);
#27318=AXIS2_PLACEMENT_3D('',#36815,#29969,#29970);
#27319=AXIS2_PLACEMENT_3D('',#36816,#29971,#29972);
#27320=AXIS2_PLACEMENT_3D('',#36820,#29975,#29976);
#27321=AXIS2_PLACEMENT_3D('',#36823,#29978,#29979);
#27322=AXIS2_PLACEMENT_3D('',#36824,#29980,#29981);
#27323=AXIS2_PLACEMENT_3D('',#36826,#29983,#29984);
#27324=AXIS2_PLACEMENT_3D('',#36829,#29986,#29987);
#27325=AXIS2_PLACEMENT_3D('',#36830,#29988,#29989);
#27326=AXIS2_PLACEMENT_3D('',#36834,#29992,#29993);
#27327=AXIS2_PLACEMENT_3D('',#36837,#29995,#29996);
#27328=AXIS2_PLACEMENT_3D('',#36838,#29997,#29998);
#27329=AXIS2_PLACEMENT_3D('',#36840,#30000,#30001);
#27330=AXIS2_PLACEMENT_3D('',#36843,#30003,#30004);
#27331=AXIS2_PLACEMENT_3D('',#36844,#30005,#30006);
#27332=AXIS2_PLACEMENT_3D('',#36846,#30008,#30009);
#27333=AXIS2_PLACEMENT_3D('',#36849,#30012,#30013);
#27334=AXIS2_PLACEMENT_3D('',#36851,#30015,#30016);
#27335=AXIS2_PLACEMENT_3D('',#36853,#30018,#30019);
#27336=AXIS2_PLACEMENT_3D('',#36855,#30021,#30022);
#27337=AXIS2_PLACEMENT_3D('',#36857,#30024,#30025);
#27338=AXIS2_PLACEMENT_3D('',#36859,#30027,#30028);
#27339=AXIS2_PLACEMENT_3D('',#36861,#30030,#30031);
#27340=AXIS2_PLACEMENT_3D('',#36863,#30033,#30034);
#27341=AXIS2_PLACEMENT_3D('',#36865,#30036,#30037);
#27342=AXIS2_PLACEMENT_3D('',#36868,#30040,#30041);
#27343=AXIS2_PLACEMENT_3D('',#36869,#30042,#30043);
#27344=AXIS2_PLACEMENT_3D('',#36871,#30045,#30046);
#27345=AXIS2_PLACEMENT_3D('',#36873,#30048,#30049);
#27346=AXIS2_PLACEMENT_3D('',#36875,#30051,#30052);
#27347=AXIS2_PLACEMENT_3D('',#36877,#30054,#30055);
#27348=AXIS2_PLACEMENT_3D('',#36878,#30056,#30057);
#27349=AXIS2_PLACEMENT_3D('',#36880,#30059,#30060);
#27350=AXIS2_PLACEMENT_3D('',#36883,#30063,#30064);
#27351=AXIS2_PLACEMENT_3D('',#36884,#30065,#30066);
#27352=AXIS2_PLACEMENT_3D('',#36886,#30068,#30069);
#27353=AXIS2_PLACEMENT_3D('',#36889,#30072,#30073);
#27354=AXIS2_PLACEMENT_3D('',#36891,#30075,#30076);
#27355=AXIS2_PLACEMENT_3D('',#36892,#30077,#30078);
#27356=AXIS2_PLACEMENT_3D('',#36894,#30080,#30081);
#27357=AXIS2_PLACEMENT_3D('',#36896,#30083,#30084);
#27358=AXIS2_PLACEMENT_3D('',#36898,#30086,#30087);
#27359=AXIS2_PLACEMENT_3D('',#36900,#30089,#30090);
#27360=AXIS2_PLACEMENT_3D('',#36901,#30091,#30092);
#27361=AXIS2_PLACEMENT_3D('',#36902,#30093,#30094);
#27362=AXIS2_PLACEMENT_3D('',#36904,#30095,#30096);
#27363=AXIS2_PLACEMENT_3D('',#36907,#30098,#30099);
#27364=AXIS2_PLACEMENT_3D('',#36908,#30100,#30101);
#27365=AXIS2_PLACEMENT_3D('',#36909,#30102,#30103);
#27366=AXIS2_PLACEMENT_3D('',#36911,#30104,#30105);
#27367=AXIS2_PLACEMENT_3D('',#36914,#30107,#30108);
#27368=AXIS2_PLACEMENT_3D('',#36915,#30109,#30110);
#27369=AXIS2_PLACEMENT_3D('',#36917,#30111,#30112);
#27370=AXIS2_PLACEMENT_3D('',#36920,#30114,#30115);
#27371=AXIS2_PLACEMENT_3D('',#36921,#30116,#30117);
#27372=AXIS2_PLACEMENT_3D('',#36923,#30118,#30119);
#27373=AXIS2_PLACEMENT_3D('',#36926,#30121,#30122);
#27374=AXIS2_PLACEMENT_3D('',#36927,#30123,#30124);
#27375=AXIS2_PLACEMENT_3D('',#36929,#30125,#30126);
#27376=AXIS2_PLACEMENT_3D('',#36932,#30128,#30129);
#27377=AXIS2_PLACEMENT_3D('',#36933,#30130,#30131);
#27378=AXIS2_PLACEMENT_3D('',#36935,#30132,#30133);
#27379=AXIS2_PLACEMENT_3D('',#36938,#30135,#30136);
#27380=AXIS2_PLACEMENT_3D('',#36939,#30137,#30138);
#27381=AXIS2_PLACEMENT_3D('',#36942,#30140,#30141);
#27382=AXIS2_PLACEMENT_3D('',#36943,#30142,#30143);
#27383=AXIS2_PLACEMENT_3D('',#36945,#30144,#30145);
#27384=AXIS2_PLACEMENT_3D('',#36946,#30146,#30147);
#27385=AXIS2_PLACEMENT_3D('',#36949,#30149,#30150);
#27386=AXIS2_PLACEMENT_3D('',#36951,#30151,#30152);
#27387=AXIS2_PLACEMENT_3D('',#36954,#30154,#30155);
#27388=AXIS2_PLACEMENT_3D('',#36955,#30156,#30157);
#27389=AXIS2_PLACEMENT_3D('',#36957,#30159,#30160);
#27390=AXIS2_PLACEMENT_3D('',#36959,#30161,#30162);
#27391=AXIS2_PLACEMENT_3D('',#36962,#30164,#30165);
#27392=AXIS2_PLACEMENT_3D('',#36963,#30166,#30167);
#27393=AXIS2_PLACEMENT_3D('',#36965,#30168,#30169);
#27394=AXIS2_PLACEMENT_3D('',#36966,#30170,#30171);
#27395=AXIS2_PLACEMENT_3D('',#36968,#30173,#30174);
#27396=AXIS2_PLACEMENT_3D('',#36977,#30179,#30180);
#27397=AXIS2_PLACEMENT_3D('',#36979,#30181,#30182);
#27398=AXIS2_PLACEMENT_3D('',#36981,#30183,#30184);
#27399=AXIS2_PLACEMENT_3D('',#36983,#30186,#30187);
#27400=AXIS2_PLACEMENT_3D('',#36986,#30188,#30189);
#27401=AXIS2_PLACEMENT_3D('',#36990,#30191,#30192);
#27402=AXIS2_PLACEMENT_3D('',#36992,#30194,#30195);
#27403=AXIS2_PLACEMENT_3D('',#36998,#30199,#30200);
#27404=AXIS2_PLACEMENT_3D('',#37000,#30201,#30202);
#27405=AXIS2_PLACEMENT_3D('',#37002,#30203,#30204);
#27406=AXIS2_PLACEMENT_3D('',#37004,#30206,#30207);
#27407=AXIS2_PLACEMENT_3D('',#37006,#30208,#30209);
#27408=AXIS2_PLACEMENT_3D('',#37009,#30211,#30212);
#27409=AXIS2_PLACEMENT_3D('',#37010,#30213,#30214);
#27410=AXIS2_PLACEMENT_3D('',#37013,#30217,#30218);
#27411=AXIS2_PLACEMENT_3D('',#37017,#30220,#30221);
#27412=AXIS2_PLACEMENT_3D('',#37021,#30223,#30224);
#27413=AXIS2_PLACEMENT_3D('',#37023,#30226,#30227);
#27414=AXIS2_PLACEMENT_3D('',#37027,#30229,#30230);
#27415=AXIS2_PLACEMENT_3D('',#37031,#30232,#30233);
#27416=AXIS2_PLACEMENT_3D('',#37033,#30235,#30236);
#27417=AXIS2_PLACEMENT_3D('',#37036,#30237,#30238);
#27418=AXIS2_PLACEMENT_3D('',#37040,#30240,#30241);
#27419=AXIS2_PLACEMENT_3D('',#37044,#30243,#30244);
#27420=AXIS2_PLACEMENT_3D('',#37048,#30246,#30247);
#27421=AXIS2_PLACEMENT_3D('',#37050,#30249,#30250);
#27422=AXIS2_PLACEMENT_3D('',#37053,#30253,#30254);
#27423=AXIS2_PLACEMENT_3D('',#37055,#30256,#30257);
#27424=AXIS2_PLACEMENT_3D('',#37061,#30261,#30262);
#27425=AXIS2_PLACEMENT_3D('',#37063,#30263,#30264);
#27426=AXIS2_PLACEMENT_3D('',#37065,#30266,#30267);
#27427=AXIS2_PLACEMENT_3D('',#37069,#30270,#30271);
#27428=AXIS2_PLACEMENT_3D('',#37071,#30272,#30273);
#27429=AXIS2_PLACEMENT_3D('',#37073,#30275,#30276);
#27430=AXIS2_PLACEMENT_3D('',#37078,#30280,#30281);
#27431=AXIS2_PLACEMENT_3D('',#37079,#30282,#30283);
#27432=AXIS2_PLACEMENT_3D('',#37081,#30284,#30285);
#27433=AXIS2_PLACEMENT_3D('',#37083,#30286,#30287);
#27434=AXIS2_PLACEMENT_3D('',#37085,#30289,#30290);
#27435=AXIS2_PLACEMENT_3D('',#37087,#30291,#30292);
#27436=AXIS2_PLACEMENT_3D('',#37090,#30294,#30295);
#27437=AXIS2_PLACEMENT_3D('',#37091,#30296,#30297);
#27438=AXIS2_PLACEMENT_3D('',#37097,#30301,#30302);
#27439=AXIS2_PLACEMENT_3D('',#37099,#30303,#30304);
#27440=AXIS2_PLACEMENT_3D('',#37101,#30305,#30306);
#27441=AXIS2_PLACEMENT_3D('',#37103,#30308,#30309);
#27442=AXIS2_PLACEMENT_3D('',#37109,#30313,#30314);
#27443=AXIS2_PLACEMENT_3D('',#37111,#30315,#30316);
#27444=AXIS2_PLACEMENT_3D('',#37112,#30317,#30318);
#27445=AXIS2_PLACEMENT_3D('',#37114,#30320,#30321);
#27446=AXIS2_PLACEMENT_3D('',#37118,#30324,#30325);
#27447=AXIS2_PLACEMENT_3D('',#37120,#30326,#30327);
#27448=AXIS2_PLACEMENT_3D('',#37122,#30329,#30330);
#27449=AXIS2_PLACEMENT_3D('',#37126,#30333,#30334);
#27450=AXIS2_PLACEMENT_3D('',#37127,#30335,#30336);
#27451=AXIS2_PLACEMENT_3D('',#37128,#30337,#30338);
#27452=AXIS2_PLACEMENT_3D('',#37129,#30339,#30340);
#27453=AXIS2_PLACEMENT_3D('',#37130,#30341,#30342);
#27454=AXIS2_PLACEMENT_3D('',#37131,#30343,#30344);
#27455=AXIS2_PLACEMENT_3D('',#37140,#30349,#30350);
#27456=AXIS2_PLACEMENT_3D('',#37143,#30351,#30352);
#27457=AXIS2_PLACEMENT_3D('',#37147,#30354,#30355);
#27458=AXIS2_PLACEMENT_3D('',#37292,#30358,#30359);
#27459=AXIS2_PLACEMENT_3D('',#37438,#30363,#30364);
#27460=AXIS2_PLACEMENT_3D('',#37440,#30365,#30366);
#27461=AXIS2_PLACEMENT_3D('',#37480,#30368,#30369);
#27462=AXIS2_PLACEMENT_3D('',#37520,#30371,#30372);
#27463=AXIS2_PLACEMENT_3D('',#37560,#30374,#30375);
#27464=AXIS2_PLACEMENT_3D('',#37600,#30377,#30378);
#27465=AXIS2_PLACEMENT_3D('',#37640,#30380,#30381);
#27466=AXIS2_PLACEMENT_3D('',#37680,#30383,#30384);
#27467=AXIS2_PLACEMENT_3D('',#37720,#30386,#30387);
#27468=AXIS2_PLACEMENT_3D('',#37760,#30389,#30390);
#27469=AXIS2_PLACEMENT_3D('',#37800,#30392,#30393);
#27470=AXIS2_PLACEMENT_3D('',#37840,#30395,#30396);
#27471=AXIS2_PLACEMENT_3D('',#37880,#30398,#30399);
#27472=AXIS2_PLACEMENT_3D('',#37920,#30401,#30402);
#27473=AXIS2_PLACEMENT_3D('',#37960,#30404,#30405);
#27474=AXIS2_PLACEMENT_3D('',#38000,#30407,#30408);
#27475=AXIS2_PLACEMENT_3D('',#38040,#30410,#30411);
#27476=AXIS2_PLACEMENT_3D('',#38080,#30413,#30414);
#27477=AXIS2_PLACEMENT_3D('',#38120,#30416,#30417);
#27478=AXIS2_PLACEMENT_3D('',#38160,#30419,#30420);
#27479=AXIS2_PLACEMENT_3D('',#38200,#30422,#30423);
#27480=AXIS2_PLACEMENT_3D('',#38240,#30425,#30426);
#27481=AXIS2_PLACEMENT_3D('',#38280,#30428,#30429);
#27482=AXIS2_PLACEMENT_3D('',#38320,#30431,#30432);
#27483=AXIS2_PLACEMENT_3D('',#38360,#30434,#30435);
#27484=AXIS2_PLACEMENT_3D('',#38400,#30437,#30438);
#27485=AXIS2_PLACEMENT_3D('',#38440,#30440,#30441);
#27486=AXIS2_PLACEMENT_3D('',#38480,#30443,#30444);
#27487=AXIS2_PLACEMENT_3D('',#38520,#30446,#30447);
#27488=AXIS2_PLACEMENT_3D('',#38560,#30449,#30450);
#27489=AXIS2_PLACEMENT_3D('',#38600,#30452,#30453);
#27490=AXIS2_PLACEMENT_3D('',#38639,#30455,#30456);
#27491=AXIS2_PLACEMENT_3D('',#38641,#30457,#30458);
#27492=AXIS2_PLACEMENT_3D('',#38642,#30459,#30460);
#27493=AXIS2_PLACEMENT_3D('',#38644,#30461,#30462);
#27494=AXIS2_PLACEMENT_3D('',#38646,#30464,#30465);
#27495=AXIS2_PLACEMENT_3D('',#38650,#30468,#30469);
#27496=AXIS2_PLACEMENT_3D('',#38654,#30471,#30472);
#27497=AXIS2_PLACEMENT_3D('',#38763,#30475,#30476);
#27498=AXIS2_PLACEMENT_3D('',#38872,#30479,#30480);
#27499=AXIS2_PLACEMENT_3D('',#38874,#30481,#30482);
#27500=AXIS2_PLACEMENT_3D('',#38876,#30484,#30485);
#27501=AXIS2_PLACEMENT_3D('',#38880,#30488,#30489);
#27502=AXIS2_PLACEMENT_3D('',#38884,#30491,#30492);
#27503=AXIS2_PLACEMENT_3D('',#38993,#30495,#30496);
#27504=AXIS2_PLACEMENT_3D('',#39102,#30499,#30500);
#27505=AXIS2_PLACEMENT_3D('',#39104,#30501,#30502);
#27506=AXIS2_PLACEMENT_3D('',#39106,#30504,#30505);
#27507=AXIS2_PLACEMENT_3D('',#39110,#30508,#30509);
#27508=AXIS2_PLACEMENT_3D('',#39114,#30511,#30512);
#27509=AXIS2_PLACEMENT_3D('',#39223,#30515,#30516);
#27510=AXIS2_PLACEMENT_3D('',#39332,#30519,#30520);
#27511=AXIS2_PLACEMENT_3D('',#39334,#30521,#30522);
#27512=AXIS2_PLACEMENT_3D('',#39336,#30524,#30525);
#27513=AXIS2_PLACEMENT_3D('',#39340,#30528,#30529);
#27514=AXIS2_PLACEMENT_3D('',#39344,#30531,#30532);
#27515=AXIS2_PLACEMENT_3D('',#39453,#30535,#30536);
#27516=AXIS2_PLACEMENT_3D('',#39562,#30539,#30540);
#27517=AXIS2_PLACEMENT_3D('',#39564,#30541,#30542);
#27518=AXIS2_PLACEMENT_3D('',#39566,#30544,#30545);
#27519=AXIS2_PLACEMENT_3D('',#39570,#30548,#30549);
#27520=AXIS2_PLACEMENT_3D('',#39574,#30551,#30552);
#27521=AXIS2_PLACEMENT_3D('',#39683,#30555,#30556);
#27522=AXIS2_PLACEMENT_3D('',#39792,#30559,#30560);
#27523=AXIS2_PLACEMENT_3D('',#39794,#30561,#30562);
#27524=AXIS2_PLACEMENT_3D('',#39796,#30564,#30565);
#27525=AXIS2_PLACEMENT_3D('',#39800,#30568,#30569);
#27526=AXIS2_PLACEMENT_3D('',#39804,#30571,#30572);
#27527=AXIS2_PLACEMENT_3D('',#39913,#30575,#30576);
#27528=AXIS2_PLACEMENT_3D('',#40022,#30579,#30580);
#27529=AXIS2_PLACEMENT_3D('',#40024,#30581,#30582);
#27530=AXIS2_PLACEMENT_3D('',#40026,#30584,#30585);
#27531=AXIS2_PLACEMENT_3D('',#40030,#30588,#30589);
#27532=AXIS2_PLACEMENT_3D('',#40034,#30591,#30592);
#27533=AXIS2_PLACEMENT_3D('',#40143,#30595,#30596);
#27534=AXIS2_PLACEMENT_3D('',#40252,#30599,#30600);
#27535=AXIS2_PLACEMENT_3D('',#40254,#30601,#30602);
#27536=AXIS2_PLACEMENT_3D('',#40256,#30604,#30605);
#27537=AXIS2_PLACEMENT_3D('',#40260,#30608,#30609);
#27538=AXIS2_PLACEMENT_3D('',#40264,#30611,#30612);
#27539=AXIS2_PLACEMENT_3D('',#40373,#30615,#30616);
#27540=AXIS2_PLACEMENT_3D('',#40482,#30619,#30620);
#27541=AXIS2_PLACEMENT_3D('',#40484,#30621,#30622);
#27542=AXIS2_PLACEMENT_3D('',#40486,#30624,#30625);
#27543=AXIS2_PLACEMENT_3D('',#40490,#30628,#30629);
#27544=AXIS2_PLACEMENT_3D('',#40494,#30631,#30632);
#27545=AXIS2_PLACEMENT_3D('',#40603,#30635,#30636);
#27546=AXIS2_PLACEMENT_3D('',#40712,#30639,#30640);
#27547=AXIS2_PLACEMENT_3D('',#40714,#30641,#30642);
#27548=AXIS2_PLACEMENT_3D('',#40716,#30644,#30645);
#27549=AXIS2_PLACEMENT_3D('',#40720,#30648,#30649);
#27550=AXIS2_PLACEMENT_3D('',#40724,#30651,#30652);
#27551=AXIS2_PLACEMENT_3D('',#40833,#30655,#30656);
#27552=AXIS2_PLACEMENT_3D('',#40942,#30659,#30660);
#27553=AXIS2_PLACEMENT_3D('',#40944,#30661,#30662);
#27554=AXIS2_PLACEMENT_3D('',#40946,#30664,#30665);
#27555=AXIS2_PLACEMENT_3D('',#40950,#30668,#30669);
#27556=AXIS2_PLACEMENT_3D('',#40954,#30671,#30672);
#27557=AXIS2_PLACEMENT_3D('',#41063,#30675,#30676);
#27558=AXIS2_PLACEMENT_3D('',#41172,#30679,#30680);
#27559=AXIS2_PLACEMENT_3D('',#41174,#30681,#30682);
#27560=AXIS2_PLACEMENT_3D('',#41176,#30684,#30685);
#27561=AXIS2_PLACEMENT_3D('',#41180,#30688,#30689);
#27562=AXIS2_PLACEMENT_3D('',#41184,#30691,#30692);
#27563=AXIS2_PLACEMENT_3D('',#41293,#30695,#30696);
#27564=AXIS2_PLACEMENT_3D('',#41402,#30699,#30700);
#27565=AXIS2_PLACEMENT_3D('',#41404,#30701,#30702);
#27566=AXIS2_PLACEMENT_3D('',#41406,#30704,#30705);
#27567=AXIS2_PLACEMENT_3D('',#41410,#30708,#30709);
#27568=AXIS2_PLACEMENT_3D('',#41414,#30711,#30712);
#27569=AXIS2_PLACEMENT_3D('',#41523,#30715,#30716);
#27570=AXIS2_PLACEMENT_3D('',#41632,#30719,#30720);
#27571=AXIS2_PLACEMENT_3D('',#41634,#30721,#30722);
#27572=AXIS2_PLACEMENT_3D('',#41636,#30724,#30725);
#27573=AXIS2_PLACEMENT_3D('',#41642,#30729,#30730);
#27574=AXIS2_PLACEMENT_3D('',#41646,#30733,#30734);
#27575=AXIS2_PLACEMENT_3D('',#41650,#30736,#30737);
#27576=AXIS2_PLACEMENT_3D('',#41862,#30739,#30740);
#27577=AXIS2_PLACEMENT_3D('',#41864,#30741,#30742);
#27578=AXIS2_PLACEMENT_3D('',#41904,#30744,#30745);
#27579=AXIS2_PLACEMENT_3D('',#41943,#30747,#30748);
#27580=AXIS2_PLACEMENT_3D('',#41945,#30749,#30750);
#27581=AXIS2_PLACEMENT_3D('',#41946,#30751,#30752);
#27582=AXIS2_PLACEMENT_3D('',#41948,#30754,#30755);
#27583=AXIS2_PLACEMENT_3D('',#41950,#30757,#30758);
#27584=AXIS2_PLACEMENT_3D('',#42023,#30761,#30762);
#27585=AXIS2_PLACEMENT_3D('',#42096,#30765,#30766);
#27586=AXIS2_PLACEMENT_3D('',#42097,#30767,#30768);
#27587=AXIS2_PLACEMENT_3D('',#42099,#30769,#30770);
#27588=AXIS2_PLACEMENT_3D('',#42101,#30771,#30772);
#27589=AXIS2_PLACEMENT_3D('',#42102,#30773,#30774);
#27590=AXIS2_PLACEMENT_3D('',#42104,#30775,#30776);
#27591=AXIS2_PLACEMENT_3D('',#42106,#30778,#30779);
#27592=AXIS2_PLACEMENT_3D('',#42108,#30780,#30781);
#27593=AXIS2_PLACEMENT_3D('',#42109,#30782,#30783);
#27594=AXIS2_PLACEMENT_3D('',#42111,#30785,#30786);
#27595=AXIS2_PLACEMENT_3D('',#42113,#30788,#30789);
#27596=AXIS2_PLACEMENT_3D('',#42114,#30790,#30791);
#27597=AXIS2_PLACEMENT_3D('',#42217,#30793,#30794);
#27598=AXIS2_PLACEMENT_3D('',#42279,#30795,#30796);
#27599=AXIS2_PLACEMENT_3D('',#42523,#30798,#30799);
#27600=AXIS2_PLACEMENT_3D('',#42836,#30801,#30802);
#27601=AXIS2_PLACEMENT_3D('',#43219,#30804,#30805);
#27602=AXIS2_PLACEMENT_3D('',#43575,#30807,#30808);
#27603=AXIS2_PLACEMENT_3D('',#43951,#30810,#30811);
#27604=AXIS2_PLACEMENT_3D('',#44323,#30813,#30814);
#27605=AXIS2_PLACEMENT_3D('',#44571,#30816,#30817);
#27606=AXIS2_PLACEMENT_3D('',#44900,#30819,#30820);
#27607=AXIS2_PLACEMENT_3D('',#45261,#30822,#30823);
#27608=AXIS2_PLACEMENT_3D('',#45504,#30825,#30826);
#27609=AXIS2_PLACEMENT_3D('',#45568,#30828,#30829);
#27610=AXIS2_PLACEMENT_3D('',#45574,#30830,#30831);
#27611=AXIS2_PLACEMENT_3D('',#45922,#30833,#30834);
#27612=AXIS2_PLACEMENT_3D('',#46108,#30836,#30837);
#27613=AXIS2_PLACEMENT_3D('',#46456,#30839,#30840);
#27614=AXIS2_PLACEMENT_3D('',#46804,#30842,#30843);
#27615=AXIS2_PLACEMENT_3D('',#46990,#30845,#30846);
#27616=AXIS2_PLACEMENT_3D('',#47176,#30848,#30849);
#27617=AXIS2_PLACEMENT_3D('',#47524,#30851,#30852);
#27618=AXIS2_PLACEMENT_3D('',#47710,#30854,#30855);
#27619=AXIS2_PLACEMENT_3D('',#48058,#30857,#30858);
#27620=AXIS2_PLACEMENT_3D('',#48406,#30860,#30861);
#27621=AXIS2_PLACEMENT_3D('',#48569,#30862,#30863);
#27622=AXIS2_PLACEMENT_3D('',#48578,#30864,#30865);
#27623=AXIS2_PLACEMENT_3D('',#48664,#30866,#30867);
#27624=AXIS2_PLACEMENT_3D('',#48755,#30868,#30869);
#27625=AXIS2_PLACEMENT_3D('',#48758,#30870,#30871);
#27626=AXIS2_PLACEMENT_3D('',#48923,#30872,#30873);
#27627=AXIS2_PLACEMENT_3D('',#49310,#30874,#30875);
#27628=AXIS2_PLACEMENT_3D('',#49313,#30876,#30877);
#27629=AXIS2_PLACEMENT_3D('',#49396,#30878,#30879);
#27630=AXIS2_PLACEMENT_3D('',#49701,#30880,#30881);
#27631=AXIS2_PLACEMENT_3D('',#49703,#30882,#30883);
#27632=AXIS2_PLACEMENT_3D('',#49704,#30884,#30885);
#27633=AXIS2_PLACEMENT_3D('',#49705,#30886,#30887);
#27634=AXIS2_PLACEMENT_3D('',#49707,#30888,#30889);
#27635=AXIS2_PLACEMENT_3D('',#49708,#30890,#30891);
#27636=AXIS2_PLACEMENT_3D('',#49711,#30893,#30894);
#27637=AXIS2_PLACEMENT_3D('',#49712,#30895,#30896);
#27638=AXIS2_PLACEMENT_3D('',#49713,#30897,#30898);
#27639=AXIS2_PLACEMENT_3D('',#49724,#30902,#30903);
#27640=AXIS2_PLACEMENT_3D('',#49726,#30904,#30905);
#27641=AXIS2_PLACEMENT_3D('',#49728,#30907,#30908);
#27642=AXIS2_PLACEMENT_3D('',#49734,#30910,#30911);
#27643=AXIS2_PLACEMENT_3D('',#49737,#30912,#30913);
#27644=AXIS2_PLACEMENT_3D('',#49741,#30915,#30916);
#27645=AXIS2_PLACEMENT_3D('',#49742,#30917,#30918);
#27646=AXIS2_PLACEMENT_3D('',#49744,#30919,#30920);
#27647=AXIS2_PLACEMENT_3D('',#49748,#30922,#30923);
#27648=AXIS2_PLACEMENT_3D('',#49752,#30925,#30926);
#27649=AXIS2_PLACEMENT_3D('',#49756,#30928,#30929);
#27650=AXIS2_PLACEMENT_3D('',#49760,#30931,#30932);
#27651=AXIS2_PLACEMENT_3D('',#49764,#30934,#30935);
#27652=AXIS2_PLACEMENT_3D('',#49768,#30937,#30938);
#27653=AXIS2_PLACEMENT_3D('',#49772,#30940,#30941);
#27654=AXIS2_PLACEMENT_3D('',#49776,#30943,#30944);
#27655=AXIS2_PLACEMENT_3D('',#49780,#30946,#30947);
#27656=AXIS2_PLACEMENT_3D('',#49784,#30949,#30950);
#27657=AXIS2_PLACEMENT_3D('',#49788,#30952,#30953);
#27658=AXIS2_PLACEMENT_3D('',#49792,#30955,#30956);
#27659=AXIS2_PLACEMENT_3D('',#49796,#30958,#30959);
#27660=AXIS2_PLACEMENT_3D('',#49800,#30961,#30962);
#27661=AXIS2_PLACEMENT_3D('',#49804,#30964,#30965);
#27662=AXIS2_PLACEMENT_3D('',#49808,#30967,#30968);
#27663=AXIS2_PLACEMENT_3D('',#49812,#30970,#30971);
#27664=AXIS2_PLACEMENT_3D('',#49816,#30973,#30974);
#27665=AXIS2_PLACEMENT_3D('',#49820,#30976,#30977);
#27666=AXIS2_PLACEMENT_3D('',#49824,#30979,#30980);
#27667=AXIS2_PLACEMENT_3D('',#49828,#30982,#30983);
#27668=AXIS2_PLACEMENT_3D('',#49832,#30985,#30986);
#27669=AXIS2_PLACEMENT_3D('',#49836,#30988,#30989);
#27670=AXIS2_PLACEMENT_3D('',#49840,#30991,#30992);
#27671=AXIS2_PLACEMENT_3D('',#49844,#30994,#30995);
#27672=AXIS2_PLACEMENT_3D('',#49848,#30997,#30998);
#27673=AXIS2_PLACEMENT_3D('',#49852,#31000,#31001);
#27674=AXIS2_PLACEMENT_3D('',#49856,#31003,#31004);
#27675=AXIS2_PLACEMENT_3D('',#49860,#31006,#31007);
#27676=AXIS2_PLACEMENT_3D('',#49864,#31009,#31010);
#27677=AXIS2_PLACEMENT_3D('',#49868,#31012,#31013);
#27678=AXIS2_PLACEMENT_3D('',#49872,#31015,#31016);
#27679=AXIS2_PLACEMENT_3D('',#49875,#31018,#31019);
#27680=AXIS2_PLACEMENT_3D('',#49877,#31020,#31021);
#27681=AXIS2_PLACEMENT_3D('',#49881,#31023,#31024);
#27682=AXIS2_PLACEMENT_3D('',#49885,#31026,#31027);
#27683=AXIS2_PLACEMENT_3D('',#49889,#31029,#31030);
#27684=AXIS2_PLACEMENT_3D('',#49893,#31032,#31033);
#27685=AXIS2_PLACEMENT_3D('',#49897,#31035,#31036);
#27686=AXIS2_PLACEMENT_3D('',#49901,#31038,#31039);
#27687=AXIS2_PLACEMENT_3D('',#49905,#31041,#31042);
#27688=AXIS2_PLACEMENT_3D('',#49909,#31044,#31045);
#27689=AXIS2_PLACEMENT_3D('',#49913,#31047,#31048);
#27690=AXIS2_PLACEMENT_3D('',#49917,#31050,#31051);
#27691=AXIS2_PLACEMENT_3D('',#49921,#31053,#31054);
#27692=AXIS2_PLACEMENT_3D('',#49925,#31056,#31057);
#27693=AXIS2_PLACEMENT_3D('',#49929,#31059,#31060);
#27694=AXIS2_PLACEMENT_3D('',#49933,#31062,#31063);
#27695=AXIS2_PLACEMENT_3D('',#49937,#31065,#31066);
#27696=AXIS2_PLACEMENT_3D('',#49941,#31068,#31069);
#27697=AXIS2_PLACEMENT_3D('',#49945,#31071,#31072);
#27698=AXIS2_PLACEMENT_3D('',#49949,#31074,#31075);
#27699=AXIS2_PLACEMENT_3D('',#49953,#31077,#31078);
#27700=AXIS2_PLACEMENT_3D('',#49957,#31080,#31081);
#27701=AXIS2_PLACEMENT_3D('',#49961,#31083,#31084);
#27702=AXIS2_PLACEMENT_3D('',#49965,#31086,#31087);
#27703=AXIS2_PLACEMENT_3D('',#49969,#31089,#31090);
#27704=AXIS2_PLACEMENT_3D('',#49973,#31092,#31093);
#27705=AXIS2_PLACEMENT_3D('',#49977,#31095,#31096);
#27706=AXIS2_PLACEMENT_3D('',#49981,#31098,#31099);
#27707=AXIS2_PLACEMENT_3D('',#49985,#31101,#31102);
#27708=AXIS2_PLACEMENT_3D('',#49989,#31104,#31105);
#27709=AXIS2_PLACEMENT_3D('',#49993,#31107,#31108);
#27710=AXIS2_PLACEMENT_3D('',#49997,#31110,#31111);
#27711=AXIS2_PLACEMENT_3D('',#50001,#31113,#31114);
#27712=AXIS2_PLACEMENT_3D('',#50005,#31116,#31117);
#27713=AXIS2_PLACEMENT_3D('',#50009,#31119,#31120);
#27714=AXIS2_PLACEMENT_3D('',#50013,#31122,#31123);
#27715=AXIS2_PLACEMENT_3D('',#50017,#31125,#31126);
#27716=AXIS2_PLACEMENT_3D('',#50021,#31128,#31129);
#27717=AXIS2_PLACEMENT_3D('',#50023,#31131,#31132);
#27718=AXIS2_PLACEMENT_3D('',#50031,#31135,#31136);
#27719=AXIS2_PLACEMENT_3D('',#50033,#31138,#31139);
#27720=AXIS2_PLACEMENT_3D('',#50037,#31140,#31141);
#27721=AXIS2_PLACEMENT_3D('',#50045,#31144,#31145);
#27722=AXIS2_PLACEMENT_3D('',#50047,#31147,#31148);
#27723=AXIS2_PLACEMENT_3D('',#50051,#31149,#31150);
#27724=AXIS2_PLACEMENT_3D('',#50059,#31153,#31154);
#27725=AXIS2_PLACEMENT_3D('',#50061,#31156,#31157);
#27726=AXIS2_PLACEMENT_3D('',#50065,#31158,#31159);
#27727=AXIS2_PLACEMENT_3D('',#50073,#31162,#31163);
#27728=AXIS2_PLACEMENT_3D('',#50075,#31165,#31166);
#27729=AXIS2_PLACEMENT_3D('',#50079,#31167,#31168);
#27730=AXIS2_PLACEMENT_3D('',#50087,#31171,#31172);
#27731=AXIS2_PLACEMENT_3D('',#50089,#31174,#31175);
#27732=AXIS2_PLACEMENT_3D('',#50093,#31176,#31177);
#27733=AXIS2_PLACEMENT_3D('',#50101,#31180,#31181);
#27734=AXIS2_PLACEMENT_3D('',#50103,#31183,#31184);
#27735=AXIS2_PLACEMENT_3D('',#50107,#31185,#31186);
#27736=AXIS2_PLACEMENT_3D('',#50115,#31189,#31190);
#27737=AXIS2_PLACEMENT_3D('',#50117,#31192,#31193);
#27738=AXIS2_PLACEMENT_3D('',#50121,#31194,#31195);
#27739=AXIS2_PLACEMENT_3D('',#50129,#31198,#31199);
#27740=AXIS2_PLACEMENT_3D('',#50131,#31201,#31202);
#27741=AXIS2_PLACEMENT_3D('',#50135,#31203,#31204);
#27742=AXIS2_PLACEMENT_3D('',#50143,#31207,#31208);
#27743=AXIS2_PLACEMENT_3D('',#50145,#31210,#31211);
#27744=AXIS2_PLACEMENT_3D('',#50149,#31212,#31213);
#27745=AXIS2_PLACEMENT_3D('',#50157,#31216,#31217);
#27746=AXIS2_PLACEMENT_3D('',#50159,#31219,#31220);
#27747=AXIS2_PLACEMENT_3D('',#50163,#31221,#31222);
#27748=AXIS2_PLACEMENT_3D('',#50171,#31225,#31226);
#27749=AXIS2_PLACEMENT_3D('',#50173,#31228,#31229);
#27750=AXIS2_PLACEMENT_3D('',#50177,#31230,#31231);
#27751=AXIS2_PLACEMENT_3D('',#50185,#31234,#31235);
#27752=AXIS2_PLACEMENT_3D('',#50187,#31237,#31238);
#27753=AXIS2_PLACEMENT_3D('',#50191,#31239,#31240);
#27754=AXIS2_PLACEMENT_3D('',#50199,#31243,#31244);
#27755=AXIS2_PLACEMENT_3D('',#50201,#31246,#31247);
#27756=AXIS2_PLACEMENT_3D('',#50205,#31248,#31249);
#27757=AXIS2_PLACEMENT_3D('',#50213,#31252,#31253);
#27758=AXIS2_PLACEMENT_3D('',#50215,#31255,#31256);
#27759=AXIS2_PLACEMENT_3D('',#50219,#31257,#31258);
#27760=AXIS2_PLACEMENT_3D('',#50227,#31261,#31262);
#27761=AXIS2_PLACEMENT_3D('',#50229,#31264,#31265);
#27762=AXIS2_PLACEMENT_3D('',#50233,#31266,#31267);
#27763=AXIS2_PLACEMENT_3D('',#50241,#31270,#31271);
#27764=AXIS2_PLACEMENT_3D('',#50243,#31273,#31274);
#27765=AXIS2_PLACEMENT_3D('',#50247,#31275,#31276);
#27766=AXIS2_PLACEMENT_3D('',#50255,#31279,#31280);
#27767=AXIS2_PLACEMENT_3D('',#50257,#31282,#31283);
#27768=AXIS2_PLACEMENT_3D('',#50261,#31284,#31285);
#27769=AXIS2_PLACEMENT_3D('',#50269,#31288,#31289);
#27770=AXIS2_PLACEMENT_3D('',#50271,#31291,#31292);
#27771=AXIS2_PLACEMENT_3D('',#50275,#31293,#31294);
#27772=AXIS2_PLACEMENT_3D('',#50283,#31297,#31298);
#27773=AXIS2_PLACEMENT_3D('',#50285,#31300,#31301);
#27774=AXIS2_PLACEMENT_3D('',#50289,#31302,#31303);
#27775=AXIS2_PLACEMENT_3D('',#50297,#31306,#31307);
#27776=AXIS2_PLACEMENT_3D('',#50299,#31309,#31310);
#27777=AXIS2_PLACEMENT_3D('',#50303,#31311,#31312);
#27778=AXIS2_PLACEMENT_3D('',#50311,#31315,#31316);
#27779=AXIS2_PLACEMENT_3D('',#50313,#31318,#31319);
#27780=AXIS2_PLACEMENT_3D('',#50317,#31320,#31321);
#27781=AXIS2_PLACEMENT_3D('',#50325,#31324,#31325);
#27782=AXIS2_PLACEMENT_3D('',#50327,#31327,#31328);
#27783=AXIS2_PLACEMENT_3D('',#50331,#31329,#31330);
#27784=AXIS2_PLACEMENT_3D('',#50339,#31333,#31334);
#27785=AXIS2_PLACEMENT_3D('',#50341,#31336,#31337);
#27786=AXIS2_PLACEMENT_3D('',#50345,#31338,#31339);
#27787=AXIS2_PLACEMENT_3D('',#50353,#31342,#31343);
#27788=AXIS2_PLACEMENT_3D('',#50355,#31345,#31346);
#27789=AXIS2_PLACEMENT_3D('',#50359,#31347,#31348);
#27790=AXIS2_PLACEMENT_3D('',#50367,#31351,#31352);
#27791=AXIS2_PLACEMENT_3D('',#50369,#31354,#31355);
#27792=AXIS2_PLACEMENT_3D('',#50373,#31356,#31357);
#27793=AXIS2_PLACEMENT_3D('',#50381,#31360,#31361);
#27794=AXIS2_PLACEMENT_3D('',#50383,#31363,#31364);
#27795=AXIS2_PLACEMENT_3D('',#50387,#31365,#31366);
#27796=AXIS2_PLACEMENT_3D('',#50395,#31369,#31370);
#27797=AXIS2_PLACEMENT_3D('',#50397,#31372,#31373);
#27798=AXIS2_PLACEMENT_3D('',#50401,#31374,#31375);
#27799=AXIS2_PLACEMENT_3D('',#50409,#31378,#31379);
#27800=AXIS2_PLACEMENT_3D('',#50411,#31381,#31382);
#27801=AXIS2_PLACEMENT_3D('',#50415,#31383,#31384);
#27802=AXIS2_PLACEMENT_3D('',#50423,#31387,#31388);
#27803=AXIS2_PLACEMENT_3D('',#50425,#31390,#31391);
#27804=AXIS2_PLACEMENT_3D('',#50429,#31392,#31393);
#27805=AXIS2_PLACEMENT_3D('',#50437,#31396,#31397);
#27806=AXIS2_PLACEMENT_3D('',#50439,#31399,#31400);
#27807=AXIS2_PLACEMENT_3D('',#50443,#31401,#31402);
#27808=AXIS2_PLACEMENT_3D('',#50451,#31405,#31406);
#27809=AXIS2_PLACEMENT_3D('',#50453,#31408,#31409);
#27810=AXIS2_PLACEMENT_3D('',#50457,#31410,#31411);
#27811=AXIS2_PLACEMENT_3D('',#50465,#31414,#31415);
#27812=AXIS2_PLACEMENT_3D('',#50467,#31417,#31418);
#27813=AXIS2_PLACEMENT_3D('',#50471,#31419,#31420);
#27814=AXIS2_PLACEMENT_3D('',#50479,#31423,#31424);
#27815=AXIS2_PLACEMENT_3D('',#50481,#31426,#31427);
#27816=AXIS2_PLACEMENT_3D('',#50485,#31428,#31429);
#27817=AXIS2_PLACEMENT_3D('',#50493,#31432,#31433);
#27818=AXIS2_PLACEMENT_3D('',#50495,#31435,#31436);
#27819=AXIS2_PLACEMENT_3D('',#50499,#31437,#31438);
#27820=AXIS2_PLACEMENT_3D('',#50507,#31441,#31442);
#27821=AXIS2_PLACEMENT_3D('',#50509,#31444,#31445);
#27822=AXIS2_PLACEMENT_3D('',#50513,#31446,#31447);
#27823=AXIS2_PLACEMENT_3D('',#50514,#31448,#31449);
#27824=AXIS2_PLACEMENT_3D('',#50515,#31450,#31451);
#27825=AXIS2_PLACEMENT_3D('',#50518,#31453,#31454);
#27826=AXIS2_PLACEMENT_3D('',#50519,#31455,#31456);
#27827=AXIS2_PLACEMENT_3D('',#50521,#31457,#31458);
#27828=AXIS2_PLACEMENT_3D('',#50522,#31459,#31460);
#27829=AXIS2_PLACEMENT_3D('',#50529,#31461,#31462);
#27830=AXIS2_PLACEMENT_3D('',#50539,#31463,#31464);
#27831=AXIS2_PLACEMENT_3D('',#50549,#31465,#31466);
#27832=AXIS2_PLACEMENT_3D('',#50559,#31467,#31468);
#27833=AXIS2_PLACEMENT_3D('',#50569,#31469,#31470);
#27834=AXIS2_PLACEMENT_3D('',#50579,#31471,#31472);
#27835=AXIS2_PLACEMENT_3D('',#50584,#31474,#31475);
#27836=AXIS2_PLACEMENT_3D('',#50589,#31478,#31479);
#27837=AXIS2_PLACEMENT_3D('',#50590,#31480,#31481);
#27838=AXIS2_PLACEMENT_3D('',#50595,#31484,#31485);
#27839=AXIS2_PLACEMENT_3D('',#50596,#31486,#31487);
#27840=AXIS2_PLACEMENT_3D('',#50600,#31489,#31490);
#27841=AXIS2_PLACEMENT_3D('',#50602,#31492,#31493);
#27842=AXIS2_PLACEMENT_3D('',#50607,#31496,#31497);
#27843=AXIS2_PLACEMENT_3D('',#50608,#31498,#31499);
#27844=AXIS2_PLACEMENT_3D('',#50612,#31501,#31502);
#27845=AXIS2_PLACEMENT_3D('',#50614,#31504,#31505);
#27846=AXIS2_PLACEMENT_3D('',#50618,#31507,#31508);
#27847=AXIS2_PLACEMENT_3D('',#50620,#31510,#31511);
#27848=AXIS2_PLACEMENT_3D('',#50627,#31516,#31517);
#27849=AXIS2_PLACEMENT_3D('',#50632,#31521,#31522);
#27850=AXIS2_PLACEMENT_3D('',#50637,#31526,#31527);
#27851=AXIS2_PLACEMENT_3D('',#50638,#31528,#31529);
#27852=AXIS2_PLACEMENT_3D('',#50639,#31530,#31531);
#27853=AXIS2_PLACEMENT_3D('',#50641,#31533,#31534);
#27854=AXIS2_PLACEMENT_3D('',#50642,#31535,#31536);
#27855=AXIS2_PLACEMENT_3D('',#50644,#31538,#31539);
#27856=AXIS2_PLACEMENT_3D('',#50646,#31541,#31542);
#27857=AXIS2_PLACEMENT_3D('',#50649,#31544,#31545);
#27858=AXIS2_PLACEMENT_3D('',#50650,#31546,#31547);
#27859=AXIS2_PLACEMENT_3D('',#50651,#31548,#31549);
#27860=AXIS2_PLACEMENT_3D('',#50652,#31550,#31551);
#27861=AXIS2_PLACEMENT_3D('',#50653,#31552,#31553);
#27862=AXIS2_PLACEMENT_3D('',#50654,#31554,#31555);
#27863=AXIS2_PLACEMENT_3D('',#50655,#31556,#31557);
#27864=AXIS2_PLACEMENT_3D('',#50656,#31558,#31559);
#27865=AXIS2_PLACEMENT_3D('',#50659,#31561,#31562);
#27866=AXIS2_PLACEMENT_3D('',#50660,#31563,#31564);
#27867=AXIS2_PLACEMENT_3D('',#50662,#31566,#31567);
#27868=AXIS2_PLACEMENT_3D('',#50663,#31568,#31569);
#27869=AXIS2_PLACEMENT_3D('',#50666,#31571,#31572);
#27870=AXIS2_PLACEMENT_3D('',#50668,#31574,#31575);
#27871=AXIS2_PLACEMENT_3D('',#50670,#31577,#31578);
#27872=AXIS2_PLACEMENT_3D('',#50671,#31579,#31580);
#27873=AXIS2_PLACEMENT_3D('',#50672,#31581,#31582);
#27874=AXIS2_PLACEMENT_3D('',#50674,#31583,#31584);
#27875=AXIS2_PLACEMENT_3D('',#50677,#31586,#31587);
#27876=AXIS2_PLACEMENT_3D('',#50678,#31588,#31589);
#27877=AXIS2_PLACEMENT_3D('',#50683,#31591,#31592);
#27878=AXIS2_PLACEMENT_3D('',#50686,#31594,#31595);
#27879=AXIS2_PLACEMENT_3D('',#50688,#31596,#31597);
#27880=AXIS2_PLACEMENT_3D('',#50690,#31598,#31599);
#27881=AXIS2_PLACEMENT_3D('',#50692,#31600,#31601);
#27882=AXIS2_PLACEMENT_3D('',#50694,#31602,#31603);
#27883=AXIS2_PLACEMENT_3D('',#50696,#31604,#31605);
#27884=AXIS2_PLACEMENT_3D('',#50698,#31606,#31607);
#27885=AXIS2_PLACEMENT_3D('',#50700,#31608,#31609);
#27886=AXIS2_PLACEMENT_3D('',#50702,#31610,#31611);
#27887=AXIS2_PLACEMENT_3D('',#50704,#31612,#31613);
#27888=AXIS2_PLACEMENT_3D('',#50706,#31614,#31615);
#27889=AXIS2_PLACEMENT_3D('',#50708,#31616,#31617);
#27890=AXIS2_PLACEMENT_3D('',#50710,#31618,#31619);
#27891=AXIS2_PLACEMENT_3D('',#50712,#31620,#31621);
#27892=AXIS2_PLACEMENT_3D('',#50714,#31622,#31623);
#27893=AXIS2_PLACEMENT_3D('',#50716,#31624,#31625);
#27894=AXIS2_PLACEMENT_3D('',#50718,#31626,#31627);
#27895=AXIS2_PLACEMENT_3D('',#50720,#31628,#31629);
#27896=AXIS2_PLACEMENT_3D('',#50722,#31630,#31631);
#27897=AXIS2_PLACEMENT_3D('',#50724,#31632,#31633);
#27898=AXIS2_PLACEMENT_3D('',#50726,#31634,#31635);
#27899=AXIS2_PLACEMENT_3D('',#50727,#31636,#31637);
#27900=AXIS2_PLACEMENT_3D('',#50730,#31639,#31640);
#27901=AXIS2_PLACEMENT_3D('',#50731,#31641,#31642);
#27902=AXIS2_PLACEMENT_3D('',#50733,#31643,#31644);
#27903=AXIS2_PLACEMENT_3D('',#50735,#31646,#31647);
#27904=AXIS2_PLACEMENT_3D('',#50738,#31649,#31650);
#27905=AXIS2_PLACEMENT_3D('',#50739,#31651,#31652);
#27906=AXIS2_PLACEMENT_3D('',#50741,#31653,#31654);
#27907=AXIS2_PLACEMENT_3D('',#50743,#31656,#31657);
#27908=AXIS2_PLACEMENT_3D('',#50746,#31659,#31660);
#27909=AXIS2_PLACEMENT_3D('',#50747,#31661,#31662);
#27910=AXIS2_PLACEMENT_3D('',#50749,#31663,#31664);
#27911=AXIS2_PLACEMENT_3D('',#50751,#31666,#31667);
#27912=AXIS2_PLACEMENT_3D('',#50754,#31669,#31670);
#27913=AXIS2_PLACEMENT_3D('',#50755,#31671,#31672);
#27914=AXIS2_PLACEMENT_3D('',#50757,#31673,#31674);
#27915=AXIS2_PLACEMENT_3D('',#50759,#31676,#31677);
#27916=AXIS2_PLACEMENT_3D('',#50762,#31679,#31680);
#27917=AXIS2_PLACEMENT_3D('',#50763,#31681,#31682);
#27918=AXIS2_PLACEMENT_3D('',#50765,#31683,#31684);
#27919=AXIS2_PLACEMENT_3D('',#50767,#31686,#31687);
#27920=AXIS2_PLACEMENT_3D('',#50770,#31689,#31690);
#27921=AXIS2_PLACEMENT_3D('',#50771,#31691,#31692);
#27922=AXIS2_PLACEMENT_3D('',#50773,#31693,#31694);
#27923=AXIS2_PLACEMENT_3D('',#50775,#31696,#31697);
#27924=AXIS2_PLACEMENT_3D('',#50778,#31699,#31700);
#27925=AXIS2_PLACEMENT_3D('',#50779,#31701,#31702);
#27926=AXIS2_PLACEMENT_3D('',#50781,#31703,#31704);
#27927=AXIS2_PLACEMENT_3D('',#50783,#31706,#31707);
#27928=AXIS2_PLACEMENT_3D('',#50786,#31709,#31710);
#27929=AXIS2_PLACEMENT_3D('',#50787,#31711,#31712);
#27930=AXIS2_PLACEMENT_3D('',#50789,#31713,#31714);
#27931=AXIS2_PLACEMENT_3D('',#50791,#31716,#31717);
#27932=AXIS2_PLACEMENT_3D('',#50794,#31719,#31720);
#27933=AXIS2_PLACEMENT_3D('',#50795,#31721,#31722);
#27934=AXIS2_PLACEMENT_3D('',#50797,#31723,#31724);
#27935=AXIS2_PLACEMENT_3D('',#50799,#31726,#31727);
#27936=AXIS2_PLACEMENT_3D('',#50802,#31729,#31730);
#27937=AXIS2_PLACEMENT_3D('',#50803,#31731,#31732);
#27938=AXIS2_PLACEMENT_3D('',#50805,#31733,#31734);
#27939=AXIS2_PLACEMENT_3D('',#50807,#31736,#31737);
#27940=AXIS2_PLACEMENT_3D('',#50810,#31739,#31740);
#27941=AXIS2_PLACEMENT_3D('',#50811,#31741,#31742);
#27942=AXIS2_PLACEMENT_3D('',#50813,#31743,#31744);
#27943=AXIS2_PLACEMENT_3D('',#50815,#31746,#31747);
#27944=AXIS2_PLACEMENT_3D('',#50818,#31749,#31750);
#27945=AXIS2_PLACEMENT_3D('',#50819,#31751,#31752);
#27946=AXIS2_PLACEMENT_3D('',#50821,#31753,#31754);
#27947=AXIS2_PLACEMENT_3D('',#50823,#31756,#31757);
#27948=AXIS2_PLACEMENT_3D('',#50826,#31759,#31760);
#27949=AXIS2_PLACEMENT_3D('',#50827,#31761,#31762);
#27950=AXIS2_PLACEMENT_3D('',#50829,#31763,#31764);
#27951=AXIS2_PLACEMENT_3D('',#50831,#31766,#31767);
#27952=AXIS2_PLACEMENT_3D('',#50834,#31769,#31770);
#27953=AXIS2_PLACEMENT_3D('',#50835,#31771,#31772);
#27954=AXIS2_PLACEMENT_3D('',#50837,#31773,#31774);
#27955=AXIS2_PLACEMENT_3D('',#50839,#31776,#31777);
#27956=AXIS2_PLACEMENT_3D('',#50842,#31779,#31780);
#27957=AXIS2_PLACEMENT_3D('',#50843,#31781,#31782);
#27958=AXIS2_PLACEMENT_3D('',#50845,#31783,#31784);
#27959=AXIS2_PLACEMENT_3D('',#50847,#31786,#31787);
#27960=AXIS2_PLACEMENT_3D('',#50850,#31789,#31790);
#27961=AXIS2_PLACEMENT_3D('',#50851,#31791,#31792);
#27962=AXIS2_PLACEMENT_3D('',#50853,#31793,#31794);
#27963=AXIS2_PLACEMENT_3D('',#50855,#31796,#31797);
#27964=AXIS2_PLACEMENT_3D('',#50858,#31799,#31800);
#27965=AXIS2_PLACEMENT_3D('',#50859,#31801,#31802);
#27966=AXIS2_PLACEMENT_3D('',#50861,#31803,#31804);
#27967=AXIS2_PLACEMENT_3D('',#50863,#31806,#31807);
#27968=AXIS2_PLACEMENT_3D('',#50866,#31809,#31810);
#27969=AXIS2_PLACEMENT_3D('',#50867,#31811,#31812);
#27970=AXIS2_PLACEMENT_3D('',#50869,#31813,#31814);
#27971=AXIS2_PLACEMENT_3D('',#50871,#31816,#31817);
#27972=AXIS2_PLACEMENT_3D('',#50874,#31819,#31820);
#27973=AXIS2_PLACEMENT_3D('',#50875,#31821,#31822);
#27974=AXIS2_PLACEMENT_3D('',#50877,#31823,#31824);
#27975=AXIS2_PLACEMENT_3D('',#50879,#31826,#31827);
#27976=AXIS2_PLACEMENT_3D('',#50882,#31829,#31830);
#27977=AXIS2_PLACEMENT_3D('',#50883,#31831,#31832);
#27978=AXIS2_PLACEMENT_3D('',#50885,#31833,#31834);
#27979=AXIS2_PLACEMENT_3D('',#50887,#31836,#31837);
#27980=AXIS2_PLACEMENT_3D('',#50890,#31839,#31840);
#27981=AXIS2_PLACEMENT_3D('',#50891,#31841,#31842);
#27982=AXIS2_PLACEMENT_3D('',#50897,#31846,#31847);
#27983=AXIS2_PLACEMENT_3D('',#50900,#31849,#31850);
#27984=AXIS2_PLACEMENT_3D('',#50901,#31851,#31852);
#27985=AXIS2_PLACEMENT_3D('',#50905,#31855,#31856);
#27986=AXIS2_PLACEMENT_3D('',#50906,#31857,#31858);
#27987=AXIS2_PLACEMENT_3D('',#50907,#31859,#31860);
#27988=AXIS2_PLACEMENT_3D('',#50911,#31862,#31863);
#27989=AXIS2_PLACEMENT_3D('',#50913,#31865,#31866);
#27990=AXIS2_PLACEMENT_3D('',#50917,#31869,#31870);
#27991=AXIS2_PLACEMENT_3D('',#50923,#31874,#31875);
#27992=AXIS2_PLACEMENT_3D('',#50925,#31876,#31877);
#27993=AXIS2_PLACEMENT_3D('',#50928,#31879,#31880);
#27994=AXIS2_PLACEMENT_3D('',#50929,#31881,#31882);
#27995=AXIS2_PLACEMENT_3D('',#50934,#31886,#31887);
#27996=AXIS2_PLACEMENT_3D('',#50935,#31888,#31889);
#27997=AXIS2_PLACEMENT_3D('',#50936,#31890,#31891);
#27998=AXIS2_PLACEMENT_3D('',#50938,#31893,#31894);
#27999=AXIS2_PLACEMENT_3D('',#50939,#31895,#31896);
#28000=AXIS2_PLACEMENT_3D('',#50940,#31897,#31898);
#28001=AXIS2_PLACEMENT_3D('',#50941,#31899,#31900);
#28002=AXIS2_PLACEMENT_3D('',#50950,#31905,#31906);
#28003=AXIS2_PLACEMENT_3D('',#50954,#31908,#31909);
#28004=AXIS2_PLACEMENT_3D('',#50955,#31910,#31911);
#28005=AXIS2_PLACEMENT_3D('',#50956,#31912,#31913);
#28006=AXIS2_PLACEMENT_3D('',#50962,#31917,#31918);
#28007=AXIS2_PLACEMENT_3D('',#50966,#31920,#31921);
#28008=AXIS2_PLACEMENT_3D('',#50967,#31922,#31923);
#28009=AXIS2_PLACEMENT_3D('',#50968,#31924,#31925);
#28010=AXIS2_PLACEMENT_3D('',#50974,#31929,#31930);
#28011=AXIS2_PLACEMENT_3D('',#50980,#31934,#31935);
#28012=AXIS2_PLACEMENT_3D('',#50983,#31937,#31938);
#28013=AXIS2_PLACEMENT_3D('',#50984,#31939,#31940);
#28014=AXIS2_PLACEMENT_3D('',#50988,#31943,#31944);
#28015=AXIS2_PLACEMENT_3D('',#50991,#31946,#31947);
#28016=AXIS2_PLACEMENT_3D('',#50992,#31948,#31949);
#28017=AXIS2_PLACEMENT_3D('',#50996,#31952,#31953);
#28018=AXIS2_PLACEMENT_3D('',#51002,#31957,#31958);
#28019=AXIS2_PLACEMENT_3D('',#51005,#31960,#31961);
#28020=AXIS2_PLACEMENT_3D('',#51006,#31962,#31963);
#28021=AXIS2_PLACEMENT_3D('',#51010,#31966,#31967);
#28022=AXIS2_PLACEMENT_3D('',#51013,#31969,#31970);
#28023=AXIS2_PLACEMENT_3D('',#51014,#31971,#31972);
#28024=AXIS2_PLACEMENT_3D('',#51018,#31975,#31976);
#28025=AXIS2_PLACEMENT_3D('',#51020,#31977,#31978);
#28026=AXIS2_PLACEMENT_3D('',#51023,#31980,#31981);
#28027=AXIS2_PLACEMENT_3D('',#51024,#31982,#31983);
#28028=AXIS2_PLACEMENT_3D('',#51026,#31984,#31985);
#28029=AXIS2_PLACEMENT_3D('',#51029,#31987,#31988);
#28030=AXIS2_PLACEMENT_3D('',#51030,#31989,#31990);
#28031=AXIS2_PLACEMENT_3D('',#51032,#31991,#31992);
#28032=AXIS2_PLACEMENT_3D('',#51035,#31994,#31995);
#28033=AXIS2_PLACEMENT_3D('',#51036,#31996,#31997);
#28034=AXIS2_PLACEMENT_3D('',#51038,#31998,#31999);
#28035=AXIS2_PLACEMENT_3D('',#51041,#32001,#32002);
#28036=AXIS2_PLACEMENT_3D('',#51042,#32003,#32004);
#28037=AXIS2_PLACEMENT_3D('',#51044,#32005,#32006);
#28038=AXIS2_PLACEMENT_3D('',#51047,#32008,#32009);
#28039=AXIS2_PLACEMENT_3D('',#51048,#32010,#32011);
#28040=AXIS2_PLACEMENT_3D('',#51050,#32012,#32013);
#28041=AXIS2_PLACEMENT_3D('',#51053,#32015,#32016);
#28042=AXIS2_PLACEMENT_3D('',#51054,#32017,#32018);
#28043=AXIS2_PLACEMENT_3D('',#51056,#32019,#32020);
#28044=AXIS2_PLACEMENT_3D('',#51059,#32022,#32023);
#28045=AXIS2_PLACEMENT_3D('',#51060,#32024,#32025);
#28046=AXIS2_PLACEMENT_3D('',#51062,#32026,#32027);
#28047=AXIS2_PLACEMENT_3D('',#51065,#32029,#32030);
#28048=AXIS2_PLACEMENT_3D('',#51066,#32031,#32032);
#28049=AXIS2_PLACEMENT_3D('',#51068,#32033,#32034);
#28050=AXIS2_PLACEMENT_3D('',#51071,#32036,#32037);
#28051=AXIS2_PLACEMENT_3D('',#51072,#32038,#32039);
#28052=AXIS2_PLACEMENT_3D('',#51074,#32040,#32041);
#28053=AXIS2_PLACEMENT_3D('',#51077,#32043,#32044);
#28054=AXIS2_PLACEMENT_3D('',#51078,#32045,#32046);
#28055=AXIS2_PLACEMENT_3D('',#51084,#32050,#32051);
#28056=AXIS2_PLACEMENT_3D('',#51090,#32055,#32056);
#28057=AXIS2_PLACEMENT_3D('',#51096,#32060,#32061);
#28058=AXIS2_PLACEMENT_3D('',#51102,#32065,#32066);
#28059=AXIS2_PLACEMENT_3D('',#51108,#32070,#32071);
#28060=AXIS2_PLACEMENT_3D('',#51114,#32075,#32076);
#28061=AXIS2_PLACEMENT_3D('',#51120,#32080,#32081);
#28062=AXIS2_PLACEMENT_3D('',#51126,#32085,#32086);
#28063=AXIS2_PLACEMENT_3D('',#51132,#32090,#32091);
#28064=AXIS2_PLACEMENT_3D('',#51138,#32095,#32096);
#28065=AXIS2_PLACEMENT_3D('',#51144,#32100,#32101);
#28066=AXIS2_PLACEMENT_3D('',#51150,#32105,#32106);
#28067=AXIS2_PLACEMENT_3D('',#51156,#32110,#32111);
#28068=AXIS2_PLACEMENT_3D('',#51162,#32115,#32116);
#28069=AXIS2_PLACEMENT_3D('',#51168,#32120,#32121);
#28070=AXIS2_PLACEMENT_3D('',#51174,#32125,#32126);
#28071=AXIS2_PLACEMENT_3D('',#51180,#32130,#32131);
#28072=AXIS2_PLACEMENT_3D('',#51186,#32135,#32136);
#28073=AXIS2_PLACEMENT_3D('',#51192,#32140,#32141);
#28074=AXIS2_PLACEMENT_3D('',#51198,#32145,#32146);
#28075=AXIS2_PLACEMENT_3D('',#51204,#32150,#32151);
#28076=AXIS2_PLACEMENT_3D('',#51210,#32155,#32156);
#28077=AXIS2_PLACEMENT_3D('',#51216,#32160,#32161);
#28078=AXIS2_PLACEMENT_3D('',#51222,#32165,#32166);
#28079=AXIS2_PLACEMENT_3D('',#51228,#32170,#32171);
#28080=AXIS2_PLACEMENT_3D('',#51234,#32175,#32176);
#28081=AXIS2_PLACEMENT_3D('',#51240,#32180,#32181);
#28082=AXIS2_PLACEMENT_3D('',#51246,#32185,#32186);
#28083=AXIS2_PLACEMENT_3D('',#51252,#32190,#32191);
#28084=AXIS2_PLACEMENT_3D('',#51258,#32195,#32196);
#28085=AXIS2_PLACEMENT_3D('',#51264,#32200,#32201);
#28086=AXIS2_PLACEMENT_3D('',#51270,#32205,#32206);
#28087=AXIS2_PLACEMENT_3D('',#51276,#32210,#32211);
#28088=AXIS2_PLACEMENT_3D('',#51282,#32215,#32216);
#28089=AXIS2_PLACEMENT_3D('',#51288,#32220,#32221);
#28090=AXIS2_PLACEMENT_3D('',#51294,#32225,#32226);
#28091=AXIS2_PLACEMENT_3D('',#51300,#32230,#32231);
#28092=AXIS2_PLACEMENT_3D('',#51306,#32235,#32236);
#28093=AXIS2_PLACEMENT_3D('',#51312,#32240,#32241);
#28094=AXIS2_PLACEMENT_3D('',#51318,#32245,#32246);
#28095=AXIS2_PLACEMENT_3D('',#51324,#32250,#32251);
#28096=AXIS2_PLACEMENT_3D('',#51330,#32255,#32256);
#28097=AXIS2_PLACEMENT_3D('',#51336,#32260,#32261);
#28098=AXIS2_PLACEMENT_3D('',#51342,#32265,#32266);
#28099=AXIS2_PLACEMENT_3D('',#51348,#32270,#32271);
#28100=AXIS2_PLACEMENT_3D('',#51354,#32275,#32276);
#28101=AXIS2_PLACEMENT_3D('',#51360,#32280,#32281);
#28102=AXIS2_PLACEMENT_3D('',#51366,#32285,#32286);
#28103=AXIS2_PLACEMENT_3D('',#51372,#32290,#32291);
#28104=AXIS2_PLACEMENT_3D('',#51378,#32295,#32296);
#28105=AXIS2_PLACEMENT_3D('',#51384,#32300,#32301);
#28106=AXIS2_PLACEMENT_3D('',#51390,#32305,#32306);
#28107=AXIS2_PLACEMENT_3D('',#51396,#32310,#32311);
#28108=AXIS2_PLACEMENT_3D('',#51402,#32315,#32316);
#28109=AXIS2_PLACEMENT_3D('',#51408,#32320,#32321);
#28110=AXIS2_PLACEMENT_3D('',#51414,#32325,#32326);
#28111=AXIS2_PLACEMENT_3D('',#51420,#32330,#32331);
#28112=AXIS2_PLACEMENT_3D('',#51426,#32335,#32336);
#28113=AXIS2_PLACEMENT_3D('',#51432,#32340,#32341);
#28114=AXIS2_PLACEMENT_3D('',#51438,#32345,#32346);
#28115=AXIS2_PLACEMENT_3D('',#51444,#32350,#32351);
#28116=AXIS2_PLACEMENT_3D('',#51450,#32355,#32356);
#28117=AXIS2_PLACEMENT_3D('',#51456,#32360,#32361);
#28118=AXIS2_PLACEMENT_3D('',#51462,#32365,#32366);
#28119=AXIS2_PLACEMENT_3D('',#51468,#32370,#32371);
#28120=AXIS2_PLACEMENT_3D('',#51474,#32375,#32376);
#28121=AXIS2_PLACEMENT_3D('',#51480,#32380,#32381);
#28122=AXIS2_PLACEMENT_3D('',#51486,#32385,#32386);
#28123=AXIS2_PLACEMENT_3D('',#51492,#32390,#32391);
#28124=AXIS2_PLACEMENT_3D('',#51498,#32395,#32396);
#28125=AXIS2_PLACEMENT_3D('',#51504,#32400,#32401);
#28126=AXIS2_PLACEMENT_3D('',#51510,#32405,#32406);
#28127=AXIS2_PLACEMENT_3D('',#51516,#32410,#32411);
#28128=AXIS2_PLACEMENT_3D('',#51522,#32415,#32416);
#28129=AXIS2_PLACEMENT_3D('',#51528,#32420,#32421);
#28130=AXIS2_PLACEMENT_3D('',#51534,#32425,#32426);
#28131=AXIS2_PLACEMENT_3D('',#51540,#32430,#32431);
#28132=AXIS2_PLACEMENT_3D('',#51546,#32435,#32436);
#28133=AXIS2_PLACEMENT_3D('',#51552,#32440,#32441);
#28134=AXIS2_PLACEMENT_3D('',#51558,#32445,#32446);
#28135=AXIS2_PLACEMENT_3D('',#51564,#32450,#32451);
#28136=AXIS2_PLACEMENT_3D('',#51570,#32455,#32456);
#28137=AXIS2_PLACEMENT_3D('',#51576,#32460,#32461);
#28138=AXIS2_PLACEMENT_3D('',#51582,#32465,#32466);
#28139=AXIS2_PLACEMENT_3D('',#51588,#32470,#32471);
#28140=AXIS2_PLACEMENT_3D('',#51594,#32475,#32476);
#28141=AXIS2_PLACEMENT_3D('',#51600,#32480,#32481);
#28142=AXIS2_PLACEMENT_3D('',#51606,#32485,#32486);
#28143=AXIS2_PLACEMENT_3D('',#51612,#32490,#32491);
#28144=AXIS2_PLACEMENT_3D('',#51618,#32495,#32496);
#28145=AXIS2_PLACEMENT_3D('',#51624,#32500,#32501);
#28146=AXIS2_PLACEMENT_3D('',#51630,#32505,#32506);
#28147=AXIS2_PLACEMENT_3D('',#51636,#32510,#32511);
#28148=AXIS2_PLACEMENT_3D('',#51642,#32515,#32516);
#28149=AXIS2_PLACEMENT_3D('',#51648,#32520,#32521);
#28150=AXIS2_PLACEMENT_3D('',#51654,#32525,#32526);
#28151=AXIS2_PLACEMENT_3D('',#51660,#32530,#32531);
#28152=AXIS2_PLACEMENT_3D('',#51666,#32535,#32536);
#28153=AXIS2_PLACEMENT_3D('',#51672,#32540,#32541);
#28154=AXIS2_PLACEMENT_3D('',#51678,#32545,#32546);
#28155=AXIS2_PLACEMENT_3D('',#51684,#32550,#32551);
#28156=AXIS2_PLACEMENT_3D('',#51690,#32555,#32556);
#28157=AXIS2_PLACEMENT_3D('',#51696,#32560,#32561);
#28158=AXIS2_PLACEMENT_3D('',#51702,#32565,#32566);
#28159=AXIS2_PLACEMENT_3D('',#51708,#32570,#32571);
#28160=AXIS2_PLACEMENT_3D('',#51714,#32575,#32576);
#28161=AXIS2_PLACEMENT_3D('',#51720,#32580,#32581);
#28162=AXIS2_PLACEMENT_3D('',#51726,#32585,#32586);
#28163=AXIS2_PLACEMENT_3D('',#51732,#32590,#32591);
#28164=AXIS2_PLACEMENT_3D('',#51738,#32595,#32596);
#28165=AXIS2_PLACEMENT_3D('',#51744,#32600,#32601);
#28166=AXIS2_PLACEMENT_3D('',#51750,#32605,#32606);
#28167=AXIS2_PLACEMENT_3D('',#51756,#32610,#32611);
#28168=AXIS2_PLACEMENT_3D('',#51762,#32615,#32616);
#28169=AXIS2_PLACEMENT_3D('',#51768,#32620,#32621);
#28170=AXIS2_PLACEMENT_3D('',#51774,#32625,#32626);
#28171=AXIS2_PLACEMENT_3D('',#51780,#32630,#32631);
#28172=AXIS2_PLACEMENT_3D('',#51786,#32635,#32636);
#28173=AXIS2_PLACEMENT_3D('',#51792,#32640,#32641);
#28174=AXIS2_PLACEMENT_3D('',#51798,#32645,#32646);
#28175=AXIS2_PLACEMENT_3D('',#51804,#32650,#32651);
#28176=AXIS2_PLACEMENT_3D('',#51810,#32655,#32656);
#28177=AXIS2_PLACEMENT_3D('',#51816,#32660,#32661);
#28178=AXIS2_PLACEMENT_3D('',#51822,#32665,#32666);
#28179=AXIS2_PLACEMENT_3D('',#51828,#32670,#32671);
#28180=AXIS2_PLACEMENT_3D('',#51834,#32675,#32676);
#28181=AXIS2_PLACEMENT_3D('',#51840,#32680,#32681);
#28182=AXIS2_PLACEMENT_3D('',#51846,#32685,#32686);
#28183=AXIS2_PLACEMENT_3D('',#51852,#32690,#32691);
#28184=AXIS2_PLACEMENT_3D('',#51858,#32695,#32696);
#28185=AXIS2_PLACEMENT_3D('',#51864,#32700,#32701);
#28186=AXIS2_PLACEMENT_3D('',#51870,#32705,#32706);
#28187=AXIS2_PLACEMENT_3D('',#51876,#32710,#32711);
#28188=AXIS2_PLACEMENT_3D('',#51882,#32715,#32716);
#28189=AXIS2_PLACEMENT_3D('',#51888,#32720,#32721);
#28190=AXIS2_PLACEMENT_3D('',#51894,#32725,#32726);
#28191=AXIS2_PLACEMENT_3D('',#51900,#32730,#32731);
#28192=AXIS2_PLACEMENT_3D('',#51906,#32735,#32736);
#28193=AXIS2_PLACEMENT_3D('',#51912,#32740,#32741);
#28194=AXIS2_PLACEMENT_3D('',#51918,#32745,#32746);
#28195=AXIS2_PLACEMENT_3D('',#51924,#32750,#32751);
#28196=AXIS2_PLACEMENT_3D('',#51930,#32755,#32756);
#28197=AXIS2_PLACEMENT_3D('',#51936,#32760,#32761);
#28198=AXIS2_PLACEMENT_3D('',#51942,#32765,#32766);
#28199=AXIS2_PLACEMENT_3D('',#51948,#32770,#32771);
#28200=AXIS2_PLACEMENT_3D('',#51954,#32775,#32776);
#28201=AXIS2_PLACEMENT_3D('',#51960,#32780,#32781);
#28202=AXIS2_PLACEMENT_3D('',#51966,#32785,#32786);
#28203=AXIS2_PLACEMENT_3D('',#51972,#32790,#32791);
#28204=AXIS2_PLACEMENT_3D('',#51978,#32795,#32796);
#28205=AXIS2_PLACEMENT_3D('',#51984,#32800,#32801);
#28206=AXIS2_PLACEMENT_3D('',#51990,#32805,#32806);
#28207=AXIS2_PLACEMENT_3D('',#51996,#32810,#32811);
#28208=AXIS2_PLACEMENT_3D('',#52002,#32815,#32816);
#28209=AXIS2_PLACEMENT_3D('',#52008,#32820,#32821);
#28210=AXIS2_PLACEMENT_3D('',#52014,#32825,#32826);
#28211=AXIS2_PLACEMENT_3D('',#52020,#32830,#32831);
#28212=AXIS2_PLACEMENT_3D('',#52026,#32835,#32836);
#28213=AXIS2_PLACEMENT_3D('',#52032,#32840,#32841);
#28214=AXIS2_PLACEMENT_3D('',#52038,#32845,#32846);
#28215=AXIS2_PLACEMENT_3D('',#52044,#32850,#32851);
#28216=AXIS2_PLACEMENT_3D('',#52050,#32855,#32856);
#28217=AXIS2_PLACEMENT_3D('',#52056,#32860,#32861);
#28218=AXIS2_PLACEMENT_3D('',#52062,#32865,#32866);
#28219=AXIS2_PLACEMENT_3D('',#52068,#32870,#32871);
#28220=AXIS2_PLACEMENT_3D('',#52074,#32875,#32876);
#28221=AXIS2_PLACEMENT_3D('',#52080,#32880,#32881);
#28222=AXIS2_PLACEMENT_3D('',#52086,#32885,#32886);
#28223=AXIS2_PLACEMENT_3D('',#52092,#32890,#32891);
#28224=AXIS2_PLACEMENT_3D('',#52098,#32895,#32896);
#28225=AXIS2_PLACEMENT_3D('',#52104,#32900,#32901);
#28226=AXIS2_PLACEMENT_3D('',#52110,#32905,#32906);
#28227=AXIS2_PLACEMENT_3D('',#52116,#32910,#32911);
#28228=AXIS2_PLACEMENT_3D('',#52122,#32915,#32916);
#28229=AXIS2_PLACEMENT_3D('',#52128,#32920,#32921);
#28230=AXIS2_PLACEMENT_3D('',#52134,#32925,#32926);
#28231=AXIS2_PLACEMENT_3D('',#52140,#32930,#32931);
#28232=AXIS2_PLACEMENT_3D('',#52146,#32935,#32936);
#28233=AXIS2_PLACEMENT_3D('',#52152,#32940,#32941);
#28234=AXIS2_PLACEMENT_3D('',#52158,#32945,#32946);
#28235=AXIS2_PLACEMENT_3D('',#52164,#32950,#32951);
#28236=AXIS2_PLACEMENT_3D('',#52170,#32955,#32956);
#28237=AXIS2_PLACEMENT_3D('',#52176,#32960,#32961);
#28238=AXIS2_PLACEMENT_3D('',#52182,#32965,#32966);
#28239=AXIS2_PLACEMENT_3D('',#52188,#32970,#32971);
#28240=AXIS2_PLACEMENT_3D('',#52194,#32975,#32976);
#28241=AXIS2_PLACEMENT_3D('',#52200,#32980,#32981);
#28242=AXIS2_PLACEMENT_3D('',#52206,#32985,#32986);
#28243=AXIS2_PLACEMENT_3D('',#52212,#32990,#32991);
#28244=AXIS2_PLACEMENT_3D('',#52218,#32995,#32996);
#28245=AXIS2_PLACEMENT_3D('',#52224,#33000,#33001);
#28246=AXIS2_PLACEMENT_3D('',#52230,#33005,#33006);
#28247=AXIS2_PLACEMENT_3D('',#52236,#33010,#33011);
#28248=AXIS2_PLACEMENT_3D('',#52242,#33015,#33016);
#28249=AXIS2_PLACEMENT_3D('',#52248,#33020,#33021);
#28250=AXIS2_PLACEMENT_3D('',#52254,#33025,#33026);
#28251=AXIS2_PLACEMENT_3D('',#52260,#33030,#33031);
#28252=AXIS2_PLACEMENT_3D('',#52266,#33035,#33036);
#28253=AXIS2_PLACEMENT_3D('',#52272,#33040,#33041);
#28254=AXIS2_PLACEMENT_3D('',#52278,#33045,#33046);
#28255=AXIS2_PLACEMENT_3D('',#52284,#33050,#33051);
#28256=AXIS2_PLACEMENT_3D('',#52290,#33055,#33056);
#28257=AXIS2_PLACEMENT_3D('',#52296,#33060,#33061);
#28258=AXIS2_PLACEMENT_3D('',#52302,#33065,#33066);
#28259=AXIS2_PLACEMENT_3D('',#52308,#33070,#33071);
#28260=AXIS2_PLACEMENT_3D('',#52314,#33075,#33076);
#28261=AXIS2_PLACEMENT_3D('',#52320,#33080,#33081);
#28262=AXIS2_PLACEMENT_3D('',#52326,#33085,#33086);
#28263=AXIS2_PLACEMENT_3D('',#52332,#33090,#33091);
#28264=AXIS2_PLACEMENT_3D('',#52338,#33095,#33096);
#28265=AXIS2_PLACEMENT_3D('',#52344,#33100,#33101);
#28266=AXIS2_PLACEMENT_3D('',#52350,#33105,#33106);
#28267=AXIS2_PLACEMENT_3D('',#52356,#33110,#33111);
#28268=AXIS2_PLACEMENT_3D('',#52362,#33115,#33116);
#28269=AXIS2_PLACEMENT_3D('',#52368,#33120,#33121);
#28270=AXIS2_PLACEMENT_3D('',#52374,#33125,#33126);
#28271=AXIS2_PLACEMENT_3D('',#52380,#33130,#33131);
#28272=AXIS2_PLACEMENT_3D('',#52386,#33135,#33136);
#28273=AXIS2_PLACEMENT_3D('',#52392,#33140,#33141);
#28274=AXIS2_PLACEMENT_3D('',#52398,#33145,#33146);
#28275=AXIS2_PLACEMENT_3D('',#52404,#33150,#33151);
#28276=AXIS2_PLACEMENT_3D('',#52410,#33155,#33156);
#28277=AXIS2_PLACEMENT_3D('',#52416,#33160,#33161);
#28278=AXIS2_PLACEMENT_3D('',#52422,#33165,#33166);
#28279=AXIS2_PLACEMENT_3D('',#52428,#33170,#33171);
#28280=AXIS2_PLACEMENT_3D('',#52434,#33175,#33176);
#28281=AXIS2_PLACEMENT_3D('',#52440,#33180,#33181);
#28282=AXIS2_PLACEMENT_3D('',#52446,#33185,#33186);
#28283=AXIS2_PLACEMENT_3D('',#52452,#33190,#33191);
#28284=AXIS2_PLACEMENT_3D('',#52458,#33195,#33196);
#28285=AXIS2_PLACEMENT_3D('',#52464,#33200,#33201);
#28286=AXIS2_PLACEMENT_3D('',#52470,#33205,#33206);
#28287=AXIS2_PLACEMENT_3D('',#52476,#33210,#33211);
#28288=AXIS2_PLACEMENT_3D('',#52482,#33215,#33216);
#28289=AXIS2_PLACEMENT_3D('',#52488,#33220,#33221);
#28290=AXIS2_PLACEMENT_3D('',#52494,#33225,#33226);
#28291=AXIS2_PLACEMENT_3D('',#52500,#33230,#33231);
#28292=AXIS2_PLACEMENT_3D('',#52506,#33235,#33236);
#28293=AXIS2_PLACEMENT_3D('',#52512,#33240,#33241);
#28294=AXIS2_PLACEMENT_3D('',#52518,#33245,#33246);
#28295=AXIS2_PLACEMENT_3D('',#52524,#33250,#33251);
#28296=AXIS2_PLACEMENT_3D('',#52530,#33255,#33256);
#28297=AXIS2_PLACEMENT_3D('',#52536,#33260,#33261);
#28298=AXIS2_PLACEMENT_3D('',#52542,#33265,#33266);
#28299=AXIS2_PLACEMENT_3D('',#52548,#33270,#33271);
#28300=AXIS2_PLACEMENT_3D('',#52554,#33275,#33276);
#28301=AXIS2_PLACEMENT_3D('',#52560,#33280,#33281);
#28302=AXIS2_PLACEMENT_3D('',#52566,#33285,#33286);
#28303=AXIS2_PLACEMENT_3D('',#52572,#33290,#33291);
#28304=AXIS2_PLACEMENT_3D('',#52578,#33295,#33296);
#28305=AXIS2_PLACEMENT_3D('',#52584,#33300,#33301);
#28306=AXIS2_PLACEMENT_3D('',#52590,#33305,#33306);
#28307=AXIS2_PLACEMENT_3D('',#52596,#33310,#33311);
#28308=AXIS2_PLACEMENT_3D('',#52602,#33315,#33316);
#28309=AXIS2_PLACEMENT_3D('',#52608,#33320,#33321);
#28310=AXIS2_PLACEMENT_3D('',#52614,#33325,#33326);
#28311=AXIS2_PLACEMENT_3D('',#52620,#33330,#33331);
#28312=AXIS2_PLACEMENT_3D('',#52626,#33335,#33336);
#28313=AXIS2_PLACEMENT_3D('',#52632,#33340,#33341);
#28314=AXIS2_PLACEMENT_3D('',#52638,#33345,#33346);
#28315=AXIS2_PLACEMENT_3D('',#52644,#33350,#33351);
#28316=AXIS2_PLACEMENT_3D('',#52650,#33355,#33356);
#28317=AXIS2_PLACEMENT_3D('',#52656,#33360,#33361);
#28318=AXIS2_PLACEMENT_3D('',#52662,#33365,#33366);
#28319=AXIS2_PLACEMENT_3D('',#52668,#33370,#33371);
#28320=AXIS2_PLACEMENT_3D('',#52674,#33375,#33376);
#28321=AXIS2_PLACEMENT_3D('',#52680,#33380,#33381);
#28322=AXIS2_PLACEMENT_3D('',#52686,#33385,#33386);
#28323=AXIS2_PLACEMENT_3D('',#52692,#33390,#33391);
#28324=AXIS2_PLACEMENT_3D('',#52698,#33395,#33396);
#28325=AXIS2_PLACEMENT_3D('',#52704,#33400,#33401);
#28326=AXIS2_PLACEMENT_3D('',#52710,#33405,#33406);
#28327=AXIS2_PLACEMENT_3D('',#52716,#33410,#33411);
#28328=AXIS2_PLACEMENT_3D('',#52722,#33415,#33416);
#28329=AXIS2_PLACEMENT_3D('',#52728,#33420,#33421);
#28330=AXIS2_PLACEMENT_3D('',#52734,#33425,#33426);
#28331=AXIS2_PLACEMENT_3D('',#52740,#33430,#33431);
#28332=AXIS2_PLACEMENT_3D('',#52746,#33435,#33436);
#28333=AXIS2_PLACEMENT_3D('',#52749,#33439,#33440);
#28334=AXIS2_PLACEMENT_3D('',#52750,#33441,#33442);
#28335=AXIS2_PLACEMENT_3D('',#52751,#33443,#33444);
#28336=AXIS2_PLACEMENT_3D('',#52752,#33445,#33446);
#28337=AXIS2_PLACEMENT_3D('',#52754,#33447,#33448);
#28338=AXIS2_PLACEMENT_3D('',#52757,#33450,#33451);
#28339=AXIS2_PLACEMENT_3D('',#52758,#33452,#33453);
#28340=AXIS2_PLACEMENT_3D('',#52776,#33462,#33463);
#28341=AXIS2_PLACEMENT_3D('',#52778,#33464,#33465);
#28342=AXIS2_PLACEMENT_3D('',#52780,#33466,#33467);
#28343=AXIS2_PLACEMENT_3D('',#52782,#33468,#33469);
#28344=AXIS2_PLACEMENT_3D('',#52808,#33482,#33483);
#28345=AXIS2_PLACEMENT_3D('',#52810,#33484,#33485);
#28346=AXIS2_PLACEMENT_3D('',#52812,#33486,#33487);
#28347=AXIS2_PLACEMENT_3D('',#52813,#33488,#33489);
#28348=AXIS2_PLACEMENT_3D('',#52816,#33491,#33492);
#28349=AXIS2_PLACEMENT_3D('',#52817,#33493,#33494);
#28350=AXIS2_PLACEMENT_3D('',#52819,#33495,#33496);
#28351=AXIS2_PLACEMENT_3D('',#52821,#33498,#33499);
#28352=AXIS2_PLACEMENT_3D('',#52824,#33501,#33502);
#28353=AXIS2_PLACEMENT_3D('',#52825,#33503,#33504);
#28354=AXIS2_PLACEMENT_3D('',#52827,#33505,#33506);
#28355=AXIS2_PLACEMENT_3D('',#52829,#33508,#33509);
#28356=AXIS2_PLACEMENT_3D('',#52832,#33511,#33512);
#28357=AXIS2_PLACEMENT_3D('',#52833,#33513,#33514);
#28358=AXIS2_PLACEMENT_3D('',#52835,#33515,#33516);
#28359=AXIS2_PLACEMENT_3D('',#52837,#33518,#33519);
#28360=AXIS2_PLACEMENT_3D('',#52840,#33521,#33522);
#28361=AXIS2_PLACEMENT_3D('',#52841,#33523,#33524);
#28362=AXIS2_PLACEMENT_3D('',#52843,#33525,#33526);
#28363=AXIS2_PLACEMENT_3D('',#52845,#33528,#33529);
#28364=AXIS2_PLACEMENT_3D('',#52848,#33531,#33532);
#28365=AXIS2_PLACEMENT_3D('',#52849,#33533,#33534);
#28366=AXIS2_PLACEMENT_3D('',#52851,#33535,#33536);
#28367=AXIS2_PLACEMENT_3D('',#52853,#33538,#33539);
#28368=AXIS2_PLACEMENT_3D('',#52856,#33541,#33542);
#28369=AXIS2_PLACEMENT_3D('',#52857,#33543,#33544);
#28370=AXIS2_PLACEMENT_3D('',#52859,#33545,#33546);
#28371=AXIS2_PLACEMENT_3D('',#52861,#33548,#33549);
#28372=AXIS2_PLACEMENT_3D('',#52864,#33551,#33552);
#28373=AXIS2_PLACEMENT_3D('',#52865,#33553,#33554);
#28374=AXIS2_PLACEMENT_3D('',#52867,#33555,#33556);
#28375=AXIS2_PLACEMENT_3D('',#52869,#33558,#33559);
#28376=AXIS2_PLACEMENT_3D('',#52872,#33561,#33562);
#28377=AXIS2_PLACEMENT_3D('',#52873,#33563,#33564);
#28378=AXIS2_PLACEMENT_3D('',#52879,#33568,#33569);
#28379=AXIS2_PLACEMENT_3D('',#52883,#33572,#33573);
#28380=AXIS2_PLACEMENT_3D('',#52887,#33576,#33577);
#28381=AXIS2_PLACEMENT_3D('',#52891,#33580,#33581);
#28382=AXIS2_PLACEMENT_3D('',#52895,#33584,#33585);
#28383=AXIS2_PLACEMENT_3D('',#52897,#33587,#33588);
#28384=AXIS2_PLACEMENT_3D('',#52903,#33592,#33593);
#28385=AXIS2_PLACEMENT_3D('',#52907,#33596,#33597);
#28386=AXIS2_PLACEMENT_3D('',#52911,#33600,#33601);
#28387=AXIS2_PLACEMENT_3D('',#52915,#33604,#33605);
#28388=AXIS2_PLACEMENT_3D('',#52919,#33608,#33609);
#28389=AXIS2_PLACEMENT_3D('',#52921,#33611,#33612);
#28390=AXIS2_PLACEMENT_3D('',#52927,#33616,#33617);
#28391=AXIS2_PLACEMENT_3D('',#52931,#33620,#33621);
#28392=AXIS2_PLACEMENT_3D('',#52935,#33624,#33625);
#28393=AXIS2_PLACEMENT_3D('',#52939,#33628,#33629);
#28394=AXIS2_PLACEMENT_3D('',#52943,#33632,#33633);
#28395=AXIS2_PLACEMENT_3D('',#52947,#33636,#33637);
#28396=AXIS2_PLACEMENT_3D('',#52951,#33640,#33641);
#28397=AXIS2_PLACEMENT_3D('',#52953,#33643,#33644);
#28398=AXIS2_PLACEMENT_3D('',#52959,#33648,#33649);
#28399=AXIS2_PLACEMENT_3D('',#52963,#33652,#33653);
#28400=AXIS2_PLACEMENT_3D('',#52967,#33656,#33657);
#28401=AXIS2_PLACEMENT_3D('',#52971,#33660,#33661);
#28402=AXIS2_PLACEMENT_3D('',#52975,#33664,#33665);
#28403=AXIS2_PLACEMENT_3D('',#52979,#33668,#33669);
#28404=AXIS2_PLACEMENT_3D('',#52983,#33672,#33673);
#28405=AXIS2_PLACEMENT_3D('',#52985,#33675,#33676);
#28406=AXIS2_PLACEMENT_3D('',#52986,#33677,#33678);
#28407=AXIS2_PLACEMENT_3D('',#52987,#33679,#33680);
#28408=AXIS2_PLACEMENT_3D('',#52989,#33681,#33682);
#28409=AXIS2_PLACEMENT_3D('',#52992,#33684,#33685);
#28410=AXIS2_PLACEMENT_3D('',#52993,#33686,#33687);
#28411=AXIS2_PLACEMENT_3D('',#52995,#33688,#33689);
#28412=AXIS2_PLACEMENT_3D('',#52998,#33691,#33692);
#28413=AXIS2_PLACEMENT_3D('',#52999,#33693,#33694);
#28414=AXIS2_PLACEMENT_3D('',#53001,#33695,#33696);
#28415=AXIS2_PLACEMENT_3D('',#53004,#33698,#33699);
#28416=AXIS2_PLACEMENT_3D('',#53005,#33700,#33701);
#28417=AXIS2_PLACEMENT_3D('',#53009,#33703,#33704);
#28418=AXIS2_PLACEMENT_3D('',#53011,#33705,#33706);
#28419=AXIS2_PLACEMENT_3D('',#53013,#33707,#33708);
#28420=AXIS2_PLACEMENT_3D('',#53015,#33709,#33710);
#28421=AXIS2_PLACEMENT_3D('',#53016,#33711,#33712);
#28422=AXIS2_PLACEMENT_3D('',#53017,#33713,#33714);
#28423=AXIS2_PLACEMENT_3D('',#53026,#33719,#33720);
#28424=AXIS2_PLACEMENT_3D('',#53028,#33721,#33722);
#28425=AXIS2_PLACEMENT_3D('',#53031,#33724,#33725);
#28426=AXIS2_PLACEMENT_3D('',#53032,#33726,#33727);
#28427=AXIS2_PLACEMENT_3D('',#53036,#33729,#33730);
#28428=AXIS2_PLACEMENT_3D('',#53038,#33731,#33732);
#28429=AXIS2_PLACEMENT_3D('',#53040,#33733,#33734);
#28430=AXIS2_PLACEMENT_3D('',#53042,#33735,#33736);
#28431=AXIS2_PLACEMENT_3D('',#53043,#33737,#33738);
#28432=AXIS2_PLACEMENT_3D('',#53044,#33739,#33740);
#28433=AXIS2_PLACEMENT_3D('',#53053,#33745,#33746);
#28434=AXIS2_PLACEMENT_3D('',#53061,#33747,#33748);
#28435=AXIS2_PLACEMENT_3D('',#53068,#33749,#33750);
#28436=AXIS2_PLACEMENT_3D('',#53070,#33751,#33752);
#28437=AXIS2_PLACEMENT_3D('',#53074,#33754,#33755);
#28438=AXIS2_PLACEMENT_3D('',#53075,#33756,#33757);
#28439=AXIS2_PLACEMENT_3D('',#53076,#33758,#33759);
#28440=AXIS2_PLACEMENT_3D('',#53084,#33760,#33761);
#28441=AXIS2_PLACEMENT_3D('',#53091,#33762,#33763);
#28442=AXIS2_PLACEMENT_3D('',#53093,#33764,#33765);
#28443=AXIS2_PLACEMENT_3D('',#53097,#33767,#33768);
#28444=AXIS2_PLACEMENT_3D('',#53098,#33769,#33770);
#28445=AXIS2_PLACEMENT_3D('',#53099,#33771,#33772);
#28446=AXIS2_PLACEMENT_3D('',#53102,#33774,#33775);
#28447=AXIS2_PLACEMENT_3D('',#53103,#33776,#33777);
#28448=AXIS2_PLACEMENT_3D('',#53113,#33783,#33784);
#28449=AXIS2_PLACEMENT_3D('',#53116,#33786,#33787);
#28450=AXIS2_PLACEMENT_3D('',#53119,#33789,#33790);
#28451=AXIS2_PLACEMENT_3D('',#53120,#33791,#33792);
#28452=AXIS2_PLACEMENT_3D('',#53130,#33798,#33799);
#28453=AXIS2_PLACEMENT_3D('',#53133,#33801,#33802);
#28454=AXIS2_PLACEMENT_3D('',#53136,#33805,#33806);
#28455=AXIS2_PLACEMENT_3D('',#53138,#33808,#33809);
#28456=AXIS2_PLACEMENT_3D('',#53140,#33811,#33812);
#28457=AXIS2_PLACEMENT_3D('',#53146,#33816,#33817);
#28458=AXIS2_PLACEMENT_3D('',#53152,#33821,#33822);
#28459=AXIS2_PLACEMENT_3D('',#53155,#33825,#33826);
#28460=AXIS2_PLACEMENT_3D('',#53156,#33827,#33828);
#28461=AXIS2_PLACEMENT_3D('',#53157,#33829,#33830);
#28462=AXIS2_PLACEMENT_3D('',#53158,#33831,#33832);
#28463=AXIS2_PLACEMENT_3D('',#53270,#33834,#33835);
#28464=AXIS2_PLACEMENT_3D('',#53345,#33836,#33837);
#28465=AXIS2_PLACEMENT_3D('',#53643,#33839,#33840);
#28466=AXIS2_PLACEMENT_3D('',#53943,#33842,#33843);
#28467=AXIS2_PLACEMENT_3D('',#54233,#33845,#33846);
#28468=AXIS2_PLACEMENT_3D('',#54531,#33848,#33849);
#28469=AXIS2_PLACEMENT_3D('',#54823,#33851,#33852);
#28470=AXIS2_PLACEMENT_3D('',#55113,#33854,#33855);
#28471=AXIS2_PLACEMENT_3D('',#55175,#33856,#33857);
#28472=AXIS2_PLACEMENT_3D('',#56447,#33858,#33859);
#28473=AXIS2_PLACEMENT_3D('',#57519,#33860,#33861);
#28474=AXIS2_PLACEMENT_3D('',#57650,#33862,#33863);
#28475=AXIS2_PLACEMENT_3D('',#57747,#33864,#33865);
#28476=AXIS2_PLACEMENT_3D('',#57750,#33866,#33867);
#28477=AXIS2_PLACEMENT_3D('',#57920,#33868,#33869);
#28478=AXIS2_PLACEMENT_3D('',#58223,#33870,#33871);
#28479=AXIS2_PLACEMENT_3D('',#58226,#33872,#33873);
#28480=AXIS2_PLACEMENT_3D('',#58306,#33874,#33875);
#28481=AXIS2_PLACEMENT_3D('',#58519,#33876,#33877);
#28482=AXIS2_PLACEMENT_3D('',#58521,#33878,#33879);
#28483=AXIS2_PLACEMENT_3D('',#58522,#33880,#33881);
#28484=AXIS2_PLACEMENT_3D('',#58523,#33882,#33883);
#28485=AXIS2_PLACEMENT_3D('',#58525,#33884,#33885);
#28486=AXIS2_PLACEMENT_3D('',#58526,#33886,#33887);
#28487=AXIS2_PLACEMENT_3D('',#58529,#33889,#33890);
#28488=AXIS2_PLACEMENT_3D('',#58530,#33891,#33892);
#28489=AXIS2_PLACEMENT_3D('',#58531,#33893,#33894);
#28490=AXIS2_PLACEMENT_3D('',#58542,#33898,#33899);
#28491=AXIS2_PLACEMENT_3D('',#58550,#33902,#33903);
#28492=AXIS2_PLACEMENT_3D('',#58551,#33904,#33905);
#28493=AXIS2_PLACEMENT_3D('',#58552,#33906,#33907);
#28494=AXIS2_PLACEMENT_3D('',#58559,#33908,#33909);
#28495=AXIS2_PLACEMENT_3D('',#58569,#33910,#33911);
#28496=AXIS2_PLACEMENT_3D('',#58579,#33912,#33913);
#28497=AXIS2_PLACEMENT_3D('',#58589,#33914,#33915);
#28498=AXIS2_PLACEMENT_3D('',#58599,#33916,#33917);
#28499=AXIS2_PLACEMENT_3D('',#58609,#33918,#33919);
#28500=AXIS2_PLACEMENT_3D('',#58619,#33920,#33921);
#28501=AXIS2_PLACEMENT_3D('',#58629,#33922,#33923);
#28502=AXIS2_PLACEMENT_3D('',#58639,#33924,#33925);
#28503=AXIS2_PLACEMENT_3D('',#58649,#33926,#33927);
#28504=AXIS2_PLACEMENT_3D('',#58659,#33928,#33929);
#28505=AXIS2_PLACEMENT_3D('',#58669,#33930,#33931);
#28506=AXIS2_PLACEMENT_3D('',#58679,#33932,#33933);
#28507=AXIS2_PLACEMENT_3D('',#58689,#33934,#33935);
#28508=AXIS2_PLACEMENT_3D('',#58699,#33936,#33937);
#28509=AXIS2_PLACEMENT_3D('',#58709,#33938,#33939);
#28510=AXIS2_PLACEMENT_3D('',#58719,#33940,#33941);
#28511=AXIS2_PLACEMENT_3D('',#58729,#33942,#33943);
#28512=AXIS2_PLACEMENT_3D('',#58739,#33944,#33945);
#28513=AXIS2_PLACEMENT_3D('',#58749,#33946,#33947);
#28514=AXIS2_PLACEMENT_3D('',#58759,#33948,#33949);
#28515=AXIS2_PLACEMENT_3D('',#58769,#33950,#33951);
#28516=AXIS2_PLACEMENT_3D('',#58779,#33952,#33953);
#28517=AXIS2_PLACEMENT_3D('',#58789,#33954,#33955);
#28518=AXIS2_PLACEMENT_3D('',#58799,#33956,#33957);
#28519=AXIS2_PLACEMENT_3D('',#58809,#33958,#33959);
#28520=AXIS2_PLACEMENT_3D('',#58819,#33960,#33961);
#28521=AXIS2_PLACEMENT_3D('',#58828,#33962,#33963);
#28522=AXIS2_PLACEMENT_3D('',#58830,#33964,#33965);
#28523=AXIS2_PLACEMENT_3D('',#58840,#33966,#33967);
#28524=AXIS2_PLACEMENT_3D('',#58850,#33968,#33969);
#28525=AXIS2_PLACEMENT_3D('',#58860,#33970,#33971);
#28526=AXIS2_PLACEMENT_3D('',#58870,#33972,#33973);
#28527=AXIS2_PLACEMENT_3D('',#58880,#33974,#33975);
#28528=AXIS2_PLACEMENT_3D('',#58890,#33976,#33977);
#28529=AXIS2_PLACEMENT_3D('',#58900,#33978,#33979);
#28530=AXIS2_PLACEMENT_3D('',#58906,#33981,#33982);
#28531=AXIS2_PLACEMENT_3D('',#58907,#33983,#33984);
#28532=AXIS2_PLACEMENT_3D('',#58913,#33988,#33989);
#28533=AXIS2_PLACEMENT_3D('',#58917,#33992,#33993);
#28534=AXIS2_PLACEMENT_3D('',#58918,#33994,#33995);
#28535=AXIS2_PLACEMENT_3D('',#58919,#33996,#33997);
#28536=AXIS2_PLACEMENT_3D('',#58925,#34001,#34002);
#28537=AXIS2_PLACEMENT_3D('',#58929,#34005,#34006);
#28538=AXIS2_PLACEMENT_3D('',#58930,#34007,#34008);
#28539=AXIS2_PLACEMENT_3D('',#58931,#34009,#34010);
#28540=AXIS2_PLACEMENT_3D('',#58937,#34014,#34015);
#28541=AXIS2_PLACEMENT_3D('',#58941,#34018,#34019);
#28542=AXIS2_PLACEMENT_3D('',#58942,#34020,#34021);
#28543=AXIS2_PLACEMENT_3D('',#58943,#34022,#34023);
#28544=AXIS2_PLACEMENT_3D('',#58949,#34027,#34028);
#28545=AXIS2_PLACEMENT_3D('',#58953,#34031,#34032);
#28546=AXIS2_PLACEMENT_3D('',#58954,#34033,#34034);
#28547=AXIS2_PLACEMENT_3D('',#58955,#34035,#34036);
#28548=AXIS2_PLACEMENT_3D('',#58961,#34040,#34041);
#28549=AXIS2_PLACEMENT_3D('',#58965,#34044,#34045);
#28550=AXIS2_PLACEMENT_3D('',#58966,#34046,#34047);
#28551=AXIS2_PLACEMENT_3D('',#58967,#34048,#34049);
#28552=AXIS2_PLACEMENT_3D('',#58973,#34053,#34054);
#28553=AXIS2_PLACEMENT_3D('',#58977,#34057,#34058);
#28554=AXIS2_PLACEMENT_3D('',#58978,#34059,#34060);
#28555=AXIS2_PLACEMENT_3D('',#58979,#34061,#34062);
#28556=AXIS2_PLACEMENT_3D('',#58985,#34066,#34067);
#28557=AXIS2_PLACEMENT_3D('',#58989,#34070,#34071);
#28558=AXIS2_PLACEMENT_3D('',#58990,#34072,#34073);
#28559=AXIS2_PLACEMENT_3D('',#58991,#34074,#34075);
#28560=AXIS2_PLACEMENT_3D('',#58997,#34079,#34080);
#28561=AXIS2_PLACEMENT_3D('',#59001,#34083,#34084);
#28562=AXIS2_PLACEMENT_3D('',#59003,#34085,#34086);
#28563=AXIS2_PLACEMENT_3D('',#59004,#34087,#34088);
#28564=AXIS2_PLACEMENT_3D('',#59005,#34089,#34090);
#28565=AXIS2_PLACEMENT_3D('',#59011,#34094,#34095);
#28566=AXIS2_PLACEMENT_3D('',#59015,#34098,#34099);
#28567=AXIS2_PLACEMENT_3D('',#59016,#34100,#34101);
#28568=AXIS2_PLACEMENT_3D('',#59017,#34102,#34103);
#28569=AXIS2_PLACEMENT_3D('',#59023,#34107,#34108);
#28570=AXIS2_PLACEMENT_3D('',#59027,#34111,#34112);
#28571=AXIS2_PLACEMENT_3D('',#59028,#34113,#34114);
#28572=AXIS2_PLACEMENT_3D('',#59029,#34115,#34116);
#28573=AXIS2_PLACEMENT_3D('',#59035,#34120,#34121);
#28574=AXIS2_PLACEMENT_3D('',#59039,#34124,#34125);
#28575=AXIS2_PLACEMENT_3D('',#59040,#34126,#34127);
#28576=AXIS2_PLACEMENT_3D('',#59041,#34128,#34129);
#28577=AXIS2_PLACEMENT_3D('',#59047,#34133,#34134);
#28578=AXIS2_PLACEMENT_3D('',#59051,#34137,#34138);
#28579=AXIS2_PLACEMENT_3D('',#59052,#34139,#34140);
#28580=AXIS2_PLACEMENT_3D('',#59053,#34141,#34142);
#28581=AXIS2_PLACEMENT_3D('',#59059,#34146,#34147);
#28582=AXIS2_PLACEMENT_3D('',#59063,#34150,#34151);
#28583=AXIS2_PLACEMENT_3D('',#59064,#34152,#34153);
#28584=AXIS2_PLACEMENT_3D('',#59065,#34154,#34155);
#28585=AXIS2_PLACEMENT_3D('',#59071,#34159,#34160);
#28586=AXIS2_PLACEMENT_3D('',#59075,#34163,#34164);
#28587=AXIS2_PLACEMENT_3D('',#59076,#34165,#34166);
#28588=AXIS2_PLACEMENT_3D('',#59077,#34167,#34168);
#28589=AXIS2_PLACEMENT_3D('',#59083,#34172,#34173);
#28590=AXIS2_PLACEMENT_3D('',#59087,#34176,#34177);
#28591=AXIS2_PLACEMENT_3D('',#59088,#34178,#34179);
#28592=AXIS2_PLACEMENT_3D('',#59089,#34180,#34181);
#28593=AXIS2_PLACEMENT_3D('',#59095,#34185,#34186);
#28594=AXIS2_PLACEMENT_3D('',#59099,#34189,#34190);
#28595=AXIS2_PLACEMENT_3D('',#59100,#34191,#34192);
#28596=AXIS2_PLACEMENT_3D('',#59101,#34193,#34194);
#28597=AXIS2_PLACEMENT_3D('',#59107,#34198,#34199);
#28598=AXIS2_PLACEMENT_3D('',#59111,#34202,#34203);
#28599=AXIS2_PLACEMENT_3D('',#59112,#34204,#34205);
#28600=AXIS2_PLACEMENT_3D('',#59113,#34206,#34207);
#28601=AXIS2_PLACEMENT_3D('',#59119,#34211,#34212);
#28602=AXIS2_PLACEMENT_3D('',#59123,#34215,#34216);
#28603=AXIS2_PLACEMENT_3D('',#59124,#34217,#34218);
#28604=AXIS2_PLACEMENT_3D('',#59125,#34219,#34220);
#28605=AXIS2_PLACEMENT_3D('',#59131,#34224,#34225);
#28606=AXIS2_PLACEMENT_3D('',#59135,#34228,#34229);
#28607=AXIS2_PLACEMENT_3D('',#59136,#34230,#34231);
#28608=AXIS2_PLACEMENT_3D('',#59137,#34232,#34233);
#28609=AXIS2_PLACEMENT_3D('',#59143,#34237,#34238);
#28610=AXIS2_PLACEMENT_3D('',#59147,#34241,#34242);
#28611=AXIS2_PLACEMENT_3D('',#59148,#34243,#34244);
#28612=AXIS2_PLACEMENT_3D('',#59149,#34245,#34246);
#28613=AXIS2_PLACEMENT_3D('',#59155,#34250,#34251);
#28614=AXIS2_PLACEMENT_3D('',#59159,#34254,#34255);
#28615=AXIS2_PLACEMENT_3D('',#59160,#34256,#34257);
#28616=AXIS2_PLACEMENT_3D('',#59161,#34258,#34259);
#28617=AXIS2_PLACEMENT_3D('',#59167,#34263,#34264);
#28618=AXIS2_PLACEMENT_3D('',#59171,#34267,#34268);
#28619=AXIS2_PLACEMENT_3D('',#59172,#34269,#34270);
#28620=AXIS2_PLACEMENT_3D('',#59173,#34271,#34272);
#28621=AXIS2_PLACEMENT_3D('',#59179,#34276,#34277);
#28622=AXIS2_PLACEMENT_3D('',#59183,#34280,#34281);
#28623=AXIS2_PLACEMENT_3D('',#59184,#34282,#34283);
#28624=AXIS2_PLACEMENT_3D('',#59185,#34284,#34285);
#28625=AXIS2_PLACEMENT_3D('',#59191,#34289,#34290);
#28626=AXIS2_PLACEMENT_3D('',#59195,#34293,#34294);
#28627=AXIS2_PLACEMENT_3D('',#59196,#34295,#34296);
#28628=AXIS2_PLACEMENT_3D('',#59197,#34297,#34298);
#28629=AXIS2_PLACEMENT_3D('',#59203,#34302,#34303);
#28630=AXIS2_PLACEMENT_3D('',#59207,#34306,#34307);
#28631=AXIS2_PLACEMENT_3D('',#59208,#34308,#34309);
#28632=AXIS2_PLACEMENT_3D('',#59209,#34310,#34311);
#28633=AXIS2_PLACEMENT_3D('',#59215,#34315,#34316);
#28634=AXIS2_PLACEMENT_3D('',#59219,#34319,#34320);
#28635=AXIS2_PLACEMENT_3D('',#59220,#34321,#34322);
#28636=AXIS2_PLACEMENT_3D('',#59221,#34323,#34324);
#28637=AXIS2_PLACEMENT_3D('',#59227,#34328,#34329);
#28638=AXIS2_PLACEMENT_3D('',#59231,#34332,#34333);
#28639=AXIS2_PLACEMENT_3D('',#59232,#34334,#34335);
#28640=AXIS2_PLACEMENT_3D('',#59233,#34336,#34337);
#28641=AXIS2_PLACEMENT_3D('',#59239,#34341,#34342);
#28642=AXIS2_PLACEMENT_3D('',#59243,#34345,#34346);
#28643=AXIS2_PLACEMENT_3D('',#59244,#34347,#34348);
#28644=AXIS2_PLACEMENT_3D('',#59245,#34349,#34350);
#28645=AXIS2_PLACEMENT_3D('',#59251,#34354,#34355);
#28646=AXIS2_PLACEMENT_3D('',#59255,#34358,#34359);
#28647=AXIS2_PLACEMENT_3D('',#59256,#34360,#34361);
#28648=AXIS2_PLACEMENT_3D('',#59257,#34362,#34363);
#28649=AXIS2_PLACEMENT_3D('',#59263,#34367,#34368);
#28650=AXIS2_PLACEMENT_3D('',#59267,#34371,#34372);
#28651=AXIS2_PLACEMENT_3D('',#59268,#34373,#34374);
#28652=AXIS2_PLACEMENT_3D('',#59269,#34375,#34376);
#28653=AXIS2_PLACEMENT_3D('',#59275,#34380,#34381);
#28654=AXIS2_PLACEMENT_3D('',#59279,#34384,#34385);
#28655=AXIS2_PLACEMENT_3D('',#59280,#34386,#34387);
#28656=AXIS2_PLACEMENT_3D('',#59281,#34388,#34389);
#28657=AXIS2_PLACEMENT_3D('',#59287,#34393,#34394);
#28658=AXIS2_PLACEMENT_3D('',#59291,#34397,#34398);
#28659=AXIS2_PLACEMENT_3D('',#59292,#34399,#34400);
#28660=AXIS2_PLACEMENT_3D('',#59293,#34401,#34402);
#28661=AXIS2_PLACEMENT_3D('',#59299,#34406,#34407);
#28662=AXIS2_PLACEMENT_3D('',#59303,#34410,#34411);
#28663=AXIS2_PLACEMENT_3D('',#59304,#34412,#34413);
#28664=AXIS2_PLACEMENT_3D('',#59305,#34414,#34415);
#28665=AXIS2_PLACEMENT_3D('',#59311,#34419,#34420);
#28666=AXIS2_PLACEMENT_3D('',#59315,#34423,#34424);
#28667=AXIS2_PLACEMENT_3D('',#59316,#34425,#34426);
#28668=AXIS2_PLACEMENT_3D('',#59317,#34427,#34428);
#28669=AXIS2_PLACEMENT_3D('',#59323,#34432,#34433);
#28670=AXIS2_PLACEMENT_3D('',#59327,#34436,#34437);
#28671=AXIS2_PLACEMENT_3D('',#59328,#34438,#34439);
#28672=AXIS2_PLACEMENT_3D('',#59329,#34440,#34441);
#28673=AXIS2_PLACEMENT_3D('',#59331,#34443,#34444);
#28674=AXIS2_PLACEMENT_3D('',#59344,#34451,#34452);
#28675=AXIS2_PLACEMENT_3D('',#59348,#34454,#34455);
#28676=AXIS2_PLACEMENT_3D('',#59349,#34456,#34457);
#28677=AXIS2_PLACEMENT_3D('',#59352,#34459,#34460);
#28678=AXIS2_PLACEMENT_3D('',#59353,#34461,#34462);
#28679=AXIS2_PLACEMENT_3D('',#59356,#34464,#34465);
#28680=AXIS2_PLACEMENT_3D('',#59357,#34466,#34467);
#28681=AXIS2_PLACEMENT_3D('',#59360,#34469,#34470);
#28682=AXIS2_PLACEMENT_3D('',#59361,#34471,#34472);
#28683=AXIS2_PLACEMENT_3D('',#59364,#34474,#34475);
#28684=AXIS2_PLACEMENT_3D('',#59365,#34476,#34477);
#28685=AXIS2_PLACEMENT_3D('',#59367,#34479,#34480);
#28686=AXIS2_PLACEMENT_3D('',#59368,#34481,#34482);
#28687=AXIS2_PLACEMENT_3D('',#59371,#34484,#34485);
#28688=AXIS2_PLACEMENT_3D('',#59374,#34488,#34489);
#28689=AXIS2_PLACEMENT_3D('',#59376,#34491,#34492);
#28690=AXIS2_PLACEMENT_3D('',#59378,#34494,#34495);
#28691=AXIS2_PLACEMENT_3D('',#59380,#34497,#34498);
#28692=AXIS2_PLACEMENT_3D('',#59382,#34500,#34501);
#28693=AXIS2_PLACEMENT_3D('',#59383,#34502,#34503);
#28694=AXIS2_PLACEMENT_3D('',#59384,#34504,#34505);
#28695=AXIS2_PLACEMENT_3D('',#59517,#34507,#34508);
#28696=AXIS2_PLACEMENT_3D('',#59606,#34509,#34510);
#28697=AXIS2_PLACEMENT_3D('',#59939,#34512,#34513);
#28698=AXIS2_PLACEMENT_3D('',#60135,#34515,#34516);
#28699=AXIS2_PLACEMENT_3D('',#60332,#34518,#34519);
#28700=AXIS2_PLACEMENT_3D('',#60511,#34521,#34522);
#28701=AXIS2_PLACEMENT_3D('',#60811,#34524,#34525);
#28702=AXIS2_PLACEMENT_3D('',#61130,#34527,#34528);
#28703=AXIS2_PLACEMENT_3D('',#61451,#34530,#34531);
#28704=AXIS2_PLACEMENT_3D('',#61780,#34533,#34534);
#28705=AXIS2_PLACEMENT_3D('',#61845,#34535,#34536);
#28706=AXIS2_PLACEMENT_3D('',#63460,#34537,#34538);
#28707=AXIS2_PLACEMENT_3D('',#64860,#34539,#34540);
#28708=AXIS2_PLACEMENT_3D('',#65016,#34541,#34542);
#28709=AXIS2_PLACEMENT_3D('',#65132,#34543,#34544);
#28710=AXIS2_PLACEMENT_3D('',#65135,#34545,#34546);
#28711=AXIS2_PLACEMENT_3D('',#65291,#34547,#34548);
#28712=AXIS2_PLACEMENT_3D('',#65631,#34549,#34550);
#28713=AXIS2_PLACEMENT_3D('',#65634,#34551,#34552);
#28714=AXIS2_PLACEMENT_3D('',#65711,#34553,#34554);
#28715=AXIS2_PLACEMENT_3D('',#65972,#34555,#34556);
#28716=AXIS2_PLACEMENT_3D('',#65974,#34557,#34558);
#28717=AXIS2_PLACEMENT_3D('',#65975,#34559,#34560);
#28718=AXIS2_PLACEMENT_3D('',#65976,#34561,#34562);
#28719=AXIS2_PLACEMENT_3D('',#65978,#34563,#34564);
#28720=AXIS2_PLACEMENT_3D('',#65979,#34565,#34566);
#28721=AXIS2_PLACEMENT_3D('',#65982,#34568,#34569);
#28722=AXIS2_PLACEMENT_3D('',#65983,#34570,#34571);
#28723=AXIS2_PLACEMENT_3D('',#65984,#34572,#34573);
#28724=AXIS2_PLACEMENT_3D('',#65995,#34577,#34578);
#28725=AXIS2_PLACEMENT_3D('',#66003,#34581,#34582);
#28726=AXIS2_PLACEMENT_3D('',#66004,#34583,#34584);
#28727=AXIS2_PLACEMENT_3D('',#66005,#34585,#34586);
#28728=AXIS2_PLACEMENT_3D('',#66012,#34587,#34588);
#28729=AXIS2_PLACEMENT_3D('',#66022,#34589,#34590);
#28730=AXIS2_PLACEMENT_3D('',#66032,#34591,#34592);
#28731=AXIS2_PLACEMENT_3D('',#66042,#34593,#34594);
#28732=AXIS2_PLACEMENT_3D('',#66052,#34595,#34596);
#28733=AXIS2_PLACEMENT_3D('',#66062,#34597,#34598);
#28734=AXIS2_PLACEMENT_3D('',#66072,#34599,#34600);
#28735=AXIS2_PLACEMENT_3D('',#66082,#34601,#34602);
#28736=AXIS2_PLACEMENT_3D('',#66092,#34603,#34604);
#28737=AXIS2_PLACEMENT_3D('',#66102,#34605,#34606);
#28738=AXIS2_PLACEMENT_3D('',#66112,#34607,#34608);
#28739=AXIS2_PLACEMENT_3D('',#66122,#34609,#34610);
#28740=AXIS2_PLACEMENT_3D('',#66132,#34611,#34612);
#28741=AXIS2_PLACEMENT_3D('',#66142,#34613,#34614);
#28742=AXIS2_PLACEMENT_3D('',#66152,#34615,#34616);
#28743=AXIS2_PLACEMENT_3D('',#66162,#34617,#34618);
#28744=AXIS2_PLACEMENT_3D('',#66172,#34619,#34620);
#28745=AXIS2_PLACEMENT_3D('',#66182,#34621,#34622);
#28746=AXIS2_PLACEMENT_3D('',#66191,#34623,#34624);
#28747=AXIS2_PLACEMENT_3D('',#66193,#34625,#34626);
#28748=AXIS2_PLACEMENT_3D('',#66203,#34627,#34628);
#28749=AXIS2_PLACEMENT_3D('',#66213,#34629,#34630);
#28750=AXIS2_PLACEMENT_3D('',#66223,#34631,#34632);
#28751=AXIS2_PLACEMENT_3D('',#66233,#34633,#34634);
#28752=AXIS2_PLACEMENT_3D('',#66243,#34635,#34636);
#28753=AXIS2_PLACEMENT_3D('',#66253,#34637,#34638);
#28754=AXIS2_PLACEMENT_3D('',#66263,#34639,#34640);
#28755=AXIS2_PLACEMENT_3D('',#66273,#34641,#34642);
#28756=AXIS2_PLACEMENT_3D('',#66283,#34643,#34644);
#28757=AXIS2_PLACEMENT_3D('',#66293,#34645,#34646);
#28758=AXIS2_PLACEMENT_3D('',#66303,#34647,#34648);
#28759=AXIS2_PLACEMENT_3D('',#66313,#34649,#34650);
#28760=AXIS2_PLACEMENT_3D('',#66323,#34651,#34652);
#28761=AXIS2_PLACEMENT_3D('',#66333,#34653,#34654);
#28762=AXIS2_PLACEMENT_3D('',#66343,#34655,#34656);
#28763=AXIS2_PLACEMENT_3D('',#66353,#34657,#34658);
#28764=AXIS2_PLACEMENT_3D('',#66359,#34660,#34661);
#28765=AXIS2_PLACEMENT_3D('',#66360,#34662,#34663);
#28766=AXIS2_PLACEMENT_3D('',#66366,#34667,#34668);
#28767=AXIS2_PLACEMENT_3D('',#66370,#34671,#34672);
#28768=AXIS2_PLACEMENT_3D('',#66371,#34673,#34674);
#28769=AXIS2_PLACEMENT_3D('',#66372,#34675,#34676);
#28770=AXIS2_PLACEMENT_3D('',#66378,#34680,#34681);
#28771=AXIS2_PLACEMENT_3D('',#66382,#34684,#34685);
#28772=AXIS2_PLACEMENT_3D('',#66383,#34686,#34687);
#28773=AXIS2_PLACEMENT_3D('',#66384,#34688,#34689);
#28774=AXIS2_PLACEMENT_3D('',#66390,#34693,#34694);
#28775=AXIS2_PLACEMENT_3D('',#66394,#34697,#34698);
#28776=AXIS2_PLACEMENT_3D('',#66395,#34699,#34700);
#28777=AXIS2_PLACEMENT_3D('',#66396,#34701,#34702);
#28778=AXIS2_PLACEMENT_3D('',#66402,#34706,#34707);
#28779=AXIS2_PLACEMENT_3D('',#66406,#34710,#34711);
#28780=AXIS2_PLACEMENT_3D('',#66407,#34712,#34713);
#28781=AXIS2_PLACEMENT_3D('',#66408,#34714,#34715);
#28782=AXIS2_PLACEMENT_3D('',#66414,#34719,#34720);
#28783=AXIS2_PLACEMENT_3D('',#66418,#34723,#34724);
#28784=AXIS2_PLACEMENT_3D('',#66419,#34725,#34726);
#28785=AXIS2_PLACEMENT_3D('',#66420,#34727,#34728);
#28786=AXIS2_PLACEMENT_3D('',#66426,#34732,#34733);
#28787=AXIS2_PLACEMENT_3D('',#66430,#34736,#34737);
#28788=AXIS2_PLACEMENT_3D('',#66431,#34738,#34739);
#28789=AXIS2_PLACEMENT_3D('',#66432,#34740,#34741);
#28790=AXIS2_PLACEMENT_3D('',#66438,#34745,#34746);
#28791=AXIS2_PLACEMENT_3D('',#66442,#34749,#34750);
#28792=AXIS2_PLACEMENT_3D('',#66443,#34751,#34752);
#28793=AXIS2_PLACEMENT_3D('',#66444,#34753,#34754);
#28794=AXIS2_PLACEMENT_3D('',#66450,#34758,#34759);
#28795=AXIS2_PLACEMENT_3D('',#66454,#34762,#34763);
#28796=AXIS2_PLACEMENT_3D('',#66455,#34764,#34765);
#28797=AXIS2_PLACEMENT_3D('',#66456,#34766,#34767);
#28798=AXIS2_PLACEMENT_3D('',#66462,#34771,#34772);
#28799=AXIS2_PLACEMENT_3D('',#66466,#34775,#34776);
#28800=AXIS2_PLACEMENT_3D('',#66467,#34777,#34778);
#28801=AXIS2_PLACEMENT_3D('',#66468,#34779,#34780);
#28802=AXIS2_PLACEMENT_3D('',#66474,#34784,#34785);
#28803=AXIS2_PLACEMENT_3D('',#66478,#34788,#34789);
#28804=AXIS2_PLACEMENT_3D('',#66479,#34790,#34791);
#28805=AXIS2_PLACEMENT_3D('',#66480,#34792,#34793);
#28806=AXIS2_PLACEMENT_3D('',#66486,#34797,#34798);
#28807=AXIS2_PLACEMENT_3D('',#66490,#34801,#34802);
#28808=AXIS2_PLACEMENT_3D('',#66491,#34803,#34804);
#28809=AXIS2_PLACEMENT_3D('',#66492,#34805,#34806);
#28810=AXIS2_PLACEMENT_3D('',#66498,#34810,#34811);
#28811=AXIS2_PLACEMENT_3D('',#66502,#34814,#34815);
#28812=AXIS2_PLACEMENT_3D('',#66503,#34816,#34817);
#28813=AXIS2_PLACEMENT_3D('',#66504,#34818,#34819);
#28814=AXIS2_PLACEMENT_3D('',#66510,#34823,#34824);
#28815=AXIS2_PLACEMENT_3D('',#66514,#34827,#34828);
#28816=AXIS2_PLACEMENT_3D('',#66515,#34829,#34830);
#28817=AXIS2_PLACEMENT_3D('',#66516,#34831,#34832);
#28818=AXIS2_PLACEMENT_3D('',#66522,#34836,#34837);
#28819=AXIS2_PLACEMENT_3D('',#66526,#34840,#34841);
#28820=AXIS2_PLACEMENT_3D('',#66527,#34842,#34843);
#28821=AXIS2_PLACEMENT_3D('',#66528,#34844,#34845);
#28822=AXIS2_PLACEMENT_3D('',#66534,#34849,#34850);
#28823=AXIS2_PLACEMENT_3D('',#66538,#34853,#34854);
#28824=AXIS2_PLACEMENT_3D('',#66539,#34855,#34856);
#28825=AXIS2_PLACEMENT_3D('',#66540,#34857,#34858);
#28826=AXIS2_PLACEMENT_3D('',#66546,#34862,#34863);
#28827=AXIS2_PLACEMENT_3D('',#66550,#34866,#34867);
#28828=AXIS2_PLACEMENT_3D('',#66551,#34868,#34869);
#28829=AXIS2_PLACEMENT_3D('',#66552,#34870,#34871);
#28830=AXIS2_PLACEMENT_3D('',#66558,#34875,#34876);
#28831=AXIS2_PLACEMENT_3D('',#66562,#34879,#34880);
#28832=AXIS2_PLACEMENT_3D('',#66564,#34881,#34882);
#28833=AXIS2_PLACEMENT_3D('',#66565,#34883,#34884);
#28834=AXIS2_PLACEMENT_3D('',#66566,#34885,#34886);
#28835=AXIS2_PLACEMENT_3D('',#66572,#34890,#34891);
#28836=AXIS2_PLACEMENT_3D('',#66576,#34894,#34895);
#28837=AXIS2_PLACEMENT_3D('',#66577,#34896,#34897);
#28838=AXIS2_PLACEMENT_3D('',#66578,#34898,#34899);
#28839=AXIS2_PLACEMENT_3D('',#66584,#34903,#34904);
#28840=AXIS2_PLACEMENT_3D('',#66588,#34907,#34908);
#28841=AXIS2_PLACEMENT_3D('',#66589,#34909,#34910);
#28842=AXIS2_PLACEMENT_3D('',#66590,#34911,#34912);
#28843=AXIS2_PLACEMENT_3D('',#66596,#34916,#34917);
#28844=AXIS2_PLACEMENT_3D('',#66600,#34920,#34921);
#28845=AXIS2_PLACEMENT_3D('',#66601,#34922,#34923);
#28846=AXIS2_PLACEMENT_3D('',#66602,#34924,#34925);
#28847=AXIS2_PLACEMENT_3D('',#66608,#34929,#34930);
#28848=AXIS2_PLACEMENT_3D('',#66612,#34933,#34934);
#28849=AXIS2_PLACEMENT_3D('',#66613,#34935,#34936);
#28850=AXIS2_PLACEMENT_3D('',#66614,#34937,#34938);
#28851=AXIS2_PLACEMENT_3D('',#66620,#34942,#34943);
#28852=AXIS2_PLACEMENT_3D('',#66624,#34946,#34947);
#28853=AXIS2_PLACEMENT_3D('',#66625,#34948,#34949);
#28854=AXIS2_PLACEMENT_3D('',#66626,#34950,#34951);
#28855=AXIS2_PLACEMENT_3D('',#66632,#34955,#34956);
#28856=AXIS2_PLACEMENT_3D('',#66636,#34959,#34960);
#28857=AXIS2_PLACEMENT_3D('',#66637,#34961,#34962);
#28858=AXIS2_PLACEMENT_3D('',#66638,#34963,#34964);
#28859=AXIS2_PLACEMENT_3D('',#66644,#34968,#34969);
#28860=AXIS2_PLACEMENT_3D('',#66648,#34972,#34973);
#28861=AXIS2_PLACEMENT_3D('',#66649,#34974,#34975);
#28862=AXIS2_PLACEMENT_3D('',#66650,#34976,#34977);
#28863=AXIS2_PLACEMENT_3D('',#66656,#34981,#34982);
#28864=AXIS2_PLACEMENT_3D('',#66660,#34985,#34986);
#28865=AXIS2_PLACEMENT_3D('',#66661,#34987,#34988);
#28866=AXIS2_PLACEMENT_3D('',#66662,#34989,#34990);
#28867=AXIS2_PLACEMENT_3D('',#66668,#34994,#34995);
#28868=AXIS2_PLACEMENT_3D('',#66672,#34998,#34999);
#28869=AXIS2_PLACEMENT_3D('',#66673,#35000,#35001);
#28870=AXIS2_PLACEMENT_3D('',#66674,#35002,#35003);
#28871=AXIS2_PLACEMENT_3D('',#66680,#35007,#35008);
#28872=AXIS2_PLACEMENT_3D('',#66684,#35011,#35012);
#28873=AXIS2_PLACEMENT_3D('',#66685,#35013,#35014);
#28874=AXIS2_PLACEMENT_3D('',#66686,#35015,#35016);
#28875=AXIS2_PLACEMENT_3D('',#66692,#35020,#35021);
#28876=AXIS2_PLACEMENT_3D('',#66696,#35024,#35025);
#28877=AXIS2_PLACEMENT_3D('',#66697,#35026,#35027);
#28878=AXIS2_PLACEMENT_3D('',#66698,#35028,#35029);
#28879=AXIS2_PLACEMENT_3D('',#66704,#35033,#35034);
#28880=AXIS2_PLACEMENT_3D('',#66708,#35037,#35038);
#28881=AXIS2_PLACEMENT_3D('',#66709,#35039,#35040);
#28882=AXIS2_PLACEMENT_3D('',#66710,#35041,#35042);
#28883=AXIS2_PLACEMENT_3D('',#66716,#35046,#35047);
#28884=AXIS2_PLACEMENT_3D('',#66720,#35050,#35051);
#28885=AXIS2_PLACEMENT_3D('',#66721,#35052,#35053);
#28886=AXIS2_PLACEMENT_3D('',#66722,#35054,#35055);
#28887=AXIS2_PLACEMENT_3D('',#66728,#35059,#35060);
#28888=AXIS2_PLACEMENT_3D('',#66732,#35063,#35064);
#28889=AXIS2_PLACEMENT_3D('',#66733,#35065,#35066);
#28890=AXIS2_PLACEMENT_3D('',#66734,#35067,#35068);
#28891=AXIS2_PLACEMENT_3D('',#66740,#35072,#35073);
#28892=AXIS2_PLACEMENT_3D('',#66744,#35076,#35077);
#28893=AXIS2_PLACEMENT_3D('',#66745,#35078,#35079);
#28894=AXIS2_PLACEMENT_3D('',#66746,#35080,#35081);
#28895=AXIS2_PLACEMENT_3D('',#66752,#35085,#35086);
#28896=AXIS2_PLACEMENT_3D('',#66756,#35089,#35090);
#28897=AXIS2_PLACEMENT_3D('',#66757,#35091,#35092);
#28898=AXIS2_PLACEMENT_3D('',#66758,#35093,#35094);
#28899=AXIS2_PLACEMENT_3D('',#66764,#35098,#35099);
#28900=AXIS2_PLACEMENT_3D('',#66768,#35102,#35103);
#28901=AXIS2_PLACEMENT_3D('',#66769,#35104,#35105);
#28902=AXIS2_PLACEMENT_3D('',#66770,#35106,#35107);
#28903=AXIS2_PLACEMENT_3D('',#66776,#35111,#35112);
#28904=AXIS2_PLACEMENT_3D('',#66780,#35115,#35116);
#28905=AXIS2_PLACEMENT_3D('',#66781,#35117,#35118);
#28906=AXIS2_PLACEMENT_3D('',#66782,#35119,#35120);
#28907=AXIS2_PLACEMENT_3D('',#66784,#35122,#35123);
#28908=AXIS2_PLACEMENT_3D('',#66797,#35130,#35131);
#28909=AXIS2_PLACEMENT_3D('',#66801,#35133,#35134);
#28910=AXIS2_PLACEMENT_3D('',#66802,#35135,#35136);
#28911=AXIS2_PLACEMENT_3D('',#66805,#35138,#35139);
#28912=AXIS2_PLACEMENT_3D('',#66806,#35140,#35141);
#28913=AXIS2_PLACEMENT_3D('',#66809,#35143,#35144);
#28914=AXIS2_PLACEMENT_3D('',#66810,#35145,#35146);
#28915=AXIS2_PLACEMENT_3D('',#66813,#35148,#35149);
#28916=AXIS2_PLACEMENT_3D('',#66814,#35150,#35151);
#28917=AXIS2_PLACEMENT_3D('',#66817,#35153,#35154);
#28918=AXIS2_PLACEMENT_3D('',#66818,#35155,#35156);
#28919=AXIS2_PLACEMENT_3D('',#66820,#35158,#35159);
#28920=AXIS2_PLACEMENT_3D('',#66821,#35160,#35161);
#28921=AXIS2_PLACEMENT_3D('',#66824,#35163,#35164);
#28922=AXIS2_PLACEMENT_3D('',#66827,#35167,#35168);
#28923=AXIS2_PLACEMENT_3D('',#66829,#35170,#35171);
#28924=AXIS2_PLACEMENT_3D('',#66831,#35173,#35174);
#28925=AXIS2_PLACEMENT_3D('',#66833,#35176,#35177);
#28926=AXIS2_PLACEMENT_3D('',#66835,#35179,#35180);
#28927=AXIS2_PLACEMENT_3D('',#66836,#35181,#35182);
#28928=AXIS2_PLACEMENT_3D('',#66837,#35183,#35184);
#28929=AXIS2_PLACEMENT_3D('',#66993,#35186,#35187);
#28930=AXIS2_PLACEMENT_3D('',#67096,#35188,#35189);
#28931=AXIS2_PLACEMENT_3D('',#67514,#35191,#35192);
#28932=AXIS2_PLACEMENT_3D('',#67782,#35194,#35195);
#28933=AXIS2_PLACEMENT_3D('',#68178,#35197,#35198);
#28934=AXIS2_PLACEMENT_3D('',#68614,#35200,#35201);
#28935=AXIS2_PLACEMENT_3D('',#69036,#35203,#35204);
#28936=AXIS2_PLACEMENT_3D('',#69470,#35206,#35207);
#28937=AXIS2_PLACEMENT_3D('',#69902,#35209,#35210);
#28938=AXIS2_PLACEMENT_3D('',#70145,#35212,#35213);
#28939=AXIS2_PLACEMENT_3D('',#70517,#35215,#35216);
#28940=AXIS2_PLACEMENT_3D('',#70784,#35218,#35219);
#28941=AXIS2_PLACEMENT_3D('',#71230,#35221,#35222);
#28942=AXIS2_PLACEMENT_3D('',#71649,#35224,#35225);
#28943=AXIS2_PLACEMENT_3D('',#72064,#35227,#35228);
#28944=AXIS2_PLACEMENT_3D('',#72501,#35230,#35231);
#28945=AXIS2_PLACEMENT_3D('',#72911,#35233,#35234);
#28946=AXIS2_PLACEMENT_3D('',#73166,#35236,#35237);
#28947=AXIS2_PLACEMENT_3D('',#73534,#35239,#35240);
#28948=AXIS2_PLACEMENT_3D('',#73945,#35242,#35243);
#28949=AXIS2_PLACEMENT_3D('',#74010,#35244,#35245);
#28950=AXIS2_PLACEMENT_3D('',#77370,#35246,#35247);
#28951=AXIS2_PLACEMENT_3D('',#80497,#35248,#35249);
#28952=AXIS2_PLACEMENT_3D('',#80684,#35250,#35251);
#28953=AXIS2_PLACEMENT_3D('',#80819,#35252,#35253);
#28954=AXIS2_PLACEMENT_3D('',#80822,#35254,#35255);
#28955=AXIS2_PLACEMENT_3D('',#80983,#35256,#35257);
#28956=AXIS2_PLACEMENT_3D('',#81580,#35258,#35259);
#28957=AXIS2_PLACEMENT_3D('',#81583,#35260,#35261);
#28958=AXIS2_PLACEMENT_3D('',#81660,#35262,#35263);
#28959=AXIS2_PLACEMENT_3D('',#82173,#35264,#35265);
#28960=AXIS2_PLACEMENT_3D('',#82175,#35266,#35267);
#28961=AXIS2_PLACEMENT_3D('',#82176,#35268,#35269);
#28962=AXIS2_PLACEMENT_3D('',#82177,#35270,#35271);
#28963=AXIS2_PLACEMENT_3D('',#82179,#35272,#35273);
#28964=AXIS2_PLACEMENT_3D('',#82180,#35274,#35275);
#28965=AXIS2_PLACEMENT_3D('',#82183,#35277,#35278);
#28966=AXIS2_PLACEMENT_3D('',#82184,#35279,#35280);
#28967=AXIS2_PLACEMENT_3D('',#82185,#35281,#35282);
#28968=AXIS2_PLACEMENT_3D('',#82196,#35286,#35287);
#28969=AXIS2_PLACEMENT_3D('',#82204,#35290,#35291);
#28970=AXIS2_PLACEMENT_3D('',#82205,#35292,#35293);
#28971=AXIS2_PLACEMENT_3D('',#82206,#35294,#35295);
#28972=AXIS2_PLACEMENT_3D('',#82213,#35296,#35297);
#28973=AXIS2_PLACEMENT_3D('',#82223,#35298,#35299);
#28974=AXIS2_PLACEMENT_3D('',#82233,#35300,#35301);
#28975=AXIS2_PLACEMENT_3D('',#82243,#35302,#35303);
#28976=AXIS2_PLACEMENT_3D('',#82253,#35304,#35305);
#28977=AXIS2_PLACEMENT_3D('',#82263,#35306,#35307);
#28978=AXIS2_PLACEMENT_3D('',#82273,#35308,#35309);
#28979=AXIS2_PLACEMENT_3D('',#82283,#35310,#35311);
#28980=AXIS2_PLACEMENT_3D('',#82293,#35312,#35313);
#28981=AXIS2_PLACEMENT_3D('',#82303,#35314,#35315);
#28982=AXIS2_PLACEMENT_3D('',#82313,#35316,#35317);
#28983=AXIS2_PLACEMENT_3D('',#82323,#35318,#35319);
#28984=AXIS2_PLACEMENT_3D('',#82333,#35320,#35321);
#28985=AXIS2_PLACEMENT_3D('',#82343,#35322,#35323);
#28986=AXIS2_PLACEMENT_3D('',#82353,#35324,#35325);
#28987=AXIS2_PLACEMENT_3D('',#82363,#35326,#35327);
#28988=AXIS2_PLACEMENT_3D('',#82373,#35328,#35329);
#28989=AXIS2_PLACEMENT_3D('',#82383,#35330,#35331);
#28990=AXIS2_PLACEMENT_3D('',#82392,#35332,#35333);
#28991=AXIS2_PLACEMENT_3D('',#82394,#35334,#35335);
#28992=AXIS2_PLACEMENT_3D('',#82404,#35336,#35337);
#28993=AXIS2_PLACEMENT_3D('',#82414,#35338,#35339);
#28994=AXIS2_PLACEMENT_3D('',#82424,#35340,#35341);
#28995=AXIS2_PLACEMENT_3D('',#82434,#35342,#35343);
#28996=AXIS2_PLACEMENT_3D('',#82444,#35344,#35345);
#28997=AXIS2_PLACEMENT_3D('',#82454,#35346,#35347);
#28998=AXIS2_PLACEMENT_3D('',#82464,#35348,#35349);
#28999=AXIS2_PLACEMENT_3D('',#82474,#35350,#35351);
#29000=AXIS2_PLACEMENT_3D('',#82484,#35352,#35353);
#29001=AXIS2_PLACEMENT_3D('',#82494,#35354,#35355);
#29002=AXIS2_PLACEMENT_3D('',#82504,#35356,#35357);
#29003=AXIS2_PLACEMENT_3D('',#82514,#35358,#35359);
#29004=AXIS2_PLACEMENT_3D('',#82524,#35360,#35361);
#29005=AXIS2_PLACEMENT_3D('',#82534,#35362,#35363);
#29006=AXIS2_PLACEMENT_3D('',#82544,#35364,#35365);
#29007=AXIS2_PLACEMENT_3D('',#82554,#35366,#35367);
#29008=AXIS2_PLACEMENT_3D('',#82560,#35369,#35370);
#29009=AXIS2_PLACEMENT_3D('',#82561,#35371,#35372);
#29010=AXIS2_PLACEMENT_3D('',#82567,#35376,#35377);
#29011=AXIS2_PLACEMENT_3D('',#82571,#35380,#35381);
#29012=AXIS2_PLACEMENT_3D('',#82572,#35382,#35383);
#29013=AXIS2_PLACEMENT_3D('',#82573,#35384,#35385);
#29014=AXIS2_PLACEMENT_3D('',#82579,#35389,#35390);
#29015=AXIS2_PLACEMENT_3D('',#82583,#35393,#35394);
#29016=AXIS2_PLACEMENT_3D('',#82584,#35395,#35396);
#29017=AXIS2_PLACEMENT_3D('',#82585,#35397,#35398);
#29018=AXIS2_PLACEMENT_3D('',#82591,#35402,#35403);
#29019=AXIS2_PLACEMENT_3D('',#82595,#35406,#35407);
#29020=AXIS2_PLACEMENT_3D('',#82596,#35408,#35409);
#29021=AXIS2_PLACEMENT_3D('',#82597,#35410,#35411);
#29022=AXIS2_PLACEMENT_3D('',#82603,#35415,#35416);
#29023=AXIS2_PLACEMENT_3D('',#82607,#35419,#35420);
#29024=AXIS2_PLACEMENT_3D('',#82608,#35421,#35422);
#29025=AXIS2_PLACEMENT_3D('',#82609,#35423,#35424);
#29026=AXIS2_PLACEMENT_3D('',#82615,#35428,#35429);
#29027=AXIS2_PLACEMENT_3D('',#82619,#35432,#35433);
#29028=AXIS2_PLACEMENT_3D('',#82620,#35434,#35435);
#29029=AXIS2_PLACEMENT_3D('',#82621,#35436,#35437);
#29030=AXIS2_PLACEMENT_3D('',#82627,#35441,#35442);
#29031=AXIS2_PLACEMENT_3D('',#82631,#35445,#35446);
#29032=AXIS2_PLACEMENT_3D('',#82632,#35447,#35448);
#29033=AXIS2_PLACEMENT_3D('',#82633,#35449,#35450);
#29034=AXIS2_PLACEMENT_3D('',#82639,#35454,#35455);
#29035=AXIS2_PLACEMENT_3D('',#82643,#35458,#35459);
#29036=AXIS2_PLACEMENT_3D('',#82644,#35460,#35461);
#29037=AXIS2_PLACEMENT_3D('',#82645,#35462,#35463);
#29038=AXIS2_PLACEMENT_3D('',#82651,#35467,#35468);
#29039=AXIS2_PLACEMENT_3D('',#82655,#35471,#35472);
#29040=AXIS2_PLACEMENT_3D('',#82656,#35473,#35474);
#29041=AXIS2_PLACEMENT_3D('',#82657,#35475,#35476);
#29042=AXIS2_PLACEMENT_3D('',#82663,#35480,#35481);
#29043=AXIS2_PLACEMENT_3D('',#82667,#35484,#35485);
#29044=AXIS2_PLACEMENT_3D('',#82668,#35486,#35487);
#29045=AXIS2_PLACEMENT_3D('',#82669,#35488,#35489);
#29046=AXIS2_PLACEMENT_3D('',#82675,#35493,#35494);
#29047=AXIS2_PLACEMENT_3D('',#82679,#35497,#35498);
#29048=AXIS2_PLACEMENT_3D('',#82680,#35499,#35500);
#29049=AXIS2_PLACEMENT_3D('',#82681,#35501,#35502);
#29050=AXIS2_PLACEMENT_3D('',#82687,#35506,#35507);
#29051=AXIS2_PLACEMENT_3D('',#82691,#35510,#35511);
#29052=AXIS2_PLACEMENT_3D('',#82692,#35512,#35513);
#29053=AXIS2_PLACEMENT_3D('',#82693,#35514,#35515);
#29054=AXIS2_PLACEMENT_3D('',#82699,#35519,#35520);
#29055=AXIS2_PLACEMENT_3D('',#82703,#35523,#35524);
#29056=AXIS2_PLACEMENT_3D('',#82704,#35525,#35526);
#29057=AXIS2_PLACEMENT_3D('',#82705,#35527,#35528);
#29058=AXIS2_PLACEMENT_3D('',#82711,#35532,#35533);
#29059=AXIS2_PLACEMENT_3D('',#82715,#35536,#35537);
#29060=AXIS2_PLACEMENT_3D('',#82716,#35538,#35539);
#29061=AXIS2_PLACEMENT_3D('',#82717,#35540,#35541);
#29062=AXIS2_PLACEMENT_3D('',#82723,#35545,#35546);
#29063=AXIS2_PLACEMENT_3D('',#82727,#35549,#35550);
#29064=AXIS2_PLACEMENT_3D('',#82728,#35551,#35552);
#29065=AXIS2_PLACEMENT_3D('',#82729,#35553,#35554);
#29066=AXIS2_PLACEMENT_3D('',#82735,#35558,#35559);
#29067=AXIS2_PLACEMENT_3D('',#82739,#35562,#35563);
#29068=AXIS2_PLACEMENT_3D('',#82740,#35564,#35565);
#29069=AXIS2_PLACEMENT_3D('',#82741,#35566,#35567);
#29070=AXIS2_PLACEMENT_3D('',#82747,#35571,#35572);
#29071=AXIS2_PLACEMENT_3D('',#82751,#35575,#35576);
#29072=AXIS2_PLACEMENT_3D('',#82752,#35577,#35578);
#29073=AXIS2_PLACEMENT_3D('',#82753,#35579,#35580);
#29074=AXIS2_PLACEMENT_3D('',#82759,#35584,#35585);
#29075=AXIS2_PLACEMENT_3D('',#82763,#35588,#35589);
#29076=AXIS2_PLACEMENT_3D('',#82765,#35590,#35591);
#29077=AXIS2_PLACEMENT_3D('',#82766,#35592,#35593);
#29078=AXIS2_PLACEMENT_3D('',#82767,#35594,#35595);
#29079=AXIS2_PLACEMENT_3D('',#82773,#35599,#35600);
#29080=AXIS2_PLACEMENT_3D('',#82777,#35603,#35604);
#29081=AXIS2_PLACEMENT_3D('',#82778,#35605,#35606);
#29082=AXIS2_PLACEMENT_3D('',#82779,#35607,#35608);
#29083=AXIS2_PLACEMENT_3D('',#82785,#35612,#35613);
#29084=AXIS2_PLACEMENT_3D('',#82789,#35616,#35617);
#29085=AXIS2_PLACEMENT_3D('',#82790,#35618,#35619);
#29086=AXIS2_PLACEMENT_3D('',#82791,#35620,#35621);
#29087=AXIS2_PLACEMENT_3D('',#82797,#35625,#35626);
#29088=AXIS2_PLACEMENT_3D('',#82801,#35629,#35630);
#29089=AXIS2_PLACEMENT_3D('',#82802,#35631,#35632);
#29090=AXIS2_PLACEMENT_3D('',#82803,#35633,#35634);
#29091=AXIS2_PLACEMENT_3D('',#82809,#35638,#35639);
#29092=AXIS2_PLACEMENT_3D('',#82813,#35642,#35643);
#29093=AXIS2_PLACEMENT_3D('',#82814,#35644,#35645);
#29094=AXIS2_PLACEMENT_3D('',#82815,#35646,#35647);
#29095=AXIS2_PLACEMENT_3D('',#82821,#35651,#35652);
#29096=AXIS2_PLACEMENT_3D('',#82825,#35655,#35656);
#29097=AXIS2_PLACEMENT_3D('',#82826,#35657,#35658);
#29098=AXIS2_PLACEMENT_3D('',#82827,#35659,#35660);
#29099=AXIS2_PLACEMENT_3D('',#82833,#35664,#35665);
#29100=AXIS2_PLACEMENT_3D('',#82837,#35668,#35669);
#29101=AXIS2_PLACEMENT_3D('',#82838,#35670,#35671);
#29102=AXIS2_PLACEMENT_3D('',#82839,#35672,#35673);
#29103=AXIS2_PLACEMENT_3D('',#82845,#35677,#35678);
#29104=AXIS2_PLACEMENT_3D('',#82849,#35681,#35682);
#29105=AXIS2_PLACEMENT_3D('',#82850,#35683,#35684);
#29106=AXIS2_PLACEMENT_3D('',#82851,#35685,#35686);
#29107=AXIS2_PLACEMENT_3D('',#82857,#35690,#35691);
#29108=AXIS2_PLACEMENT_3D('',#82861,#35694,#35695);
#29109=AXIS2_PLACEMENT_3D('',#82862,#35696,#35697);
#29110=AXIS2_PLACEMENT_3D('',#82863,#35698,#35699);
#29111=AXIS2_PLACEMENT_3D('',#82869,#35703,#35704);
#29112=AXIS2_PLACEMENT_3D('',#82873,#35707,#35708);
#29113=AXIS2_PLACEMENT_3D('',#82874,#35709,#35710);
#29114=AXIS2_PLACEMENT_3D('',#82875,#35711,#35712);
#29115=AXIS2_PLACEMENT_3D('',#82881,#35716,#35717);
#29116=AXIS2_PLACEMENT_3D('',#82885,#35720,#35721);
#29117=AXIS2_PLACEMENT_3D('',#82886,#35722,#35723);
#29118=AXIS2_PLACEMENT_3D('',#82887,#35724,#35725);
#29119=AXIS2_PLACEMENT_3D('',#82893,#35729,#35730);
#29120=AXIS2_PLACEMENT_3D('',#82897,#35733,#35734);
#29121=AXIS2_PLACEMENT_3D('',#82898,#35735,#35736);
#29122=AXIS2_PLACEMENT_3D('',#82899,#35737,#35738);
#29123=AXIS2_PLACEMENT_3D('',#82905,#35742,#35743);
#29124=AXIS2_PLACEMENT_3D('',#82909,#35746,#35747);
#29125=AXIS2_PLACEMENT_3D('',#82910,#35748,#35749);
#29126=AXIS2_PLACEMENT_3D('',#82911,#35750,#35751);
#29127=AXIS2_PLACEMENT_3D('',#82917,#35755,#35756);
#29128=AXIS2_PLACEMENT_3D('',#82921,#35759,#35760);
#29129=AXIS2_PLACEMENT_3D('',#82922,#35761,#35762);
#29130=AXIS2_PLACEMENT_3D('',#82923,#35763,#35764);
#29131=AXIS2_PLACEMENT_3D('',#82929,#35768,#35769);
#29132=AXIS2_PLACEMENT_3D('',#82933,#35772,#35773);
#29133=AXIS2_PLACEMENT_3D('',#82934,#35774,#35775);
#29134=AXIS2_PLACEMENT_3D('',#82935,#35776,#35777);
#29135=AXIS2_PLACEMENT_3D('',#82941,#35781,#35782);
#29136=AXIS2_PLACEMENT_3D('',#82945,#35785,#35786);
#29137=AXIS2_PLACEMENT_3D('',#82946,#35787,#35788);
#29138=AXIS2_PLACEMENT_3D('',#82947,#35789,#35790);
#29139=AXIS2_PLACEMENT_3D('',#82953,#35794,#35795);
#29140=AXIS2_PLACEMENT_3D('',#82957,#35798,#35799);
#29141=AXIS2_PLACEMENT_3D('',#82958,#35800,#35801);
#29142=AXIS2_PLACEMENT_3D('',#82959,#35802,#35803);
#29143=AXIS2_PLACEMENT_3D('',#82965,#35807,#35808);
#29144=AXIS2_PLACEMENT_3D('',#82969,#35811,#35812);
#29145=AXIS2_PLACEMENT_3D('',#82970,#35813,#35814);
#29146=AXIS2_PLACEMENT_3D('',#82971,#35815,#35816);
#29147=AXIS2_PLACEMENT_3D('',#82977,#35820,#35821);
#29148=AXIS2_PLACEMENT_3D('',#82981,#35824,#35825);
#29149=AXIS2_PLACEMENT_3D('',#82982,#35826,#35827);
#29150=AXIS2_PLACEMENT_3D('',#82983,#35828,#35829);
#29151=AXIS2_PLACEMENT_3D('',#82985,#35831,#35832);
#29152=AXIS2_PLACEMENT_3D('',#82998,#35839,#35840);
#29153=AXIS2_PLACEMENT_3D('',#83002,#35842,#35843);
#29154=AXIS2_PLACEMENT_3D('',#83003,#35844,#35845);
#29155=AXIS2_PLACEMENT_3D('',#83006,#35847,#35848);
#29156=AXIS2_PLACEMENT_3D('',#83007,#35849,#35850);
#29157=AXIS2_PLACEMENT_3D('',#83010,#35852,#35853);
#29158=AXIS2_PLACEMENT_3D('',#83011,#35854,#35855);
#29159=AXIS2_PLACEMENT_3D('',#83014,#35857,#35858);
#29160=AXIS2_PLACEMENT_3D('',#83015,#35859,#35860);
#29161=AXIS2_PLACEMENT_3D('',#83018,#35862,#35863);
#29162=AXIS2_PLACEMENT_3D('',#83019,#35864,#35865);
#29163=AXIS2_PLACEMENT_3D('',#83021,#35867,#35868);
#29164=AXIS2_PLACEMENT_3D('',#83022,#35869,#35870);
#29165=AXIS2_PLACEMENT_3D('',#83025,#35872,#35873);
#29166=AXIS2_PLACEMENT_3D('',#83028,#35876,#35877);
#29167=AXIS2_PLACEMENT_3D('',#83030,#35879,#35880);
#29168=AXIS2_PLACEMENT_3D('',#83032,#35882,#35883);
#29169=AXIS2_PLACEMENT_3D('',#83034,#35885,#35886);
#29170=AXIS2_PLACEMENT_3D('',#83036,#35888,#35889);
#29171=AXIS2_PLACEMENT_3D('',#83037,#35890,#35891);
#29172=AXIS2_PLACEMENT_3D('',#83038,#35892,#35893);
#29173=AXIS2_PLACEMENT_3D('',#83040,#35894,#35895);
#29174=AXIS2_PLACEMENT_3D('',#83043,#35897,#35898);
#29175=AXIS2_PLACEMENT_3D('',#83044,#35899,#35900);
#29176=AXIS2_PLACEMENT_3D('',#83046,#35901,#35902);
#29177=AXIS2_PLACEMENT_3D('',#83047,#35903,#35904);
#29178=AXIS2_PLACEMENT_3D('',#83049,#35905,#35906);
#29179=AXIS2_PLACEMENT_3D('',#83051,#35908,#35909);
#29180=AXIS2_PLACEMENT_3D('',#83054,#35911,#35912);
#29181=AXIS2_PLACEMENT_3D('',#83055,#35913,#35914);
#29182=AXIS2_PLACEMENT_3D('',#83057,#35915,#35916);
#29183=AXIS2_PLACEMENT_3D('',#83058,#35917,#35918);
#29184=AXIS2_PLACEMENT_3D('',#83060,#35920,#35921);
#29185=AXIS2_PLACEMENT_3D('',#83061,#35922,#35923);
#29186=AXIS2_PLACEMENT_3D('',#83063,#35924,#35925);
#29187=AXIS2_PLACEMENT_3D('',#83066,#35927,#35928);
#29188=AXIS2_PLACEMENT_3D('',#83067,#35929,#35930);
#29189=AXIS2_PLACEMENT_3D('',#83070,#35932,#35933);
#29190=AXIS2_PLACEMENT_3D('',#83071,#35934,#35935);
#29191=AXIS2_PLACEMENT_3D('',#83073,#35936,#35937);
#29192=AXIS2_PLACEMENT_3D('',#83074,#35938,#35939);
#29193=AXIS2_PLACEMENT_3D('',#83076,#35940,#35941);
#29194=AXIS2_PLACEMENT_3D('',#83079,#35943,#35944);
#29195=AXIS2_PLACEMENT_3D('',#83080,#35945,#35946);
#29196=AXIS2_PLACEMENT_3D('',#83083,#35948,#35949);
#29197=AXIS2_PLACEMENT_3D('',#83084,#35950,#35951);
#29198=AXIS2_PLACEMENT_3D('',#83086,#35952,#35953);
#29199=AXIS2_PLACEMENT_3D('',#83087,#35954,#35955);
#29200=AXIS2_PLACEMENT_3D('',#83089,#35956,#35957);
#29201=AXIS2_PLACEMENT_3D('',#83091,#35959,#35960);
#29202=AXIS2_PLACEMENT_3D('',#83092,#35961,#35962);
#29203=AXIS2_PLACEMENT_3D('',#83118,#35964,#35965);
#29204=AXIS2_PLACEMENT_3D('',#83124,#35969,#35970);
#29205=AXIS2_PLACEMENT_3D('',#83128,#35973,#35974);
#29206=AXIS2_PLACEMENT_3D('',#83132,#35977,#35978);
#29207=AXIS2_PLACEMENT_3D('',#83136,#35981,#35982);
#29208=AXIS2_PLACEMENT_3D('',#83140,#35985,#35986);
#29209=AXIS2_PLACEMENT_3D('',#83142,#35988,#35989);
#29210=AXIS2_PLACEMENT_3D('',#83143,#35990,#35991);
#29211=AXIS2_PLACEMENT_3D('',#83144,#35992,#35993);
#29212=AXIS2_PLACEMENT_3D('',#83145,#35994,#35995);
#29213=AXIS2_PLACEMENT_3D('',#83146,#35996,#35997);
#29214=AXIS2_PLACEMENT_3D('',#83147,#35998,#35999);
#29215=AXIS2_PLACEMENT_3D('',#83148,#36000,#36001);
#29216=AXIS2_PLACEMENT_3D('',#83149,#36002,#36003);
#29217=AXIS2_PLACEMENT_3D('',#83150,#36004,#36005);
#29218=AXIS2_PLACEMENT_3D('',#83151,#36006,#36007);
#29219=AXIS2_PLACEMENT_3D('',#83152,#36008,#36009);
#29220=AXIS2_PLACEMENT_3D('',#83153,#36010,#36011);
#29221=AXIS2_PLACEMENT_3D('',#83154,#36012,#36013);
#29222=AXIS2_PLACEMENT_3D('',#83155,#36014,#36015);
#29223=AXIS2_PLACEMENT_3D('',#83156,#36016,#36017);
#29224=AXIS2_PLACEMENT_3D('',#83157,#36018,#36019);
#29225=AXIS2_PLACEMENT_3D('',#83158,#36020,#36021);
#29226=AXIS2_PLACEMENT_3D('',#83159,#36022,#36023);
#29227=AXIS2_PLACEMENT_3D('',#83160,#36024,#36025);
#29228=AXIS2_PLACEMENT_3D('',#83161,#36026,#36027);
#29229=AXIS2_PLACEMENT_3D('',#83162,#36028,#36029);
#29230=AXIS2_PLACEMENT_3D('',#83163,#36030,#36031);
#29231=AXIS2_PLACEMENT_3D('',#83164,#36032,#36033);
#29232=AXIS2_PLACEMENT_3D('',#83165,#36034,#36035);
#29233=AXIS2_PLACEMENT_3D('',#83166,#36036,#36037);
#29234=AXIS2_PLACEMENT_3D('',#83167,#36038,#36039);
#29235=AXIS2_PLACEMENT_3D('',#83168,#36040,#36041);
#29236=AXIS2_PLACEMENT_3D('',#83169,#36042,#36043);
#29237=AXIS2_PLACEMENT_3D('',#83170,#36044,#36045);
#29238=AXIS2_PLACEMENT_3D('',#83171,#36046,#36047);
#29239=AXIS2_PLACEMENT_3D('',#83172,#36048,#36049);
#29240=AXIS2_PLACEMENT_3D('',#83173,#36050,#36051);
#29241=AXIS2_PLACEMENT_3D('',#83174,#36052,#36053);
#29242=AXIS2_PLACEMENT_3D('',#83175,#36054,#36055);
#29243=AXIS2_PLACEMENT_3D('',#83176,#36056,#36057);
#29244=AXIS2_PLACEMENT_3D('',#83177,#36058,#36059);
#29245=AXIS2_PLACEMENT_3D('',#83178,#36060,#36061);
#29246=AXIS2_PLACEMENT_3D('',#83179,#36062,#36063);
#29247=AXIS2_PLACEMENT_3D('',#83180,#36064,#36065);
#29248=AXIS2_PLACEMENT_3D('',#83181,#36066,#36067);
#29249=AXIS2_PLACEMENT_3D('',#83182,#36068,#36069);
#29250=AXIS2_PLACEMENT_3D('',#83183,#36070,#36071);
#29251=AXIS2_PLACEMENT_3D('',#83184,#36072,#36073);
#29252=AXIS2_PLACEMENT_3D('',#83185,#36074,#36075);
#29253=AXIS2_PLACEMENT_3D('',#83186,#36076,#36077);
#29254=AXIS2_PLACEMENT_3D('',#83187,#36078,#36079);
#29255=DIRECTION('axis',(0.,0.,1.));
#29256=DIRECTION('refdir',(1.,0.,0.));
#29257=DIRECTION('axis',(0.,0.,1.));
#29258=DIRECTION('refdir',(1.,0.,0.));
#29259=DIRECTION('center_axis',(-1.,0.,0.));
#29260=DIRECTION('ref_axis',(0.,0.,-1.));
#29261=DIRECTION('center_axis',(1.,0.,0.));
#29262=DIRECTION('ref_axis',(0.,0.,-1.));
#29263=DIRECTION('',(-0.707106781186548,8.65956056235493E-17,0.707106781186547));
#29264=DIRECTION('center_axis',(-1.,0.,0.));
#29265=DIRECTION('ref_axis',(0.,0.,-1.));
#29266=DIRECTION('center_axis',(1.,0.,0.));
#29267=DIRECTION('ref_axis',(0.,0.,-1.));
#29268=DIRECTION('',(1.,0.,0.));
#29269=DIRECTION('center_axis',(1.,0.,0.));
#29270=DIRECTION('ref_axis',(0.,0.,-1.));
#29271=DIRECTION('center_axis',(1.,0.,0.));
#29272=DIRECTION('ref_axis',(0.,0.,-1.));
#29273=DIRECTION('center_axis',(-1.,0.,0.));
#29274=DIRECTION('ref_axis',(0.,0.,1.));
#29275=DIRECTION('',(0.,0.,1.));
#29276=DIRECTION('',(0.,1.,0.));
#29277=DIRECTION('',(0.,0.,-1.));
#29278=DIRECTION('',(0.,1.,0.));
#29279=DIRECTION('center_axis',(-1.,0.,0.));
#29280=DIRECTION('ref_axis',(0.,0.,-1.));
#29281=DIRECTION('center_axis',(1.,0.,0.));
#29282=DIRECTION('ref_axis',(0.,0.,-1.));
#29283=DIRECTION('',(-0.707106781186548,8.65956056235493E-17,0.707106781186547));
#29284=DIRECTION('center_axis',(-1.,0.,0.));
#29285=DIRECTION('ref_axis',(0.,0.,-1.));
#29286=DIRECTION('center_axis',(1.,0.,0.));
#29287=DIRECTION('ref_axis',(0.,0.,-1.));
#29288=DIRECTION('',(1.,0.,0.));
#29289=DIRECTION('center_axis',(1.,0.,0.));
#29290=DIRECTION('ref_axis',(0.,0.,-1.));
#29291=DIRECTION('center_axis',(1.,0.,0.));
#29292=DIRECTION('ref_axis',(0.,0.,-1.));
#29293=DIRECTION('center_axis',(-1.,0.,0.));
#29294=DIRECTION('ref_axis',(0.,0.,1.));
#29295=DIRECTION('',(0.,0.,1.));
#29296=DIRECTION('',(0.,-1.,0.));
#29297=DIRECTION('',(0.,0.,-1.));
#29298=DIRECTION('',(0.,1.,0.));
#29299=DIRECTION('center_axis',(-1.,0.,0.));
#29300=DIRECTION('ref_axis',(0.,1.,0.));
#29301=DIRECTION('',(-0.515038074910058,-0.85716730070211,1.04972719113862E-16));
#29302=DIRECTION('center_axis',(-1.,0.,0.));
#29303=DIRECTION('ref_axis',(0.,1.,0.));
#29304=DIRECTION('',(-0.515038074910058,-0.85716730070211,1.04972719113862E-16));
#29305=DIRECTION('center_axis',(1.,0.,0.));
#29306=DIRECTION('ref_axis',(0.,0.,-1.));
#29307=DIRECTION('center_axis',(-1.,0.,0.));
#29308=DIRECTION('ref_axis',(0.,0.,-1.));
#29309=DIRECTION('',(0.707106781186548,-8.65956056235493E-17,0.707106781186547));
#29310=DIRECTION('center_axis',(1.,0.,0.));
#29311=DIRECTION('ref_axis',(0.,0.,-1.));
#29312=DIRECTION('center_axis',(-1.,0.,0.));
#29313=DIRECTION('ref_axis',(0.,0.,-1.));
#29314=DIRECTION('',(-1.,0.,0.));
#29315=DIRECTION('center_axis',(-1.,0.,0.));
#29316=DIRECTION('ref_axis',(0.,0.,-1.));
#29317=DIRECTION('center_axis',(-1.,0.,0.));
#29318=DIRECTION('ref_axis',(0.,0.,-1.));
#29319=DIRECTION('center_axis',(1.,0.,0.));
#29320=DIRECTION('ref_axis',(0.,0.,-1.));
#29321=DIRECTION('',(0.,0.,-1.));
#29322=DIRECTION('',(0.,-1.,0.));
#29323=DIRECTION('',(0.,0.,1.));
#29324=DIRECTION('',(0.,1.,0.));
#29325=DIRECTION('center_axis',(1.,0.,0.));
#29326=DIRECTION('ref_axis',(0.,0.,-1.));
#29327=DIRECTION('center_axis',(-1.,0.,0.));
#29328=DIRECTION('ref_axis',(0.,0.,-1.));
#29329=DIRECTION('',(0.707106781186548,-8.65956056235493E-17,0.707106781186547));
#29330=DIRECTION('center_axis',(1.,0.,0.));
#29331=DIRECTION('ref_axis',(0.,0.,-1.));
#29332=DIRECTION('center_axis',(-1.,0.,0.));
#29333=DIRECTION('ref_axis',(0.,0.,-1.));
#29334=DIRECTION('',(-1.,0.,0.));
#29335=DIRECTION('center_axis',(-1.,0.,0.));
#29336=DIRECTION('ref_axis',(0.,0.,-1.));
#29337=DIRECTION('center_axis',(-1.,0.,0.));
#29338=DIRECTION('ref_axis',(0.,0.,-1.));
#29339=DIRECTION('center_axis',(1.,0.,0.));
#29340=DIRECTION('ref_axis',(0.,0.,-1.));
#29341=DIRECTION('',(0.,0.,-1.));
#29342=DIRECTION('',(0.,1.,0.));
#29343=DIRECTION('',(0.,0.,1.));
#29344=DIRECTION('',(0.,1.,0.));
#29345=DIRECTION('center_axis',(1.,0.,0.));
#29346=DIRECTION('ref_axis',(0.,1.,0.));
#29347=DIRECTION('',(0.515038074910058,-0.85716730070211,-1.04972719113862E-16));
#29348=DIRECTION('center_axis',(1.,0.,0.));
#29349=DIRECTION('ref_axis',(0.,1.,0.));
#29350=DIRECTION('',(0.515038074910058,-0.85716730070211,-1.04972719113862E-16));
#29351=DIRECTION('center_axis',(0.,-1.,0.));
#29352=DIRECTION('ref_axis',(1.,0.,0.));
#29353=DIRECTION('center_axis',(0.,-1.,0.));
#29354=DIRECTION('ref_axis',(1.,0.,0.));
#29355=DIRECTION('',(0.,-1.,0.));
#29356=DIRECTION('center_axis',(0.,1.,0.));
#29357=DIRECTION('ref_axis',(1.,0.,0.));
#29358=DIRECTION('center_axis',(0.,-1.,0.));
#29359=DIRECTION('ref_axis',(1.,0.,0.));
#29360=DIRECTION('center_axis',(0.,-1.,0.));
#29361=DIRECTION('ref_axis',(1.,0.,0.));
#29362=DIRECTION('',(0.,-1.,0.));
#29363=DIRECTION('center_axis',(0.,1.,0.));
#29364=DIRECTION('ref_axis',(1.,0.,0.));
#29365=DIRECTION('center_axis',(0.,-1.,0.));
#29366=DIRECTION('ref_axis',(1.,0.,0.));
#29367=DIRECTION('center_axis',(0.,-1.,0.));
#29368=DIRECTION('ref_axis',(1.,0.,0.));
#29369=DIRECTION('',(0.,-1.,0.));
#29370=DIRECTION('center_axis',(0.,1.,0.));
#29371=DIRECTION('ref_axis',(1.,0.,0.));
#29372=DIRECTION('center_axis',(0.,-1.,0.));
#29373=DIRECTION('ref_axis',(1.,0.,0.));
#29374=DIRECTION('center_axis',(0.,-1.,0.));
#29375=DIRECTION('ref_axis',(1.,0.,0.));
#29376=DIRECTION('',(0.,-1.,0.));
#29377=DIRECTION('center_axis',(0.,1.,0.));
#29378=DIRECTION('ref_axis',(1.,0.,0.));
#29379=DIRECTION('center_axis',(0.,1.,0.));
#29380=DIRECTION('ref_axis',(1.,0.,0.));
#29381=DIRECTION('center_axis',(0.,-1.,0.));
#29382=DIRECTION('ref_axis',(1.,0.,0.));
#29383=DIRECTION('',(-0.707106781186545,0.70710678118655,8.6595605623549E-17));
#29384=DIRECTION('center_axis',(0.,1.,0.));
#29385=DIRECTION('ref_axis',(1.,0.,0.));
#29386=DIRECTION('center_axis',(0.,1.,0.));
#29387=DIRECTION('ref_axis',(0.,0.,1.));
#29388=DIRECTION('',(0.541178323236022,0.,-0.840907856105203));
#29389=DIRECTION('',(1.,0.,0.));
#29390=DIRECTION('',(0.541178323236022,0.,0.840907856105203));
#29391=DIRECTION('',(1.,0.,0.));
#29392=DIRECTION('',(0.,0.,-1.));
#29393=DIRECTION('',(-1.,0.,0.));
#29394=DIRECTION('',(0.,0.,-1.));
#29395=DIRECTION('',(1.,0.,0.));
#29396=DIRECTION('',(0.,0.,-1.));
#29397=DIRECTION('',(-1.,0.,0.));
#29398=DIRECTION('',(-0.541178323236022,0.,0.840907856105203));
#29399=DIRECTION('',(-1.,0.,0.));
#29400=DIRECTION('',(-0.541178323236022,0.,-0.840907856105203));
#29401=DIRECTION('',(-1.,0.,0.));
#29402=DIRECTION('',(0.,0.,1.));
#29403=DIRECTION('',(1.,0.,0.));
#29404=DIRECTION('',(0.,0.,1.));
#29405=DIRECTION('',(-1.,0.,0.));
#29406=DIRECTION('',(0.,0.,1.));
#29407=DIRECTION('',(1.,0.,0.));
#29408=DIRECTION('center_axis',(0.,1.,0.));
#29409=DIRECTION('ref_axis',(1.,0.,0.));
#29410=DIRECTION('center_axis',(0.,1.,0.));
#29411=DIRECTION('ref_axis',(1.,0.,0.));
#29412=DIRECTION('center_axis',(0.,1.,0.));
#29413=DIRECTION('ref_axis',(1.,0.,0.));
#29414=DIRECTION('center_axis',(0.,1.,0.));
#29415=DIRECTION('ref_axis',(1.,0.,0.));
#29416=DIRECTION('center_axis',(0.,-1.,0.));
#29417=DIRECTION('ref_axis',(1.,0.,0.));
#29418=DIRECTION('',(0.,-1.,0.));
#29419=DIRECTION('center_axis',(0.,1.,0.));
#29420=DIRECTION('ref_axis',(1.,0.,0.));
#29421=DIRECTION('center_axis',(0.,1.,0.));
#29422=DIRECTION('ref_axis',(1.,0.,0.));
#29423=DIRECTION('center_axis',(0.,-1.,0.));
#29424=DIRECTION('ref_axis',(1.,0.,0.));
#29425=DIRECTION('',(-0.707106781186545,0.707106781186551,8.65956056235489E-17));
#29426=DIRECTION('center_axis',(0.,-1.,0.));
#29427=DIRECTION('ref_axis',(1.,0.,0.));
#29428=DIRECTION('',(0.,-1.,0.));
#29429=DIRECTION('center_axis',(0.,1.,0.));
#29430=DIRECTION('ref_axis',(1.,0.,0.));
#29431=DIRECTION('center_axis',(0.,1.,0.));
#29432=DIRECTION('ref_axis',(1.,0.,0.));
#29433=DIRECTION('center_axis',(0.,-1.,0.));
#29434=DIRECTION('ref_axis',(1.,0.,0.));
#29435=DIRECTION('',(-0.707106781186545,0.707106781186551,8.65956056235489E-17));
#29436=DIRECTION('center_axis',(0.,-1.,0.));
#29437=DIRECTION('ref_axis',(1.,0.,0.));
#29438=DIRECTION('',(0.,-1.,0.));
#29439=DIRECTION('center_axis',(0.,1.,0.));
#29440=DIRECTION('ref_axis',(1.,0.,0.));
#29441=DIRECTION('center_axis',(0.,1.,0.));
#29442=DIRECTION('ref_axis',(1.,0.,0.));
#29443=DIRECTION('center_axis',(0.,-1.,0.));
#29444=DIRECTION('ref_axis',(1.,0.,0.));
#29445=DIRECTION('',(-0.707106781186545,0.70710678118655,8.6595605623549E-17));
#29446=DIRECTION('center_axis',(0.,-1.,0.));
#29447=DIRECTION('ref_axis',(1.,0.,0.));
#29448=DIRECTION('',(0.,-1.,0.));
#29449=DIRECTION('center_axis',(0.,1.,0.));
#29450=DIRECTION('ref_axis',(1.,0.,0.));
#29451=DIRECTION('center_axis',(0.,1.,0.));
#29452=DIRECTION('ref_axis',(1.,0.,0.));
#29453=DIRECTION('center_axis',(0.,-1.,0.));
#29454=DIRECTION('ref_axis',(1.,0.,0.));
#29455=DIRECTION('',(-0.707106781186547,0.707106781186548,8.65956056235493E-17));
#29456=DIRECTION('center_axis',(0.,-1.,0.));
#29457=DIRECTION('ref_axis',(1.,0.,0.));
#29458=DIRECTION('',(0.,-1.,0.));
#29459=DIRECTION('center_axis',(0.,1.,0.));
#29460=DIRECTION('ref_axis',(1.,0.,0.));
#29461=DIRECTION('center_axis',(0.594611647405038,0.707106781186538,0.382670862191361));
#29462=DIRECTION('ref_axis',(0.541178323236022,-2.00621933738417E-16,-0.840907856105203));
#29463=DIRECTION('',(0.359954879607299,-0.659709210427941,0.659709210427926));
#29464=DIRECTION('',(0.541178323236022,0.,-0.840907856105203));
#29465=DIRECTION('',(-0.359954879607298,0.659709210427941,-0.659709210427927));
#29466=DIRECTION('center_axis',(0.,0.70710678118654,0.707106781186555));
#29467=DIRECTION('ref_axis',(1.,0.,0.));
#29468=DIRECTION('',(-0.577350269189623,-0.577350269189635,0.577350269189619));
#29469=DIRECTION('',(1.,0.,0.));
#29470=DIRECTION('center_axis',(-0.707106781186555,0.70710678118654,0.));
#29471=DIRECTION('ref_axis',(0.,0.,1.));
#29472=DIRECTION('',(-0.577350269189622,-0.577350269189635,-0.57735026918962));
#29473=DIRECTION('center_axis',(0.707106781186555,0.70710678118654,0.));
#29474=DIRECTION('ref_axis',(0.,0.,-1.));
#29475=DIRECTION('',(0.,0.,-1.));
#29476=DIRECTION('',(-0.577350269189622,0.577350269189634,-0.577350269189622));
#29477=DIRECTION('',(0.577350269189622,-0.577350269189634,-0.577350269189622));
#29478=DIRECTION('center_axis',(0.,0.70710678118654,-0.707106781186555));
#29479=DIRECTION('ref_axis',(-1.,0.,0.));
#29480=DIRECTION('',(-0.577350269189622,-0.577350269189634,-0.577350269189622));
#29481=DIRECTION('',(-1.,0.,0.));
#29482=DIRECTION('center_axis',(0.,0.70710678118654,0.707106781186555));
#29483=DIRECTION('ref_axis',(1.,0.,0.));
#29484=DIRECTION('',(-0.577350269189622,-0.577350269189635,0.57735026918962));
#29485=DIRECTION('',(1.,0.,0.));
#29486=DIRECTION('',(0.577350269189622,0.577350269189635,-0.57735026918962));
#29487=DIRECTION('center_axis',(-0.707106781186555,0.70710678118654,0.));
#29488=DIRECTION('ref_axis',(0.,0.,1.));
#29489=DIRECTION('',(-0.577350269189624,-0.577350269189633,-0.57735026918962));
#29490=DIRECTION('center_axis',(-0.594611647405038,0.707106781186538,-0.382670862191361));
#29491=DIRECTION('ref_axis',(-0.541178323236022,-2.00621933738417E-16,0.840907856105203));
#29492=DIRECTION('',(-0.541178323236022,0.,0.840907856105203));
#29493=DIRECTION('',(0.359954879607298,0.659709210427941,0.659709210427927));
#29494=DIRECTION('',(-0.359954879607299,-0.659709210427941,-0.659709210427926));
#29495=DIRECTION('center_axis',(0.,0.70710678118654,-0.707106781186555));
#29496=DIRECTION('ref_axis',(-1.,0.,0.));
#29497=DIRECTION('',(0.359954879607296,-0.659709210427942,-0.659709210427927));
#29498=DIRECTION('',(-1.,0.,0.));
#29499=DIRECTION('center_axis',(0.,0.70710678118654,-0.707106781186555));
#29500=DIRECTION('ref_axis',(-1.,0.,0.));
#29501=DIRECTION('',(-1.,0.,0.));
#29502=DIRECTION('',(-0.359954879607298,0.659709210427941,0.659709210427927));
#29503=DIRECTION('center_axis',(0.594611647405038,0.707106781186539,-0.382670862191361));
#29504=DIRECTION('ref_axis',(-0.541178323236022,1.9046781686272E-16,-0.840907856105203));
#29505=DIRECTION('',(-0.541178323236022,0.,-0.840907856105203));
#29506=DIRECTION('center_axis',(0.,0.70710678118654,-0.707106781186555));
#29507=DIRECTION('ref_axis',(-1.,0.,0.));
#29508=DIRECTION('',(-1.,0.,0.));
#29509=DIRECTION('',(0.577350269189623,-0.577350269189635,-0.577350269189619));
#29510=DIRECTION('center_axis',(0.707106781186555,0.70710678118654,0.));
#29511=DIRECTION('ref_axis',(0.,0.,-1.));
#29512=DIRECTION('',(0.577350269189622,-0.577350269189635,0.57735026918962));
#29513=DIRECTION('center_axis',(-0.707106781186555,0.70710678118654,0.));
#29514=DIRECTION('ref_axis',(0.,0.,1.));
#29515=DIRECTION('',(0.,0.,1.));
#29516=DIRECTION('center_axis',(0.,0.70710678118654,0.707106781186555));
#29517=DIRECTION('ref_axis',(1.,0.,0.));
#29518=DIRECTION('',(1.,0.,0.));
#29519=DIRECTION('center_axis',(0.,0.70710678118654,-0.707106781186555));
#29520=DIRECTION('ref_axis',(-1.,0.,0.));
#29521=DIRECTION('',(-1.,0.,0.));
#29522=DIRECTION('',(0.577350269189622,-0.577350269189635,-0.57735026918962));
#29523=DIRECTION('center_axis',(0.707106781186555,0.70710678118654,0.));
#29524=DIRECTION('ref_axis',(0.,0.,-1.));
#29525=DIRECTION('',(0.577350269189624,-0.577350269189633,0.57735026918962));
#29526=DIRECTION('center_axis',(0.,0.70710678118654,0.707106781186555));
#29527=DIRECTION('ref_axis',(1.,0.,0.));
#29528=DIRECTION('',(1.,0.,0.));
#29529=DIRECTION('',(-0.359954879607296,-0.659709210427942,0.659709210427927));
#29530=DIRECTION('center_axis',(0.,0.70710678118654,0.707106781186555));
#29531=DIRECTION('ref_axis',(1.,0.,0.));
#29532=DIRECTION('',(1.,0.,0.));
#29533=DIRECTION('',(0.359954879607298,0.659709210427941,-0.659709210427927));
#29534=DIRECTION('center_axis',(-0.594611647405038,0.707106781186539,0.382670862191361));
#29535=DIRECTION('ref_axis',(0.541178323236022,1.9046781686272E-16,0.840907856105203));
#29536=DIRECTION('',(0.541178323236022,0.,0.840907856105203));
#29537=DIRECTION('center_axis',(0.,0.,1.));
#29538=DIRECTION('ref_axis',(1.,0.,0.));
#29539=DIRECTION('',(-1.,0.,0.));
#29540=DIRECTION('',(0.,1.,0.));
#29541=DIRECTION('center_axis',(0.,0.,1.));
#29542=DIRECTION('ref_axis',(1.,0.,0.));
#29543=DIRECTION('',(0.,1.,0.));
#29544=DIRECTION('',(1.,0.,0.));
#29545=DIRECTION('center_axis',(1.,0.,0.));
#29546=DIRECTION('ref_axis',(0.,0.,-1.));
#29547=DIRECTION('',(0.,1.,0.));
#29548=DIRECTION('',(0.,0.,-1.));
#29549=DIRECTION('center_axis',(0.,0.,-1.));
#29550=DIRECTION('ref_axis',(-1.,0.,0.));
#29551=DIRECTION('',(-1.,0.,0.));
#29552=DIRECTION('center_axis',(0.,0.,-1.));
#29553=DIRECTION('ref_axis',(-1.,0.,0.));
#29554=DIRECTION('',(0.,-1.,0.));
#29555=DIRECTION('',(1.,0.,0.));
#29556=DIRECTION('center_axis',(-0.840907856105203,0.,0.541178323236022));
#29557=DIRECTION('ref_axis',(0.541178323236022,0.,0.840907856105203));
#29558=DIRECTION('',(0.,1.,0.));
#29559=DIRECTION('',(0.541178323236022,0.,0.840907856105203));
#29560=DIRECTION('center_axis',(0.,0.,1.));
#29561=DIRECTION('ref_axis',(1.,0.,0.));
#29562=DIRECTION('',(0.,1.,0.));
#29563=DIRECTION('',(1.,0.,0.));
#29564=DIRECTION('center_axis',(0.840907856105203,0.,0.541178323236022));
#29565=DIRECTION('ref_axis',(0.541178323236022,0.,-0.840907856105203));
#29566=DIRECTION('',(0.,1.,0.));
#29567=DIRECTION('',(0.541178323236022,0.,-0.840907856105203));
#29568=DIRECTION('center_axis',(0.840907856105203,0.,-0.541178323236022));
#29569=DIRECTION('ref_axis',(-0.541178323236022,0.,-0.840907856105203));
#29570=DIRECTION('',(0.,1.,0.));
#29571=DIRECTION('',(-0.541178323236022,0.,-0.840907856105203));
#29572=DIRECTION('',(0.,-1.,0.));
#29573=DIRECTION('center_axis',(-0.840907856105203,0.,-0.541178323236022));
#29574=DIRECTION('ref_axis',(-0.541178323236022,0.,0.840907856105203));
#29575=DIRECTION('',(-0.541178323236022,0.,0.840907856105203));
#29576=DIRECTION('',(0.,1.,0.));
#29577=DIRECTION('center_axis',(0.,0.,-1.));
#29578=DIRECTION('ref_axis',(-1.,0.,0.));
#29579=DIRECTION('',(-1.,0.,0.));
#29580=DIRECTION('center_axis',(0.,0.,-1.));
#29581=DIRECTION('ref_axis',(-1.,0.,0.));
#29582=DIRECTION('',(1.,0.,0.));
#29583=DIRECTION('center_axis',(0.,0.,1.));
#29584=DIRECTION('ref_axis',(1.,0.,0.));
#29585=DIRECTION('',(-1.,0.,0.));
#29586=DIRECTION('center_axis',(0.,1.,0.));
#29587=DIRECTION('ref_axis',(1.,0.,0.));
#29588=DIRECTION('',(-1.,0.,0.));
#29589=DIRECTION('',(0.,0.,1.));
#29590=DIRECTION('',(1.,0.,0.));
#29591=DIRECTION('center_axis',(-1.,0.,0.));
#29592=DIRECTION('ref_axis',(0.,0.,1.));
#29593=DIRECTION('',(0.,1.,0.));
#29594=DIRECTION('',(0.,1.,0.));
#29595=DIRECTION('center_axis',(0.,0.,-1.));
#29596=DIRECTION('ref_axis',(-1.,0.,0.));
#29597=DIRECTION('center_axis',(0.,0.,1.));
#29598=DIRECTION('ref_axis',(1.,0.,0.));
#29599=DIRECTION('axis',(0.,0.,1.));
#29600=DIRECTION('refdir',(1.,0.,0.));
#29601=DIRECTION('center_axis',(0.,-1.,0.));
#29602=DIRECTION('ref_axis',(1.,0.,0.));
#29603=DIRECTION('center_axis',(0.,1.,0.));
#29604=DIRECTION('ref_axis',(1.,0.,0.));
#29605=DIRECTION('',(-0.707106781186547,-0.707106781186548,-8.65956056235493E-17));
#29606=DIRECTION('center_axis',(0.,-1.,0.));
#29607=DIRECTION('ref_axis',(1.,0.,0.));
#29608=DIRECTION('center_axis',(0.,1.,0.));
#29609=DIRECTION('ref_axis',(1.,0.,0.));
#29610=DIRECTION('',(1.,0.,0.));
#29611=DIRECTION('center_axis',(0.,1.,0.));
#29612=DIRECTION('ref_axis',(1.,0.,6.96064592241478E-16));
#29613=DIRECTION('',(0.,0.,1.));
#29614=DIRECTION('center_axis',(0.,1.,0.));
#29615=DIRECTION('ref_axis',(2.78425836896591E-15,0.,1.));
#29616=DIRECTION('',(-1.,0.,0.));
#29617=DIRECTION('',(0.,0.,1.));
#29618=DIRECTION('',(-1.,0.,0.));
#29619=DIRECTION('',(0.,0.,-1.));
#29620=DIRECTION('',(-1.,0.,0.));
#29621=DIRECTION('',(0.,0.,1.));
#29622=DIRECTION('',(-1.,0.,0.));
#29623=DIRECTION('',(0.,0.,-1.));
#29624=DIRECTION('',(-1.,0.,0.));
#29625=DIRECTION('center_axis',(0.,1.,0.));
#29626=DIRECTION('ref_axis',(-1.,0.,-2.08819377672444E-15));
#29627=DIRECTION('',(0.,0.,-1.));
#29628=DIRECTION('center_axis',(0.,1.,0.));
#29629=DIRECTION('ref_axis',(-2.78425836896591E-15,0.,-1.));
#29630=DIRECTION('',(1.,0.,0.));
#29631=DIRECTION('',(0.,0.,1.));
#29632=DIRECTION('',(-1.,0.,0.));
#29633=DIRECTION('',(0.,0.,-1.));
#29634=DIRECTION('',(1.,0.,0.));
#29635=DIRECTION('',(0.,0.,1.));
#29636=DIRECTION('',(-1.,0.,0.));
#29637=DIRECTION('',(0.,0.,-1.));
#29638=DIRECTION('center_axis',(0.,-1.,0.));
#29639=DIRECTION('ref_axis',(1.,0.,0.));
#29640=DIRECTION('center_axis',(0.,-1.,0.));
#29641=DIRECTION('ref_axis',(1.,0.,0.));
#29642=DIRECTION('center_axis',(0.,1.,0.));
#29643=DIRECTION('ref_axis',(1.,0.,0.));
#29644=DIRECTION('center_axis',(0.,1.,0.));
#29645=DIRECTION('ref_axis',(1.,0.,0.));
#29646=DIRECTION('center_axis',(0.,1.,0.));
#29647=DIRECTION('ref_axis',(1.,0.,0.));
#29648=DIRECTION('center_axis',(0.,1.,0.));
#29649=DIRECTION('ref_axis',(1.,0.,0.));
#29650=DIRECTION('',(-1.,0.,0.));
#29651=DIRECTION('',(0.,0.,-1.));
#29652=DIRECTION('center_axis',(0.,1.,0.));
#29653=DIRECTION('ref_axis',(1.,0.,8.32667268468876E-15));
#29654=DIRECTION('',(-1.,0.,0.));
#29655=DIRECTION('center_axis',(0.,1.,0.));
#29656=DIRECTION('ref_axis',(8.32667268468874E-15,0.,-1.));
#29657=DIRECTION('',(0.,0.,1.));
#29658=DIRECTION('',(-1.,0.,0.));
#29659=DIRECTION('center_axis',(0.,1.,0.));
#29660=DIRECTION('ref_axis',(8.97149918889015E-16,0.,-1.));
#29661=DIRECTION('',(1.,0.,0.));
#29662=DIRECTION('',(0.,0.,1.));
#29663=DIRECTION('center_axis',(0.,1.,0.));
#29664=DIRECTION('ref_axis',(-1.,0.,-8.32667268468874E-15));
#29665=DIRECTION('',(1.,0.,0.));
#29666=DIRECTION('center_axis',(0.,1.,0.));
#29667=DIRECTION('ref_axis',(-1.11022302462516E-14,0.,1.));
#29668=DIRECTION('',(0.,0.,-1.));
#29669=DIRECTION('',(1.,0.,0.));
#29670=DIRECTION('center_axis',(0.,1.,0.));
#29671=DIRECTION('ref_axis',(-3.58859967555606E-15,0.,1.));
#29672=DIRECTION('center_axis',(0.,-1.,0.));
#29673=DIRECTION('ref_axis',(1.,0.,0.));
#29674=DIRECTION('center_axis',(0.,-1.,0.));
#29675=DIRECTION('ref_axis',(1.,0.,0.));
#29676=DIRECTION('center_axis',(0.,-1.,0.));
#29677=DIRECTION('ref_axis',(1.,0.,0.));
#29678=DIRECTION('',(0.,-1.,0.));
#29679=DIRECTION('center_axis',(0.,-1.,0.));
#29680=DIRECTION('ref_axis',(1.,0.,0.));
#29681=DIRECTION('center_axis',(0.,1.,0.));
#29682=DIRECTION('ref_axis',(1.,0.,0.));
#29683=DIRECTION('',(-0.707106781186547,-0.707106781186548,-8.65956056235493E-17));
#29684=DIRECTION('center_axis',(0.,-1.,0.));
#29685=DIRECTION('ref_axis',(1.,0.,0.));
#29686=DIRECTION('center_axis',(0.,-1.,0.));
#29687=DIRECTION('ref_axis',(1.,0.,0.));
#29688=DIRECTION('',(0.,-1.,0.));
#29689=DIRECTION('center_axis',(0.,-1.,0.));
#29690=DIRECTION('ref_axis',(1.,0.,0.));
#29691=DIRECTION('center_axis',(0.,1.,0.));
#29692=DIRECTION('ref_axis',(1.,0.,0.));
#29693=DIRECTION('',(-0.707106781186547,-0.707106781186548,-8.65956056235493E-17));
#29694=DIRECTION('center_axis',(0.,-1.,0.));
#29695=DIRECTION('ref_axis',(1.,0.,0.));
#29696=DIRECTION('center_axis',(0.,-1.,0.));
#29697=DIRECTION('ref_axis',(1.,0.,0.));
#29698=DIRECTION('',(0.,-1.,0.));
#29699=DIRECTION('center_axis',(0.,-1.,0.));
#29700=DIRECTION('ref_axis',(1.,0.,0.));
#29701=DIRECTION('center_axis',(0.,1.,0.));
#29702=DIRECTION('ref_axis',(1.,0.,0.));
#29703=DIRECTION('',(-0.707106781186547,-0.707106781186548,-8.65956056235493E-17));
#29704=DIRECTION('center_axis',(0.,-1.,0.));
#29705=DIRECTION('ref_axis',(1.,0.,0.));
#29706=DIRECTION('center_axis',(0.,-1.,0.));
#29707=DIRECTION('ref_axis',(1.,0.,0.));
#29708=DIRECTION('',(0.,-1.,0.));
#29709=DIRECTION('center_axis',(0.,1.,0.));
#29710=DIRECTION('ref_axis',(1.,0.,0.));
#29711=DIRECTION('center_axis',(0.,-1.,0.));
#29712=DIRECTION('ref_axis',(1.,0.,0.));
#29713=DIRECTION('',(-0.707106781186553,0.707106781186542,8.659560562355E-17));
#29714=DIRECTION('center_axis',(0.,1.,0.));
#29715=DIRECTION('ref_axis',(1.,0.,0.));
#29716=DIRECTION('center_axis',(0.,1.,0.));
#29717=DIRECTION('ref_axis',(1.,0.,0.));
#29718=DIRECTION('',(-1.,0.,0.));
#29719=DIRECTION('center_axis',(0.,-1.,0.));
#29720=DIRECTION('ref_axis',(2.78425836896591E-15,0.,1.));
#29721=DIRECTION('',(0.,0.,1.));
#29722=DIRECTION('center_axis',(0.,-1.,0.));
#29723=DIRECTION('ref_axis',(1.,0.,6.96064592241478E-16));
#29724=DIRECTION('',(1.,0.,0.));
#29725=DIRECTION('',(0.,0.,1.));
#29726=DIRECTION('',(1.,0.,0.));
#29727=DIRECTION('',(0.,0.,-1.));
#29728=DIRECTION('',(1.,0.,0.));
#29729=DIRECTION('',(0.,0.,1.));
#29730=DIRECTION('',(1.,0.,0.));
#29731=DIRECTION('',(0.,0.,-1.));
#29732=DIRECTION('',(1.,0.,0.));
#29733=DIRECTION('center_axis',(0.,-1.,0.));
#29734=DIRECTION('ref_axis',(-2.78425836896591E-15,0.,-1.));
#29735=DIRECTION('',(0.,0.,-1.));
#29736=DIRECTION('center_axis',(0.,-1.,0.));
#29737=DIRECTION('ref_axis',(-1.,0.,-2.08819377672444E-15));
#29738=DIRECTION('',(-1.,0.,0.));
#29739=DIRECTION('',(0.,0.,-1.));
#29740=DIRECTION('',(-1.,0.,0.));
#29741=DIRECTION('',(0.,0.,1.));
#29742=DIRECTION('',(-1.,0.,0.));
#29743=DIRECTION('',(0.,0.,-1.));
#29744=DIRECTION('',(-1.,0.,0.));
#29745=DIRECTION('',(0.,0.,1.));
#29746=DIRECTION('center_axis',(0.,1.,0.));
#29747=DIRECTION('ref_axis',(1.,0.,0.));
#29748=DIRECTION('',(0.,0.,1.));
#29749=DIRECTION('center_axis',(0.,1.,0.));
#29750=DIRECTION('ref_axis',(8.32667268468873E-15,0.,-1.));
#29751=DIRECTION('',(-1.,0.,0.));
#29752=DIRECTION('center_axis',(0.,1.,0.));
#29753=DIRECTION('ref_axis',(1.,0.,8.32667268468876E-15));
#29754=DIRECTION('',(0.,0.,-1.));
#29755=DIRECTION('',(-1.,0.,0.));
#29756=DIRECTION('center_axis',(0.,1.,0.));
#29757=DIRECTION('ref_axis',(-3.58859967555606E-15,0.,1.));
#29758=DIRECTION('',(1.,0.,0.));
#29759=DIRECTION('',(0.,0.,-1.));
#29760=DIRECTION('center_axis',(0.,1.,0.));
#29761=DIRECTION('ref_axis',(-1.11022302462516E-14,0.,1.));
#29762=DIRECTION('',(1.,0.,0.));
#29763=DIRECTION('center_axis',(0.,1.,0.));
#29764=DIRECTION('ref_axis',(-1.,0.,-8.32667268468873E-15));
#29765=DIRECTION('',(0.,0.,1.));
#29766=DIRECTION('',(1.,0.,0.));
#29767=DIRECTION('center_axis',(0.,1.,0.));
#29768=DIRECTION('ref_axis',(8.97149918889015E-16,0.,-1.));
#29769=DIRECTION('',(-1.,0.,0.));
#29770=DIRECTION('center_axis',(0.,1.,0.));
#29771=DIRECTION('ref_axis',(1.,0.,0.));
#29772=DIRECTION('center_axis',(0.,1.,0.));
#29773=DIRECTION('ref_axis',(1.,0.,0.));
#29774=DIRECTION('center_axis',(0.,-1.,0.));
#29775=DIRECTION('ref_axis',(1.,0.,0.));
#29776=DIRECTION('',(0.,-1.,0.));
#29777=DIRECTION('center_axis',(0.,1.,0.));
#29778=DIRECTION('ref_axis',(1.,0.,0.));
#29779=DIRECTION('center_axis',(0.,-1.,0.));
#29780=DIRECTION('ref_axis',(1.,0.,0.));
#29781=DIRECTION('',(-0.70710678118655,0.707106781186545,8.65956056235497E-17));
#29782=DIRECTION('center_axis',(0.,-1.,0.));
#29783=DIRECTION('ref_axis',(1.,0.,0.));
#29784=DIRECTION('',(0.,-1.,0.));
#29785=DIRECTION('center_axis',(0.,1.,0.));
#29786=DIRECTION('ref_axis',(1.,0.,0.));
#29787=DIRECTION('center_axis',(0.,-1.,0.));
#29788=DIRECTION('ref_axis',(1.,0.,0.));
#29789=DIRECTION('',(-0.70710678118655,0.707106781186545,8.65956056235497E-17));
#29790=DIRECTION('center_axis',(0.,-1.,0.));
#29791=DIRECTION('ref_axis',(1.,0.,0.));
#29792=DIRECTION('',(0.,-1.,0.));
#29793=DIRECTION('center_axis',(0.,1.,0.));
#29794=DIRECTION('ref_axis',(1.,0.,0.));
#29795=DIRECTION('center_axis',(0.,-1.,0.));
#29796=DIRECTION('ref_axis',(1.,0.,0.));
#29797=DIRECTION('',(-0.707106781186553,0.707106781186542,8.659560562355E-17));
#29798=DIRECTION('center_axis',(0.,-1.,0.));
#29799=DIRECTION('ref_axis',(1.,0.,0.));
#29800=DIRECTION('',(0.,-1.,0.));
#29801=DIRECTION('center_axis',(0.,0.70710678118655,0.707106781186545));
#29802=DIRECTION('ref_axis',(1.,0.,0.));
#29803=DIRECTION('',(0.577350269189627,-0.577350269189623,0.577350269189627));
#29804=DIRECTION('',(1.,0.,0.));
#29805=DIRECTION('',(-0.577350269189627,-0.577350269189623,0.577350269189627));
#29806=DIRECTION('center_axis',(0.707106781186544,0.707106781186551,0.));
#29807=DIRECTION('ref_axis',(0.,0.,-1.));
#29808=DIRECTION('',(0.57735026918963,-0.577350269189624,0.577350269189624));
#29809=DIRECTION('',(0.,0.,-1.));
#29810=DIRECTION('center_axis',(0.,0.707106781186548,0.707106781186548));
#29811=DIRECTION('ref_axis',(1.,0.,0.));
#29812=DIRECTION('',(-0.577350269189629,-0.577350269189624,0.577350269189624));
#29813=DIRECTION('',(1.,0.,0.));
#29814=DIRECTION('center_axis',(-0.707106781186545,0.70710678118655,0.));
#29815=DIRECTION('ref_axis',(0.,0.,1.));
#29816=DIRECTION('',(-0.577350269189624,-0.577350269189624,0.577350269189629));
#29817=DIRECTION('',(0.,0.,1.));
#29818=DIRECTION('center_axis',(0.,0.70710678118655,-0.707106781186545));
#29819=DIRECTION('ref_axis',(-1.,0.,0.));
#29820=DIRECTION('',(-1.,0.,0.));
#29821=DIRECTION('',(0.,0.707106781186545,0.70710678118655));
#29822=DIRECTION('',(-0.577350269189624,-0.577350269189624,-0.577350269189629));
#29823=DIRECTION('center_axis',(-0.707106781186545,0.70710678118655,0.));
#29824=DIRECTION('ref_axis',(0.,0.,1.));
#29825=DIRECTION('',(-0.577350269189629,-0.577350269189624,-0.577350269189624));
#29826=DIRECTION('',(0.,0.,1.));
#29827=DIRECTION('center_axis',(0.,0.707106781186548,-0.707106781186548));
#29828=DIRECTION('ref_axis',(-1.,0.,0.));
#29829=DIRECTION('',(0.57735026918963,-0.577350269189624,-0.577350269189624));
#29830=DIRECTION('',(-1.,0.,0.));
#29831=DIRECTION('center_axis',(0.707106781186544,0.707106781186551,0.));
#29832=DIRECTION('ref_axis',(0.,0.,-1.));
#29833=DIRECTION('',(0.57735026918963,-0.577350269189622,-0.577350269189626));
#29834=DIRECTION('',(0.,0.,-1.));
#29835=DIRECTION('center_axis',(0.,0.70710678118655,-0.707106781186545));
#29836=DIRECTION('ref_axis',(-1.,0.,0.));
#29837=DIRECTION('',(-0.577350269189624,-0.577350269189624,-0.577350269189629));
#29838=DIRECTION('',(-1.,0.,0.));
#29839=DIRECTION('center_axis',(-0.707106781186545,0.70710678118655,0.));
#29840=DIRECTION('ref_axis',(0.,0.,1.));
#29841=DIRECTION('',(0.,0.,1.));
#29842=DIRECTION('',(-0.577350269189629,-0.577350269189624,-0.577350269189624));
#29843=DIRECTION('center_axis',(0.,0.707106781186548,-0.707106781186548));
#29844=DIRECTION('ref_axis',(-1.,0.,0.));
#29845=DIRECTION('',(-1.,0.,0.));
#29846=DIRECTION('',(0.577350269189629,-0.577350269189624,-0.577350269189624));
#29847=DIRECTION('center_axis',(0.707106781186545,0.70710678118655,0.));
#29848=DIRECTION('ref_axis',(0.,0.,-1.));
#29849=DIRECTION('',(0.,0.,-1.));
#29850=DIRECTION('',(0.577350269189624,-0.577350269189624,-0.577350269189629));
#29851=DIRECTION('center_axis',(0.,0.70710678118655,0.707106781186545));
#29852=DIRECTION('ref_axis',(1.,0.,0.));
#29853=DIRECTION('',(1.,0.,0.));
#29854=DIRECTION('',(0.,0.707106781186545,-0.70710678118655));
#29855=DIRECTION('',(0.577350269189627,-0.577350269189623,0.577350269189627));
#29856=DIRECTION('center_axis',(0.,-1.,0.));
#29857=DIRECTION('ref_axis',(2.78425836896591E-15,0.,1.));
#29858=DIRECTION('',(-0.707106781186553,0.707106781186542,0.));
#29859=DIRECTION('center_axis',(0.,1.,0.));
#29860=DIRECTION('ref_axis',(2.78425836896591E-15,0.,1.));
#29861=DIRECTION('center_axis',(0.707106781186542,0.707106781186553,0.));
#29862=DIRECTION('ref_axis',(0.,0.,-1.));
#29863=DIRECTION('',(-0.707106781186553,0.707106781186542,-5.23364152894591E-15));
#29864=DIRECTION('',(0.,0.,-1.));
#29865=DIRECTION('center_axis',(0.,-1.,0.));
#29866=DIRECTION('ref_axis',(1.,0.,6.96064592241478E-16));
#29867=DIRECTION('',(0.,0.70710678118654,0.707106781186555));
#29868=DIRECTION('center_axis',(0.,1.,0.));
#29869=DIRECTION('ref_axis',(1.,0.,6.96064592241478E-16));
#29870=DIRECTION('center_axis',(0.,0.70710678118655,-0.707106781186545));
#29871=DIRECTION('ref_axis',(-1.,0.,0.));
#29872=DIRECTION('',(-1.,0.,0.));
#29873=DIRECTION('center_axis',(0.,-1.,0.));
#29874=DIRECTION('ref_axis',(-2.78425836896591E-15,0.,-1.));
#29875=DIRECTION('',(0.707106781186547,0.707106781186547,0.));
#29876=DIRECTION('center_axis',(0.,1.,0.));
#29877=DIRECTION('ref_axis',(-2.78425836896591E-15,0.,-1.));
#29878=DIRECTION('center_axis',(-0.707106781186548,0.707106781186548,0.));
#29879=DIRECTION('ref_axis',(0.,0.,1.));
#29880=DIRECTION('',(0.707106781186547,0.707106781186547,5.23364152894595E-15));
#29881=DIRECTION('',(0.,0.,1.));
#29882=DIRECTION('center_axis',(0.,-1.,0.));
#29883=DIRECTION('ref_axis',(-1.,0.,-2.08819377672444E-15));
#29884=DIRECTION('',(0.,0.707106781186547,-0.707106781186547));
#29885=DIRECTION('center_axis',(0.,1.,0.));
#29886=DIRECTION('ref_axis',(-1.,0.,-2.08819377672444E-15));
#29887=DIRECTION('center_axis',(0.,0.70710678118655,0.707106781186545));
#29888=DIRECTION('ref_axis',(1.,0.,0.));
#29889=DIRECTION('',(1.,0.,0.));
#29890=DIRECTION('center_axis',(0.707106781186545,0.70710678118655,0.));
#29891=DIRECTION('ref_axis',(0.,0.,-1.));
#29892=DIRECTION('',(0.,0.,-1.));
#29893=DIRECTION('',(0.577350269189629,-0.577350269189624,0.577350269189624));
#29894=DIRECTION('center_axis',(0.,0.707106781186548,0.707106781186548));
#29895=DIRECTION('ref_axis',(1.,0.,0.));
#29896=DIRECTION('',(1.,0.,0.));
#29897=DIRECTION('',(-0.577350269189629,-0.577350269189624,0.577350269189624));
#29898=DIRECTION('center_axis',(-0.707106781186545,0.70710678118655,0.));
#29899=DIRECTION('ref_axis',(0.,0.,1.));
#29900=DIRECTION('',(0.,0.,1.));
#29901=DIRECTION('center_axis',(-1.,0.,0.));
#29902=DIRECTION('ref_axis',(0.,0.,1.));
#29903=DIRECTION('',(0.,1.,0.));
#29904=DIRECTION('',(0.,-1.,0.));
#29905=DIRECTION('center_axis',(0.,0.,-1.));
#29906=DIRECTION('ref_axis',(-1.,0.,0.));
#29907=DIRECTION('',(0.,1.,0.));
#29908=DIRECTION('center_axis',(1.,0.,0.));
#29909=DIRECTION('ref_axis',(0.,0.,-1.));
#29910=DIRECTION('',(0.,1.,0.));
#29911=DIRECTION('center_axis',(0.,0.,-1.));
#29912=DIRECTION('ref_axis',(-1.,0.,0.));
#29913=DIRECTION('',(0.,-1.,0.));
#29914=DIRECTION('center_axis',(-1.,0.,0.));
#29915=DIRECTION('ref_axis',(0.,0.,1.));
#29916=DIRECTION('',(0.,1.,0.));
#29917=DIRECTION('center_axis',(0.,0.,-1.));
#29918=DIRECTION('ref_axis',(-1.,0.,0.));
#29919=DIRECTION('',(0.,1.,0.));
#29920=DIRECTION('center_axis',(1.,0.,0.));
#29921=DIRECTION('ref_axis',(0.,0.,-1.));
#29922=DIRECTION('',(0.,1.,0.));
#29923=DIRECTION('center_axis',(0.,0.,-1.));
#29924=DIRECTION('ref_axis',(-1.,0.,0.));
#29925=DIRECTION('',(0.,1.,0.));
#29926=DIRECTION('center_axis',(0.,1.,0.));
#29927=DIRECTION('ref_axis',(1.,0.,6.96064592241478E-16));
#29928=DIRECTION('',(0.,1.,0.));
#29929=DIRECTION('center_axis',(1.,0.,0.));
#29930=DIRECTION('ref_axis',(0.,0.,-1.));
#29931=DIRECTION('',(0.,1.,0.));
#29932=DIRECTION('center_axis',(0.,1.,0.));
#29933=DIRECTION('ref_axis',(2.78425836896591E-15,0.,1.));
#29934=DIRECTION('',(0.,1.,0.));
#29935=DIRECTION('center_axis',(0.,0.,1.));
#29936=DIRECTION('ref_axis',(1.,0.,0.));
#29937=DIRECTION('',(0.,-1.,0.));
#29938=DIRECTION('center_axis',(0.,0.707106781186549,-0.707106781186546));
#29939=DIRECTION('ref_axis',(-1.,0.,0.));
#29940=DIRECTION('',(-1.,0.,0.));
#29941=DIRECTION('',(0.,0.707106781186546,0.707106781186549));
#29942=DIRECTION('',(0.577350269189628,-0.577350269189624,-0.577350269189626));
#29943=DIRECTION('center_axis',(-0.707106781186542,0.707106781186553,0.));
#29944=DIRECTION('ref_axis',(0.,0.,1.));
#29945=DIRECTION('',(0.,0.,1.));
#29946=DIRECTION('',(0.707106781186553,0.707106781186542,0.));
#29947=DIRECTION('',(-0.577350269189631,-0.577350269189622,-0.577350269189624));
#29948=DIRECTION('center_axis',(0.,0.707106781186549,0.707106781186546));
#29949=DIRECTION('ref_axis',(1.,0.,0.));
#29950=DIRECTION('',(1.,0.,0.));
#29951=DIRECTION('',(0.,0.707106781186546,-0.707106781186549));
#29952=DIRECTION('',(-0.577350269189631,-0.577350269189622,0.577350269189624));
#29953=DIRECTION('center_axis',(0.,1.,0.));
#29954=DIRECTION('ref_axis',(-3.58859967555606E-15,0.,1.));
#29955=DIRECTION('',(0.,0.707106781186542,0.707106781186553));
#29956=DIRECTION('center_axis',(0.,-1.,0.));
#29957=DIRECTION('ref_axis',(-3.58859967555606E-15,0.,1.));
#29958=DIRECTION('center_axis',(0.,0.707106781186549,-0.707106781186546));
#29959=DIRECTION('ref_axis',(-1.,0.,0.));
#29960=DIRECTION('',(-1.,0.,0.));
#29961=DIRECTION('center_axis',(0.707106781186545,0.70710678118655,0.));
#29962=DIRECTION('ref_axis',(0.,0.,-1.));
#29963=DIRECTION('',(0.,0.,-1.));
#29964=DIRECTION('',(-0.70710678118655,0.707106781186545,0.));
#29965=DIRECTION('',(0.577350269189628,-0.577350269189624,0.577350269189626));
#29966=DIRECTION('center_axis',(0.,1.,0.));
#29967=DIRECTION('ref_axis',(8.32667268468874E-15,0.,-1.));
#29968=DIRECTION('',(5.23364152894593E-15,0.707106781186545,-0.70710678118655));
#29969=DIRECTION('center_axis',(0.,-1.,0.));
#29970=DIRECTION('ref_axis',(8.32667268468874E-15,0.,-1.));
#29971=DIRECTION('center_axis',(0.,0.70710678118655,0.707106781186545));
#29972=DIRECTION('ref_axis',(1.,0.,0.));
#29973=DIRECTION('',(0.,0.707106781186542,-0.707106781186553));
#29974=DIRECTION('',(1.,0.,0.));
#29975=DIRECTION('center_axis',(0.,1.,0.));
#29976=DIRECTION('ref_axis',(1.,0.,8.32667268468876E-15));
#29977=DIRECTION('',(0.707106781186553,0.707106781186542,5.23364152894591E-15));
#29978=DIRECTION('center_axis',(0.,-1.,0.));
#29979=DIRECTION('ref_axis',(1.,0.,8.32667268468876E-15));
#29980=DIRECTION('center_axis',(-0.707106781186542,0.707106781186553,0.));
#29981=DIRECTION('ref_axis',(0.,0.,1.));
#29982=DIRECTION('',(0.,0.,1.));
#29983=DIRECTION('center_axis',(0.,1.,0.));
#29984=DIRECTION('ref_axis',(-1.11022302462516E-14,0.,1.));
#29985=DIRECTION('',(0.,0.70710678118654,0.707106781186555));
#29986=DIRECTION('center_axis',(0.,-1.,0.));
#29987=DIRECTION('ref_axis',(-1.11022302462516E-14,0.,1.));
#29988=DIRECTION('center_axis',(0.,0.70710678118655,-0.707106781186545));
#29989=DIRECTION('ref_axis',(-1.,0.,0.));
#29990=DIRECTION('',(0.,0.707106781186545,0.70710678118655));
#29991=DIRECTION('',(-1.,0.,0.));
#29992=DIRECTION('center_axis',(0.,1.,0.));
#29993=DIRECTION('ref_axis',(-1.,0.,-8.32667268468874E-15));
#29994=DIRECTION('',(-0.70710678118655,0.707106781186545,-5.23364152894593E-15));
#29995=DIRECTION('center_axis',(0.,-1.,0.));
#29996=DIRECTION('ref_axis',(-1.,0.,-8.32667268468874E-15));
#29997=DIRECTION('center_axis',(0.707106781186545,0.70710678118655,0.));
#29998=DIRECTION('ref_axis',(0.,0.,-1.));
#29999=DIRECTION('',(0.,0.,-1.));
#30000=DIRECTION('center_axis',(0.,1.,0.));
#30001=DIRECTION('ref_axis',(8.97149918889015E-16,0.,-1.));
#30002=DIRECTION('',(0.,0.707106781186547,-0.707106781186547));
#30003=DIRECTION('center_axis',(0.,-1.,0.));
#30004=DIRECTION('ref_axis',(8.97149918889015E-16,0.,-1.));
#30005=DIRECTION('center_axis',(0.,0.707106781186549,0.707106781186546));
#30006=DIRECTION('ref_axis',(1.,0.,0.));
#30007=DIRECTION('',(1.,0.,0.));
#30008=DIRECTION('center_axis',(0.,0.,1.));
#30009=DIRECTION('ref_axis',(1.,0.,0.));
#30010=DIRECTION('',(0.,1.,0.));
#30011=DIRECTION('',(0.,-1.,0.));
#30012=DIRECTION('center_axis',(0.,1.,0.));
#30013=DIRECTION('ref_axis',(-3.58859967555606E-15,0.,1.));
#30014=DIRECTION('',(0.,1.,0.));
#30015=DIRECTION('center_axis',(0.,0.,-1.));
#30016=DIRECTION('ref_axis',(-1.,0.,0.));
#30017=DIRECTION('',(0.,1.,0.));
#30018=DIRECTION('center_axis',(1.,0.,0.));
#30019=DIRECTION('ref_axis',(0.,0.,-1.));
#30020=DIRECTION('',(0.,1.,0.));
#30021=DIRECTION('center_axis',(0.,1.,0.));
#30022=DIRECTION('ref_axis',(1.,0.,8.32667268468876E-15));
#30023=DIRECTION('',(0.,1.,0.));
#30024=DIRECTION('center_axis',(0.,0.,-1.));
#30025=DIRECTION('ref_axis',(-1.,0.,0.));
#30026=DIRECTION('',(0.,1.,0.));
#30027=DIRECTION('center_axis',(0.,1.,0.));
#30028=DIRECTION('ref_axis',(8.32667268468874E-15,0.,-1.));
#30029=DIRECTION('',(0.,1.,0.));
#30030=DIRECTION('center_axis',(-1.,0.,0.));
#30031=DIRECTION('ref_axis',(0.,0.,1.));
#30032=DIRECTION('',(0.,-1.,0.));
#30033=DIRECTION('center_axis',(0.,0.,-1.));
#30034=DIRECTION('ref_axis',(-1.,0.,0.));
#30035=DIRECTION('',(0.,1.,0.));
#30036=DIRECTION('center_axis',(0.,0.,1.));
#30037=DIRECTION('ref_axis',(1.,0.,0.));
#30038=DIRECTION('',(0.,1.,0.));
#30039=DIRECTION('',(0.,1.,0.));
#30040=DIRECTION('center_axis',(0.,1.,0.));
#30041=DIRECTION('ref_axis',(8.97149918889015E-16,0.,-1.));
#30042=DIRECTION('center_axis',(1.,0.,0.));
#30043=DIRECTION('ref_axis',(0.,0.,-1.));
#30044=DIRECTION('',(0.,1.,0.));
#30045=DIRECTION('center_axis',(-1.,0.,0.));
#30046=DIRECTION('ref_axis',(0.,0.,1.));
#30047=DIRECTION('',(0.,1.,0.));
#30048=DIRECTION('center_axis',(0.,1.,0.));
#30049=DIRECTION('ref_axis',(-1.11022302462516E-14,0.,1.));
#30050=DIRECTION('',(0.,1.,0.));
#30051=DIRECTION('center_axis',(0.,0.,1.));
#30052=DIRECTION('ref_axis',(1.,0.,0.));
#30053=DIRECTION('',(0.,1.,0.));
#30054=DIRECTION('center_axis',(0.,1.,0.));
#30055=DIRECTION('ref_axis',(-1.,0.,-8.32667268468874E-15));
#30056=DIRECTION('center_axis',(1.,0.,0.));
#30057=DIRECTION('ref_axis',(0.,0.,-1.));
#30058=DIRECTION('',(0.,1.,0.));
#30059=DIRECTION('center_axis',(-1.,0.,0.));
#30060=DIRECTION('ref_axis',(0.,0.,1.));
#30061=DIRECTION('',(0.,1.,0.));
#30062=DIRECTION('',(0.,1.,0.));
#30063=DIRECTION('center_axis',(0.,0.,1.));
#30064=DIRECTION('ref_axis',(1.,0.,0.));
#30065=DIRECTION('center_axis',(0.,0.,1.));
#30066=DIRECTION('ref_axis',(1.,0.,0.));
#30067=DIRECTION('',(0.,-1.,0.));
#30068=DIRECTION('center_axis',(-1.,0.,0.));
#30069=DIRECTION('ref_axis',(0.,0.,1.));
#30070=DIRECTION('',(0.,1.,0.));
#30071=DIRECTION('',(0.,1.,0.));
#30072=DIRECTION('center_axis',(1.,0.,0.));
#30073=DIRECTION('ref_axis',(0.,0.,-1.));
#30074=DIRECTION('',(0.,1.,0.));
#30075=DIRECTION('center_axis',(0.,0.,1.));
#30076=DIRECTION('ref_axis',(1.,0.,0.));
#30077=DIRECTION('center_axis',(0.,0.,1.));
#30078=DIRECTION('ref_axis',(1.,0.,0.));
#30079=DIRECTION('',(0.,1.,0.));
#30080=DIRECTION('center_axis',(0.,1.,0.));
#30081=DIRECTION('ref_axis',(-1.,0.,-2.08819377672444E-15));
#30082=DIRECTION('',(0.,1.,0.));
#30083=DIRECTION('center_axis',(-1.,0.,0.));
#30084=DIRECTION('ref_axis',(0.,0.,1.));
#30085=DIRECTION('',(0.,1.,0.));
#30086=DIRECTION('center_axis',(0.,1.,0.));
#30087=DIRECTION('ref_axis',(-2.78425836896591E-15,0.,-1.));
#30088=DIRECTION('',(0.,1.,0.));
#30089=DIRECTION('center_axis',(0.,0.,-1.));
#30090=DIRECTION('ref_axis',(-1.,0.,0.));
#30091=DIRECTION('axis',(0.,0.,1.));
#30092=DIRECTION('refdir',(1.,0.,0.));
#30093=DIRECTION('center_axis',(-1.,0.,0.));
#30094=DIRECTION('ref_axis',(0.,0.,-1.));
#30095=DIRECTION('center_axis',(-1.,0.,0.));
#30096=DIRECTION('ref_axis',(0.,0.,-1.));
#30097=DIRECTION('',(1.,0.,0.));
#30098=DIRECTION('center_axis',(1.,0.,0.));
#30099=DIRECTION('ref_axis',(0.,0.,-1.));
#30100=DIRECTION('center_axis',(1.,0.,0.));
#30101=DIRECTION('ref_axis',(0.,0.,-1.));
#30102=DIRECTION('center_axis',(0.,-1.,0.));
#30103=DIRECTION('ref_axis',(1.,0.,0.));
#30104=DIRECTION('center_axis',(0.,-1.,0.));
#30105=DIRECTION('ref_axis',(1.,0.,0.));
#30106=DIRECTION('',(0.,-1.,0.));
#30107=DIRECTION('center_axis',(0.,1.,0.));
#30108=DIRECTION('ref_axis',(1.,0.,0.));
#30109=DIRECTION('center_axis',(0.,-1.,0.));
#30110=DIRECTION('ref_axis',(1.,0.,0.));
#30111=DIRECTION('center_axis',(0.,-1.,0.));
#30112=DIRECTION('ref_axis',(1.,0.,0.));
#30113=DIRECTION('',(0.,-1.,0.));
#30114=DIRECTION('center_axis',(0.,1.,0.));
#30115=DIRECTION('ref_axis',(1.,0.,0.));
#30116=DIRECTION('center_axis',(0.,-1.,0.));
#30117=DIRECTION('ref_axis',(1.,0.,0.));
#30118=DIRECTION('center_axis',(0.,-1.,0.));
#30119=DIRECTION('ref_axis',(1.,0.,0.));
#30120=DIRECTION('',(0.,-1.,0.));
#30121=DIRECTION('center_axis',(0.,1.,0.));
#30122=DIRECTION('ref_axis',(1.,0.,0.));
#30123=DIRECTION('center_axis',(0.,-1.,0.));
#30124=DIRECTION('ref_axis',(1.,0.,0.));
#30125=DIRECTION('center_axis',(0.,-1.,0.));
#30126=DIRECTION('ref_axis',(1.,0.,0.));
#30127=DIRECTION('',(0.,-1.,0.));
#30128=DIRECTION('center_axis',(0.,1.,0.));
#30129=DIRECTION('ref_axis',(1.,0.,0.));
#30130=DIRECTION('center_axis',(0.,1.,0.));
#30131=DIRECTION('ref_axis',(1.,0.,0.));
#30132=DIRECTION('center_axis',(0.,-1.,0.));
#30133=DIRECTION('ref_axis',(1.,0.,0.));
#30134=DIRECTION('',(-0.707106781186555,0.70710678118654,8.65956056235503E-17));
#30135=DIRECTION('center_axis',(0.,1.,0.));
#30136=DIRECTION('ref_axis',(1.,0.,0.));
#30137=DIRECTION('center_axis',(0.,-1.,0.));
#30138=DIRECTION('ref_axis',(1.,0.,0.));
#30139=DIRECTION('',(0.,-1.,0.));
#30140=DIRECTION('center_axis',(0.,-1.,0.));
#30141=DIRECTION('ref_axis',(1.,0.,0.));
#30142=DIRECTION('center_axis',(0.,1.,0.));
#30143=DIRECTION('ref_axis',(0.,0.,1.));
#30144=DIRECTION('center_axis',(0.,-1.,0.));
#30145=DIRECTION('ref_axis',(1.,0.,0.));
#30146=DIRECTION('center_axis',(0.,1.,0.));
#30147=DIRECTION('ref_axis',(1.,0.,0.));
#30148=DIRECTION('',(-0.85716730070211,0.515038074910058,1.04972719113862E-16));
#30149=DIRECTION('center_axis',(0.,-1.,0.));
#30150=DIRECTION('ref_axis',(1.,0.,0.));
#30151=DIRECTION('center_axis',(0.,-1.,0.));
#30152=DIRECTION('ref_axis',(1.,0.,0.));
#30153=DIRECTION('',(0.,1.,0.));
#30154=DIRECTION('center_axis',(0.,-1.,0.));
#30155=DIRECTION('ref_axis',(1.,0.,0.));
#30156=DIRECTION('center_axis',(0.,-1.,0.));
#30157=DIRECTION('ref_axis',(1.,0.,0.));
#30158=DIRECTION('',(0.707106781186555,0.70710678118654,8.65956056235503E-17));
#30159=DIRECTION('center_axis',(0.,-1.,0.));
#30160=DIRECTION('ref_axis',(1.,0.,0.));
#30161=DIRECTION('center_axis',(0.,-1.,0.));
#30162=DIRECTION('ref_axis',(1.,0.,0.));
#30163=DIRECTION('',(0.,1.,0.));
#30164=DIRECTION('center_axis',(0.,-1.,0.));
#30165=DIRECTION('ref_axis',(1.,0.,0.));
#30166=DIRECTION('center_axis',(0.,1.,0.));
#30167=DIRECTION('ref_axis',(0.,0.,1.));
#30168=DIRECTION('center_axis',(0.,-1.,0.));
#30169=DIRECTION('ref_axis',(1.,0.,0.));
#30170=DIRECTION('center_axis',(0.,-1.,0.));
#30171=DIRECTION('ref_axis',(1.,0.,0.));
#30172=DIRECTION('',(0.707106781186545,0.70710678118655,8.6595605623549E-17));
#30173=DIRECTION('center_axis',(1.,0.,0.));
#30174=DIRECTION('ref_axis',(0.,0.,-1.));
#30175=DIRECTION('',(0.,0.,1.));
#30176=DIRECTION('',(0.,1.,0.));
#30177=DIRECTION('',(0.,0.,-1.));
#30178=DIRECTION('',(0.,1.,0.));
#30179=DIRECTION('center_axis',(0.,1.,0.));
#30180=DIRECTION('ref_axis',(0.,0.,1.));
#30181=DIRECTION('center_axis',(0.,-1.,0.));
#30182=DIRECTION('ref_axis',(0.,0.,1.));
#30183=DIRECTION('center_axis',(0.,1.,0.));
#30184=DIRECTION('ref_axis',(0.,0.,1.));
#30185=DIRECTION('',(0.,1.,0.));
#30186=DIRECTION('center_axis',(0.,1.,0.));
#30187=DIRECTION('ref_axis',(-1.,0.,1.48029736616687E-15));
#30188=DIRECTION('center_axis',(0.,-1.,0.));
#30189=DIRECTION('ref_axis',(-1.,0.,1.48029736616687E-15));
#30190=DIRECTION('',(0.,1.,0.));
#30191=DIRECTION('center_axis',(0.,1.,0.));
#30192=DIRECTION('ref_axis',(-1.,0.,1.48029736616687E-15));
#30193=DIRECTION('',(0.,1.,0.));
#30194=DIRECTION('center_axis',(-1.,0.,0.));
#30195=DIRECTION('ref_axis',(0.,0.,1.));
#30196=DIRECTION('',(0.,0.,-1.));
#30197=DIRECTION('',(0.,0.,1.));
#30198=DIRECTION('',(0.,1.,0.));
#30199=DIRECTION('center_axis',(0.,1.,0.));
#30200=DIRECTION('ref_axis',(-1.48029736616687E-15,0.,-1.));
#30201=DIRECTION('center_axis',(0.,-1.,0.));
#30202=DIRECTION('ref_axis',(-1.48029736616687E-15,0.,-1.));
#30203=DIRECTION('center_axis',(0.,1.,0.));
#30204=DIRECTION('ref_axis',(-1.48029736616687E-15,0.,-1.));
#30205=DIRECTION('',(0.,1.,0.));
#30206=DIRECTION('center_axis',(0.,1.,0.));
#30207=DIRECTION('ref_axis',(1.,0.,1.48029736616688E-15));
#30208=DIRECTION('center_axis',(0.,-1.,0.));
#30209=DIRECTION('ref_axis',(1.,0.,1.48029736616688E-15));
#30210=DIRECTION('',(0.,1.,0.));
#30211=DIRECTION('center_axis',(0.,1.,0.));
#30212=DIRECTION('ref_axis',(1.,0.,1.48029736616688E-15));
#30213=DIRECTION('center_axis',(0.,1.,0.));
#30214=DIRECTION('ref_axis',(1.,0.,0.));
#30215=DIRECTION('',(-1.,0.,0.));
#30216=DIRECTION('',(1.,0.,0.));
#30217=DIRECTION('center_axis',(0.,1.,0.));
#30218=DIRECTION('ref_axis',(1.,0.,0.));
#30219=DIRECTION('',(1.,0.,0.));
#30220=DIRECTION('center_axis',(0.,1.,0.));
#30221=DIRECTION('ref_axis',(-8.88178419700132E-15,0.,1.));
#30222=DIRECTION('',(0.,0.,-1.));
#30223=DIRECTION('center_axis',(0.,1.,0.));
#30224=DIRECTION('ref_axis',(1.,0.,6.66133814775096E-15));
#30225=DIRECTION('',(-1.,0.,0.));
#30226=DIRECTION('center_axis',(0.,1.,0.));
#30227=DIRECTION('ref_axis',(1.,0.,0.));
#30228=DIRECTION('',(-1.,0.,0.));
#30229=DIRECTION('center_axis',(0.,1.,0.));
#30230=DIRECTION('ref_axis',(0.,0.,-1.));
#30231=DIRECTION('',(0.,0.,1.));
#30232=DIRECTION('center_axis',(0.,1.,0.));
#30233=DIRECTION('ref_axis',(-1.,0.,0.));
#30234=DIRECTION('',(1.,0.,0.));
#30235=DIRECTION('center_axis',(0.,1.,0.));
#30236=DIRECTION('ref_axis',(1.,0.,0.));
#30237=DIRECTION('center_axis',(0.,1.,0.));
#30238=DIRECTION('ref_axis',(0.,0.,1.));
#30239=DIRECTION('',(0.,0.,-1.));
#30240=DIRECTION('center_axis',(0.,1.,0.));
#30241=DIRECTION('ref_axis',(1.,0.,1.48029736616688E-15));
#30242=DIRECTION('',(1.,0.,0.));
#30243=DIRECTION('center_axis',(0.,1.,0.));
#30244=DIRECTION('ref_axis',(1.,0.,6.66133814775096E-15));
#30245=DIRECTION('',(0.,0.,1.));
#30246=DIRECTION('center_axis',(0.,1.,0.));
#30247=DIRECTION('ref_axis',(-8.88178419700132E-15,0.,1.));
#30248=DIRECTION('',(-1.,0.,0.));
#30249=DIRECTION('center_axis',(1.,0.,0.));
#30250=DIRECTION('ref_axis',(0.,0.,-1.));
#30251=DIRECTION('',(0.,1.,0.));
#30252=DIRECTION('',(0.,1.,0.));
#30253=DIRECTION('center_axis',(0.,1.,0.));
#30254=DIRECTION('ref_axis',(-8.88178419700132E-15,0.,1.));
#30255=DIRECTION('',(0.,1.,0.));
#30256=DIRECTION('center_axis',(0.,0.,1.));
#30257=DIRECTION('ref_axis',(1.,0.,0.));
#30258=DIRECTION('',(0.,1.,0.));
#30259=DIRECTION('',(-1.,0.,0.));
#30260=DIRECTION('',(-1.,0.,0.));
#30261=DIRECTION('center_axis',(0.,1.,0.));
#30262=DIRECTION('ref_axis',(-1.,0.,0.));
#30263=DIRECTION('center_axis',(0.,1.,0.));
#30264=DIRECTION('ref_axis',(-1.,0.,0.));
#30265=DIRECTION('',(0.,1.,0.));
#30266=DIRECTION('center_axis',(-1.,0.,0.));
#30267=DIRECTION('ref_axis',(0.,0.,1.));
#30268=DIRECTION('',(0.,0.,-1.));
#30269=DIRECTION('',(0.,1.,0.));
#30270=DIRECTION('center_axis',(0.,1.,0.));
#30271=DIRECTION('ref_axis',(0.,0.,-1.));
#30272=DIRECTION('center_axis',(0.,1.,0.));
#30273=DIRECTION('ref_axis',(0.,0.,-1.));
#30274=DIRECTION('',(0.,1.,0.));
#30275=DIRECTION('center_axis',(0.,0.,-1.));
#30276=DIRECTION('ref_axis',(-1.,0.,0.));
#30277=DIRECTION('',(1.,0.,0.));
#30278=DIRECTION('',(0.,1.,0.));
#30279=DIRECTION('',(1.,0.,0.));
#30280=DIRECTION('center_axis',(0.,1.,0.));
#30281=DIRECTION('ref_axis',(1.,0.,6.66133814775096E-15));
#30282=DIRECTION('center_axis',(0.,1.,0.));
#30283=DIRECTION('ref_axis',(1.,0.,0.));
#30284=DIRECTION('center_axis',(0.,1.,0.));
#30285=DIRECTION('ref_axis',(-1.,0.,1.48029736616688E-15));
#30286=DIRECTION('center_axis',(0.,1.,0.));
#30287=DIRECTION('ref_axis',(1.48029736616687E-15,0.,-1.));
#30288=DIRECTION('',(0.,0.,1.));
#30289=DIRECTION('center_axis',(0.,1.,0.));
#30290=DIRECTION('ref_axis',(1.,0.,0.));
#30291=DIRECTION('center_axis',(0.,1.,0.));
#30292=DIRECTION('ref_axis',(1.,0.,1.48029736616688E-15));
#30293=DIRECTION('',(-1.,0.,0.));
#30294=DIRECTION('center_axis',(0.,1.,0.));
#30295=DIRECTION('ref_axis',(1.48029736616687E-15,0.,-1.));
#30296=DIRECTION('center_axis',(1.,0.,0.));
#30297=DIRECTION('ref_axis',(0.,0.,-1.));
#30298=DIRECTION('',(0.,0.,1.));
#30299=DIRECTION('',(0.,1.,0.));
#30300=DIRECTION('',(0.,1.,0.));
#30301=DIRECTION('center_axis',(0.,1.,0.));
#30302=DIRECTION('ref_axis',(0.,0.,1.));
#30303=DIRECTION('center_axis',(0.,1.,0.));
#30304=DIRECTION('ref_axis',(0.,0.,1.));
#30305=DIRECTION('center_axis',(0.,1.,0.));
#30306=DIRECTION('ref_axis',(0.,0.,1.));
#30307=DIRECTION('',(0.,1.,0.));
#30308=DIRECTION('center_axis',(0.,0.,1.));
#30309=DIRECTION('ref_axis',(1.,0.,0.));
#30310=DIRECTION('',(-1.,0.,0.));
#30311=DIRECTION('',(1.,0.,0.));
#30312=DIRECTION('',(0.,1.,0.));
#30313=DIRECTION('center_axis',(0.,1.,0.));
#30314=DIRECTION('ref_axis',(-1.,0.,1.48029736616688E-15));
#30315=DIRECTION('center_axis',(0.,1.,0.));
#30316=DIRECTION('ref_axis',(-1.,0.,1.48029736616688E-15));
#30317=DIRECTION('center_axis',(0.,1.,0.));
#30318=DIRECTION('ref_axis',(-1.,0.,1.48029736616688E-15));
#30319=DIRECTION('',(0.,1.,0.));
#30320=DIRECTION('center_axis',(-1.,0.,0.));
#30321=DIRECTION('ref_axis',(0.,0.,1.));
#30322=DIRECTION('',(0.,0.,-1.));
#30323=DIRECTION('',(0.,1.,0.));
#30324=DIRECTION('center_axis',(0.,1.,0.));
#30325=DIRECTION('ref_axis',(1.48029736616687E-15,0.,-1.));
#30326=DIRECTION('center_axis',(0.,1.,0.));
#30327=DIRECTION('ref_axis',(1.48029736616687E-15,0.,-1.));
#30328=DIRECTION('',(0.,1.,0.));
#30329=DIRECTION('center_axis',(0.,0.,-1.));
#30330=DIRECTION('ref_axis',(-1.,0.,0.));
#30331=DIRECTION('',(1.,0.,0.));
#30332=DIRECTION('',(0.,1.,0.));
#30333=DIRECTION('center_axis',(0.,1.,0.));
#30334=DIRECTION('ref_axis',(1.,0.,1.48029736616688E-15));
#30335=DIRECTION('center_axis',(0.,1.,0.));
#30336=DIRECTION('ref_axis',(1.,0.,1.48029736616688E-15));
#30337=DIRECTION('center_axis',(0.,1.,0.));
#30338=DIRECTION('ref_axis',(1.,0.,0.));
#30339=DIRECTION('center_axis',(0.,1.,0.));
#30340=DIRECTION('ref_axis',(1.,0.,0.));
#30341=DIRECTION('axis',(0.,0.,1.));
#30342=DIRECTION('refdir',(1.,0.,0.));
#30343=DIRECTION('center_axis',(-0.960505777339176,0.,0.278260043301344));
#30344=DIRECTION('ref_axis',(-0.278260043301344,0.,-0.960505777339176));
#30345=DIRECTION('',(0.,1.,0.));
#30346=DIRECTION('',(-0.278260043301344,0.,-0.960505777339176));
#30347=DIRECTION('',(0.,-1.,0.));
#30348=DIRECTION('',(-0.278260043301344,0.,-0.960505777339176));
#30349=DIRECTION('center_axis',(0.,-1.,0.));
#30350=DIRECTION('ref_axis',(0.350496277439372,0.,0.936564124607142));
#30351=DIRECTION('center_axis',(0.,1.,0.));
#30352=DIRECTION('ref_axis',(0.350496277439372,0.,0.936564124607142));
#30353=DIRECTION('',(0.,-1.,0.));
#30354=DIRECTION('center_axis',(0.,-1.,0.));
#30355=DIRECTION('ref_axis',(0.350496277439372,0.,0.936564124607142));
#30356=DIRECTION('',(0.,-1.,0.));
#30357=DIRECTION('',(0.,-1.,0.));
#30358=DIRECTION('center_axis',(0.875939712077029,0.,-0.482420584973746));
#30359=DIRECTION('ref_axis',(0.482420584973746,0.,0.875939712077029));
#30360=DIRECTION('',(0.,-1.,0.));
#30361=DIRECTION('',(0.482420584973746,0.,0.875939712077029));
#30362=DIRECTION('',(0.482420584973746,0.,0.875939712077029));
#30363=DIRECTION('center_axis',(0.,1.,0.));
#30364=DIRECTION('ref_axis',(0.,0.,1.));
#30365=DIRECTION('center_axis',(0.,-1.,0.));
#30366=DIRECTION('ref_axis',(1.,0.,0.));
#30367=DIRECTION('',(-0.62464840640047,0.,-0.780906120081891));
#30368=DIRECTION('center_axis',(0.,1.,0.));
#30369=DIRECTION('ref_axis',(0.6822239107823,0.,0.731143307127204));
#30370=DIRECTION('',(0.780906120081892,0.,0.624648406400469));
#30371=DIRECTION('center_axis',(0.,-1.,0.));
#30372=DIRECTION('ref_axis',(1.,0.,0.));
#30373=DIRECTION('',(-0.87593971207703,0.,-0.482420584973745));
#30374=DIRECTION('center_axis',(0.,1.,0.));
#30375=DIRECTION('ref_axis',(0.910089138083774,0.,0.414412548967732));
#30376=DIRECTION('',(0.960505777339176,0.,0.278260043301343));
#30377=DIRECTION('center_axis',(0.,-1.,0.));
#30378=DIRECTION('ref_axis',(1.,0.,0.));
#30379=DIRECTION('',(-0.993877137003125,0.,-0.110490888956839));
#30380=DIRECTION('center_axis',(0.,1.,0.));
#30381=DIRECTION('ref_axis',(0.999401544090575,0.,0.0345912368870341));
#30382=DIRECTION('',(0.993877137003124,0.,-0.11049088895684));
#30383=DIRECTION('center_axis',(0.,-1.,0.));
#30384=DIRECTION('ref_axis',(1.,0.,0.));
#30385=DIRECTION('',(-0.960505777339176,0.,0.278260043301344));
#30386=DIRECTION('center_axis',(0.,1.,0.));
#30387=DIRECTION('ref_axis',(0.936564124607142,0.,-0.350496277439372));
#30388=DIRECTION('',(0.875939712077029,0.,-0.482420584973746));
#30389=DIRECTION('center_axis',(0.,-1.,0.));
#30390=DIRECTION('ref_axis',(1.,0.,0.));
#30391=DIRECTION('',(-0.780906120081891,0.,0.62464840640047));
#30392=DIRECTION('center_axis',(0.,1.,0.));
#30393=DIRECTION('ref_axis',(0.731143307127204,0.,-0.6822239107823));
#30394=DIRECTION('',(0.624648406400469,0.,-0.780906120081892));
#30395=DIRECTION('center_axis',(0.,-1.,0.));
#30396=DIRECTION('ref_axis',(1.,0.,0.));
#30397=DIRECTION('',(-0.482420584973745,0.,0.87593971207703));
#30398=DIRECTION('center_axis',(0.,1.,0.));
#30399=DIRECTION('ref_axis',(0.414412548967732,0.,-0.910089138083774));
#30400=DIRECTION('',(0.278260043301343,0.,-0.960505777339176));
#30401=DIRECTION('center_axis',(0.,-1.,0.));
#30402=DIRECTION('ref_axis',(1.,0.,0.));
#30403=DIRECTION('',(-0.110490888956839,0.,0.993877137003125));
#30404=DIRECTION('center_axis',(0.,1.,0.));
#30405=DIRECTION('ref_axis',(0.0345912368870341,0.,-0.999401544090575));
#30406=DIRECTION('',(-0.11049088895684,0.,-0.993877137003124));
#30407=DIRECTION('center_axis',(0.,-1.,0.));
#30408=DIRECTION('ref_axis',(1.,0.,0.));
#30409=DIRECTION('',(0.278260043301344,0.,0.960505777339176));
#30410=DIRECTION('center_axis',(0.,1.,0.));
#30411=DIRECTION('ref_axis',(-0.350496277439372,0.,-0.936564124607142));
#30412=DIRECTION('',(-0.482420584973746,0.,-0.875939712077029));
#30413=DIRECTION('center_axis',(0.,-1.,0.));
#30414=DIRECTION('ref_axis',(1.,0.,0.));
#30415=DIRECTION('',(0.62464840640047,0.,0.780906120081891));
#30416=DIRECTION('center_axis',(0.,1.,0.));
#30417=DIRECTION('ref_axis',(-0.6822239107823,0.,-0.731143307127204));
#30418=DIRECTION('',(-0.780906120081892,0.,-0.62464840640047));
#30419=DIRECTION('center_axis',(0.,-1.,0.));
#30420=DIRECTION('ref_axis',(1.,0.,0.));
#30421=DIRECTION('',(0.87593971207703,0.,0.482420584973745));
#30422=DIRECTION('center_axis',(0.,1.,0.));
#30423=DIRECTION('ref_axis',(-0.910089138083774,0.,-0.414412548967732));
#30424=DIRECTION('',(-0.960505777339176,0.,-0.278260043301343));
#30425=DIRECTION('center_axis',(0.,-1.,0.));
#30426=DIRECTION('ref_axis',(1.,0.,0.));
#30427=DIRECTION('',(0.993877137003125,0.,0.110490888956839));
#30428=DIRECTION('center_axis',(0.,1.,0.));
#30429=DIRECTION('ref_axis',(-0.999401544090575,0.,-0.0345912368870342));
#30430=DIRECTION('',(-0.993877137003124,0.,0.110490888956839));
#30431=DIRECTION('center_axis',(0.,-1.,0.));
#30432=DIRECTION('ref_axis',(1.,0.,0.));
#30433=DIRECTION('',(0.960505777339176,0.,-0.278260043301343));
#30434=DIRECTION('center_axis',(0.,1.,0.));
#30435=DIRECTION('ref_axis',(-0.936564124607143,0.,0.350496277439371));
#30436=DIRECTION('',(-0.875939712077029,0.,0.482420584973746));
#30437=DIRECTION('center_axis',(0.,-1.,0.));
#30438=DIRECTION('ref_axis',(1.,0.,0.));
#30439=DIRECTION('',(0.780906120081891,0.,-0.62464840640047));
#30440=DIRECTION('center_axis',(0.,1.,0.));
#30441=DIRECTION('ref_axis',(-0.731143307127204,0.,0.6822239107823));
#30442=DIRECTION('',(-0.62464840640047,0.,0.780906120081892));
#30443=DIRECTION('center_axis',(0.,-1.,0.));
#30444=DIRECTION('ref_axis',(1.,0.,0.));
#30445=DIRECTION('',(0.482420584973745,0.,-0.87593971207703));
#30446=DIRECTION('center_axis',(0.,1.,0.));
#30447=DIRECTION('ref_axis',(-0.414412548967732,0.,0.910089138083774));
#30448=DIRECTION('',(-0.278260043301343,0.,0.960505777339176));
#30449=DIRECTION('center_axis',(0.,-1.,0.));
#30450=DIRECTION('ref_axis',(1.,0.,0.));
#30451=DIRECTION('',(0.110490888956839,0.,-0.993877137003125));
#30452=DIRECTION('center_axis',(0.,1.,0.));
#30453=DIRECTION('ref_axis',(-0.0345912368870343,0.,0.999401544090575));
#30454=DIRECTION('',(0.110490888956839,0.,0.993877137003124));
#30455=DIRECTION('center_axis',(0.,-1.,0.));
#30456=DIRECTION('ref_axis',(1.,0.,0.));
#30457=DIRECTION('center_axis',(0.,-1.,0.));
#30458=DIRECTION('ref_axis',(1.,0.,0.));
#30459=DIRECTION('center_axis',(0.,-1.,0.));
#30460=DIRECTION('ref_axis',(1.,0.,0.));
#30461=DIRECTION('center_axis',(0.,-1.,0.));
#30462=DIRECTION('ref_axis',(1.,0.,0.));
#30463=DIRECTION('',(0.,1.,0.));
#30464=DIRECTION('center_axis',(-0.780906120081891,0.,0.62464840640047));
#30465=DIRECTION('ref_axis',(-0.62464840640047,0.,-0.780906120081891));
#30466=DIRECTION('',(-0.62464840640047,0.,-0.780906120081891));
#30467=DIRECTION('',(0.,-1.,0.));
#30468=DIRECTION('center_axis',(0.,-1.,0.));
#30469=DIRECTION('ref_axis',(0.6822239107823,0.,0.731143307127204));
#30470=DIRECTION('',(0.,-1.,0.));
#30471=DIRECTION('center_axis',(0.,-1.,0.));
#30472=DIRECTION('ref_axis',(0.6822239107823,0.,0.731143307127204));
#30473=DIRECTION('',(0.,-1.,0.));
#30474=DIRECTION('',(0.,-1.,0.));
#30475=DIRECTION('center_axis',(0.624648406400469,0.,-0.780906120081892));
#30476=DIRECTION('ref_axis',(0.780906120081892,0.,0.624648406400469));
#30477=DIRECTION('',(0.,-1.,0.));
#30478=DIRECTION('',(0.780906120081892,0.,0.624648406400469));
#30479=DIRECTION('center_axis',(0.,-1.,0.));
#30480=DIRECTION('ref_axis',(1.,0.,0.));
#30481=DIRECTION('center_axis',(0.,-1.,0.));
#30482=DIRECTION('ref_axis',(1.,0.,0.));
#30483=DIRECTION('',(0.,1.,0.));
#30484=DIRECTION('center_axis',(-0.482420584973745,0.,0.87593971207703));
#30485=DIRECTION('ref_axis',(-0.87593971207703,0.,-0.482420584973745));
#30486=DIRECTION('',(-0.87593971207703,0.,-0.482420584973745));
#30487=DIRECTION('',(0.,-1.,0.));
#30488=DIRECTION('center_axis',(0.,-1.,0.));
#30489=DIRECTION('ref_axis',(0.910089138083774,0.,0.414412548967732));
#30490=DIRECTION('',(0.,-1.,0.));
#30491=DIRECTION('center_axis',(0.,-1.,0.));
#30492=DIRECTION('ref_axis',(0.910089138083774,0.,0.414412548967732));
#30493=DIRECTION('',(0.,-1.,0.));
#30494=DIRECTION('',(0.,-1.,0.));
#30495=DIRECTION('center_axis',(0.278260043301343,0.,-0.960505777339176));
#30496=DIRECTION('ref_axis',(0.960505777339176,0.,0.278260043301343));
#30497=DIRECTION('',(0.,-1.,0.));
#30498=DIRECTION('',(0.960505777339176,0.,0.278260043301343));
#30499=DIRECTION('center_axis',(0.,-1.,0.));
#30500=DIRECTION('ref_axis',(1.,0.,0.));
#30501=DIRECTION('center_axis',(0.,-1.,0.));
#30502=DIRECTION('ref_axis',(1.,0.,0.));
#30503=DIRECTION('',(0.,1.,0.));
#30504=DIRECTION('center_axis',(-0.110490888956839,0.,0.993877137003125));
#30505=DIRECTION('ref_axis',(-0.993877137003125,0.,-0.110490888956839));
#30506=DIRECTION('',(-0.993877137003125,0.,-0.110490888956839));
#30507=DIRECTION('',(0.,-1.,0.));
#30508=DIRECTION('center_axis',(0.,-1.,0.));
#30509=DIRECTION('ref_axis',(0.999401544090575,0.,0.0345912368870341));
#30510=DIRECTION('',(0.,-1.,0.));
#30511=DIRECTION('center_axis',(0.,-1.,0.));
#30512=DIRECTION('ref_axis',(0.999401544090575,0.,0.0345912368870341));
#30513=DIRECTION('',(0.,-1.,0.));
#30514=DIRECTION('',(0.,-1.,0.));
#30515=DIRECTION('center_axis',(-0.11049088895684,0.,-0.993877137003125));
#30516=DIRECTION('ref_axis',(0.993877137003125,0.,-0.11049088895684));
#30517=DIRECTION('',(0.,-1.,0.));
#30518=DIRECTION('',(0.993877137003124,0.,-0.11049088895684));
#30519=DIRECTION('center_axis',(0.,-1.,0.));
#30520=DIRECTION('ref_axis',(1.,0.,0.));
#30521=DIRECTION('center_axis',(0.,-1.,0.));
#30522=DIRECTION('ref_axis',(1.,0.,0.));
#30523=DIRECTION('',(0.,1.,0.));
#30524=DIRECTION('center_axis',(0.278260043301344,0.,0.960505777339176));
#30525=DIRECTION('ref_axis',(-0.960505777339176,0.,0.278260043301344));
#30526=DIRECTION('',(-0.960505777339176,0.,0.278260043301344));
#30527=DIRECTION('',(0.,-1.,0.));
#30528=DIRECTION('center_axis',(0.,-1.,0.));
#30529=DIRECTION('ref_axis',(0.936564124607142,0.,-0.350496277439372));
#30530=DIRECTION('',(0.,-1.,0.));
#30531=DIRECTION('center_axis',(0.,-1.,0.));
#30532=DIRECTION('ref_axis',(0.936564124607142,0.,-0.350496277439372));
#30533=DIRECTION('',(0.,-1.,0.));
#30534=DIRECTION('',(0.,-1.,0.));
#30535=DIRECTION('center_axis',(-0.482420584973746,0.,-0.875939712077029));
#30536=DIRECTION('ref_axis',(0.875939712077029,0.,-0.482420584973746));
#30537=DIRECTION('',(0.,-1.,0.));
#30538=DIRECTION('',(0.875939712077029,0.,-0.482420584973746));
#30539=DIRECTION('center_axis',(0.,-1.,0.));
#30540=DIRECTION('ref_axis',(1.,0.,0.));
#30541=DIRECTION('center_axis',(0.,-1.,0.));
#30542=DIRECTION('ref_axis',(1.,0.,0.));
#30543=DIRECTION('',(0.,1.,0.));
#30544=DIRECTION('center_axis',(0.62464840640047,0.,0.780906120081891));
#30545=DIRECTION('ref_axis',(-0.780906120081891,0.,0.62464840640047));
#30546=DIRECTION('',(-0.780906120081891,0.,0.62464840640047));
#30547=DIRECTION('',(0.,-1.,0.));
#30548=DIRECTION('center_axis',(0.,-1.,0.));
#30549=DIRECTION('ref_axis',(0.731143307127204,0.,-0.6822239107823));
#30550=DIRECTION('',(0.,-1.,0.));
#30551=DIRECTION('center_axis',(0.,-1.,0.));
#30552=DIRECTION('ref_axis',(0.731143307127204,0.,-0.6822239107823));
#30553=DIRECTION('',(0.,-1.,0.));
#30554=DIRECTION('',(0.,-1.,0.));
#30555=DIRECTION('center_axis',(-0.780906120081892,0.,-0.624648406400469));
#30556=DIRECTION('ref_axis',(0.624648406400469,0.,-0.780906120081892));
#30557=DIRECTION('',(0.,-1.,0.));
#30558=DIRECTION('',(0.624648406400469,0.,-0.780906120081892));
#30559=DIRECTION('center_axis',(0.,-1.,0.));
#30560=DIRECTION('ref_axis',(1.,0.,0.));
#30561=DIRECTION('center_axis',(0.,-1.,0.));
#30562=DIRECTION('ref_axis',(1.,0.,0.));
#30563=DIRECTION('',(0.,1.,0.));
#30564=DIRECTION('center_axis',(0.87593971207703,0.,0.482420584973745));
#30565=DIRECTION('ref_axis',(-0.482420584973745,0.,0.87593971207703));
#30566=DIRECTION('',(-0.482420584973745,0.,0.87593971207703));
#30567=DIRECTION('',(0.,-1.,0.));
#30568=DIRECTION('center_axis',(0.,-1.,0.));
#30569=DIRECTION('ref_axis',(0.414412548967732,0.,-0.910089138083774));
#30570=DIRECTION('',(0.,-1.,0.));
#30571=DIRECTION('center_axis',(0.,-1.,0.));
#30572=DIRECTION('ref_axis',(0.414412548967732,0.,-0.910089138083774));
#30573=DIRECTION('',(0.,-1.,0.));
#30574=DIRECTION('',(0.,-1.,0.));
#30575=DIRECTION('center_axis',(-0.960505777339176,0.,-0.278260043301343));
#30576=DIRECTION('ref_axis',(0.278260043301343,0.,-0.960505777339176));
#30577=DIRECTION('',(0.,-1.,0.));
#30578=DIRECTION('',(0.278260043301343,0.,-0.960505777339176));
#30579=DIRECTION('center_axis',(0.,-1.,0.));
#30580=DIRECTION('ref_axis',(1.,0.,0.));
#30581=DIRECTION('center_axis',(0.,-1.,0.));
#30582=DIRECTION('ref_axis',(1.,0.,0.));
#30583=DIRECTION('',(0.,1.,0.));
#30584=DIRECTION('center_axis',(0.993877137003125,0.,0.110490888956839));
#30585=DIRECTION('ref_axis',(-0.110490888956839,0.,0.993877137003125));
#30586=DIRECTION('',(-0.110490888956839,0.,0.993877137003125));
#30587=DIRECTION('',(0.,-1.,0.));
#30588=DIRECTION('center_axis',(0.,-1.,0.));
#30589=DIRECTION('ref_axis',(0.0345912368870341,0.,-0.999401544090575));
#30590=DIRECTION('',(0.,-1.,0.));
#30591=DIRECTION('center_axis',(0.,-1.,0.));
#30592=DIRECTION('ref_axis',(0.0345912368870341,0.,-0.999401544090575));
#30593=DIRECTION('',(0.,-1.,0.));
#30594=DIRECTION('',(0.,-1.,0.));
#30595=DIRECTION('center_axis',(-0.993877137003125,0.,0.11049088895684));
#30596=DIRECTION('ref_axis',(-0.11049088895684,0.,-0.993877137003125));
#30597=DIRECTION('',(0.,-1.,0.));
#30598=DIRECTION('',(-0.11049088895684,0.,-0.993877137003124));
#30599=DIRECTION('center_axis',(0.,-1.,0.));
#30600=DIRECTION('ref_axis',(1.,0.,0.));
#30601=DIRECTION('center_axis',(0.,-1.,0.));
#30602=DIRECTION('ref_axis',(1.,0.,0.));
#30603=DIRECTION('',(0.,1.,0.));
#30604=DIRECTION('center_axis',(0.960505777339176,0.,-0.278260043301344));
#30605=DIRECTION('ref_axis',(0.278260043301344,0.,0.960505777339176));
#30606=DIRECTION('',(0.278260043301344,0.,0.960505777339176));
#30607=DIRECTION('',(0.,-1.,0.));
#30608=DIRECTION('center_axis',(0.,-1.,0.));
#30609=DIRECTION('ref_axis',(-0.350496277439372,0.,-0.936564124607142));
#30610=DIRECTION('',(0.,-1.,0.));
#30611=DIRECTION('center_axis',(0.,-1.,0.));
#30612=DIRECTION('ref_axis',(-0.350496277439372,0.,-0.936564124607142));
#30613=DIRECTION('',(0.,-1.,0.));
#30614=DIRECTION('',(0.,-1.,0.));
#30615=DIRECTION('center_axis',(-0.875939712077029,0.,0.482420584973746));
#30616=DIRECTION('ref_axis',(-0.482420584973746,0.,-0.875939712077029));
#30617=DIRECTION('',(0.,-1.,0.));
#30618=DIRECTION('',(-0.482420584973746,0.,-0.875939712077029));
#30619=DIRECTION('center_axis',(0.,-1.,0.));
#30620=DIRECTION('ref_axis',(1.,0.,0.));
#30621=DIRECTION('center_axis',(0.,-1.,0.));
#30622=DIRECTION('ref_axis',(1.,0.,0.));
#30623=DIRECTION('',(0.,1.,0.));
#30624=DIRECTION('center_axis',(0.780906120081891,0.,-0.62464840640047));
#30625=DIRECTION('ref_axis',(0.62464840640047,0.,0.780906120081891));
#30626=DIRECTION('',(0.62464840640047,0.,0.780906120081891));
#30627=DIRECTION('',(0.,-1.,0.));
#30628=DIRECTION('center_axis',(0.,-1.,0.));
#30629=DIRECTION('ref_axis',(-0.6822239107823,0.,-0.731143307127204));
#30630=DIRECTION('',(0.,-1.,0.));
#30631=DIRECTION('center_axis',(0.,-1.,0.));
#30632=DIRECTION('ref_axis',(-0.6822239107823,0.,-0.731143307127204));
#30633=DIRECTION('',(0.,-1.,0.));
#30634=DIRECTION('',(0.,-1.,0.));
#30635=DIRECTION('center_axis',(-0.62464840640047,0.,0.780906120081892));
#30636=DIRECTION('ref_axis',(-0.780906120081892,0.,-0.62464840640047));
#30637=DIRECTION('',(0.,-1.,0.));
#30638=DIRECTION('',(-0.780906120081892,0.,-0.62464840640047));
#30639=DIRECTION('center_axis',(0.,-1.,0.));
#30640=DIRECTION('ref_axis',(1.,0.,0.));
#30641=DIRECTION('center_axis',(0.,-1.,0.));
#30642=DIRECTION('ref_axis',(1.,0.,0.));
#30643=DIRECTION('',(0.,1.,0.));
#30644=DIRECTION('center_axis',(0.482420584973745,0.,-0.87593971207703));
#30645=DIRECTION('ref_axis',(0.87593971207703,0.,0.482420584973745));
#30646=DIRECTION('',(0.87593971207703,0.,0.482420584973745));
#30647=DIRECTION('',(0.,-1.,0.));
#30648=DIRECTION('center_axis',(0.,-1.,0.));
#30649=DIRECTION('ref_axis',(-0.910089138083774,0.,-0.414412548967732));
#30650=DIRECTION('',(0.,-1.,0.));
#30651=DIRECTION('center_axis',(0.,-1.,0.));
#30652=DIRECTION('ref_axis',(-0.910089138083774,0.,-0.414412548967732));
#30653=DIRECTION('',(0.,-1.,0.));
#30654=DIRECTION('',(0.,-1.,0.));
#30655=DIRECTION('center_axis',(-0.278260043301343,0.,0.960505777339176));
#30656=DIRECTION('ref_axis',(-0.960505777339176,0.,-0.278260043301343));
#30657=DIRECTION('',(0.,-1.,0.));
#30658=DIRECTION('',(-0.960505777339176,0.,-0.278260043301343));
#30659=DIRECTION('center_axis',(0.,-1.,0.));
#30660=DIRECTION('ref_axis',(1.,0.,0.));
#30661=DIRECTION('center_axis',(0.,-1.,0.));
#30662=DIRECTION('ref_axis',(1.,0.,0.));
#30663=DIRECTION('',(0.,1.,0.));
#30664=DIRECTION('center_axis',(0.110490888956839,0.,-0.993877137003125));
#30665=DIRECTION('ref_axis',(0.993877137003125,0.,0.110490888956839));
#30666=DIRECTION('',(0.993877137003125,0.,0.110490888956839));
#30667=DIRECTION('',(0.,-1.,0.));
#30668=DIRECTION('center_axis',(0.,-1.,0.));
#30669=DIRECTION('ref_axis',(-0.999401544090575,0.,-0.0345912368870342));
#30670=DIRECTION('',(0.,-1.,0.));
#30671=DIRECTION('center_axis',(0.,-1.,0.));
#30672=DIRECTION('ref_axis',(-0.999401544090575,0.,-0.0345912368870342));
#30673=DIRECTION('',(0.,-1.,0.));
#30674=DIRECTION('',(0.,-1.,0.));
#30675=DIRECTION('center_axis',(0.110490888956839,0.,0.993877137003125));
#30676=DIRECTION('ref_axis',(-0.993877137003125,0.,0.110490888956839));
#30677=DIRECTION('',(0.,-1.,0.));
#30678=DIRECTION('',(-0.993877137003124,0.,0.110490888956839));
#30679=DIRECTION('center_axis',(0.,-1.,0.));
#30680=DIRECTION('ref_axis',(1.,0.,0.));
#30681=DIRECTION('center_axis',(0.,-1.,0.));
#30682=DIRECTION('ref_axis',(1.,0.,0.));
#30683=DIRECTION('',(0.,1.,0.));
#30684=DIRECTION('center_axis',(-0.278260043301344,0.,-0.960505777339176));
#30685=DIRECTION('ref_axis',(0.960505777339176,0.,-0.278260043301344));
#30686=DIRECTION('',(0.960505777339176,0.,-0.278260043301343));
#30687=DIRECTION('',(0.,-1.,0.));
#30688=DIRECTION('center_axis',(0.,-1.,0.));
#30689=DIRECTION('ref_axis',(-0.936564124607143,0.,0.350496277439371));
#30690=DIRECTION('',(0.,-1.,0.));
#30691=DIRECTION('center_axis',(0.,-1.,0.));
#30692=DIRECTION('ref_axis',(-0.936564124607143,0.,0.350496277439371));
#30693=DIRECTION('',(0.,-1.,0.));
#30694=DIRECTION('',(0.,-1.,0.));
#30695=DIRECTION('center_axis',(0.482420584973746,0.,0.875939712077029));
#30696=DIRECTION('ref_axis',(-0.875939712077029,0.,0.482420584973746));
#30697=DIRECTION('',(0.,-1.,0.));
#30698=DIRECTION('',(-0.875939712077029,0.,0.482420584973746));
#30699=DIRECTION('center_axis',(0.,-1.,0.));
#30700=DIRECTION('ref_axis',(1.,0.,0.));
#30701=DIRECTION('center_axis',(0.,-1.,0.));
#30702=DIRECTION('ref_axis',(1.,0.,0.));
#30703=DIRECTION('',(0.,1.,0.));
#30704=DIRECTION('center_axis',(-0.62464840640047,0.,-0.780906120081891));
#30705=DIRECTION('ref_axis',(0.780906120081891,0.,-0.62464840640047));
#30706=DIRECTION('',(0.780906120081891,0.,-0.62464840640047));
#30707=DIRECTION('',(0.,-1.,0.));
#30708=DIRECTION('center_axis',(0.,-1.,0.));
#30709=DIRECTION('ref_axis',(-0.731143307127204,0.,0.6822239107823));
#30710=DIRECTION('',(0.,-1.,0.));
#30711=DIRECTION('center_axis',(0.,-1.,0.));
#30712=DIRECTION('ref_axis',(-0.731143307127204,0.,0.6822239107823));
#30713=DIRECTION('',(0.,-1.,0.));
#30714=DIRECTION('',(0.,-1.,0.));
#30715=DIRECTION('center_axis',(0.780906120081892,0.,0.62464840640047));
#30716=DIRECTION('ref_axis',(-0.62464840640047,0.,0.780906120081892));
#30717=DIRECTION('',(0.,-1.,0.));
#30718=DIRECTION('',(-0.62464840640047,0.,0.780906120081892));
#30719=DIRECTION('center_axis',(0.,-1.,0.));
#30720=DIRECTION('ref_axis',(1.,0.,0.));
#30721=DIRECTION('center_axis',(0.,-1.,0.));
#30722=DIRECTION('ref_axis',(1.,0.,0.));
#30723=DIRECTION('',(0.,1.,0.));
#30724=DIRECTION('center_axis',(0.960505777339176,0.,0.278260043301343));
#30725=DIRECTION('ref_axis',(-0.278260043301343,0.,0.960505777339176));
#30726=DIRECTION('',(0.,-1.,0.));
#30727=DIRECTION('',(0.,-1.,0.));
#30728=DIRECTION('',(-0.278260043301343,0.,0.960505777339176));
#30729=DIRECTION('center_axis',(-0.87593971207703,0.,-0.482420584973745));
#30730=DIRECTION('ref_axis',(0.482420584973745,0.,-0.87593971207703));
#30731=DIRECTION('',(0.482420584973745,0.,-0.87593971207703));
#30732=DIRECTION('',(0.,-1.,0.));
#30733=DIRECTION('center_axis',(0.,-1.,0.));
#30734=DIRECTION('ref_axis',(-0.414412548967732,0.,0.910089138083774));
#30735=DIRECTION('',(0.,-1.,0.));
#30736=DIRECTION('center_axis',(0.,-1.,0.));
#30737=DIRECTION('ref_axis',(-0.414412548967732,0.,0.910089138083774));
#30738=DIRECTION('',(0.,-1.,0.));
#30739=DIRECTION('center_axis',(0.,-1.,0.));
#30740=DIRECTION('ref_axis',(0.,0.,-1.));
#30741=DIRECTION('center_axis',(0.,-1.,0.));
#30742=DIRECTION('ref_axis',(1.,0.,0.));
#30743=DIRECTION('',(0.110490888956839,0.,0.993877137003124));
#30744=DIRECTION('center_axis',(0.,-1.,0.));
#30745=DIRECTION('ref_axis',(-0.0345912368870343,0.,0.999401544090575));
#30746=DIRECTION('',(0.110490888956839,0.,-0.993877137003125));
#30747=DIRECTION('center_axis',(0.,-1.,0.));
#30748=DIRECTION('ref_axis',(1.,0.,0.));
#30749=DIRECTION('center_axis',(0.,-1.,0.));
#30750=DIRECTION('ref_axis',(1.,0.,0.));
#30751=DIRECTION('center_axis',(0.,-1.,0.));
#30752=DIRECTION('ref_axis',(1.,0.,0.));
#30753=DIRECTION('',(0.,-1.,0.));
#30754=DIRECTION('center_axis',(0.993877137003125,0.,-0.110490888956839));
#30755=DIRECTION('ref_axis',(0.110490888956839,0.,0.993877137003125));
#30756=DIRECTION('',(0.,-1.,0.));
#30757=DIRECTION('center_axis',(0.,-1.,0.));
#30758=DIRECTION('ref_axis',(-0.0345912368870343,0.,0.999401544090575));
#30759=DIRECTION('',(0.,-1.,0.));
#30760=DIRECTION('',(0.,-1.,0.));
#30761=DIRECTION('center_axis',(-0.993877137003125,0.,-0.110490888956839));
#30762=DIRECTION('ref_axis',(0.110490888956839,0.,-0.993877137003125));
#30763=DIRECTION('',(0.,1.,0.));
#30764=DIRECTION('',(0.,-1.,0.));
#30765=DIRECTION('center_axis',(0.,-1.,0.));
#30766=DIRECTION('ref_axis',(1.,0.,0.));
#30767=DIRECTION('center_axis',(0.,-1.,0.));
#30768=DIRECTION('ref_axis',(0.,0.,-1.));
#30769=DIRECTION('center_axis',(0.,-1.,0.));
#30770=DIRECTION('ref_axis',(1.,0.,0.));
#30771=DIRECTION('center_axis',(0.,-1.,0.));
#30772=DIRECTION('ref_axis',(1.,0.,0.));
#30773=DIRECTION('center_axis',(0.,-1.,0.));
#30774=DIRECTION('ref_axis',(1.,0.,0.));
#30775=DIRECTION('center_axis',(0.,-1.,0.));
#30776=DIRECTION('ref_axis',(1.,0.,0.));
#30777=DIRECTION('',(0.,-1.,0.));
#30778=DIRECTION('center_axis',(0.,1.,0.));
#30779=DIRECTION('ref_axis',(0.,0.,1.));
#30780=DIRECTION('center_axis',(0.,-1.,0.));
#30781=DIRECTION('ref_axis',(1.,0.,0.));
#30782=DIRECTION('center_axis',(0.,-1.,0.));
#30783=DIRECTION('ref_axis',(1.,0.,0.));
#30784=DIRECTION('',(0.,-1.,0.));
#30785=DIRECTION('center_axis',(0.,-1.,0.));
#30786=DIRECTION('ref_axis',(1.,0.,0.));
#30787=DIRECTION('',(0.,-1.,0.));
#30788=DIRECTION('axis',(0.,0.,1.));
#30789=DIRECTION('refdir',(1.,0.,0.));
#30790=DIRECTION('center_axis',(0.,-1.,0.));
#30791=DIRECTION('ref_axis',(-0.160423232777043,0.,-0.987048320187701));
#30792=DIRECTION('',(0.,1.,0.));
#30793=DIRECTION('center_axis',(0.,1.,0.));
#30794=DIRECTION('ref_axis',(1.,0.,5.99026163859831E-14));
#30795=DIRECTION('center_axis',(0.,-1.,0.));
#30796=DIRECTION('ref_axis',(-0.160423232777043,0.,-0.987048320187701));
#30797=DIRECTION('',(0.,1.,0.));
#30798=DIRECTION('center_axis',(0.,-1.,0.));
#30799=DIRECTION('ref_axis',(-0.160423232777043,0.,-0.987048320187701));
#30800=DIRECTION('',(0.,1.,0.));
#30801=DIRECTION('center_axis',(0.,-1.,0.));
#30802=DIRECTION('ref_axis',(-0.160423232777043,0.,-0.987048320187701));
#30803=DIRECTION('',(0.,1.,0.));
#30804=DIRECTION('center_axis',(0.,-1.,0.));
#30805=DIRECTION('ref_axis',(-0.160423232777043,0.,-0.987048320187701));
#30806=DIRECTION('',(0.,1.,0.));
#30807=DIRECTION('center_axis',(0.,-1.,0.));
#30808=DIRECTION('ref_axis',(-0.160423232777043,0.,-0.987048320187701));
#30809=DIRECTION('',(0.,1.,0.));
#30810=DIRECTION('center_axis',(0.,-1.,0.));
#30811=DIRECTION('ref_axis',(-0.160423232777043,0.,-0.987048320187701));
#30812=DIRECTION('',(0.,1.,0.));
#30813=DIRECTION('center_axis',(0.,-1.,0.));
#30814=DIRECTION('ref_axis',(-0.160423232777043,0.,-0.987048320187701));
#30815=DIRECTION('',(0.,1.,0.));
#30816=DIRECTION('center_axis',(0.,-1.,0.));
#30817=DIRECTION('ref_axis',(-0.160423232777043,0.,-0.987048320187701));
#30818=DIRECTION('',(0.,1.,0.));
#30819=DIRECTION('center_axis',(0.,-1.,0.));
#30820=DIRECTION('ref_axis',(-0.160423232777043,0.,-0.987048320187701));
#30821=DIRECTION('',(0.,1.,0.));
#30822=DIRECTION('center_axis',(0.,-1.,0.));
#30823=DIRECTION('ref_axis',(-0.160423232777043,0.,-0.987048320187701));
#30824=DIRECTION('',(0.,1.,0.));
#30825=DIRECTION('center_axis',(0.,-1.,0.));
#30826=DIRECTION('ref_axis',(1.,0.,0.));
#30827=DIRECTION('',(0.,1.,0.));
#30828=DIRECTION('center_axis',(0.,1.,0.));
#30829=DIRECTION('ref_axis',(1.,0.,0.));
#30830=DIRECTION('center_axis',(0.,-1.,0.));
#30831=DIRECTION('ref_axis',(1.,0.,0.));
#30832=DIRECTION('',(0.,1.,0.));
#30833=DIRECTION('center_axis',(0.,-1.,0.));
#30834=DIRECTION('ref_axis',(1.,0.,0.));
#30835=DIRECTION('',(0.,1.,0.));
#30836=DIRECTION('center_axis',(0.,-1.,0.));
#30837=DIRECTION('ref_axis',(1.,0.,0.));
#30838=DIRECTION('',(0.,1.,0.));
#30839=DIRECTION('center_axis',(0.,-1.,0.));
#30840=DIRECTION('ref_axis',(1.,0.,0.));
#30841=DIRECTION('',(0.,1.,0.));
#30842=DIRECTION('center_axis',(0.,-1.,0.));
#30843=DIRECTION('ref_axis',(1.,0.,0.));
#30844=DIRECTION('',(0.,1.,0.));
#30845=DIRECTION('center_axis',(0.,-1.,0.));
#30846=DIRECTION('ref_axis',(1.,0.,0.));
#30847=DIRECTION('',(0.,1.,0.));
#30848=DIRECTION('center_axis',(0.,-1.,0.));
#30849=DIRECTION('ref_axis',(1.,0.,0.));
#30850=DIRECTION('',(0.,1.,0.));
#30851=DIRECTION('center_axis',(0.,-1.,0.));
#30852=DIRECTION('ref_axis',(1.,0.,0.));
#30853=DIRECTION('',(0.,1.,0.));
#30854=DIRECTION('center_axis',(0.,-1.,0.));
#30855=DIRECTION('ref_axis',(1.,0.,0.));
#30856=DIRECTION('',(0.,1.,0.));
#30857=DIRECTION('center_axis',(0.,-1.,0.));
#30858=DIRECTION('ref_axis',(1.,0.,0.));
#30859=DIRECTION('',(0.,1.,0.));
#30860=DIRECTION('center_axis',(0.,-1.,0.));
#30861=DIRECTION('ref_axis',(1.,0.,0.));
#30862=DIRECTION('center_axis',(0.,-1.,0.));
#30863=DIRECTION('ref_axis',(1.,0.,0.));
#30864=DIRECTION('center_axis',(0.,-1.,0.));
#30865=DIRECTION('ref_axis',(-0.160423232777043,0.,-0.987048320187701));
#30866=DIRECTION('center_axis',(0.,-1.,0.));
#30867=DIRECTION('ref_axis',(1.,0.,5.99026163859831E-14));
#30868=DIRECTION('center_axis',(0.,1.,0.));
#30869=DIRECTION('ref_axis',(0.,0.,1.));
#30870=DIRECTION('center_axis',(0.,-1.,0.));
#30871=DIRECTION('ref_axis',(1.,0.,0.));
#30872=DIRECTION('center_axis',(0.,-1.,0.));
#30873=DIRECTION('ref_axis',(1.,0.,0.));
#30874=DIRECTION('center_axis',(0.,1.,0.));
#30875=DIRECTION('ref_axis',(0.,0.,1.));
#30876=DIRECTION('center_axis',(0.,1.,0.));
#30877=DIRECTION('ref_axis',(1.,0.,0.));
#30878=DIRECTION('center_axis',(0.,1.,0.));
#30879=DIRECTION('ref_axis',(1.,0.,0.));
#30880=DIRECTION('center_axis',(0.,1.,0.));
#30881=DIRECTION('ref_axis',(0.,0.,1.));
#30882=DIRECTION('center_axis',(0.,-1.,0.));
#30883=DIRECTION('ref_axis',(1.,0.,0.));
#30884=DIRECTION('center_axis',(1.,0.,-1.22464679914735E-16));
#30885=DIRECTION('ref_axis',(-1.22464679914735E-16,0.,-1.));
#30886=DIRECTION('center_axis',(0.,1.,0.));
#30887=DIRECTION('ref_axis',(1.,0.,0.));
#30888=DIRECTION('center_axis',(0.,1.,0.));
#30889=DIRECTION('ref_axis',(1.,0.,0.));
#30890=DIRECTION('center_axis',(0.,1.,0.));
#30891=DIRECTION('ref_axis',(1.,0.,0.));
#30892=DIRECTION('',(0.707106781186546,-0.707106781186549,-8.65956056235491E-17));
#30893=DIRECTION('center_axis',(0.,1.,0.));
#30894=DIRECTION('ref_axis',(1.,0.,0.));
#30895=DIRECTION('center_axis',(0.,1.,0.));
#30896=DIRECTION('ref_axis',(1.,0.,0.));
#30897=DIRECTION('center_axis',(-0.49353398197848,0.,-0.869726513699833));
#30898=DIRECTION('ref_axis',(0.869726513699833,0.,-0.49353398197848));
#30899=DIRECTION('',(0.,-1.,0.));
#30900=DIRECTION('',(0.869726513699833,0.,-0.49353398197848));
#30901=DIRECTION('',(0.,-1.,0.));
#30902=DIRECTION('center_axis',(0.,-1.,0.));
#30903=DIRECTION('ref_axis',(-0.17364817766693,0.,-0.984807753012208));
#30904=DIRECTION('center_axis',(0.,-1.,0.));
#30905=DIRECTION('ref_axis',(1.,0.,0.));
#30906=DIRECTION('',(-0.986074150277955,0.,-0.166306254102512));
#30907=DIRECTION('center_axis',(-0.166306254102512,0.,0.986074150277955));
#30908=DIRECTION('ref_axis',(-0.986074150277955,0.,-0.166306254102512));
#30909=DIRECTION('',(0.,1.,0.));
#30910=DIRECTION('center_axis',(0.,1.,0.));
#30911=DIRECTION('ref_axis',(1.,0.,0.));
#30912=DIRECTION('center_axis',(0.,-1.,0.));
#30913=DIRECTION('ref_axis',(1.,0.,0.));
#30914=DIRECTION('',(0.,-1.,0.));
#30915=DIRECTION('center_axis',(0.,-1.,0.));
#30916=DIRECTION('ref_axis',(1.,0.,0.));
#30917=DIRECTION('center_axis',(0.,-1.,0.));
#30918=DIRECTION('ref_axis',(1.,0.,0.));
#30919=DIRECTION('center_axis',(0.,-1.,0.));
#30920=DIRECTION('ref_axis',(1.,0.,0.));
#30921=DIRECTION('',(0.,1.,0.));
#30922=DIRECTION('center_axis',(0.,1.,0.));
#30923=DIRECTION('ref_axis',(1.,0.,0.));
#30924=DIRECTION('',(0.,-1.,0.));
#30925=DIRECTION('center_axis',(0.,-1.,0.));
#30926=DIRECTION('ref_axis',(1.,0.,0.));
#30927=DIRECTION('',(0.,1.,0.));
#30928=DIRECTION('center_axis',(0.,1.,0.));
#30929=DIRECTION('ref_axis',(1.,0.,0.));
#30930=DIRECTION('',(0.,-1.,0.));
#30931=DIRECTION('center_axis',(0.,-1.,0.));
#30932=DIRECTION('ref_axis',(1.,0.,0.));
#30933=DIRECTION('',(0.,1.,0.));
#30934=DIRECTION('center_axis',(0.,1.,0.));
#30935=DIRECTION('ref_axis',(1.,0.,0.));
#30936=DIRECTION('',(0.,-1.,0.));
#30937=DIRECTION('center_axis',(0.,-1.,0.));
#30938=DIRECTION('ref_axis',(1.,0.,0.));
#30939=DIRECTION('',(0.,1.,0.));
#30940=DIRECTION('center_axis',(0.,1.,0.));
#30941=DIRECTION('ref_axis',(1.,0.,0.));
#30942=DIRECTION('',(0.,-1.,0.));
#30943=DIRECTION('center_axis',(0.,-1.,0.));
#30944=DIRECTION('ref_axis',(1.,0.,0.));
#30945=DIRECTION('',(0.,1.,0.));
#30946=DIRECTION('center_axis',(0.,1.,0.));
#30947=DIRECTION('ref_axis',(1.,0.,0.));
#30948=DIRECTION('',(0.,-1.,0.));
#30949=DIRECTION('center_axis',(0.,-1.,0.));
#30950=DIRECTION('ref_axis',(1.,0.,0.));
#30951=DIRECTION('',(0.,1.,0.));
#30952=DIRECTION('center_axis',(0.,1.,0.));
#30953=DIRECTION('ref_axis',(1.,0.,0.));
#30954=DIRECTION('',(0.,-1.,0.));
#30955=DIRECTION('center_axis',(0.,-1.,0.));
#30956=DIRECTION('ref_axis',(1.,0.,0.));
#30957=DIRECTION('',(0.,1.,0.));
#30958=DIRECTION('center_axis',(0.,1.,0.));
#30959=DIRECTION('ref_axis',(1.,0.,0.));
#30960=DIRECTION('',(0.,-1.,0.));
#30961=DIRECTION('center_axis',(0.,-1.,0.));
#30962=DIRECTION('ref_axis',(1.,0.,0.));
#30963=DIRECTION('',(0.,1.,0.));
#30964=DIRECTION('center_axis',(0.,1.,0.));
#30965=DIRECTION('ref_axis',(1.,0.,0.));
#30966=DIRECTION('',(0.,-1.,0.));
#30967=DIRECTION('center_axis',(0.,-1.,0.));
#30968=DIRECTION('ref_axis',(1.,0.,0.));
#30969=DIRECTION('',(0.,1.,0.));
#30970=DIRECTION('center_axis',(0.,1.,0.));
#30971=DIRECTION('ref_axis',(1.,0.,0.));
#30972=DIRECTION('',(0.,-1.,0.));
#30973=DIRECTION('center_axis',(0.,-1.,0.));
#30974=DIRECTION('ref_axis',(1.,0.,0.));
#30975=DIRECTION('',(0.,1.,0.));
#30976=DIRECTION('center_axis',(0.,1.,0.));
#30977=DIRECTION('ref_axis',(1.,0.,0.));
#30978=DIRECTION('',(0.,-1.,0.));
#30979=DIRECTION('center_axis',(0.,-1.,0.));
#30980=DIRECTION('ref_axis',(1.,0.,0.));
#30981=DIRECTION('',(0.,1.,0.));
#30982=DIRECTION('center_axis',(0.,1.,0.));
#30983=DIRECTION('ref_axis',(1.,0.,0.));
#30984=DIRECTION('',(0.,-1.,0.));
#30985=DIRECTION('center_axis',(0.,-1.,0.));
#30986=DIRECTION('ref_axis',(1.,0.,0.));
#30987=DIRECTION('',(0.,1.,0.));
#30988=DIRECTION('center_axis',(0.,1.,0.));
#30989=DIRECTION('ref_axis',(1.,0.,0.));
#30990=DIRECTION('',(0.,-1.,0.));
#30991=DIRECTION('center_axis',(0.,-1.,0.));
#30992=DIRECTION('ref_axis',(1.,0.,0.));
#30993=DIRECTION('',(0.,1.,0.));
#30994=DIRECTION('center_axis',(0.,1.,0.));
#30995=DIRECTION('ref_axis',(1.,0.,0.));
#30996=DIRECTION('',(0.,-1.,0.));
#30997=DIRECTION('center_axis',(0.,-1.,0.));
#30998=DIRECTION('ref_axis',(1.,0.,0.));
#30999=DIRECTION('',(0.,1.,0.));
#31000=DIRECTION('center_axis',(0.,1.,0.));
#31001=DIRECTION('ref_axis',(1.,0.,0.));
#31002=DIRECTION('',(0.,-1.,0.));
#31003=DIRECTION('center_axis',(0.,-1.,0.));
#31004=DIRECTION('ref_axis',(1.,0.,0.));
#31005=DIRECTION('',(0.,1.,0.));
#31006=DIRECTION('center_axis',(0.,1.,0.));
#31007=DIRECTION('ref_axis',(1.,0.,0.));
#31008=DIRECTION('',(0.,-1.,0.));
#31009=DIRECTION('center_axis',(0.,-1.,0.));
#31010=DIRECTION('ref_axis',(1.,0.,0.));
#31011=DIRECTION('',(0.,1.,0.));
#31012=DIRECTION('center_axis',(0.,1.,0.));
#31013=DIRECTION('ref_axis',(1.,0.,0.));
#31014=DIRECTION('',(0.,-1.,0.));
#31015=DIRECTION('center_axis',(0.,-1.,0.));
#31016=DIRECTION('ref_axis',(1.,0.,0.));
#31017=DIRECTION('',(0.,1.,0.));
#31018=DIRECTION('center_axis',(0.,1.,0.));
#31019=DIRECTION('ref_axis',(1.,0.,0.));
#31020=DIRECTION('center_axis',(0.,1.,0.));
#31021=DIRECTION('ref_axis',(1.,0.,0.));
#31022=DIRECTION('',(0.,-1.,0.));
#31023=DIRECTION('center_axis',(0.,-1.,0.));
#31024=DIRECTION('ref_axis',(1.,0.,0.));
#31025=DIRECTION('',(0.,1.,0.));
#31026=DIRECTION('center_axis',(0.,1.,0.));
#31027=DIRECTION('ref_axis',(1.,0.,0.));
#31028=DIRECTION('',(0.,-1.,0.));
#31029=DIRECTION('center_axis',(0.,-1.,0.));
#31030=DIRECTION('ref_axis',(1.,0.,0.));
#31031=DIRECTION('',(0.,1.,0.));
#31032=DIRECTION('center_axis',(0.,1.,0.));
#31033=DIRECTION('ref_axis',(1.,0.,0.));
#31034=DIRECTION('',(0.,-1.,0.));
#31035=DIRECTION('center_axis',(0.,-1.,0.));
#31036=DIRECTION('ref_axis',(1.,0.,0.));
#31037=DIRECTION('',(0.,1.,0.));
#31038=DIRECTION('center_axis',(0.,1.,0.));
#31039=DIRECTION('ref_axis',(1.,0.,0.));
#31040=DIRECTION('',(0.,-1.,0.));
#31041=DIRECTION('center_axis',(0.,-1.,0.));
#31042=DIRECTION('ref_axis',(1.,0.,0.));
#31043=DIRECTION('',(0.,1.,0.));
#31044=DIRECTION('center_axis',(0.,1.,0.));
#31045=DIRECTION('ref_axis',(1.,0.,0.));
#31046=DIRECTION('',(0.,-1.,0.));
#31047=DIRECTION('center_axis',(0.,-1.,0.));
#31048=DIRECTION('ref_axis',(1.,0.,0.));
#31049=DIRECTION('',(0.,1.,0.));
#31050=DIRECTION('center_axis',(0.,1.,0.));
#31051=DIRECTION('ref_axis',(1.,0.,0.));
#31052=DIRECTION('',(0.,-1.,0.));
#31053=DIRECTION('center_axis',(0.,-1.,0.));
#31054=DIRECTION('ref_axis',(1.,0.,0.));
#31055=DIRECTION('',(0.,1.,0.));
#31056=DIRECTION('center_axis',(0.,1.,0.));
#31057=DIRECTION('ref_axis',(1.,0.,0.));
#31058=DIRECTION('',(0.,-1.,0.));
#31059=DIRECTION('center_axis',(0.,-1.,0.));
#31060=DIRECTION('ref_axis',(1.,0.,0.));
#31061=DIRECTION('',(0.,1.,0.));
#31062=DIRECTION('center_axis',(0.,1.,0.));
#31063=DIRECTION('ref_axis',(1.,0.,0.));
#31064=DIRECTION('',(0.,-1.,0.));
#31065=DIRECTION('center_axis',(0.,-1.,0.));
#31066=DIRECTION('ref_axis',(1.,0.,0.));
#31067=DIRECTION('',(0.,1.,0.));
#31068=DIRECTION('center_axis',(0.,1.,0.));
#31069=DIRECTION('ref_axis',(1.,0.,0.));
#31070=DIRECTION('',(0.,-1.,0.));
#31071=DIRECTION('center_axis',(0.,-1.,0.));
#31072=DIRECTION('ref_axis',(1.,0.,0.));
#31073=DIRECTION('',(0.,1.,0.));
#31074=DIRECTION('center_axis',(0.,1.,0.));
#31075=DIRECTION('ref_axis',(1.,0.,0.));
#31076=DIRECTION('',(0.,-1.,0.));
#31077=DIRECTION('center_axis',(0.,-1.,0.));
#31078=DIRECTION('ref_axis',(1.,0.,0.));
#31079=DIRECTION('',(0.,1.,0.));
#31080=DIRECTION('center_axis',(0.,1.,0.));
#31081=DIRECTION('ref_axis',(1.,0.,0.));
#31082=DIRECTION('',(0.,-1.,0.));
#31083=DIRECTION('center_axis',(0.,-1.,0.));
#31084=DIRECTION('ref_axis',(1.,0.,0.));
#31085=DIRECTION('',(0.,1.,0.));
#31086=DIRECTION('center_axis',(0.,1.,0.));
#31087=DIRECTION('ref_axis',(1.,0.,0.));
#31088=DIRECTION('',(0.,-1.,0.));
#31089=DIRECTION('center_axis',(0.,-1.,0.));
#31090=DIRECTION('ref_axis',(1.,0.,0.));
#31091=DIRECTION('',(0.,1.,0.));
#31092=DIRECTION('center_axis',(0.,1.,0.));
#31093=DIRECTION('ref_axis',(1.,0.,0.));
#31094=DIRECTION('',(0.,-1.,0.));
#31095=DIRECTION('center_axis',(0.,-1.,0.));
#31096=DIRECTION('ref_axis',(1.,0.,0.));
#31097=DIRECTION('',(0.,1.,0.));
#31098=DIRECTION('center_axis',(0.,1.,0.));
#31099=DIRECTION('ref_axis',(1.,0.,0.));
#31100=DIRECTION('',(0.,-1.,0.));
#31101=DIRECTION('center_axis',(0.,-1.,0.));
#31102=DIRECTION('ref_axis',(1.,0.,0.));
#31103=DIRECTION('',(0.,1.,0.));
#31104=DIRECTION('center_axis',(0.,1.,0.));
#31105=DIRECTION('ref_axis',(1.,0.,0.));
#31106=DIRECTION('',(0.,-1.,0.));
#31107=DIRECTION('center_axis',(0.,-1.,0.));
#31108=DIRECTION('ref_axis',(1.,0.,0.));
#31109=DIRECTION('',(0.,1.,0.));
#31110=DIRECTION('center_axis',(0.,1.,0.));
#31111=DIRECTION('ref_axis',(1.,0.,0.));
#31112=DIRECTION('',(0.,-1.,0.));
#31113=DIRECTION('center_axis',(0.,-1.,0.));
#31114=DIRECTION('ref_axis',(1.,0.,0.));
#31115=DIRECTION('',(0.,1.,0.));
#31116=DIRECTION('center_axis',(0.,1.,0.));
#31117=DIRECTION('ref_axis',(1.,0.,0.));
#31118=DIRECTION('',(0.,-1.,0.));
#31119=DIRECTION('center_axis',(0.,-1.,0.));
#31120=DIRECTION('ref_axis',(1.,0.,0.));
#31121=DIRECTION('',(0.,1.,0.));
#31122=DIRECTION('center_axis',(0.,1.,0.));
#31123=DIRECTION('ref_axis',(1.,0.,0.));
#31124=DIRECTION('',(0.,-1.,0.));
#31125=DIRECTION('center_axis',(0.,-1.,0.));
#31126=DIRECTION('ref_axis',(1.,0.,0.));
#31127=DIRECTION('',(0.,1.,0.));
#31128=DIRECTION('center_axis',(0.,1.,0.));
#31129=DIRECTION('ref_axis',(1.,0.,0.));
#31130=DIRECTION('',(0.,-1.,0.));
#31131=DIRECTION('center_axis',(-0.637062515999983,0.,-0.770812137104607));
#31132=DIRECTION('ref_axis',(0.770812137104607,0.,-0.637062515999983));
#31133=DIRECTION('',(0.,-1.,0.));
#31134=DIRECTION('',(0.770812137104607,0.,-0.637062515999983));
#31135=DIRECTION('center_axis',(0.,-1.,0.));
#31136=DIRECTION('ref_axis',(-0.342020143325669,0.,-0.939692620785908));
#31137=DIRECTION('',(-0.99997224619817,0.,0.00745029082566251));
#31138=DIRECTION('center_axis',(0.00745029082566245,0.,0.99997224619817));
#31139=DIRECTION('ref_axis',(-0.99997224619817,0.,0.00745029082566245));
#31140=DIRECTION('center_axis',(-0.761234227842014,0.,-0.648477023773219));
#31141=DIRECTION('ref_axis',(0.648477023773219,0.,-0.761234227842014));
#31142=DIRECTION('',(0.,-1.,0.));
#31143=DIRECTION('',(0.648477023773219,0.,-0.761234227842014));
#31144=DIRECTION('center_axis',(0.,-1.,0.));
#31145=DIRECTION('ref_axis',(-0.5,0.,-0.866025403784438));
#31146=DIRECTION('',(-0.983486691428025,0.,0.180980462437127));
#31147=DIRECTION('center_axis',(0.180980462437127,0.,0.983486691428025));
#31148=DIRECTION('ref_axis',(-0.983486691428025,0.,0.180980462437127));
#31149=DIRECTION('center_axis',(-0.862276222874171,0.,-0.50643826421969));
#31150=DIRECTION('ref_axis',(0.50643826421969,0.,-0.862276222874171));
#31151=DIRECTION('',(0.,-1.,0.));
#31152=DIRECTION('',(0.50643826421969,0.,-0.862276222874171));
#31153=DIRECTION('center_axis',(0.,-1.,0.));
#31154=DIRECTION('ref_axis',(-0.64278760968654,0.,-0.766044443118978));
#31155=DIRECTION('',(-0.937118391207119,0.,0.349011634277972));
#31156=DIRECTION('center_axis',(0.349011634277973,0.,0.937118391207119));
#31157=DIRECTION('ref_axis',(-0.937118391207119,0.,0.349011634277973));
#31158=DIRECTION('center_axis',(-0.937118391207119,0.,-0.349011634277972));
#31159=DIRECTION('ref_axis',(0.349011634277972,0.,-0.937118391207119));
#31160=DIRECTION('',(0.,-1.,0.));
#31161=DIRECTION('',(0.349011634277972,0.,-0.937118391207119));
#31162=DIRECTION('center_axis',(0.,-1.,0.));
#31163=DIRECTION('ref_axis',(-0.766044443118978,0.,-0.642787609686539));
#31164=DIRECTION('',(-0.862276222874171,0.,0.50643826421969));
#31165=DIRECTION('center_axis',(0.50643826421969,0.,0.862276222874171));
#31166=DIRECTION('ref_axis',(-0.862276222874171,0.,0.50643826421969));
#31167=DIRECTION('center_axis',(-0.983486691428025,0.,-0.180980462437127));
#31168=DIRECTION('ref_axis',(0.180980462437127,0.,-0.983486691428025));
#31169=DIRECTION('',(0.,-1.,0.));
#31170=DIRECTION('',(0.180980462437127,0.,-0.983486691428025));
#31171=DIRECTION('center_axis',(0.,-1.,0.));
#31172=DIRECTION('ref_axis',(-0.866025403784439,0.,-0.5));
#31173=DIRECTION('',(-0.761234227842014,0.,0.64847702377322));
#31174=DIRECTION('center_axis',(0.648477023773219,0.,0.761234227842014));
#31175=DIRECTION('ref_axis',(-0.761234227842014,0.,0.648477023773219));
#31176=DIRECTION('center_axis',(-0.99997224619817,0.,-0.00745029082566118));
#31177=DIRECTION('ref_axis',(0.00745029082566118,0.,-0.99997224619817));
#31178=DIRECTION('',(0.,-1.,0.));
#31179=DIRECTION('',(0.00745029082566118,0.,-0.99997224619817));
#31180=DIRECTION('center_axis',(0.,-1.,0.));
#31181=DIRECTION('ref_axis',(-0.939692620785909,0.,-0.342020143325668));
#31182=DIRECTION('',(-0.637062515999982,0.,0.770812137104608));
#31183=DIRECTION('center_axis',(0.770812137104608,0.,0.637062515999982));
#31184=DIRECTION('ref_axis',(-0.637062515999982,0.,0.770812137104608));
#31185=DIRECTION('center_axis',(-0.986074150277955,0.,0.166306254102512));
#31186=DIRECTION('ref_axis',(-0.166306254102512,0.,-0.986074150277955));
#31187=DIRECTION('',(0.,-1.,0.));
#31188=DIRECTION('',(-0.166306254102512,0.,-0.986074150277955));
#31189=DIRECTION('center_axis',(0.,-1.,0.));
#31190=DIRECTION('ref_axis',(-0.984807753012208,0.,-0.17364817766693));
#31191=DIRECTION('',(-0.493533981978479,0.,0.869726513699833));
#31192=DIRECTION('center_axis',(0.869726513699833,0.,0.493533981978479));
#31193=DIRECTION('ref_axis',(-0.493533981978479,0.,0.869726513699833));
#31194=DIRECTION('center_axis',(-0.942214690279141,0.,0.335009667654806));
#31195=DIRECTION('ref_axis',(-0.335009667654806,0.,-0.94221469027914));
#31196=DIRECTION('',(0.,-1.,0.));
#31197=DIRECTION('',(-0.335009667654806,0.,-0.94221469027914));
#31198=DIRECTION('center_axis',(0.,-1.,0.));
#31199=DIRECTION('ref_axis',(-1.,0.,1.83697019872103E-16));
#31200=DIRECTION('',(-0.335009667654805,0.,0.942214690279141));
#31201=DIRECTION('center_axis',(0.942214690279141,0.,0.335009667654805));
#31202=DIRECTION('ref_axis',(-0.335009667654805,0.,0.942214690279141));
#31203=DIRECTION('center_axis',(-0.869726513699833,0.,0.49353398197848));
#31204=DIRECTION('ref_axis',(-0.49353398197848,0.,-0.869726513699833));
#31205=DIRECTION('',(0.,-1.,0.));
#31206=DIRECTION('',(-0.49353398197848,0.,-0.869726513699833));
#31207=DIRECTION('center_axis',(0.,-1.,0.));
#31208=DIRECTION('ref_axis',(-0.984807753012208,0.,0.17364817766693));
#31209=DIRECTION('',(-0.166306254102512,0.,0.986074150277955));
#31210=DIRECTION('center_axis',(0.986074150277955,0.,0.166306254102512));
#31211=DIRECTION('ref_axis',(-0.166306254102512,0.,0.986074150277955));
#31212=DIRECTION('center_axis',(-0.770812137104607,0.,0.637062515999983));
#31213=DIRECTION('ref_axis',(-0.637062515999983,0.,-0.770812137104607));
#31214=DIRECTION('',(0.,-1.,0.));
#31215=DIRECTION('',(-0.637062515999983,0.,-0.770812137104607));
#31216=DIRECTION('center_axis',(0.,-1.,0.));
#31217=DIRECTION('ref_axis',(-0.939692620785908,0.,0.342020143325669));
#31218=DIRECTION('',(0.0074502908256624,0.,0.99997224619817));
#31219=DIRECTION('center_axis',(0.99997224619817,0.,-0.00745029082566234));
#31220=DIRECTION('ref_axis',(0.00745029082566234,0.,0.99997224619817));
#31221=DIRECTION('center_axis',(-0.648477023773219,0.,0.761234227842014));
#31222=DIRECTION('ref_axis',(-0.761234227842014,0.,-0.648477023773219));
#31223=DIRECTION('',(0.,-1.,0.));
#31224=DIRECTION('',(-0.761234227842014,0.,-0.648477023773219));
#31225=DIRECTION('center_axis',(0.,-1.,0.));
#31226=DIRECTION('ref_axis',(-0.866025403784438,0.,0.5));
#31227=DIRECTION('',(0.180980462437127,0.,0.983486691428025));
#31228=DIRECTION('center_axis',(0.983486691428025,0.,-0.180980462437127));
#31229=DIRECTION('ref_axis',(0.180980462437127,0.,0.983486691428025));
#31230=DIRECTION('center_axis',(-0.50643826421969,0.,0.862276222874171));
#31231=DIRECTION('ref_axis',(-0.862276222874171,0.,-0.50643826421969));
#31232=DIRECTION('',(0.,-1.,0.));
#31233=DIRECTION('',(-0.862276222874171,0.,-0.50643826421969));
#31234=DIRECTION('center_axis',(0.,-1.,0.));
#31235=DIRECTION('ref_axis',(-0.766044443118978,0.,0.642787609686539));
#31236=DIRECTION('',(0.349011634277972,0.,0.937118391207119));
#31237=DIRECTION('center_axis',(0.937118391207119,0.,-0.349011634277972));
#31238=DIRECTION('ref_axis',(0.349011634277972,0.,0.937118391207119));
#31239=DIRECTION('center_axis',(-0.349011634277972,0.,0.937118391207119));
#31240=DIRECTION('ref_axis',(-0.937118391207119,0.,-0.349011634277972));
#31241=DIRECTION('',(0.,-1.,0.));
#31242=DIRECTION('',(-0.937118391207119,0.,-0.349011634277972));
#31243=DIRECTION('center_axis',(0.,-1.,0.));
#31244=DIRECTION('ref_axis',(-0.642787609686539,0.,0.766044443118978));
#31245=DIRECTION('',(0.50643826421969,0.,0.862276222874171));
#31246=DIRECTION('center_axis',(0.862276222874171,0.,-0.50643826421969));
#31247=DIRECTION('ref_axis',(0.50643826421969,0.,0.862276222874171));
#31248=DIRECTION('center_axis',(-0.180980462437126,0.,0.983486691428025));
#31249=DIRECTION('ref_axis',(-0.983486691428025,0.,-0.180980462437126));
#31250=DIRECTION('',(0.,-1.,0.));
#31251=DIRECTION('',(-0.983486691428025,0.,-0.180980462437126));
#31252=DIRECTION('center_axis',(0.,-1.,0.));
#31253=DIRECTION('ref_axis',(-0.5,0.,0.866025403784439));
#31254=DIRECTION('',(0.64847702377322,0.,0.761234227842014));
#31255=DIRECTION('center_axis',(0.761234227842014,0.,-0.64847702377322));
#31256=DIRECTION('ref_axis',(0.64847702377322,0.,0.761234227842014));
#31257=DIRECTION('center_axis',(-0.00745029082566162,0.,0.99997224619817));
#31258=DIRECTION('ref_axis',(-0.99997224619817,0.,-0.00745029082566162));
#31259=DIRECTION('',(0.,-1.,0.));
#31260=DIRECTION('',(-0.99997224619817,0.,-0.00745029082566162));
#31261=DIRECTION('center_axis',(0.,-1.,0.));
#31262=DIRECTION('ref_axis',(-0.342020143325669,0.,0.939692620785908));
#31263=DIRECTION('',(0.770812137104607,0.,0.637062515999983));
#31264=DIRECTION('center_axis',(0.637062515999983,0.,-0.770812137104607));
#31265=DIRECTION('ref_axis',(0.770812137104607,0.,0.637062515999983));
#31266=DIRECTION('center_axis',(0.166306254102512,0.,0.986074150277955));
#31267=DIRECTION('ref_axis',(-0.986074150277955,0.,0.166306254102512));
#31268=DIRECTION('',(0.,-1.,0.));
#31269=DIRECTION('',(-0.986074150277955,0.,0.166306254102512));
#31270=DIRECTION('center_axis',(0.,-1.,0.));
#31271=DIRECTION('ref_axis',(-0.17364817766693,0.,0.984807753012208));
#31272=DIRECTION('',(0.869726513699833,0.,0.493533981978479));
#31273=DIRECTION('center_axis',(0.493533981978479,0.,-0.869726513699833));
#31274=DIRECTION('ref_axis',(0.869726513699833,0.,0.493533981978479));
#31275=DIRECTION('center_axis',(0.335009667654806,0.,0.942214690279141));
#31276=DIRECTION('ref_axis',(-0.94221469027914,0.,0.335009667654806));
#31277=DIRECTION('',(0.,-1.,0.));
#31278=DIRECTION('',(-0.94221469027914,0.,0.335009667654806));
#31279=DIRECTION('center_axis',(0.,-1.,0.));
#31280=DIRECTION('ref_axis',(1.22464679914735E-16,0.,1.));
#31281=DIRECTION('',(0.94221469027914,0.,0.335009667654806));
#31282=DIRECTION('center_axis',(0.335009667654806,0.,-0.942214690279141));
#31283=DIRECTION('ref_axis',(0.94221469027914,0.,0.335009667654806));
#31284=DIRECTION('center_axis',(0.49353398197848,0.,0.869726513699833));
#31285=DIRECTION('ref_axis',(-0.869726513699833,0.,0.49353398197848));
#31286=DIRECTION('',(0.,-1.,0.));
#31287=DIRECTION('',(-0.869726513699833,0.,0.49353398197848));
#31288=DIRECTION('center_axis',(0.,-1.,0.));
#31289=DIRECTION('ref_axis',(0.173648177666931,0.,0.984807753012208));
#31290=DIRECTION('',(0.986074150277955,0.,0.166306254102511));
#31291=DIRECTION('center_axis',(0.166306254102511,0.,-0.986074150277955));
#31292=DIRECTION('ref_axis',(0.986074150277955,0.,0.166306254102511));
#31293=DIRECTION('center_axis',(0.637062515999983,0.,0.770812137104607));
#31294=DIRECTION('ref_axis',(-0.770812137104607,0.,0.637062515999983));
#31295=DIRECTION('',(0.,-1.,0.));
#31296=DIRECTION('',(-0.770812137104607,0.,0.637062515999983));
#31297=DIRECTION('center_axis',(0.,-1.,0.));
#31298=DIRECTION('ref_axis',(0.342020143325669,0.,0.939692620785908));
#31299=DIRECTION('',(0.99997224619817,0.,-0.0074502908256619));
#31300=DIRECTION('center_axis',(-0.0074502908256619,0.,-0.99997224619817));
#31301=DIRECTION('ref_axis',(0.99997224619817,0.,-0.0074502908256619));
#31302=DIRECTION('center_axis',(0.761234227842014,0.,0.64847702377322));
#31303=DIRECTION('ref_axis',(-0.64847702377322,0.,0.761234227842014));
#31304=DIRECTION('',(0.,-1.,0.));
#31305=DIRECTION('',(-0.64847702377322,0.,0.761234227842014));
#31306=DIRECTION('center_axis',(0.,-1.,0.));
#31307=DIRECTION('ref_axis',(0.5,0.,0.866025403784439));
#31308=DIRECTION('',(0.983486691428025,0.,-0.180980462437127));
#31309=DIRECTION('center_axis',(-0.180980462437127,0.,-0.983486691428025));
#31310=DIRECTION('ref_axis',(0.983486691428025,0.,-0.180980462437127));
#31311=DIRECTION('center_axis',(0.862276222874171,0.,0.50643826421969));
#31312=DIRECTION('ref_axis',(-0.50643826421969,0.,0.862276222874171));
#31313=DIRECTION('',(0.,-1.,0.));
#31314=DIRECTION('',(-0.50643826421969,0.,0.862276222874171));
#31315=DIRECTION('center_axis',(0.,-1.,0.));
#31316=DIRECTION('ref_axis',(0.642787609686539,0.,0.766044443118978));
#31317=DIRECTION('',(0.937118391207119,0.,-0.349011634277972));
#31318=DIRECTION('center_axis',(-0.349011634277972,0.,-0.937118391207119));
#31319=DIRECTION('ref_axis',(0.937118391207119,0.,-0.349011634277972));
#31320=DIRECTION('center_axis',(0.937118391207119,0.,0.349011634277972));
#31321=DIRECTION('ref_axis',(-0.349011634277972,0.,0.937118391207119));
#31322=DIRECTION('',(0.,-1.,0.));
#31323=DIRECTION('',(-0.349011634277972,0.,0.937118391207119));
#31324=DIRECTION('center_axis',(0.,-1.,0.));
#31325=DIRECTION('ref_axis',(0.766044443118978,0.,0.642787609686539));
#31326=DIRECTION('',(0.862276222874171,0.,-0.50643826421969));
#31327=DIRECTION('center_axis',(-0.50643826421969,0.,-0.862276222874171));
#31328=DIRECTION('ref_axis',(0.862276222874171,0.,-0.50643826421969));
#31329=DIRECTION('center_axis',(0.983486691428025,0.,0.180980462437126));
#31330=DIRECTION('ref_axis',(-0.180980462437126,0.,0.983486691428025));
#31331=DIRECTION('',(0.,-1.,0.));
#31332=DIRECTION('',(-0.180980462437126,0.,0.983486691428025));
#31333=DIRECTION('center_axis',(0.,-1.,0.));
#31334=DIRECTION('ref_axis',(0.866025403784439,0.,0.5));
#31335=DIRECTION('',(0.761234227842014,0.,-0.64847702377322));
#31336=DIRECTION('center_axis',(-0.64847702377322,0.,-0.761234227842014));
#31337=DIRECTION('ref_axis',(0.761234227842014,0.,-0.64847702377322));
#31338=DIRECTION('center_axis',(0.99997224619817,0.,0.00745029082566168));
#31339=DIRECTION('ref_axis',(-0.00745029082566168,0.,0.99997224619817));
#31340=DIRECTION('',(0.,-1.,0.));
#31341=DIRECTION('',(-0.00745029082566168,0.,0.99997224619817));
#31342=DIRECTION('center_axis',(0.,-1.,0.));
#31343=DIRECTION('ref_axis',(0.939692620785908,0.,0.342020143325669));
#31344=DIRECTION('',(0.637062515999983,0.,-0.770812137104607));
#31345=DIRECTION('center_axis',(-0.770812137104607,0.,-0.637062515999983));
#31346=DIRECTION('ref_axis',(0.637062515999983,0.,-0.770812137104607));
#31347=DIRECTION('center_axis',(0.986074150277955,0.,-0.166306254102512));
#31348=DIRECTION('ref_axis',(0.166306254102512,0.,0.986074150277955));
#31349=DIRECTION('',(0.,-1.,0.));
#31350=DIRECTION('',(0.166306254102512,0.,0.986074150277955));
#31351=DIRECTION('center_axis',(0.,-1.,0.));
#31352=DIRECTION('ref_axis',(0.984807753012208,0.,0.17364817766693));
#31353=DIRECTION('',(0.49353398197848,0.,-0.869726513699833));
#31354=DIRECTION('center_axis',(-0.869726513699833,0.,-0.49353398197848));
#31355=DIRECTION('ref_axis',(0.49353398197848,0.,-0.869726513699833));
#31356=DIRECTION('center_axis',(0.942214690279141,0.,-0.335009667654806));
#31357=DIRECTION('ref_axis',(0.335009667654806,0.,0.94221469027914));
#31358=DIRECTION('',(0.,-1.,0.));
#31359=DIRECTION('',(0.335009667654806,0.,0.94221469027914));
#31360=DIRECTION('center_axis',(0.,-1.,0.));
#31361=DIRECTION('ref_axis',(1.,0.,-6.12323399573677E-17));
#31362=DIRECTION('',(0.335009667654806,0.,-0.94221469027914));
#31363=DIRECTION('center_axis',(-0.942214690279141,0.,-0.335009667654806));
#31364=DIRECTION('ref_axis',(0.335009667654806,0.,-0.94221469027914));
#31365=DIRECTION('center_axis',(0.869726513699833,0.,-0.49353398197848));
#31366=DIRECTION('ref_axis',(0.49353398197848,0.,0.869726513699833));
#31367=DIRECTION('',(0.,-1.,0.));
#31368=DIRECTION('',(0.49353398197848,0.,0.869726513699833));
#31369=DIRECTION('center_axis',(0.,-1.,0.));
#31370=DIRECTION('ref_axis',(0.984807753012208,0.,-0.17364817766693));
#31371=DIRECTION('',(0.166306254102512,0.,-0.986074150277955));
#31372=DIRECTION('center_axis',(-0.986074150277955,0.,-0.166306254102512));
#31373=DIRECTION('ref_axis',(0.166306254102512,0.,-0.986074150277955));
#31374=DIRECTION('center_axis',(0.770812137104607,0.,-0.637062515999983));
#31375=DIRECTION('ref_axis',(0.637062515999983,0.,0.770812137104607));
#31376=DIRECTION('',(0.,-1.,0.));
#31377=DIRECTION('',(0.637062515999983,0.,0.770812137104607));
#31378=DIRECTION('center_axis',(0.,-1.,0.));
#31379=DIRECTION('ref_axis',(0.939692620785908,0.,-0.342020143325669));
#31380=DIRECTION('',(-0.00745029082566184,0.,-0.99997224619817));
#31381=DIRECTION('center_axis',(-0.99997224619817,0.,0.00745029082566184));
#31382=DIRECTION('ref_axis',(-0.00745029082566184,0.,-0.99997224619817));
#31383=DIRECTION('center_axis',(0.648477023773219,0.,-0.761234227842014));
#31384=DIRECTION('ref_axis',(0.761234227842014,0.,0.648477023773219));
#31385=DIRECTION('',(0.,-1.,0.));
#31386=DIRECTION('',(0.761234227842014,0.,0.64847702377322));
#31387=DIRECTION('center_axis',(0.,-1.,0.));
#31388=DIRECTION('ref_axis',(0.866025403784439,0.,-0.5));
#31389=DIRECTION('',(-0.180980462437127,0.,-0.983486691428025));
#31390=DIRECTION('center_axis',(-0.983486691428025,0.,0.180980462437127));
#31391=DIRECTION('ref_axis',(-0.180980462437127,0.,-0.983486691428025));
#31392=DIRECTION('center_axis',(0.50643826421969,0.,-0.862276222874171));
#31393=DIRECTION('ref_axis',(0.862276222874171,0.,0.50643826421969));
#31394=DIRECTION('',(0.,-1.,0.));
#31395=DIRECTION('',(0.862276222874171,0.,0.50643826421969));
#31396=DIRECTION('center_axis',(0.,-1.,0.));
#31397=DIRECTION('ref_axis',(0.766044443118978,0.,-0.642787609686539));
#31398=DIRECTION('',(-0.349011634277972,0.,-0.937118391207119));
#31399=DIRECTION('center_axis',(-0.937118391207119,0.,0.349011634277972));
#31400=DIRECTION('ref_axis',(-0.349011634277972,0.,-0.937118391207119));
#31401=DIRECTION('center_axis',(0.349011634277972,0.,-0.937118391207119));
#31402=DIRECTION('ref_axis',(0.937118391207119,0.,0.349011634277972));
#31403=DIRECTION('',(0.,-1.,0.));
#31404=DIRECTION('',(0.937118391207119,0.,0.349011634277972));
#31405=DIRECTION('center_axis',(0.,-1.,0.));
#31406=DIRECTION('ref_axis',(0.642787609686539,0.,-0.766044443118978));
#31407=DIRECTION('',(-0.50643826421969,0.,-0.862276222874171));
#31408=DIRECTION('center_axis',(-0.862276222874171,0.,0.50643826421969));
#31409=DIRECTION('ref_axis',(-0.50643826421969,0.,-0.862276222874171));
#31410=DIRECTION('center_axis',(0.180980462437127,0.,-0.983486691428025));
#31411=DIRECTION('ref_axis',(0.983486691428025,0.,0.180980462437127));
#31412=DIRECTION('',(0.,-1.,0.));
#31413=DIRECTION('',(0.983486691428025,0.,0.180980462437127));
#31414=DIRECTION('center_axis',(0.,-1.,0.));
#31415=DIRECTION('ref_axis',(0.5,0.,-0.866025403784439));
#31416=DIRECTION('',(-0.64847702377322,0.,-0.761234227842014));
#31417=DIRECTION('center_axis',(-0.761234227842014,0.,0.64847702377322));
#31418=DIRECTION('ref_axis',(-0.64847702377322,0.,-0.761234227842014));
#31419=DIRECTION('center_axis',(0.00745029082566168,0.,-0.99997224619817));
#31420=DIRECTION('ref_axis',(0.99997224619817,0.,0.00745029082566168));
#31421=DIRECTION('',(0.,-1.,0.));
#31422=DIRECTION('',(0.99997224619817,0.,0.00745029082566168));
#31423=DIRECTION('center_axis',(0.,-1.,0.));
#31424=DIRECTION('ref_axis',(0.342020143325669,0.,-0.939692620785908));
#31425=DIRECTION('',(-0.770812137104607,0.,-0.637062515999983));
#31426=DIRECTION('center_axis',(-0.637062515999983,0.,0.770812137104607));
#31427=DIRECTION('ref_axis',(-0.770812137104607,0.,-0.637062515999983));
#31428=DIRECTION('center_axis',(-0.166306254102512,0.,-0.986074150277955));
#31429=DIRECTION('ref_axis',(0.986074150277955,0.,-0.166306254102512));
#31430=DIRECTION('',(0.,-1.,0.));
#31431=DIRECTION('',(0.986074150277955,0.,-0.166306254102512));
#31432=DIRECTION('center_axis',(0.,-1.,0.));
#31433=DIRECTION('ref_axis',(0.17364817766693,0.,-0.984807753012208));
#31434=DIRECTION('',(-0.869726513699833,0.,-0.49353398197848));
#31435=DIRECTION('center_axis',(-0.49353398197848,0.,0.869726513699833));
#31436=DIRECTION('ref_axis',(-0.869726513699833,0.,-0.49353398197848));
#31437=DIRECTION('center_axis',(-0.335009667654806,0.,-0.942214690279141));
#31438=DIRECTION('ref_axis',(0.94221469027914,0.,-0.335009667654806));
#31439=DIRECTION('',(0.,-1.,0.));
#31440=DIRECTION('',(0.94221469027914,0.,-0.335009667654806));
#31441=DIRECTION('center_axis',(0.,-1.,0.));
#31442=DIRECTION('ref_axis',(0.,0.,-1.));
#31443=DIRECTION('',(-0.94221469027914,0.,-0.335009667654806));
#31444=DIRECTION('center_axis',(-0.335009667654806,0.,0.942214690279141));
#31445=DIRECTION('ref_axis',(-0.94221469027914,0.,-0.335009667654806));
#31446=DIRECTION('center_axis',(0.,1.,0.));
#31447=DIRECTION('ref_axis',(0.,0.,1.));
#31448=DIRECTION('center_axis',(-1.,0.,1.22464679914735E-16));
#31449=DIRECTION('ref_axis',(-1.22464679914735E-16,0.,-1.));
#31450=DIRECTION('center_axis',(0.,-1.,0.));
#31451=DIRECTION('ref_axis',(1.,0.,0.));
#31452=DIRECTION('',(0.707106781186544,0.707106781186551,8.6595605623549E-17));
#31453=DIRECTION('center_axis',(0.,-1.,0.));
#31454=DIRECTION('ref_axis',(1.,0.,0.));
#31455=DIRECTION('center_axis',(0.,1.,0.));
#31456=DIRECTION('ref_axis',(1.,0.,0.));
#31457=DIRECTION('center_axis',(0.,-1.,0.));
#31458=DIRECTION('ref_axis',(1.,0.,0.));
#31459=DIRECTION('center_axis',(0.,1.,0.));
#31460=DIRECTION('ref_axis',(1.,0.,0.));
#31461=DIRECTION('center_axis',(0.,-1.,0.));
#31462=DIRECTION('ref_axis',(1.,0.,0.));
#31463=DIRECTION('center_axis',(0.,-1.,0.));
#31464=DIRECTION('ref_axis',(1.,0.,0.));
#31465=DIRECTION('center_axis',(0.,-1.,0.));
#31466=DIRECTION('ref_axis',(1.,0.,0.));
#31467=DIRECTION('center_axis',(0.,-1.,0.));
#31468=DIRECTION('ref_axis',(1.,0.,0.));
#31469=DIRECTION('center_axis',(0.,-1.,0.));
#31470=DIRECTION('ref_axis',(1.,0.,0.));
#31471=DIRECTION('center_axis',(0.,-1.,0.));
#31472=DIRECTION('ref_axis',(1.,0.,0.));
#31473=DIRECTION('',(-0.707106781186555,0.70710678118654,8.65956056235503E-17));
#31474=DIRECTION('center_axis',(0.,-1.,0.));
#31475=DIRECTION('ref_axis',(1.,0.,0.));
#31476=DIRECTION('',(0.,1.,0.));
#31477=DIRECTION('',(0.,-1.,0.));
#31478=DIRECTION('center_axis',(0.,1.,0.));
#31479=DIRECTION('ref_axis',(1.,0.,0.));
#31480=DIRECTION('center_axis',(0.,-1.,0.));
#31481=DIRECTION('ref_axis',(1.,0.,0.));
#31482=DIRECTION('',(0.,1.,0.));
#31483=DIRECTION('',(0.,-1.,0.));
#31484=DIRECTION('center_axis',(0.,1.,0.));
#31485=DIRECTION('ref_axis',(1.,0.,0.));
#31486=DIRECTION('center_axis',(0.,-1.,0.));
#31487=DIRECTION('ref_axis',(1.,0.,0.));
#31488=DIRECTION('',(0.,-1.,0.));
#31489=DIRECTION('center_axis',(0.,1.,0.));
#31490=DIRECTION('ref_axis',(1.,0.,0.));
#31491=DIRECTION('',(0.,1.,0.));
#31492=DIRECTION('center_axis',(0.,-1.,0.));
#31493=DIRECTION('ref_axis',(1.,0.,0.));
#31494=DIRECTION('',(0.,1.,0.));
#31495=DIRECTION('',(0.,-1.,0.));
#31496=DIRECTION('center_axis',(0.,1.,0.));
#31497=DIRECTION('ref_axis',(1.,0.,0.));
#31498=DIRECTION('center_axis',(0.,-1.,0.));
#31499=DIRECTION('ref_axis',(1.,0.,0.));
#31500=DIRECTION('',(0.,-1.,0.));
#31501=DIRECTION('center_axis',(0.,1.,0.));
#31502=DIRECTION('ref_axis',(1.,0.,0.));
#31503=DIRECTION('',(0.,1.,0.));
#31504=DIRECTION('center_axis',(0.,-1.,0.));
#31505=DIRECTION('ref_axis',(1.,0.,0.));
#31506=DIRECTION('',(0.,-1.,0.));
#31507=DIRECTION('center_axis',(0.,1.,0.));
#31508=DIRECTION('ref_axis',(1.,0.,0.));
#31509=DIRECTION('',(0.,1.,0.));
#31510=DIRECTION('center_axis',(0.866025403784439,0.,0.5));
#31511=DIRECTION('ref_axis',(-0.5,0.,0.866025403784439));
#31512=DIRECTION('',(-0.5,0.,0.866025403784439));
#31513=DIRECTION('',(0.,-1.,0.));
#31514=DIRECTION('',(-0.5,0.,0.866025403784439));
#31515=DIRECTION('',(0.,-1.,0.));
#31516=DIRECTION('center_axis',(0.866025403784439,0.,-0.5));
#31517=DIRECTION('ref_axis',(0.5,0.,0.866025403784439));
#31518=DIRECTION('',(0.5,0.,0.866025403784439));
#31519=DIRECTION('',(0.,-1.,0.));
#31520=DIRECTION('',(0.5,0.,0.866025403784439));
#31521=DIRECTION('center_axis',(-1.92296268638356E-16,0.,-1.));
#31522=DIRECTION('ref_axis',(1.,0.,-1.92296268638356E-16));
#31523=DIRECTION('',(1.,0.,-1.92296268638356E-16));
#31524=DIRECTION('',(0.,-1.,0.));
#31525=DIRECTION('',(1.,0.,-1.92296268638356E-16));
#31526=DIRECTION('center_axis',(0.,1.,0.));
#31527=DIRECTION('ref_axis',(1.,0.,0.));
#31528=DIRECTION('center_axis',(0.,1.,0.));
#31529=DIRECTION('ref_axis',(1.,0.,0.));
#31530=DIRECTION('center_axis',(0.,1.,0.));
#31531=DIRECTION('ref_axis',(1.,0.,0.));
#31532=DIRECTION('',(0.5,0.,-0.866025403784439));
#31533=DIRECTION('center_axis',(0.,1.,0.));
#31534=DIRECTION('ref_axis',(1.,0.,0.));
#31535=DIRECTION('center_axis',(0.,1.,0.));
#31536=DIRECTION('ref_axis',(1.,0.,0.));
#31537=DIRECTION('',(-0.5,0.,-0.866025403784438));
#31538=DIRECTION('center_axis',(0.,1.,0.));
#31539=DIRECTION('ref_axis',(1.,0.,0.));
#31540=DIRECTION('',(-1.,0.,1.92296268638356E-16));
#31541=DIRECTION('center_axis',(0.,1.,0.));
#31542=DIRECTION('ref_axis',(0.,0.,1.));
#31543=DIRECTION('',(0.5,0.,-0.866025403784439));
#31544=DIRECTION('center_axis',(0.,-1.,0.));
#31545=DIRECTION('ref_axis',(1.,0.,0.));
#31546=DIRECTION('center_axis',(0.,1.,0.));
#31547=DIRECTION('ref_axis',(0.,0.,1.));
#31548=DIRECTION('center_axis',(0.,-1.,0.));
#31549=DIRECTION('ref_axis',(1.,0.,0.));
#31550=DIRECTION('center_axis',(0.,1.,0.));
#31551=DIRECTION('ref_axis',(0.,0.,1.));
#31552=DIRECTION('center_axis',(0.,-1.,0.));
#31553=DIRECTION('ref_axis',(1.,0.,0.));
#31554=DIRECTION('center_axis',(0.,1.,0.));
#31555=DIRECTION('ref_axis',(0.,0.,1.));
#31556=DIRECTION('center_axis',(0.,-1.,0.));
#31557=DIRECTION('ref_axis',(1.,0.,0.));
#31558=DIRECTION('center_axis',(0.,1.,0.));
#31559=DIRECTION('ref_axis',(0.,0.,1.));
#31560=DIRECTION('',(-1.,0.,1.92296268638356E-16));
#31561=DIRECTION('center_axis',(0.,-1.,0.));
#31562=DIRECTION('ref_axis',(1.,0.,0.));
#31563=DIRECTION('center_axis',(0.,1.,0.));
#31564=DIRECTION('ref_axis',(0.,0.,1.));
#31565=DIRECTION('',(-0.5,0.,-0.866025403784438));
#31566=DIRECTION('center_axis',(0.,-1.,0.));
#31567=DIRECTION('ref_axis',(1.,0.,0.));
#31568=DIRECTION('center_axis',(0.,1.,0.));
#31569=DIRECTION('ref_axis',(1.,0.,0.));
#31570=DIRECTION('',(-0.85716730070211,0.515038074910058,1.04972719113862E-16));
#31571=DIRECTION('center_axis',(-0.866025403784439,0.,-0.5));
#31572=DIRECTION('ref_axis',(0.5,0.,-0.866025403784439));
#31573=DIRECTION('',(0.,-1.,0.));
#31574=DIRECTION('center_axis',(-0.866025403784438,0.,0.5));
#31575=DIRECTION('ref_axis',(-0.5,0.,-0.866025403784438));
#31576=DIRECTION('',(0.,-1.,0.));
#31577=DIRECTION('center_axis',(1.92296268638356E-16,0.,1.));
#31578=DIRECTION('ref_axis',(-1.,0.,1.92296268638356E-16));
#31579=DIRECTION('axis',(0.,0.,1.));
#31580=DIRECTION('refdir',(1.,0.,0.));
#31581=DIRECTION('center_axis',(0.,1.,0.));
#31582=DIRECTION('ref_axis',(1.,0.,0.));
#31583=DIRECTION('center_axis',(0.,-1.,0.));
#31584=DIRECTION('ref_axis',(1.,0.,0.));
#31585=DIRECTION('',(-0.707106781186547,0.707106781186548,8.65956056235493E-17));
#31586=DIRECTION('center_axis',(0.,1.,0.));
#31587=DIRECTION('ref_axis',(1.,0.,0.));
#31588=DIRECTION('center_axis',(0.,1.,0.));
#31589=DIRECTION('ref_axis',(1.,0.,0.));
#31590=DIRECTION('',(-1.,0.,0.));
#31591=DIRECTION('center_axis',(0.,-1.,0.));
#31592=DIRECTION('ref_axis',(0.,0.,1.));
#31593=DIRECTION('',(1.,0.,0.));
#31594=DIRECTION('center_axis',(0.,-1.,0.));
#31595=DIRECTION('ref_axis',(0.,0.,-1.));
#31596=DIRECTION('center_axis',(0.,1.,0.));
#31597=DIRECTION('ref_axis',(1.,0.,0.));
#31598=DIRECTION('center_axis',(0.,1.,0.));
#31599=DIRECTION('ref_axis',(1.,0.,0.));
#31600=DIRECTION('center_axis',(0.,1.,0.));
#31601=DIRECTION('ref_axis',(1.,0.,0.));
#31602=DIRECTION('center_axis',(0.,1.,0.));
#31603=DIRECTION('ref_axis',(1.,0.,0.));
#31604=DIRECTION('center_axis',(0.,1.,0.));
#31605=DIRECTION('ref_axis',(1.,0.,0.));
#31606=DIRECTION('center_axis',(0.,1.,0.));
#31607=DIRECTION('ref_axis',(1.,0.,0.));
#31608=DIRECTION('center_axis',(0.,1.,0.));
#31609=DIRECTION('ref_axis',(1.,0.,0.));
#31610=DIRECTION('center_axis',(0.,1.,0.));
#31611=DIRECTION('ref_axis',(1.,0.,0.));
#31612=DIRECTION('center_axis',(0.,1.,0.));
#31613=DIRECTION('ref_axis',(1.,0.,0.));
#31614=DIRECTION('center_axis',(0.,1.,0.));
#31615=DIRECTION('ref_axis',(1.,0.,0.));
#31616=DIRECTION('center_axis',(0.,1.,0.));
#31617=DIRECTION('ref_axis',(1.,0.,0.));
#31618=DIRECTION('center_axis',(0.,1.,0.));
#31619=DIRECTION('ref_axis',(1.,0.,0.));
#31620=DIRECTION('center_axis',(0.,1.,0.));
#31621=DIRECTION('ref_axis',(1.,0.,0.));
#31622=DIRECTION('center_axis',(0.,1.,0.));
#31623=DIRECTION('ref_axis',(1.,0.,0.));
#31624=DIRECTION('center_axis',(0.,1.,0.));
#31625=DIRECTION('ref_axis',(1.,0.,0.));
#31626=DIRECTION('center_axis',(0.,1.,0.));
#31627=DIRECTION('ref_axis',(1.,0.,0.));
#31628=DIRECTION('center_axis',(0.,1.,0.));
#31629=DIRECTION('ref_axis',(1.,0.,0.));
#31630=DIRECTION('center_axis',(0.,1.,0.));
#31631=DIRECTION('ref_axis',(1.,0.,0.));
#31632=DIRECTION('center_axis',(0.,1.,0.));
#31633=DIRECTION('ref_axis',(1.,0.,0.));
#31634=DIRECTION('center_axis',(0.,1.,0.));
#31635=DIRECTION('ref_axis',(1.,0.,0.));
#31636=DIRECTION('center_axis',(0.,-1.,0.));
#31637=DIRECTION('ref_axis',(1.,0.,0.));
#31638=DIRECTION('',(0.,-1.,0.));
#31639=DIRECTION('center_axis',(0.,1.,0.));
#31640=DIRECTION('ref_axis',(1.,0.,0.));
#31641=DIRECTION('center_axis',(0.,1.,0.));
#31642=DIRECTION('ref_axis',(1.,0.,0.));
#31643=DIRECTION('center_axis',(0.,-1.,0.));
#31644=DIRECTION('ref_axis',(1.,0.,0.));
#31645=DIRECTION('',(-0.707106781186547,0.707106781186548,8.65956056235493E-17));
#31646=DIRECTION('center_axis',(0.,-1.,0.));
#31647=DIRECTION('ref_axis',(1.,0.,0.));
#31648=DIRECTION('',(0.,-1.,0.));
#31649=DIRECTION('center_axis',(0.,1.,0.));
#31650=DIRECTION('ref_axis',(1.,0.,0.));
#31651=DIRECTION('center_axis',(0.,1.,0.));
#31652=DIRECTION('ref_axis',(1.,0.,0.));
#31653=DIRECTION('center_axis',(0.,-1.,0.));
#31654=DIRECTION('ref_axis',(1.,0.,0.));
#31655=DIRECTION('',(-0.707106781186547,0.707106781186548,8.65956056235493E-17));
#31656=DIRECTION('center_axis',(0.,-1.,0.));
#31657=DIRECTION('ref_axis',(1.,0.,0.));
#31658=DIRECTION('',(0.,-1.,0.));
#31659=DIRECTION('center_axis',(0.,1.,0.));
#31660=DIRECTION('ref_axis',(1.,0.,0.));
#31661=DIRECTION('center_axis',(0.,1.,0.));
#31662=DIRECTION('ref_axis',(1.,0.,0.));
#31663=DIRECTION('center_axis',(0.,-1.,0.));
#31664=DIRECTION('ref_axis',(1.,0.,0.));
#31665=DIRECTION('',(-0.707106781186547,0.707106781186548,8.65956056235493E-17));
#31666=DIRECTION('center_axis',(0.,-1.,0.));
#31667=DIRECTION('ref_axis',(1.,0.,0.));
#31668=DIRECTION('',(0.,-1.,0.));
#31669=DIRECTION('center_axis',(0.,1.,0.));
#31670=DIRECTION('ref_axis',(1.,0.,0.));
#31671=DIRECTION('center_axis',(0.,1.,0.));
#31672=DIRECTION('ref_axis',(1.,0.,0.));
#31673=DIRECTION('center_axis',(0.,-1.,0.));
#31674=DIRECTION('ref_axis',(1.,0.,0.));
#31675=DIRECTION('',(-0.707106781186555,0.70710678118654,8.65956056235503E-17));
#31676=DIRECTION('center_axis',(0.,-1.,0.));
#31677=DIRECTION('ref_axis',(1.,0.,0.));
#31678=DIRECTION('',(0.,-1.,0.));
#31679=DIRECTION('center_axis',(0.,1.,0.));
#31680=DIRECTION('ref_axis',(1.,0.,0.));
#31681=DIRECTION('center_axis',(0.,1.,0.));
#31682=DIRECTION('ref_axis',(1.,0.,0.));
#31683=DIRECTION('center_axis',(0.,-1.,0.));
#31684=DIRECTION('ref_axis',(1.,0.,0.));
#31685=DIRECTION('',(-0.707106781186547,0.707106781186548,8.65956056235493E-17));
#31686=DIRECTION('center_axis',(0.,-1.,0.));
#31687=DIRECTION('ref_axis',(1.,0.,0.));
#31688=DIRECTION('',(0.,-1.,0.));
#31689=DIRECTION('center_axis',(0.,1.,0.));
#31690=DIRECTION('ref_axis',(1.,0.,0.));
#31691=DIRECTION('center_axis',(0.,1.,0.));
#31692=DIRECTION('ref_axis',(1.,0.,0.));
#31693=DIRECTION('center_axis',(0.,-1.,0.));
#31694=DIRECTION('ref_axis',(1.,0.,0.));
#31695=DIRECTION('',(-0.707106781186555,0.70710678118654,8.65956056235503E-17));
#31696=DIRECTION('center_axis',(0.,-1.,0.));
#31697=DIRECTION('ref_axis',(1.,0.,0.));
#31698=DIRECTION('',(0.,-1.,0.));
#31699=DIRECTION('center_axis',(0.,1.,0.));
#31700=DIRECTION('ref_axis',(1.,0.,0.));
#31701=DIRECTION('center_axis',(0.,1.,0.));
#31702=DIRECTION('ref_axis',(1.,0.,0.));
#31703=DIRECTION('center_axis',(0.,-1.,0.));
#31704=DIRECTION('ref_axis',(1.,0.,0.));
#31705=DIRECTION('',(-0.707106781186555,0.70710678118654,8.65956056235503E-17));
#31706=DIRECTION('center_axis',(0.,-1.,0.));
#31707=DIRECTION('ref_axis',(1.,0.,0.));
#31708=DIRECTION('',(0.,-1.,0.));
#31709=DIRECTION('center_axis',(0.,1.,0.));
#31710=DIRECTION('ref_axis',(1.,0.,0.));
#31711=DIRECTION('center_axis',(0.,1.,0.));
#31712=DIRECTION('ref_axis',(1.,0.,0.));
#31713=DIRECTION('center_axis',(0.,-1.,0.));
#31714=DIRECTION('ref_axis',(1.,0.,0.));
#31715=DIRECTION('',(-0.707106781186547,0.707106781186548,8.65956056235493E-17));
#31716=DIRECTION('center_axis',(0.,-1.,0.));
#31717=DIRECTION('ref_axis',(1.,0.,0.));
#31718=DIRECTION('',(0.,-1.,0.));
#31719=DIRECTION('center_axis',(0.,1.,0.));
#31720=DIRECTION('ref_axis',(1.,0.,0.));
#31721=DIRECTION('center_axis',(0.,1.,0.));
#31722=DIRECTION('ref_axis',(1.,0.,0.));
#31723=DIRECTION('center_axis',(0.,-1.,0.));
#31724=DIRECTION('ref_axis',(1.,0.,0.));
#31725=DIRECTION('',(-0.707106781186547,0.707106781186548,8.65956056235493E-17));
#31726=DIRECTION('center_axis',(0.,-1.,0.));
#31727=DIRECTION('ref_axis',(1.,0.,0.));
#31728=DIRECTION('',(0.,-1.,0.));
#31729=DIRECTION('center_axis',(0.,1.,0.));
#31730=DIRECTION('ref_axis',(1.,0.,0.));
#31731=DIRECTION('center_axis',(0.,1.,0.));
#31732=DIRECTION('ref_axis',(1.,0.,0.));
#31733=DIRECTION('center_axis',(0.,-1.,0.));
#31734=DIRECTION('ref_axis',(1.,0.,0.));
#31735=DIRECTION('',(-0.707106781186547,0.707106781186548,8.65956056235493E-17));
#31736=DIRECTION('center_axis',(0.,-1.,0.));
#31737=DIRECTION('ref_axis',(1.,0.,0.));
#31738=DIRECTION('',(0.,-1.,0.));
#31739=DIRECTION('center_axis',(0.,1.,0.));
#31740=DIRECTION('ref_axis',(1.,0.,0.));
#31741=DIRECTION('center_axis',(0.,1.,0.));
#31742=DIRECTION('ref_axis',(1.,0.,0.));
#31743=DIRECTION('center_axis',(0.,-1.,0.));
#31744=DIRECTION('ref_axis',(1.,0.,0.));
#31745=DIRECTION('',(-0.707106781186547,0.707106781186548,8.65956056235493E-17));
#31746=DIRECTION('center_axis',(0.,-1.,0.));
#31747=DIRECTION('ref_axis',(1.,0.,0.));
#31748=DIRECTION('',(0.,-1.,0.));
#31749=DIRECTION('center_axis',(0.,1.,0.));
#31750=DIRECTION('ref_axis',(1.,0.,0.));
#31751=DIRECTION('center_axis',(0.,1.,0.));
#31752=DIRECTION('ref_axis',(1.,0.,0.));
#31753=DIRECTION('center_axis',(0.,-1.,0.));
#31754=DIRECTION('ref_axis',(1.,0.,0.));
#31755=DIRECTION('',(-0.707106781186547,0.707106781186548,8.65956056235493E-17));
#31756=DIRECTION('center_axis',(0.,-1.,0.));
#31757=DIRECTION('ref_axis',(1.,0.,0.));
#31758=DIRECTION('',(0.,-1.,0.));
#31759=DIRECTION('center_axis',(0.,1.,0.));
#31760=DIRECTION('ref_axis',(1.,0.,0.));
#31761=DIRECTION('center_axis',(0.,1.,0.));
#31762=DIRECTION('ref_axis',(1.,0.,0.));
#31763=DIRECTION('center_axis',(0.,-1.,0.));
#31764=DIRECTION('ref_axis',(1.,0.,0.));
#31765=DIRECTION('',(-0.707106781186555,0.70710678118654,8.65956056235503E-17));
#31766=DIRECTION('center_axis',(0.,-1.,0.));
#31767=DIRECTION('ref_axis',(1.,0.,0.));
#31768=DIRECTION('',(0.,-1.,0.));
#31769=DIRECTION('center_axis',(0.,1.,0.));
#31770=DIRECTION('ref_axis',(1.,0.,0.));
#31771=DIRECTION('center_axis',(0.,1.,0.));
#31772=DIRECTION('ref_axis',(1.,0.,0.));
#31773=DIRECTION('center_axis',(0.,-1.,0.));
#31774=DIRECTION('ref_axis',(1.,0.,0.));
#31775=DIRECTION('',(-0.707106781186555,0.70710678118654,8.65956056235503E-17));
#31776=DIRECTION('center_axis',(0.,-1.,0.));
#31777=DIRECTION('ref_axis',(1.,0.,0.));
#31778=DIRECTION('',(0.,-1.,0.));
#31779=DIRECTION('center_axis',(0.,1.,0.));
#31780=DIRECTION('ref_axis',(1.,0.,0.));
#31781=DIRECTION('center_axis',(0.,1.,0.));
#31782=DIRECTION('ref_axis',(1.,0.,0.));
#31783=DIRECTION('center_axis',(0.,-1.,0.));
#31784=DIRECTION('ref_axis',(1.,0.,0.));
#31785=DIRECTION('',(-0.707106781186555,0.70710678118654,8.65956056235503E-17));
#31786=DIRECTION('center_axis',(0.,-1.,0.));
#31787=DIRECTION('ref_axis',(1.,0.,0.));
#31788=DIRECTION('',(0.,-1.,0.));
#31789=DIRECTION('center_axis',(0.,1.,0.));
#31790=DIRECTION('ref_axis',(1.,0.,0.));
#31791=DIRECTION('center_axis',(0.,1.,0.));
#31792=DIRECTION('ref_axis',(1.,0.,0.));
#31793=DIRECTION('center_axis',(0.,-1.,0.));
#31794=DIRECTION('ref_axis',(1.,0.,0.));
#31795=DIRECTION('',(-0.707106781186555,0.70710678118654,8.65956056235503E-17));
#31796=DIRECTION('center_axis',(0.,-1.,0.));
#31797=DIRECTION('ref_axis',(1.,0.,0.));
#31798=DIRECTION('',(0.,-1.,0.));
#31799=DIRECTION('center_axis',(0.,1.,0.));
#31800=DIRECTION('ref_axis',(1.,0.,0.));
#31801=DIRECTION('center_axis',(0.,1.,0.));
#31802=DIRECTION('ref_axis',(1.,0.,0.));
#31803=DIRECTION('center_axis',(0.,-1.,0.));
#31804=DIRECTION('ref_axis',(1.,0.,0.));
#31805=DIRECTION('',(-0.707106781186555,0.70710678118654,8.65956056235503E-17));
#31806=DIRECTION('center_axis',(0.,-1.,0.));
#31807=DIRECTION('ref_axis',(1.,0.,0.));
#31808=DIRECTION('',(0.,-1.,0.));
#31809=DIRECTION('center_axis',(0.,1.,0.));
#31810=DIRECTION('ref_axis',(1.,0.,0.));
#31811=DIRECTION('center_axis',(0.,1.,0.));
#31812=DIRECTION('ref_axis',(1.,0.,0.));
#31813=DIRECTION('center_axis',(0.,-1.,0.));
#31814=DIRECTION('ref_axis',(1.,0.,0.));
#31815=DIRECTION('',(-0.707106781186547,0.707106781186548,8.65956056235493E-17));
#31816=DIRECTION('center_axis',(0.,-1.,0.));
#31817=DIRECTION('ref_axis',(1.,0.,0.));
#31818=DIRECTION('',(0.,-1.,0.));
#31819=DIRECTION('center_axis',(0.,1.,0.));
#31820=DIRECTION('ref_axis',(1.,0.,0.));
#31821=DIRECTION('center_axis',(0.,1.,0.));
#31822=DIRECTION('ref_axis',(1.,0.,0.));
#31823=DIRECTION('center_axis',(0.,-1.,0.));
#31824=DIRECTION('ref_axis',(1.,0.,0.));
#31825=DIRECTION('',(-0.707106781186547,0.707106781186548,8.65956056235493E-17));
#31826=DIRECTION('center_axis',(0.,-1.,0.));
#31827=DIRECTION('ref_axis',(1.,0.,0.));
#31828=DIRECTION('',(0.,-1.,0.));
#31829=DIRECTION('center_axis',(0.,1.,0.));
#31830=DIRECTION('ref_axis',(1.,0.,0.));
#31831=DIRECTION('center_axis',(0.,1.,0.));
#31832=DIRECTION('ref_axis',(1.,0.,0.));
#31833=DIRECTION('center_axis',(0.,-1.,0.));
#31834=DIRECTION('ref_axis',(1.,0.,0.));
#31835=DIRECTION('',(-0.707106781186547,0.707106781186548,8.65956056235493E-17));
#31836=DIRECTION('center_axis',(0.,-1.,0.));
#31837=DIRECTION('ref_axis',(1.,0.,0.));
#31838=DIRECTION('',(0.,-1.,0.));
#31839=DIRECTION('center_axis',(0.,1.,0.));
#31840=DIRECTION('ref_axis',(1.,0.,0.));
#31841=DIRECTION('center_axis',(0.,0.707106781186541,0.707106781186554));
#31842=DIRECTION('ref_axis',(1.,0.,0.));
#31843=DIRECTION('',(0.,0.707106781186554,-0.707106781186541));
#31844=DIRECTION('',(0.,-0.707106781186554,0.707106781186541));
#31845=DIRECTION('',(1.,0.,0.));
#31846=DIRECTION('center_axis',(0.,-1.,0.));
#31847=DIRECTION('ref_axis',(0.,0.,1.));
#31848=DIRECTION('',(0.,0.707106781186547,0.707106781186547));
#31849=DIRECTION('center_axis',(0.,1.,0.));
#31850=DIRECTION('ref_axis',(0.,0.,1.));
#31851=DIRECTION('center_axis',(0.,0.707106781186543,-0.707106781186552));
#31852=DIRECTION('ref_axis',(-1.,0.,0.));
#31853=DIRECTION('',(0.,0.707106781186552,0.707106781186543));
#31854=DIRECTION('',(-1.,0.,0.));
#31855=DIRECTION('center_axis',(0.,-1.,0.));
#31856=DIRECTION('ref_axis',(0.,0.,-1.));
#31857=DIRECTION('center_axis',(0.,1.,0.));
#31858=DIRECTION('ref_axis',(0.,0.,-1.));
#31859=DIRECTION('center_axis',(0.,1.,0.));
#31860=DIRECTION('ref_axis',(0.,0.,1.));
#31861=DIRECTION('',(0.,1.,0.));
#31862=DIRECTION('center_axis',(0.,-1.,0.));
#31863=DIRECTION('ref_axis',(0.,0.,1.));
#31864=DIRECTION('',(0.,1.,0.));
#31865=DIRECTION('center_axis',(0.,0.,1.));
#31866=DIRECTION('ref_axis',(1.,0.,0.));
#31867=DIRECTION('',(0.,1.,0.));
#31868=DIRECTION('',(-1.,0.,0.));
#31869=DIRECTION('center_axis',(0.,-0.707106781186541,0.707106781186554));
#31870=DIRECTION('ref_axis',(1.,0.,0.));
#31871=DIRECTION('',(0.,-0.707106781186554,-0.707106781186541));
#31872=DIRECTION('',(1.,0.,0.));
#31873=DIRECTION('',(0.,0.707106781186554,0.707106781186541));
#31874=DIRECTION('center_axis',(0.,1.,0.));
#31875=DIRECTION('ref_axis',(0.,0.,-1.));
#31876=DIRECTION('center_axis',(0.,-1.,0.));
#31877=DIRECTION('ref_axis',(0.,0.,-1.));
#31878=DIRECTION('',(0.,-0.707106781186547,0.707106781186547));
#31879=DIRECTION('center_axis',(0.,1.,0.));
#31880=DIRECTION('ref_axis',(0.,0.,-1.));
#31881=DIRECTION('center_axis',(0.,-0.707106781186543,-0.707106781186552));
#31882=DIRECTION('ref_axis',(-1.,0.,0.));
#31883=DIRECTION('',(0.,-0.707106781186554,0.707106781186541));
#31884=DIRECTION('',(-1.,0.,0.));
#31885=DIRECTION('',(1.,0.,0.));
#31886=DIRECTION('center_axis',(0.,1.,0.));
#31887=DIRECTION('ref_axis',(0.,0.,1.));
#31888=DIRECTION('center_axis',(0.,1.,0.));
#31889=DIRECTION('ref_axis',(0.,0.,1.));
#31890=DIRECTION('center_axis',(0.,1.,0.));
#31891=DIRECTION('ref_axis',(0.,0.,-1.));
#31892=DIRECTION('',(0.,1.,0.));
#31893=DIRECTION('center_axis',(0.,1.,0.));
#31894=DIRECTION('ref_axis',(1.,0.,0.));
#31895=DIRECTION('center_axis',(0.,0.,-1.));
#31896=DIRECTION('ref_axis',(-1.,0.,0.));
#31897=DIRECTION('axis',(0.,0.,1.));
#31898=DIRECTION('refdir',(1.,0.,0.));
#31899=DIRECTION('center_axis',(0.,0.70710678118654,-0.707106781186555));
#31900=DIRECTION('ref_axis',(-1.,0.,0.));
#31901=DIRECTION('',(-0.24924356936395,0.684791078771744,0.684791078771729));
#31902=DIRECTION('',(-1.,0.,0.));
#31903=DIRECTION('',(0.,0.707106781186557,0.707106781186538));
#31904=DIRECTION('',(1.,0.,0.));
#31905=DIRECTION('center_axis',(0.,-1.,0.));
#31906=DIRECTION('ref_axis',(0.,0.,-1.));
#31907=DIRECTION('',(0.,0.707106781186547,-0.707106781186547));
#31908=DIRECTION('center_axis',(0.,-1.,0.));
#31909=DIRECTION('ref_axis',(0.,0.,-1.));
#31910=DIRECTION('center_axis',(0.,1.,0.));
#31911=DIRECTION('ref_axis',(0.,0.,-1.));
#31912=DIRECTION('center_axis',(0.,0.70710678118654,0.707106781186555));
#31913=DIRECTION('ref_axis',(1.,0.,0.));
#31914=DIRECTION('',(6.28036983473502E-14,0.707106781186555,-0.70710678118654));
#31915=DIRECTION('',(-1.,0.,0.));
#31916=DIRECTION('',(1.,0.,0.));
#31917=DIRECTION('center_axis',(0.,-1.,0.));
#31918=DIRECTION('ref_axis',(0.,0.,1.));
#31919=DIRECTION('',(0.,0.707106781186547,0.707106781186547));
#31920=DIRECTION('center_axis',(0.,-1.,0.));
#31921=DIRECTION('ref_axis',(0.,0.,1.));
#31922=DIRECTION('center_axis',(0.,1.,0.));
#31923=DIRECTION('ref_axis',(0.,0.,1.));
#31924=DIRECTION('center_axis',(0.,0.70710678118654,-0.707106781186555));
#31925=DIRECTION('ref_axis',(-1.,0.,0.));
#31926=DIRECTION('',(-0.24924356936395,-0.684791078771744,-0.684791078771729));
#31927=DIRECTION('',(1.,0.,0.));
#31928=DIRECTION('',(-1.,0.,0.));
#31929=DIRECTION('center_axis',(0.,0.,-1.));
#31930=DIRECTION('ref_axis',(-1.,0.,0.));
#31931=DIRECTION('',(0.,1.,0.));
#31932=DIRECTION('',(1.,0.,0.));
#31933=DIRECTION('',(0.,1.,0.));
#31934=DIRECTION('center_axis',(0.,1.,0.));
#31935=DIRECTION('ref_axis',(0.,0.,1.));
#31936=DIRECTION('',(0.,1.,0.));
#31937=DIRECTION('center_axis',(0.,-1.,0.));
#31938=DIRECTION('ref_axis',(0.,0.,1.));
#31939=DIRECTION('center_axis',(0.,0.,1.));
#31940=DIRECTION('ref_axis',(1.,0.,0.));
#31941=DIRECTION('',(0.,1.,0.));
#31942=DIRECTION('',(-1.,0.,0.));
#31943=DIRECTION('center_axis',(0.,1.,0.));
#31944=DIRECTION('ref_axis',(0.,0.,-1.));
#31945=DIRECTION('',(0.,1.,0.));
#31946=DIRECTION('center_axis',(0.,-1.,0.));
#31947=DIRECTION('ref_axis',(0.,0.,-1.));
#31948=DIRECTION('center_axis',(0.,0.,-1.));
#31949=DIRECTION('ref_axis',(-1.,0.,0.));
#31950=DIRECTION('',(0.,1.,0.));
#31951=DIRECTION('',(1.,0.,0.));
#31952=DIRECTION('center_axis',(0.,-0.707106781186555,-0.70710678118654));
#31953=DIRECTION('ref_axis',(-1.,0.,0.));
#31954=DIRECTION('',(0.249243569363955,-0.684791078771728,0.684791078771743));
#31955=DIRECTION('',(0.,-0.707106781186544,0.707106781186551));
#31956=DIRECTION('',(-1.,0.,0.));
#31957=DIRECTION('center_axis',(0.,1.,0.));
#31958=DIRECTION('ref_axis',(0.,0.,1.));
#31959=DIRECTION('',(0.,-0.707106781186548,-0.707106781186548));
#31960=DIRECTION('center_axis',(0.,1.,0.));
#31961=DIRECTION('ref_axis',(0.,0.,1.));
#31962=DIRECTION('center_axis',(0.,-0.707106781186555,0.70710678118654));
#31963=DIRECTION('ref_axis',(1.,0.,0.));
#31964=DIRECTION('',(0.,-0.70710678118654,-0.707106781186555));
#31965=DIRECTION('',(1.,0.,0.));
#31966=DIRECTION('center_axis',(0.,1.,0.));
#31967=DIRECTION('ref_axis',(0.,0.,-1.));
#31968=DIRECTION('',(0.,-0.707106781186548,0.707106781186548));
#31969=DIRECTION('center_axis',(0.,1.,0.));
#31970=DIRECTION('ref_axis',(0.,0.,-1.));
#31971=DIRECTION('center_axis',(0.,-0.707106781186555,-0.70710678118654));
#31972=DIRECTION('ref_axis',(-1.,0.,0.));
#31973=DIRECTION('',(0.249243569363955,0.684791078771728,-0.684791078771743));
#31974=DIRECTION('',(-1.,0.,0.));
#31975=DIRECTION('center_axis',(0.,-1.,0.));
#31976=DIRECTION('ref_axis',(1.,0.,0.));
#31977=DIRECTION('center_axis',(0.,-1.,0.));
#31978=DIRECTION('ref_axis',(1.,0.,0.));
#31979=DIRECTION('',(0.,-1.,0.));
#31980=DIRECTION('center_axis',(0.,1.,0.));
#31981=DIRECTION('ref_axis',(1.,0.,0.));
#31982=DIRECTION('center_axis',(0.,-1.,0.));
#31983=DIRECTION('ref_axis',(1.,0.,0.));
#31984=DIRECTION('center_axis',(0.,-1.,0.));
#31985=DIRECTION('ref_axis',(1.,0.,0.));
#31986=DIRECTION('',(0.,-1.,0.));
#31987=DIRECTION('center_axis',(0.,1.,0.));
#31988=DIRECTION('ref_axis',(1.,0.,0.));
#31989=DIRECTION('center_axis',(0.,-1.,0.));
#31990=DIRECTION('ref_axis',(1.,0.,0.));
#31991=DIRECTION('center_axis',(0.,-1.,0.));
#31992=DIRECTION('ref_axis',(1.,0.,0.));
#31993=DIRECTION('',(0.,-1.,0.));
#31994=DIRECTION('center_axis',(0.,1.,0.));
#31995=DIRECTION('ref_axis',(1.,0.,0.));
#31996=DIRECTION('center_axis',(0.,-1.,0.));
#31997=DIRECTION('ref_axis',(1.,0.,0.));
#31998=DIRECTION('center_axis',(0.,-1.,0.));
#31999=DIRECTION('ref_axis',(1.,0.,0.));
#32000=DIRECTION('',(0.,-1.,0.));
#32001=DIRECTION('center_axis',(0.,1.,0.));
#32002=DIRECTION('ref_axis',(1.,0.,0.));
#32003=DIRECTION('center_axis',(0.,-1.,0.));
#32004=DIRECTION('ref_axis',(1.,0.,0.));
#32005=DIRECTION('center_axis',(0.,-1.,0.));
#32006=DIRECTION('ref_axis',(1.,0.,0.));
#32007=DIRECTION('',(0.,-1.,0.));
#32008=DIRECTION('center_axis',(0.,1.,0.));
#32009=DIRECTION('ref_axis',(1.,0.,0.));
#32010=DIRECTION('center_axis',(0.,-1.,0.));
#32011=DIRECTION('ref_axis',(1.,0.,0.));
#32012=DIRECTION('center_axis',(0.,-1.,0.));
#32013=DIRECTION('ref_axis',(1.,0.,0.));
#32014=DIRECTION('',(0.,-1.,0.));
#32015=DIRECTION('center_axis',(0.,1.,0.));
#32016=DIRECTION('ref_axis',(1.,0.,0.));
#32017=DIRECTION('center_axis',(0.,-1.,0.));
#32018=DIRECTION('ref_axis',(1.,0.,0.));
#32019=DIRECTION('center_axis',(0.,-1.,0.));
#32020=DIRECTION('ref_axis',(1.,0.,0.));
#32021=DIRECTION('',(0.,-1.,0.));
#32022=DIRECTION('center_axis',(0.,1.,0.));
#32023=DIRECTION('ref_axis',(1.,0.,0.));
#32024=DIRECTION('center_axis',(0.,-1.,0.));
#32025=DIRECTION('ref_axis',(1.,0.,0.));
#32026=DIRECTION('center_axis',(0.,-1.,0.));
#32027=DIRECTION('ref_axis',(1.,0.,0.));
#32028=DIRECTION('',(0.,-1.,0.));
#32029=DIRECTION('center_axis',(0.,1.,0.));
#32030=DIRECTION('ref_axis',(1.,0.,0.));
#32031=DIRECTION('center_axis',(0.,-1.,0.));
#32032=DIRECTION('ref_axis',(1.,0.,0.));
#32033=DIRECTION('center_axis',(0.,-1.,0.));
#32034=DIRECTION('ref_axis',(1.,0.,0.));
#32035=DIRECTION('',(0.,-1.,0.));
#32036=DIRECTION('center_axis',(0.,1.,0.));
#32037=DIRECTION('ref_axis',(1.,0.,0.));
#32038=DIRECTION('center_axis',(0.,-1.,0.));
#32039=DIRECTION('ref_axis',(1.,0.,0.));
#32040=DIRECTION('center_axis',(0.,-1.,0.));
#32041=DIRECTION('ref_axis',(1.,0.,0.));
#32042=DIRECTION('',(0.,-1.,0.));
#32043=DIRECTION('center_axis',(0.,1.,0.));
#32044=DIRECTION('ref_axis',(1.,0.,0.));
#32045=DIRECTION('center_axis',(-0.939692620785909,0.,-0.342020143325667));
#32046=DIRECTION('ref_axis',(-0.342020143325667,0.,0.939692620785909));
#32047=DIRECTION('',(0.342020143325667,0.,-0.939692620785909));
#32048=DIRECTION('',(-0.342020143325667,0.,0.939692620785909));
#32049=DIRECTION('',(0.,1.,0.));
#32050=DIRECTION('center_axis',(0.,0.,-1.));
#32051=DIRECTION('ref_axis',(-1.,0.,0.));
#32052=DIRECTION('',(1.,0.,0.));
#32053=DIRECTION('',(-1.,0.,0.));
#32054=DIRECTION('',(0.,1.,0.));
#32055=DIRECTION('center_axis',(0.939692620785909,0.,-0.342020143325667));
#32056=DIRECTION('ref_axis',(-0.342020143325667,0.,-0.939692620785909));
#32057=DIRECTION('',(0.342020143325667,0.,0.939692620785909));
#32058=DIRECTION('',(-0.342020143325667,0.,-0.939692620785909));
#32059=DIRECTION('',(0.,1.,0.));
#32060=DIRECTION('center_axis',(0.,0.,-1.));
#32061=DIRECTION('ref_axis',(-1.,0.,0.));
#32062=DIRECTION('',(1.,0.,0.));
#32063=DIRECTION('',(-1.,0.,0.));
#32064=DIRECTION('',(0.,1.,0.));
#32065=DIRECTION('center_axis',(-0.939692620785909,0.,-0.342020143325667));
#32066=DIRECTION('ref_axis',(-0.342020143325667,0.,0.939692620785909));
#32067=DIRECTION('',(0.342020143325667,0.,-0.939692620785909));
#32068=DIRECTION('',(-0.342020143325667,0.,0.939692620785909));
#32069=DIRECTION('',(0.,1.,0.));
#32070=DIRECTION('center_axis',(0.,0.,-1.));
#32071=DIRECTION('ref_axis',(-1.,0.,0.));
#32072=DIRECTION('',(1.,0.,0.));
#32073=DIRECTION('',(-1.,0.,0.));
#32074=DIRECTION('',(0.,1.,0.));
#32075=DIRECTION('center_axis',(0.939692620785909,0.,-0.342020143325667));
#32076=DIRECTION('ref_axis',(-0.342020143325667,0.,-0.939692620785909));
#32077=DIRECTION('',(0.342020143325667,0.,0.939692620785909));
#32078=DIRECTION('',(-0.342020143325667,0.,-0.939692620785909));
#32079=DIRECTION('',(0.,1.,0.));
#32080=DIRECTION('center_axis',(0.,0.,-1.));
#32081=DIRECTION('ref_axis',(-1.,0.,0.));
#32082=DIRECTION('',(1.,0.,0.));
#32083=DIRECTION('',(-1.,0.,0.));
#32084=DIRECTION('',(0.,1.,0.));
#32085=DIRECTION('center_axis',(-0.939692620785909,0.,-0.342020143325667));
#32086=DIRECTION('ref_axis',(-0.342020143325667,0.,0.939692620785909));
#32087=DIRECTION('',(0.342020143325667,0.,-0.939692620785909));
#32088=DIRECTION('',(-0.342020143325667,0.,0.939692620785909));
#32089=DIRECTION('',(0.,1.,0.));
#32090=DIRECTION('center_axis',(0.,0.,-1.));
#32091=DIRECTION('ref_axis',(-1.,0.,0.));
#32092=DIRECTION('',(1.,0.,0.));
#32093=DIRECTION('',(-1.,0.,0.));
#32094=DIRECTION('',(0.,1.,0.));
#32095=DIRECTION('center_axis',(0.939692620785909,0.,-0.342020143325667));
#32096=DIRECTION('ref_axis',(-0.342020143325667,0.,-0.939692620785909));
#32097=DIRECTION('',(0.342020143325667,0.,0.939692620785909));
#32098=DIRECTION('',(-0.342020143325667,0.,-0.939692620785909));
#32099=DIRECTION('',(0.,1.,0.));
#32100=DIRECTION('center_axis',(0.,0.,-1.));
#32101=DIRECTION('ref_axis',(-1.,0.,0.));
#32102=DIRECTION('',(1.,0.,0.));
#32103=DIRECTION('',(-1.,0.,0.));
#32104=DIRECTION('',(0.,1.,0.));
#32105=DIRECTION('center_axis',(-0.939692620785909,0.,-0.342020143325667));
#32106=DIRECTION('ref_axis',(-0.342020143325667,0.,0.939692620785909));
#32107=DIRECTION('',(0.342020143325667,0.,-0.939692620785909));
#32108=DIRECTION('',(-0.342020143325667,0.,0.939692620785909));
#32109=DIRECTION('',(0.,1.,0.));
#32110=DIRECTION('center_axis',(0.,0.,-1.));
#32111=DIRECTION('ref_axis',(-1.,0.,0.));
#32112=DIRECTION('',(1.,0.,0.));
#32113=DIRECTION('',(-1.,0.,0.));
#32114=DIRECTION('',(0.,1.,0.));
#32115=DIRECTION('center_axis',(0.939692620785909,0.,-0.342020143325667));
#32116=DIRECTION('ref_axis',(-0.342020143325667,0.,-0.939692620785909));
#32117=DIRECTION('',(0.342020143325667,0.,0.939692620785909));
#32118=DIRECTION('',(-0.342020143325667,0.,-0.939692620785909));
#32119=DIRECTION('',(0.,1.,0.));
#32120=DIRECTION('center_axis',(0.,0.,-1.));
#32121=DIRECTION('ref_axis',(-1.,0.,0.));
#32122=DIRECTION('',(1.,0.,0.));
#32123=DIRECTION('',(-1.,0.,0.));
#32124=DIRECTION('',(0.,1.,0.));
#32125=DIRECTION('center_axis',(-0.939692620785909,0.,-0.342020143325667));
#32126=DIRECTION('ref_axis',(-0.342020143325667,0.,0.939692620785909));
#32127=DIRECTION('',(0.342020143325667,0.,-0.939692620785909));
#32128=DIRECTION('',(-0.342020143325667,0.,0.939692620785909));
#32129=DIRECTION('',(0.,1.,0.));
#32130=DIRECTION('center_axis',(0.,0.,-1.));
#32131=DIRECTION('ref_axis',(-1.,0.,0.));
#32132=DIRECTION('',(1.,0.,0.));
#32133=DIRECTION('',(-1.,0.,0.));
#32134=DIRECTION('',(0.,1.,0.));
#32135=DIRECTION('center_axis',(0.939692620785909,0.,-0.342020143325667));
#32136=DIRECTION('ref_axis',(-0.342020143325667,0.,-0.939692620785909));
#32137=DIRECTION('',(0.342020143325667,0.,0.939692620785909));
#32138=DIRECTION('',(-0.342020143325667,0.,-0.939692620785909));
#32139=DIRECTION('',(0.,1.,0.));
#32140=DIRECTION('center_axis',(0.,0.,-1.));
#32141=DIRECTION('ref_axis',(-1.,0.,0.));
#32142=DIRECTION('',(1.,0.,0.));
#32143=DIRECTION('',(-1.,0.,0.));
#32144=DIRECTION('',(0.,1.,0.));
#32145=DIRECTION('center_axis',(-0.939692620785911,0.,-0.342020143325663));
#32146=DIRECTION('ref_axis',(-0.342020143325663,0.,0.939692620785911));
#32147=DIRECTION('',(0.342020143325663,0.,-0.939692620785911));
#32148=DIRECTION('',(-0.342020143325663,0.,0.939692620785911));
#32149=DIRECTION('',(0.,1.,0.));
#32150=DIRECTION('center_axis',(0.,0.,-1.));
#32151=DIRECTION('ref_axis',(-1.,0.,0.));
#32152=DIRECTION('',(1.,0.,0.));
#32153=DIRECTION('',(-1.,0.,0.));
#32154=DIRECTION('',(0.,1.,0.));
#32155=DIRECTION('center_axis',(0.939692620785911,0.,-0.342020143325663));
#32156=DIRECTION('ref_axis',(-0.342020143325663,0.,-0.939692620785911));
#32157=DIRECTION('',(0.342020143325663,0.,0.939692620785911));
#32158=DIRECTION('',(-0.342020143325663,0.,-0.939692620785911));
#32159=DIRECTION('',(0.,1.,0.));
#32160=DIRECTION('center_axis',(0.,0.,-1.));
#32161=DIRECTION('ref_axis',(-1.,0.,0.));
#32162=DIRECTION('',(1.,0.,0.));
#32163=DIRECTION('',(-1.,0.,0.));
#32164=DIRECTION('',(0.,1.,0.));
#32165=DIRECTION('center_axis',(-0.939692620785911,0.,-0.342020143325663));
#32166=DIRECTION('ref_axis',(-0.342020143325663,0.,0.939692620785911));
#32167=DIRECTION('',(0.342020143325663,0.,-0.939692620785911));
#32168=DIRECTION('',(-0.342020143325663,0.,0.939692620785911));
#32169=DIRECTION('',(0.,1.,0.));
#32170=DIRECTION('center_axis',(0.,0.,-1.));
#32171=DIRECTION('ref_axis',(-1.,0.,0.));
#32172=DIRECTION('',(1.,0.,0.));
#32173=DIRECTION('',(-1.,0.,0.));
#32174=DIRECTION('',(0.,1.,0.));
#32175=DIRECTION('center_axis',(0.939692620785911,0.,-0.342020143325663));
#32176=DIRECTION('ref_axis',(-0.342020143325663,0.,-0.939692620785911));
#32177=DIRECTION('',(0.342020143325663,0.,0.939692620785911));
#32178=DIRECTION('',(-0.342020143325663,0.,-0.939692620785911));
#32179=DIRECTION('',(0.,1.,0.));
#32180=DIRECTION('center_axis',(0.,0.,-1.));
#32181=DIRECTION('ref_axis',(-1.,0.,0.));
#32182=DIRECTION('',(1.,0.,0.));
#32183=DIRECTION('',(-1.,0.,0.));
#32184=DIRECTION('',(0.,1.,0.));
#32185=DIRECTION('center_axis',(-0.939692620785909,0.,-0.342020143325667));
#32186=DIRECTION('ref_axis',(-0.342020143325667,0.,0.939692620785909));
#32187=DIRECTION('',(0.342020143325667,0.,-0.939692620785909));
#32188=DIRECTION('',(-0.342020143325667,0.,0.939692620785909));
#32189=DIRECTION('',(0.,1.,0.));
#32190=DIRECTION('center_axis',(0.,0.,-1.));
#32191=DIRECTION('ref_axis',(-1.,0.,0.));
#32192=DIRECTION('',(1.,0.,0.));
#32193=DIRECTION('',(-1.,0.,0.));
#32194=DIRECTION('',(0.,1.,0.));
#32195=DIRECTION('center_axis',(0.939692620785909,0.,-0.342020143325667));
#32196=DIRECTION('ref_axis',(-0.342020143325667,0.,-0.939692620785909));
#32197=DIRECTION('',(0.342020143325667,0.,0.939692620785909));
#32198=DIRECTION('',(-0.342020143325667,0.,-0.939692620785909));
#32199=DIRECTION('',(0.,1.,0.));
#32200=DIRECTION('center_axis',(0.,0.,-1.));
#32201=DIRECTION('ref_axis',(-1.,0.,0.));
#32202=DIRECTION('',(1.,0.,0.));
#32203=DIRECTION('',(-1.,0.,0.));
#32204=DIRECTION('',(0.,1.,0.));
#32205=DIRECTION('center_axis',(-0.939692620785909,0.,-0.342020143325667));
#32206=DIRECTION('ref_axis',(-0.342020143325667,0.,0.939692620785909));
#32207=DIRECTION('',(0.342020143325667,0.,-0.939692620785909));
#32208=DIRECTION('',(-0.342020143325667,0.,0.939692620785909));
#32209=DIRECTION('',(0.,1.,0.));
#32210=DIRECTION('center_axis',(0.,0.,-1.));
#32211=DIRECTION('ref_axis',(-1.,0.,0.));
#32212=DIRECTION('',(1.,0.,0.));
#32213=DIRECTION('',(-1.,0.,0.));
#32214=DIRECTION('',(0.,1.,0.));
#32215=DIRECTION('center_axis',(0.939692620785909,0.,-0.342020143325667));
#32216=DIRECTION('ref_axis',(-0.342020143325667,0.,-0.939692620785909));
#32217=DIRECTION('',(0.342020143325667,0.,0.939692620785909));
#32218=DIRECTION('',(-0.342020143325667,0.,-0.939692620785909));
#32219=DIRECTION('',(0.,1.,0.));
#32220=DIRECTION('center_axis',(0.,0.,-1.));
#32221=DIRECTION('ref_axis',(-1.,0.,0.));
#32222=DIRECTION('',(1.,0.,0.));
#32223=DIRECTION('',(-1.,0.,0.));
#32224=DIRECTION('',(0.,1.,0.));
#32225=DIRECTION('center_axis',(-0.939692620785908,0.,-0.342020143325671));
#32226=DIRECTION('ref_axis',(-0.342020143325671,0.,0.939692620785908));
#32227=DIRECTION('',(0.342020143325671,0.,-0.939692620785907));
#32228=DIRECTION('',(-0.342020143325671,0.,0.939692620785907));
#32229=DIRECTION('',(0.,1.,0.));
#32230=DIRECTION('center_axis',(0.,0.,-1.));
#32231=DIRECTION('ref_axis',(-1.,0.,0.));
#32232=DIRECTION('',(1.,0.,0.));
#32233=DIRECTION('',(-1.,0.,0.));
#32234=DIRECTION('',(0.,1.,0.));
#32235=DIRECTION('center_axis',(0.939692620785908,0.,-0.342020143325671));
#32236=DIRECTION('ref_axis',(-0.342020143325671,0.,-0.939692620785908));
#32237=DIRECTION('',(0.342020143325671,0.,0.939692620785907));
#32238=DIRECTION('',(-0.342020143325671,0.,-0.939692620785907));
#32239=DIRECTION('',(0.,1.,0.));
#32240=DIRECTION('center_axis',(0.,0.,-1.));
#32241=DIRECTION('ref_axis',(-1.,0.,0.));
#32242=DIRECTION('',(1.,0.,0.));
#32243=DIRECTION('',(-1.,0.,0.));
#32244=DIRECTION('',(0.,1.,0.));
#32245=DIRECTION('center_axis',(-0.939692620785908,0.,-0.342020143325671));
#32246=DIRECTION('ref_axis',(-0.342020143325671,0.,0.939692620785908));
#32247=DIRECTION('',(0.342020143325671,0.,-0.939692620785907));
#32248=DIRECTION('',(-0.342020143325671,0.,0.939692620785907));
#32249=DIRECTION('',(0.,1.,0.));
#32250=DIRECTION('center_axis',(0.,0.,-1.));
#32251=DIRECTION('ref_axis',(-1.,0.,0.));
#32252=DIRECTION('',(1.,0.,0.));
#32253=DIRECTION('',(-1.,0.,0.));
#32254=DIRECTION('',(0.,1.,0.));
#32255=DIRECTION('center_axis',(0.939692620785909,0.,-0.342020143325667));
#32256=DIRECTION('ref_axis',(-0.342020143325667,0.,-0.939692620785909));
#32257=DIRECTION('',(0.342020143325667,0.,0.939692620785909));
#32258=DIRECTION('',(-0.342020143325667,0.,-0.939692620785909));
#32259=DIRECTION('',(0.,1.,0.));
#32260=DIRECTION('center_axis',(0.,0.,-1.));
#32261=DIRECTION('ref_axis',(-1.,0.,0.));
#32262=DIRECTION('',(1.,0.,0.));
#32263=DIRECTION('',(-1.,0.,0.));
#32264=DIRECTION('',(0.,1.,0.));
#32265=DIRECTION('center_axis',(-0.939692620785909,0.,-0.342020143325667));
#32266=DIRECTION('ref_axis',(-0.342020143325667,0.,0.939692620785909));
#32267=DIRECTION('',(0.342020143325667,0.,-0.939692620785909));
#32268=DIRECTION('',(-0.342020143325667,0.,0.939692620785909));
#32269=DIRECTION('',(0.,1.,0.));
#32270=DIRECTION('center_axis',(0.,0.,-1.));
#32271=DIRECTION('ref_axis',(-1.,0.,0.));
#32272=DIRECTION('',(1.,0.,0.));
#32273=DIRECTION('',(-1.,0.,0.));
#32274=DIRECTION('',(0.,1.,0.));
#32275=DIRECTION('center_axis',(0.939692620785909,0.,-0.342020143325667));
#32276=DIRECTION('ref_axis',(-0.342020143325667,0.,-0.939692620785909));
#32277=DIRECTION('',(0.342020143325667,0.,0.939692620785909));
#32278=DIRECTION('',(-0.342020143325667,0.,-0.939692620785909));
#32279=DIRECTION('',(0.,1.,0.));
#32280=DIRECTION('center_axis',(0.,0.,-1.));
#32281=DIRECTION('ref_axis',(-1.,0.,0.));
#32282=DIRECTION('',(1.,0.,0.));
#32283=DIRECTION('',(-1.,0.,0.));
#32284=DIRECTION('',(0.,1.,0.));
#32285=DIRECTION('center_axis',(-0.939692620785909,0.,-0.342020143325667));
#32286=DIRECTION('ref_axis',(-0.342020143325667,0.,0.939692620785909));
#32287=DIRECTION('',(0.342020143325667,0.,-0.939692620785909));
#32288=DIRECTION('',(-0.342020143325667,0.,0.939692620785909));
#32289=DIRECTION('',(0.,1.,0.));
#32290=DIRECTION('center_axis',(0.,0.,-1.));
#32291=DIRECTION('ref_axis',(-1.,0.,0.));
#32292=DIRECTION('',(1.,0.,0.));
#32293=DIRECTION('',(-1.,0.,0.));
#32294=DIRECTION('',(0.,1.,0.));
#32295=DIRECTION('center_axis',(0.939692620785909,0.,-0.342020143325667));
#32296=DIRECTION('ref_axis',(-0.342020143325667,0.,-0.939692620785909));
#32297=DIRECTION('',(0.342020143325667,0.,0.939692620785909));
#32298=DIRECTION('',(-0.342020143325667,0.,-0.939692620785909));
#32299=DIRECTION('',(0.,1.,0.));
#32300=DIRECTION('center_axis',(0.,0.,-1.));
#32301=DIRECTION('ref_axis',(-1.,0.,0.));
#32302=DIRECTION('',(1.,0.,0.));
#32303=DIRECTION('',(-1.,0.,0.));
#32304=DIRECTION('',(0.,1.,0.));
#32305=DIRECTION('center_axis',(-0.939692620785909,0.,-0.342020143325667));
#32306=DIRECTION('ref_axis',(-0.342020143325667,0.,0.939692620785909));
#32307=DIRECTION('',(0.342020143325667,0.,-0.939692620785909));
#32308=DIRECTION('',(-0.342020143325667,0.,0.939692620785909));
#32309=DIRECTION('',(0.,1.,0.));
#32310=DIRECTION('center_axis',(0.,0.,-1.));
#32311=DIRECTION('ref_axis',(-1.,0.,0.));
#32312=DIRECTION('',(1.,0.,0.));
#32313=DIRECTION('',(-1.,0.,0.));
#32314=DIRECTION('',(0.,1.,0.));
#32315=DIRECTION('center_axis',(0.939692620785908,0.,-0.342020143325671));
#32316=DIRECTION('ref_axis',(-0.342020143325671,0.,-0.939692620785908));
#32317=DIRECTION('',(0.342020143325671,0.,0.939692620785907));
#32318=DIRECTION('',(-0.342020143325671,0.,-0.939692620785907));
#32319=DIRECTION('',(0.,1.,0.));
#32320=DIRECTION('center_axis',(0.,0.,-1.));
#32321=DIRECTION('ref_axis',(-1.,0.,0.));
#32322=DIRECTION('',(1.,0.,0.));
#32323=DIRECTION('',(-1.,0.,0.));
#32324=DIRECTION('',(0.,1.,0.));
#32325=DIRECTION('center_axis',(-0.939692620785908,0.,-0.342020143325671));
#32326=DIRECTION('ref_axis',(-0.342020143325671,0.,0.939692620785908));
#32327=DIRECTION('',(0.342020143325671,0.,-0.939692620785907));
#32328=DIRECTION('',(-0.342020143325671,0.,0.939692620785907));
#32329=DIRECTION('',(0.,1.,0.));
#32330=DIRECTION('center_axis',(0.,0.,-1.));
#32331=DIRECTION('ref_axis',(-1.,0.,0.));
#32332=DIRECTION('',(1.,0.,0.));
#32333=DIRECTION('',(-1.,0.,0.));
#32334=DIRECTION('',(0.,1.,0.));
#32335=DIRECTION('center_axis',(0.939692620785908,0.,-0.342020143325671));
#32336=DIRECTION('ref_axis',(-0.342020143325671,0.,-0.939692620785908));
#32337=DIRECTION('',(0.342020143325671,0.,0.939692620785907));
#32338=DIRECTION('',(-0.342020143325671,0.,-0.939692620785907));
#32339=DIRECTION('',(0.,1.,0.));
#32340=DIRECTION('center_axis',(0.,0.,-1.));
#32341=DIRECTION('ref_axis',(-1.,0.,0.));
#32342=DIRECTION('',(1.,0.,0.));
#32343=DIRECTION('',(-1.,0.,0.));
#32344=DIRECTION('',(0.,1.,0.));
#32345=DIRECTION('center_axis',(-0.939692620785908,0.,-0.342020143325671));
#32346=DIRECTION('ref_axis',(-0.342020143325671,0.,0.939692620785908));
#32347=DIRECTION('',(0.342020143325671,0.,-0.939692620785907));
#32348=DIRECTION('',(-0.342020143325671,0.,0.939692620785907));
#32349=DIRECTION('',(0.,1.,0.));
#32350=DIRECTION('center_axis',(0.,0.,-1.));
#32351=DIRECTION('ref_axis',(-1.,0.,0.));
#32352=DIRECTION('',(1.,0.,0.));
#32353=DIRECTION('',(-1.,0.,0.));
#32354=DIRECTION('',(0.,1.,0.));
#32355=DIRECTION('center_axis',(0.939692620785908,0.,-0.342020143325671));
#32356=DIRECTION('ref_axis',(-0.342020143325671,0.,-0.939692620785908));
#32357=DIRECTION('',(0.342020143325671,0.,0.939692620785907));
#32358=DIRECTION('',(-0.342020143325671,0.,-0.939692620785907));
#32359=DIRECTION('',(0.,1.,0.));
#32360=DIRECTION('center_axis',(0.,0.,-1.));
#32361=DIRECTION('ref_axis',(-1.,0.,0.));
#32362=DIRECTION('',(1.,0.,0.));
#32363=DIRECTION('',(-1.,0.,0.));
#32364=DIRECTION('',(0.,1.,0.));
#32365=DIRECTION('center_axis',(-0.939692620785908,0.,-0.342020143325671));
#32366=DIRECTION('ref_axis',(-0.342020143325671,0.,0.939692620785908));
#32367=DIRECTION('',(0.342020143325671,0.,-0.939692620785907));
#32368=DIRECTION('',(-0.342020143325671,0.,0.939692620785907));
#32369=DIRECTION('',(0.,1.,0.));
#32370=DIRECTION('center_axis',(0.,0.,-1.));
#32371=DIRECTION('ref_axis',(-1.,0.,0.));
#32372=DIRECTION('',(1.,0.,0.));
#32373=DIRECTION('',(-1.,0.,0.));
#32374=DIRECTION('',(0.,1.,0.));
#32375=DIRECTION('center_axis',(0.939692620785909,0.,-0.342020143325667));
#32376=DIRECTION('ref_axis',(-0.342020143325667,0.,-0.939692620785909));
#32377=DIRECTION('',(0.342020143325667,0.,0.939692620785909));
#32378=DIRECTION('',(-0.342020143325667,0.,-0.939692620785909));
#32379=DIRECTION('',(0.,1.,0.));
#32380=DIRECTION('center_axis',(0.,0.,-1.));
#32381=DIRECTION('ref_axis',(-1.,0.,0.));
#32382=DIRECTION('',(1.,0.,0.));
#32383=DIRECTION('',(-1.,0.,0.));
#32384=DIRECTION('',(0.,1.,0.));
#32385=DIRECTION('center_axis',(-0.939692620785909,0.,-0.342020143325667));
#32386=DIRECTION('ref_axis',(-0.342020143325667,0.,0.939692620785909));
#32387=DIRECTION('',(0.342020143325667,0.,-0.939692620785909));
#32388=DIRECTION('',(-0.342020143325667,0.,0.939692620785909));
#32389=DIRECTION('',(0.,1.,0.));
#32390=DIRECTION('center_axis',(0.,0.,-1.));
#32391=DIRECTION('ref_axis',(-1.,0.,0.));
#32392=DIRECTION('',(1.,0.,0.));
#32393=DIRECTION('',(-1.,0.,0.));
#32394=DIRECTION('',(0.,1.,0.));
#32395=DIRECTION('center_axis',(0.939692620785909,0.,-0.342020143325667));
#32396=DIRECTION('ref_axis',(-0.342020143325667,0.,-0.939692620785909));
#32397=DIRECTION('',(0.342020143325667,0.,0.939692620785909));
#32398=DIRECTION('',(-0.342020143325667,0.,-0.939692620785909));
#32399=DIRECTION('',(0.,1.,0.));
#32400=DIRECTION('center_axis',(0.,0.,-1.));
#32401=DIRECTION('ref_axis',(-1.,0.,0.));
#32402=DIRECTION('',(1.,0.,0.));
#32403=DIRECTION('',(-1.,0.,0.));
#32404=DIRECTION('',(0.,1.,0.));
#32405=DIRECTION('center_axis',(-0.939692620785909,0.,-0.342020143325667));
#32406=DIRECTION('ref_axis',(-0.342020143325667,0.,0.939692620785909));
#32407=DIRECTION('',(0.342020143325667,0.,-0.939692620785909));
#32408=DIRECTION('',(-0.342020143325667,0.,0.939692620785909));
#32409=DIRECTION('',(0.,1.,0.));
#32410=DIRECTION('center_axis',(0.,0.,-1.));
#32411=DIRECTION('ref_axis',(-1.,0.,0.));
#32412=DIRECTION('',(1.,0.,0.));
#32413=DIRECTION('',(-1.,0.,0.));
#32414=DIRECTION('',(0.,1.,0.));
#32415=DIRECTION('center_axis',(0.939692620785909,0.,-0.342020143325667));
#32416=DIRECTION('ref_axis',(-0.342020143325667,0.,-0.939692620785909));
#32417=DIRECTION('',(0.342020143325667,0.,0.939692620785909));
#32418=DIRECTION('',(-0.342020143325667,0.,-0.939692620785909));
#32419=DIRECTION('',(0.,1.,0.));
#32420=DIRECTION('center_axis',(0.,0.,-1.));
#32421=DIRECTION('ref_axis',(-1.,0.,0.));
#32422=DIRECTION('',(1.,0.,0.));
#32423=DIRECTION('',(-1.,0.,0.));
#32424=DIRECTION('',(0.,1.,0.));
#32425=DIRECTION('center_axis',(-0.939692620785908,0.,-0.342020143325669));
#32426=DIRECTION('ref_axis',(-0.342020143325669,0.,0.939692620785908));
#32427=DIRECTION('',(0.342020143325669,0.,-0.939692620785908));
#32428=DIRECTION('',(-0.342020143325669,0.,0.939692620785908));
#32429=DIRECTION('',(0.,1.,0.));
#32430=DIRECTION('center_axis',(0.,0.,-1.));
#32431=DIRECTION('ref_axis',(-1.,0.,0.));
#32432=DIRECTION('',(1.,0.,0.));
#32433=DIRECTION('',(-1.,0.,0.));
#32434=DIRECTION('',(0.,1.,0.));
#32435=DIRECTION('center_axis',(0.939692620785908,0.,-0.342020143325669));
#32436=DIRECTION('ref_axis',(-0.342020143325669,0.,-0.939692620785908));
#32437=DIRECTION('',(0.342020143325669,0.,0.939692620785908));
#32438=DIRECTION('',(-0.342020143325669,0.,-0.939692620785908));
#32439=DIRECTION('',(0.,1.,0.));
#32440=DIRECTION('center_axis',(0.,0.,-1.));
#32441=DIRECTION('ref_axis',(-1.,0.,0.));
#32442=DIRECTION('',(1.,0.,0.));
#32443=DIRECTION('',(-1.,0.,0.));
#32444=DIRECTION('',(0.,1.,0.));
#32445=DIRECTION('center_axis',(-0.939692620785908,0.,-0.342020143325669));
#32446=DIRECTION('ref_axis',(-0.342020143325669,0.,0.939692620785908));
#32447=DIRECTION('',(0.342020143325669,0.,-0.939692620785908));
#32448=DIRECTION('',(-0.342020143325669,0.,0.939692620785908));
#32449=DIRECTION('',(0.,1.,0.));
#32450=DIRECTION('center_axis',(0.,0.,-1.));
#32451=DIRECTION('ref_axis',(-1.,0.,0.));
#32452=DIRECTION('',(1.,0.,0.));
#32453=DIRECTION('',(-1.,0.,0.));
#32454=DIRECTION('',(0.,1.,0.));
#32455=DIRECTION('center_axis',(0.939692620785908,0.,-0.342020143325669));
#32456=DIRECTION('ref_axis',(-0.342020143325669,0.,-0.939692620785908));
#32457=DIRECTION('',(0.342020143325669,0.,0.939692620785908));
#32458=DIRECTION('',(-0.342020143325669,0.,-0.939692620785908));
#32459=DIRECTION('',(0.,1.,0.));
#32460=DIRECTION('center_axis',(0.,0.,-1.));
#32461=DIRECTION('ref_axis',(-1.,0.,0.));
#32462=DIRECTION('',(1.,0.,0.));
#32463=DIRECTION('',(-1.,0.,0.));
#32464=DIRECTION('',(0.,1.,0.));
#32465=DIRECTION('center_axis',(-0.939692620785908,0.,-0.342020143325669));
#32466=DIRECTION('ref_axis',(-0.342020143325669,0.,0.939692620785908));
#32467=DIRECTION('',(0.342020143325669,0.,-0.939692620785908));
#32468=DIRECTION('',(-0.342020143325669,0.,0.939692620785908));
#32469=DIRECTION('',(0.,1.,0.));
#32470=DIRECTION('center_axis',(0.,0.,-1.));
#32471=DIRECTION('ref_axis',(-1.,0.,0.));
#32472=DIRECTION('',(1.,0.,0.));
#32473=DIRECTION('',(-1.,0.,0.));
#32474=DIRECTION('',(0.,1.,0.));
#32475=DIRECTION('center_axis',(0.939692620785908,0.,-0.342020143325669));
#32476=DIRECTION('ref_axis',(-0.342020143325669,0.,-0.939692620785908));
#32477=DIRECTION('',(0.342020143325669,0.,0.939692620785908));
#32478=DIRECTION('',(-0.342020143325669,0.,-0.939692620785908));
#32479=DIRECTION('',(0.,1.,0.));
#32480=DIRECTION('center_axis',(0.,0.,-1.));
#32481=DIRECTION('ref_axis',(-1.,0.,0.));
#32482=DIRECTION('',(1.,0.,0.));
#32483=DIRECTION('',(-1.,0.,0.));
#32484=DIRECTION('',(0.,1.,0.));
#32485=DIRECTION('center_axis',(-0.939692620785909,0.,-0.342020143325667));
#32486=DIRECTION('ref_axis',(-0.342020143325667,0.,0.939692620785909));
#32487=DIRECTION('',(0.342020143325667,0.,-0.939692620785909));
#32488=DIRECTION('',(-0.342020143325667,0.,0.939692620785909));
#32489=DIRECTION('',(0.,1.,0.));
#32490=DIRECTION('center_axis',(0.,0.,-1.));
#32491=DIRECTION('ref_axis',(-1.,0.,0.));
#32492=DIRECTION('',(1.,0.,0.));
#32493=DIRECTION('',(-1.,0.,0.));
#32494=DIRECTION('',(0.,1.,0.));
#32495=DIRECTION('center_axis',(0.939692620785908,0.,-0.342020143325669));
#32496=DIRECTION('ref_axis',(-0.342020143325669,0.,-0.939692620785908));
#32497=DIRECTION('',(0.342020143325669,0.,0.939692620785908));
#32498=DIRECTION('',(-0.342020143325669,0.,-0.939692620785908));
#32499=DIRECTION('',(0.,1.,0.));
#32500=DIRECTION('center_axis',(0.,0.,-1.));
#32501=DIRECTION('ref_axis',(-1.,0.,0.));
#32502=DIRECTION('',(1.,0.,0.));
#32503=DIRECTION('',(-1.,0.,0.));
#32504=DIRECTION('',(0.,1.,0.));
#32505=DIRECTION('center_axis',(-0.939692620785908,0.,-0.342020143325669));
#32506=DIRECTION('ref_axis',(-0.342020143325669,0.,0.939692620785908));
#32507=DIRECTION('',(0.342020143325669,0.,-0.939692620785908));
#32508=DIRECTION('',(-0.342020143325669,0.,0.939692620785908));
#32509=DIRECTION('',(0.,1.,0.));
#32510=DIRECTION('center_axis',(0.,0.,-1.));
#32511=DIRECTION('ref_axis',(-1.,0.,0.));
#32512=DIRECTION('',(1.,0.,0.));
#32513=DIRECTION('',(-1.,0.,0.));
#32514=DIRECTION('',(0.,1.,0.));
#32515=DIRECTION('center_axis',(0.939692620785908,0.,-0.342020143325669));
#32516=DIRECTION('ref_axis',(-0.342020143325669,0.,-0.939692620785908));
#32517=DIRECTION('',(0.342020143325669,0.,0.939692620785908));
#32518=DIRECTION('',(-0.342020143325669,0.,-0.939692620785908));
#32519=DIRECTION('',(0.,1.,0.));
#32520=DIRECTION('center_axis',(0.,0.,-1.));
#32521=DIRECTION('ref_axis',(-1.,0.,0.));
#32522=DIRECTION('',(1.,0.,0.));
#32523=DIRECTION('',(-1.,0.,0.));
#32524=DIRECTION('',(0.,1.,0.));
#32525=DIRECTION('center_axis',(-0.939692620785908,0.,-0.342020143325669));
#32526=DIRECTION('ref_axis',(-0.342020143325669,0.,0.939692620785908));
#32527=DIRECTION('',(0.342020143325669,0.,-0.939692620785908));
#32528=DIRECTION('',(-0.342020143325669,0.,0.939692620785908));
#32529=DIRECTION('',(0.,1.,0.));
#32530=DIRECTION('center_axis',(0.,0.,-1.));
#32531=DIRECTION('ref_axis',(-1.,0.,0.));
#32532=DIRECTION('',(1.,0.,0.));
#32533=DIRECTION('',(-1.,0.,0.));
#32534=DIRECTION('',(0.,1.,0.));
#32535=DIRECTION('center_axis',(0.939692620785908,0.,-0.342020143325669));
#32536=DIRECTION('ref_axis',(-0.342020143325669,0.,-0.939692620785908));
#32537=DIRECTION('',(0.342020143325669,0.,0.939692620785908));
#32538=DIRECTION('',(-0.342020143325669,0.,-0.939692620785908));
#32539=DIRECTION('',(0.,1.,0.));
#32540=DIRECTION('center_axis',(0.,0.,-1.));
#32541=DIRECTION('ref_axis',(-1.,0.,0.));
#32542=DIRECTION('',(1.,0.,0.));
#32543=DIRECTION('',(-1.,0.,0.));
#32544=DIRECTION('',(0.,1.,0.));
#32545=DIRECTION('center_axis',(-0.939692620785908,0.,-0.342020143325669));
#32546=DIRECTION('ref_axis',(-0.342020143325669,0.,0.939692620785908));
#32547=DIRECTION('',(0.342020143325669,0.,-0.939692620785908));
#32548=DIRECTION('',(-0.342020143325669,0.,0.939692620785908));
#32549=DIRECTION('',(0.,1.,0.));
#32550=DIRECTION('center_axis',(0.,0.,-1.));
#32551=DIRECTION('ref_axis',(-1.,0.,0.));
#32552=DIRECTION('',(1.,0.,0.));
#32553=DIRECTION('',(-1.,0.,0.));
#32554=DIRECTION('',(0.,1.,0.));
#32555=DIRECTION('center_axis',(0.939692620785908,0.,-0.342020143325669));
#32556=DIRECTION('ref_axis',(-0.342020143325669,0.,-0.939692620785908));
#32557=DIRECTION('',(0.342020143325669,0.,0.939692620785908));
#32558=DIRECTION('',(-0.342020143325669,0.,-0.939692620785908));
#32559=DIRECTION('',(0.,1.,0.));
#32560=DIRECTION('center_axis',(0.,0.,-1.));
#32561=DIRECTION('ref_axis',(-1.,0.,0.));
#32562=DIRECTION('',(1.,0.,0.));
#32563=DIRECTION('',(-1.,0.,0.));
#32564=DIRECTION('',(0.,1.,0.));
#32565=DIRECTION('center_axis',(-0.939692620785908,0.,-0.342020143325669));
#32566=DIRECTION('ref_axis',(-0.342020143325669,0.,0.939692620785908));
#32567=DIRECTION('',(0.342020143325669,0.,-0.939692620785908));
#32568=DIRECTION('',(-0.342020143325669,0.,0.939692620785908));
#32569=DIRECTION('',(0.,1.,0.));
#32570=DIRECTION('center_axis',(0.,0.,-1.));
#32571=DIRECTION('ref_axis',(-1.,0.,0.));
#32572=DIRECTION('',(1.,0.,0.));
#32573=DIRECTION('',(-1.,0.,0.));
#32574=DIRECTION('',(0.,1.,0.));
#32575=DIRECTION('center_axis',(0.939692620785908,0.,-0.342020143325669));
#32576=DIRECTION('ref_axis',(-0.342020143325669,0.,-0.939692620785908));
#32577=DIRECTION('',(0.342020143325669,0.,0.939692620785908));
#32578=DIRECTION('',(-0.342020143325669,0.,-0.939692620785908));
#32579=DIRECTION('',(0.,1.,0.));
#32580=DIRECTION('center_axis',(0.,0.,-1.));
#32581=DIRECTION('ref_axis',(-1.,0.,0.));
#32582=DIRECTION('',(1.,0.,0.));
#32583=DIRECTION('',(-1.,0.,0.));
#32584=DIRECTION('',(0.,1.,0.));
#32585=DIRECTION('center_axis',(-0.939692620785909,0.,-0.342020143325668));
#32586=DIRECTION('ref_axis',(-0.342020143325668,0.,0.939692620785909));
#32587=DIRECTION('',(0.342020143325668,0.,-0.939692620785909));
#32588=DIRECTION('',(-0.342020143325668,0.,0.939692620785909));
#32589=DIRECTION('',(0.,1.,0.));
#32590=DIRECTION('center_axis',(0.,0.,-1.));
#32591=DIRECTION('ref_axis',(-1.,0.,0.));
#32592=DIRECTION('',(1.,0.,0.));
#32593=DIRECTION('',(-1.,0.,0.));
#32594=DIRECTION('',(0.,1.,0.));
#32595=DIRECTION('center_axis',(0.939692620785908,0.,-0.342020143325669));
#32596=DIRECTION('ref_axis',(-0.342020143325669,0.,-0.939692620785908));
#32597=DIRECTION('',(0.342020143325669,0.,0.939692620785908));
#32598=DIRECTION('',(-0.342020143325669,0.,-0.939692620785908));
#32599=DIRECTION('',(0.,1.,0.));
#32600=DIRECTION('center_axis',(0.,0.,-1.));
#32601=DIRECTION('ref_axis',(-1.,0.,0.));
#32602=DIRECTION('',(1.,0.,0.));
#32603=DIRECTION('',(-1.,0.,0.));
#32604=DIRECTION('',(0.,1.,0.));
#32605=DIRECTION('center_axis',(-0.939692620785908,0.,-0.342020143325669));
#32606=DIRECTION('ref_axis',(-0.342020143325669,0.,0.939692620785908));
#32607=DIRECTION('',(0.342020143325669,0.,-0.939692620785908));
#32608=DIRECTION('',(-0.342020143325669,0.,0.939692620785908));
#32609=DIRECTION('',(0.,1.,0.));
#32610=DIRECTION('center_axis',(0.,0.,-1.));
#32611=DIRECTION('ref_axis',(-1.,0.,0.));
#32612=DIRECTION('',(1.,0.,0.));
#32613=DIRECTION('',(-1.,0.,0.));
#32614=DIRECTION('',(0.,1.,0.));
#32615=DIRECTION('center_axis',(0.939692620785908,0.,-0.34202014332567));
#32616=DIRECTION('ref_axis',(-0.34202014332567,0.,-0.939692620785908));
#32617=DIRECTION('',(0.34202014332567,0.,0.939692620785908));
#32618=DIRECTION('',(-0.34202014332567,0.,-0.939692620785908));
#32619=DIRECTION('',(0.,1.,0.));
#32620=DIRECTION('center_axis',(0.,0.,-1.));
#32621=DIRECTION('ref_axis',(-1.,0.,0.));
#32622=DIRECTION('',(1.,0.,0.));
#32623=DIRECTION('',(-1.,0.,0.));
#32624=DIRECTION('',(0.,1.,0.));
#32625=DIRECTION('center_axis',(-0.939692620785908,0.,-0.34202014332567));
#32626=DIRECTION('ref_axis',(-0.34202014332567,0.,0.939692620785908));
#32627=DIRECTION('',(0.34202014332567,0.,-0.939692620785908));
#32628=DIRECTION('',(-0.34202014332567,0.,0.939692620785908));
#32629=DIRECTION('',(0.,1.,0.));
#32630=DIRECTION('center_axis',(0.,0.,-1.));
#32631=DIRECTION('ref_axis',(-1.,0.,0.));
#32632=DIRECTION('',(1.,0.,0.));
#32633=DIRECTION('',(-1.,0.,0.));
#32634=DIRECTION('',(0.,1.,0.));
#32635=DIRECTION('center_axis',(0.939692620785908,0.,-0.342020143325669));
#32636=DIRECTION('ref_axis',(-0.342020143325669,0.,-0.939692620785908));
#32637=DIRECTION('',(0.342020143325669,0.,0.939692620785908));
#32638=DIRECTION('',(-0.342020143325669,0.,-0.939692620785908));
#32639=DIRECTION('',(0.,1.,0.));
#32640=DIRECTION('center_axis',(0.,0.,-1.));
#32641=DIRECTION('ref_axis',(-1.,0.,0.));
#32642=DIRECTION('',(1.,0.,0.));
#32643=DIRECTION('',(-1.,0.,0.));
#32644=DIRECTION('',(0.,1.,0.));
#32645=DIRECTION('center_axis',(-0.939692620785908,0.,-0.342020143325669));
#32646=DIRECTION('ref_axis',(-0.342020143325669,0.,0.939692620785908));
#32647=DIRECTION('',(0.342020143325669,0.,-0.939692620785908));
#32648=DIRECTION('',(-0.342020143325669,0.,0.939692620785908));
#32649=DIRECTION('',(0.,1.,0.));
#32650=DIRECTION('center_axis',(0.,0.,-1.));
#32651=DIRECTION('ref_axis',(-1.,0.,0.));
#32652=DIRECTION('',(1.,0.,0.));
#32653=DIRECTION('',(-1.,0.,0.));
#32654=DIRECTION('',(0.,1.,0.));
#32655=DIRECTION('center_axis',(0.939692620785908,0.,-0.34202014332567));
#32656=DIRECTION('ref_axis',(-0.34202014332567,0.,-0.939692620785908));
#32657=DIRECTION('',(0.34202014332567,0.,0.939692620785908));
#32658=DIRECTION('',(-0.34202014332567,0.,-0.939692620785908));
#32659=DIRECTION('',(0.,1.,0.));
#32660=DIRECTION('center_axis',(0.,0.,-1.));
#32661=DIRECTION('ref_axis',(-1.,0.,0.));
#32662=DIRECTION('',(1.,0.,0.));
#32663=DIRECTION('',(-1.,0.,0.));
#32664=DIRECTION('',(0.,1.,0.));
#32665=DIRECTION('center_axis',(-0.939692620785908,0.,-0.342020143325669));
#32666=DIRECTION('ref_axis',(-0.342020143325669,0.,0.939692620785908));
#32667=DIRECTION('',(0.342020143325669,0.,-0.939692620785908));
#32668=DIRECTION('',(-0.342020143325669,0.,0.939692620785908));
#32669=DIRECTION('',(0.,1.,0.));
#32670=DIRECTION('center_axis',(0.,0.,-1.));
#32671=DIRECTION('ref_axis',(-1.,0.,0.));
#32672=DIRECTION('',(1.,0.,0.));
#32673=DIRECTION('',(-1.,0.,0.));
#32674=DIRECTION('',(0.,1.,0.));
#32675=DIRECTION('center_axis',(0.939692620785908,0.,-0.342020143325669));
#32676=DIRECTION('ref_axis',(-0.342020143325669,0.,-0.939692620785908));
#32677=DIRECTION('',(0.342020143325669,0.,0.939692620785908));
#32678=DIRECTION('',(-0.342020143325669,0.,-0.939692620785908));
#32679=DIRECTION('',(0.,1.,0.));
#32680=DIRECTION('center_axis',(0.,0.,-1.));
#32681=DIRECTION('ref_axis',(-1.,0.,0.));
#32682=DIRECTION('',(1.,0.,0.));
#32683=DIRECTION('',(-1.,0.,0.));
#32684=DIRECTION('',(0.,1.,0.));
#32685=DIRECTION('center_axis',(-0.939692620785909,0.,-0.342020143325668));
#32686=DIRECTION('ref_axis',(-0.342020143325668,0.,0.939692620785909));
#32687=DIRECTION('',(0.342020143325668,0.,-0.939692620785909));
#32688=DIRECTION('',(-0.342020143325668,0.,0.939692620785909));
#32689=DIRECTION('',(0.,1.,0.));
#32690=DIRECTION('center_axis',(0.,0.,-1.));
#32691=DIRECTION('ref_axis',(-1.,0.,0.));
#32692=DIRECTION('',(1.,0.,0.));
#32693=DIRECTION('',(-1.,0.,0.));
#32694=DIRECTION('',(0.,1.,0.));
#32695=DIRECTION('center_axis',(0.939692620785908,0.,-0.342020143325669));
#32696=DIRECTION('ref_axis',(-0.342020143325669,0.,-0.939692620785908));
#32697=DIRECTION('',(0.342020143325669,0.,0.939692620785908));
#32698=DIRECTION('',(-0.342020143325669,0.,-0.939692620785908));
#32699=DIRECTION('',(0.,1.,0.));
#32700=DIRECTION('center_axis',(0.,0.,-1.));
#32701=DIRECTION('ref_axis',(-1.,0.,0.));
#32702=DIRECTION('',(1.,0.,0.));
#32703=DIRECTION('',(-1.,0.,0.));
#32704=DIRECTION('',(0.,1.,0.));
#32705=DIRECTION('center_axis',(-0.939692620785908,0.,-0.342020143325669));
#32706=DIRECTION('ref_axis',(-0.342020143325669,0.,0.939692620785908));
#32707=DIRECTION('',(0.342020143325669,0.,-0.939692620785908));
#32708=DIRECTION('',(-0.342020143325669,0.,0.939692620785908));
#32709=DIRECTION('',(0.,1.,0.));
#32710=DIRECTION('center_axis',(0.,0.,-1.));
#32711=DIRECTION('ref_axis',(-1.,0.,0.));
#32712=DIRECTION('',(1.,0.,0.));
#32713=DIRECTION('',(-1.,0.,0.));
#32714=DIRECTION('',(0.,1.,0.));
#32715=DIRECTION('center_axis',(0.939692620785908,0.,-0.342020143325669));
#32716=DIRECTION('ref_axis',(-0.342020143325669,0.,-0.939692620785908));
#32717=DIRECTION('',(0.342020143325669,0.,0.939692620785908));
#32718=DIRECTION('',(-0.342020143325669,0.,-0.939692620785908));
#32719=DIRECTION('',(0.,1.,0.));
#32720=DIRECTION('center_axis',(0.,0.,-1.));
#32721=DIRECTION('ref_axis',(-1.,0.,0.));
#32722=DIRECTION('',(1.,0.,0.));
#32723=DIRECTION('',(-1.,0.,0.));
#32724=DIRECTION('',(0.,1.,0.));
#32725=DIRECTION('center_axis',(-0.939692620785908,0.,-0.342020143325669));
#32726=DIRECTION('ref_axis',(-0.342020143325669,0.,0.939692620785908));
#32727=DIRECTION('',(0.342020143325669,0.,-0.939692620785908));
#32728=DIRECTION('',(-0.342020143325669,0.,0.939692620785908));
#32729=DIRECTION('',(0.,1.,0.));
#32730=DIRECTION('center_axis',(0.,0.,-1.));
#32731=DIRECTION('ref_axis',(-1.,0.,0.));
#32732=DIRECTION('',(1.,0.,0.));
#32733=DIRECTION('',(-1.,0.,0.));
#32734=DIRECTION('',(0.,1.,0.));
#32735=DIRECTION('center_axis',(0.939692620785908,0.,-0.342020143325669));
#32736=DIRECTION('ref_axis',(-0.342020143325669,0.,-0.939692620785908));
#32737=DIRECTION('',(0.342020143325669,0.,0.939692620785908));
#32738=DIRECTION('',(-0.342020143325669,0.,-0.939692620785908));
#32739=DIRECTION('',(0.,1.,0.));
#32740=DIRECTION('center_axis',(0.,0.,-1.));
#32741=DIRECTION('ref_axis',(-1.,0.,0.));
#32742=DIRECTION('',(1.,0.,0.));
#32743=DIRECTION('',(-1.,0.,0.));
#32744=DIRECTION('',(0.,1.,0.));
#32745=DIRECTION('center_axis',(-0.939692620785908,0.,-0.342020143325669));
#32746=DIRECTION('ref_axis',(-0.342020143325669,0.,0.939692620785908));
#32747=DIRECTION('',(0.342020143325669,0.,-0.939692620785908));
#32748=DIRECTION('',(-0.342020143325669,0.,0.939692620785908));
#32749=DIRECTION('',(0.,1.,0.));
#32750=DIRECTION('center_axis',(0.,0.,-1.));
#32751=DIRECTION('ref_axis',(-1.,0.,0.));
#32752=DIRECTION('',(1.,0.,0.));
#32753=DIRECTION('',(-1.,0.,0.));
#32754=DIRECTION('',(0.,1.,0.));
#32755=DIRECTION('center_axis',(0.939692620785908,0.,-0.342020143325669));
#32756=DIRECTION('ref_axis',(-0.342020143325669,0.,-0.939692620785908));
#32757=DIRECTION('',(0.342020143325669,0.,0.939692620785908));
#32758=DIRECTION('',(-0.342020143325669,0.,-0.939692620785908));
#32759=DIRECTION('',(0.,1.,0.));
#32760=DIRECTION('center_axis',(0.,0.,-1.));
#32761=DIRECTION('ref_axis',(-1.,0.,0.));
#32762=DIRECTION('',(1.,0.,0.));
#32763=DIRECTION('',(-1.,0.,0.));
#32764=DIRECTION('',(0.,1.,0.));
#32765=DIRECTION('center_axis',(-0.939692620785908,0.,-0.342020143325669));
#32766=DIRECTION('ref_axis',(-0.342020143325669,0.,0.939692620785908));
#32767=DIRECTION('',(0.342020143325669,0.,-0.939692620785908));
#32768=DIRECTION('',(-0.342020143325669,0.,0.939692620785908));
#32769=DIRECTION('',(0.,1.,0.));
#32770=DIRECTION('center_axis',(0.,0.,-1.));
#32771=DIRECTION('ref_axis',(-1.,0.,0.));
#32772=DIRECTION('',(1.,0.,0.));
#32773=DIRECTION('',(-1.,0.,0.));
#32774=DIRECTION('',(0.,1.,0.));
#32775=DIRECTION('center_axis',(0.939692620785908,0.,-0.342020143325669));
#32776=DIRECTION('ref_axis',(-0.342020143325669,0.,-0.939692620785908));
#32777=DIRECTION('',(0.342020143325669,0.,0.939692620785908));
#32778=DIRECTION('',(-0.342020143325669,0.,-0.939692620785908));
#32779=DIRECTION('',(0.,1.,0.));
#32780=DIRECTION('center_axis',(0.,0.,-1.));
#32781=DIRECTION('ref_axis',(-1.,0.,0.));
#32782=DIRECTION('',(1.,0.,0.));
#32783=DIRECTION('',(-1.,0.,0.));
#32784=DIRECTION('',(0.,1.,0.));
#32785=DIRECTION('center_axis',(-0.939692620785908,0.,-0.342020143325669));
#32786=DIRECTION('ref_axis',(-0.342020143325669,0.,0.939692620785908));
#32787=DIRECTION('',(0.342020143325669,0.,-0.939692620785908));
#32788=DIRECTION('',(-0.342020143325669,0.,0.939692620785908));
#32789=DIRECTION('',(0.,1.,0.));
#32790=DIRECTION('center_axis',(0.,0.,-1.));
#32791=DIRECTION('ref_axis',(-1.,0.,0.));
#32792=DIRECTION('',(1.,0.,0.));
#32793=DIRECTION('',(-1.,0.,0.));
#32794=DIRECTION('',(0.,1.,0.));
#32795=DIRECTION('center_axis',(0.939692620785909,0.,-0.342020143325668));
#32796=DIRECTION('ref_axis',(-0.342020143325668,0.,-0.939692620785909));
#32797=DIRECTION('',(0.342020143325668,0.,0.939692620785909));
#32798=DIRECTION('',(-0.342020143325668,0.,-0.939692620785909));
#32799=DIRECTION('',(0.,1.,0.));
#32800=DIRECTION('center_axis',(0.,0.,-1.));
#32801=DIRECTION('ref_axis',(-1.,0.,0.));
#32802=DIRECTION('',(1.,0.,0.));
#32803=DIRECTION('',(-1.,0.,0.));
#32804=DIRECTION('',(0.,1.,0.));
#32805=DIRECTION('center_axis',(-0.939692620785908,0.,-0.342020143325669));
#32806=DIRECTION('ref_axis',(-0.342020143325669,0.,0.939692620785908));
#32807=DIRECTION('',(0.342020143325669,0.,-0.939692620785908));
#32808=DIRECTION('',(-0.342020143325669,0.,0.939692620785908));
#32809=DIRECTION('',(0.,1.,0.));
#32810=DIRECTION('center_axis',(0.,0.,-1.));
#32811=DIRECTION('ref_axis',(-1.,0.,0.));
#32812=DIRECTION('',(1.,0.,0.));
#32813=DIRECTION('',(-1.,0.,0.));
#32814=DIRECTION('',(0.,1.,0.));
#32815=DIRECTION('center_axis',(0.939692620785908,0.,-0.342020143325669));
#32816=DIRECTION('ref_axis',(-0.342020143325669,0.,-0.939692620785908));
#32817=DIRECTION('',(0.342020143325669,0.,0.939692620785908));
#32818=DIRECTION('',(-0.342020143325669,0.,-0.939692620785908));
#32819=DIRECTION('',(0.,1.,0.));
#32820=DIRECTION('center_axis',(0.,0.,-1.));
#32821=DIRECTION('ref_axis',(-1.,0.,0.));
#32822=DIRECTION('',(1.,0.,0.));
#32823=DIRECTION('',(-1.,0.,0.));
#32824=DIRECTION('',(0.,1.,0.));
#32825=DIRECTION('center_axis',(-0.939692620785908,0.,-0.34202014332567));
#32826=DIRECTION('ref_axis',(-0.34202014332567,0.,0.939692620785908));
#32827=DIRECTION('',(0.34202014332567,0.,-0.939692620785908));
#32828=DIRECTION('',(-0.34202014332567,0.,0.939692620785908));
#32829=DIRECTION('',(0.,1.,0.));
#32830=DIRECTION('center_axis',(0.,0.,-1.));
#32831=DIRECTION('ref_axis',(-1.,0.,0.));
#32832=DIRECTION('',(1.,0.,0.));
#32833=DIRECTION('',(-1.,0.,0.));
#32834=DIRECTION('',(0.,1.,0.));
#32835=DIRECTION('center_axis',(0.939692620785908,0.,-0.342020143325669));
#32836=DIRECTION('ref_axis',(-0.342020143325669,0.,-0.939692620785908));
#32837=DIRECTION('',(0.342020143325669,0.,0.939692620785908));
#32838=DIRECTION('',(-0.342020143325669,0.,-0.939692620785908));
#32839=DIRECTION('',(0.,1.,0.));
#32840=DIRECTION('center_axis',(0.,0.,-1.));
#32841=DIRECTION('ref_axis',(-1.,0.,0.));
#32842=DIRECTION('',(1.,0.,0.));
#32843=DIRECTION('',(-1.,0.,0.));
#32844=DIRECTION('',(0.,1.,0.));
#32845=DIRECTION('center_axis',(-0.939692620785908,0.,-0.342020143325669));
#32846=DIRECTION('ref_axis',(-0.342020143325669,0.,0.939692620785908));
#32847=DIRECTION('',(0.342020143325669,0.,-0.939692620785908));
#32848=DIRECTION('',(-0.342020143325669,0.,0.939692620785908));
#32849=DIRECTION('',(0.,1.,0.));
#32850=DIRECTION('center_axis',(0.,0.,-1.));
#32851=DIRECTION('ref_axis',(-1.,0.,0.));
#32852=DIRECTION('',(1.,0.,0.));
#32853=DIRECTION('',(-1.,0.,0.));
#32854=DIRECTION('',(0.,1.,0.));
#32855=DIRECTION('center_axis',(0.939692620785908,0.,-0.34202014332567));
#32856=DIRECTION('ref_axis',(-0.34202014332567,0.,-0.939692620785908));
#32857=DIRECTION('',(0.34202014332567,0.,0.939692620785908));
#32858=DIRECTION('',(-0.34202014332567,0.,-0.939692620785908));
#32859=DIRECTION('',(0.,1.,0.));
#32860=DIRECTION('center_axis',(0.,0.,-1.));
#32861=DIRECTION('ref_axis',(-1.,0.,0.));
#32862=DIRECTION('',(1.,0.,0.));
#32863=DIRECTION('',(-1.,0.,0.));
#32864=DIRECTION('',(0.,1.,0.));
#32865=DIRECTION('center_axis',(-0.939692620785908,0.,-0.34202014332567));
#32866=DIRECTION('ref_axis',(-0.34202014332567,0.,0.939692620785908));
#32867=DIRECTION('',(0.34202014332567,0.,-0.939692620785908));
#32868=DIRECTION('',(-0.34202014332567,0.,0.939692620785908));
#32869=DIRECTION('',(0.,1.,0.));
#32870=DIRECTION('center_axis',(0.,0.,-1.));
#32871=DIRECTION('ref_axis',(-1.,0.,0.));
#32872=DIRECTION('',(1.,0.,0.));
#32873=DIRECTION('',(-1.,0.,0.));
#32874=DIRECTION('',(0.,1.,0.));
#32875=DIRECTION('center_axis',(0.939692620785908,0.,-0.342020143325669));
#32876=DIRECTION('ref_axis',(-0.342020143325669,0.,-0.939692620785908));
#32877=DIRECTION('',(0.342020143325669,0.,0.939692620785908));
#32878=DIRECTION('',(-0.342020143325669,0.,-0.939692620785908));
#32879=DIRECTION('',(0.,1.,0.));
#32880=DIRECTION('center_axis',(0.,0.,-1.));
#32881=DIRECTION('ref_axis',(-1.,0.,0.));
#32882=DIRECTION('',(1.,0.,0.));
#32883=DIRECTION('',(-1.,0.,0.));
#32884=DIRECTION('',(0.,1.,0.));
#32885=DIRECTION('center_axis',(-0.939692620785908,0.,-0.342020143325669));
#32886=DIRECTION('ref_axis',(-0.342020143325669,0.,0.939692620785908));
#32887=DIRECTION('',(0.342020143325669,0.,-0.939692620785908));
#32888=DIRECTION('',(-0.342020143325669,0.,0.939692620785908));
#32889=DIRECTION('',(0.,1.,0.));
#32890=DIRECTION('center_axis',(0.,0.,-1.));
#32891=DIRECTION('ref_axis',(-1.,0.,0.));
#32892=DIRECTION('',(1.,0.,0.));
#32893=DIRECTION('',(-1.,0.,0.));
#32894=DIRECTION('',(0.,1.,0.));
#32895=DIRECTION('center_axis',(0.939692620785909,0.,-0.342020143325668));
#32896=DIRECTION('ref_axis',(-0.342020143325668,0.,-0.939692620785909));
#32897=DIRECTION('',(0.342020143325668,0.,0.939692620785909));
#32898=DIRECTION('',(-0.342020143325668,0.,-0.939692620785909));
#32899=DIRECTION('',(0.,1.,0.));
#32900=DIRECTION('center_axis',(0.,0.,-1.));
#32901=DIRECTION('ref_axis',(-1.,0.,0.));
#32902=DIRECTION('',(1.,0.,0.));
#32903=DIRECTION('',(-1.,0.,0.));
#32904=DIRECTION('',(0.,1.,0.));
#32905=DIRECTION('center_axis',(-0.939692620785908,0.,-0.342020143325669));
#32906=DIRECTION('ref_axis',(-0.342020143325669,0.,0.939692620785908));
#32907=DIRECTION('',(0.342020143325669,0.,-0.939692620785908));
#32908=DIRECTION('',(-0.342020143325669,0.,0.939692620785908));
#32909=DIRECTION('',(0.,1.,0.));
#32910=DIRECTION('center_axis',(0.,0.,-1.));
#32911=DIRECTION('ref_axis',(-1.,0.,0.));
#32912=DIRECTION('',(1.,0.,0.));
#32913=DIRECTION('',(-1.,0.,0.));
#32914=DIRECTION('',(0.,1.,0.));
#32915=DIRECTION('center_axis',(0.939692620785908,0.,-0.342020143325669));
#32916=DIRECTION('ref_axis',(-0.342020143325669,0.,-0.939692620785908));
#32917=DIRECTION('',(0.342020143325669,0.,0.939692620785908));
#32918=DIRECTION('',(-0.342020143325669,0.,-0.939692620785908));
#32919=DIRECTION('',(0.,1.,0.));
#32920=DIRECTION('center_axis',(0.,0.,-1.));
#32921=DIRECTION('ref_axis',(-1.,0.,0.));
#32922=DIRECTION('',(1.,0.,0.));
#32923=DIRECTION('',(-1.,0.,0.));
#32924=DIRECTION('',(0.,1.,0.));
#32925=DIRECTION('center_axis',(-0.939692620785908,0.,-0.342020143325669));
#32926=DIRECTION('ref_axis',(-0.342020143325669,0.,0.939692620785908));
#32927=DIRECTION('',(0.342020143325669,0.,-0.939692620785908));
#32928=DIRECTION('',(-0.342020143325669,0.,0.939692620785908));
#32929=DIRECTION('',(0.,1.,0.));
#32930=DIRECTION('center_axis',(0.,0.,-1.));
#32931=DIRECTION('ref_axis',(-1.,0.,0.));
#32932=DIRECTION('',(1.,0.,0.));
#32933=DIRECTION('',(-1.,0.,0.));
#32934=DIRECTION('',(0.,1.,0.));
#32935=DIRECTION('center_axis',(0.939692620785908,0.,-0.342020143325669));
#32936=DIRECTION('ref_axis',(-0.342020143325669,0.,-0.939692620785908));
#32937=DIRECTION('',(0.342020143325669,0.,0.939692620785908));
#32938=DIRECTION('',(-0.342020143325669,0.,-0.939692620785908));
#32939=DIRECTION('',(0.,1.,0.));
#32940=DIRECTION('center_axis',(0.,0.,-1.));
#32941=DIRECTION('ref_axis',(-1.,0.,0.));
#32942=DIRECTION('',(1.,0.,0.));
#32943=DIRECTION('',(-1.,0.,0.));
#32944=DIRECTION('',(0.,1.,0.));
#32945=DIRECTION('center_axis',(-0.939692620785908,0.,-0.342020143325669));
#32946=DIRECTION('ref_axis',(-0.342020143325669,0.,0.939692620785908));
#32947=DIRECTION('',(0.342020143325669,0.,-0.939692620785908));
#32948=DIRECTION('',(-0.342020143325669,0.,0.939692620785908));
#32949=DIRECTION('',(0.,1.,0.));
#32950=DIRECTION('center_axis',(0.,0.,-1.));
#32951=DIRECTION('ref_axis',(-1.,0.,0.));
#32952=DIRECTION('',(1.,0.,0.));
#32953=DIRECTION('',(-1.,0.,0.));
#32954=DIRECTION('',(0.,1.,0.));
#32955=DIRECTION('center_axis',(0.939692620785908,0.,-0.342020143325669));
#32956=DIRECTION('ref_axis',(-0.342020143325669,0.,-0.939692620785908));
#32957=DIRECTION('',(0.342020143325669,0.,0.939692620785908));
#32958=DIRECTION('',(-0.342020143325669,0.,-0.939692620785908));
#32959=DIRECTION('',(0.,1.,0.));
#32960=DIRECTION('center_axis',(0.,0.,-1.));
#32961=DIRECTION('ref_axis',(-1.,0.,0.));
#32962=DIRECTION('',(1.,0.,0.));
#32963=DIRECTION('',(-1.,0.,0.));
#32964=DIRECTION('',(0.,1.,0.));
#32965=DIRECTION('center_axis',(-0.939692620785908,0.,-0.342020143325669));
#32966=DIRECTION('ref_axis',(-0.342020143325669,0.,0.939692620785908));
#32967=DIRECTION('',(0.342020143325669,0.,-0.939692620785908));
#32968=DIRECTION('',(-0.342020143325669,0.,0.939692620785908));
#32969=DIRECTION('',(0.,1.,0.));
#32970=DIRECTION('center_axis',(0.,0.,-1.));
#32971=DIRECTION('ref_axis',(-1.,0.,0.));
#32972=DIRECTION('',(1.,0.,0.));
#32973=DIRECTION('',(-1.,0.,0.));
#32974=DIRECTION('',(0.,1.,0.));
#32975=DIRECTION('center_axis',(0.939692620785908,0.,-0.342020143325669));
#32976=DIRECTION('ref_axis',(-0.342020143325669,0.,-0.939692620785908));
#32977=DIRECTION('',(0.342020143325669,0.,0.939692620785908));
#32978=DIRECTION('',(-0.342020143325669,0.,-0.939692620785908));
#32979=DIRECTION('',(0.,1.,0.));
#32980=DIRECTION('center_axis',(0.,0.,-1.));
#32981=DIRECTION('ref_axis',(-1.,0.,0.));
#32982=DIRECTION('',(1.,0.,0.));
#32983=DIRECTION('',(-1.,0.,0.));
#32984=DIRECTION('',(0.,1.,0.));
#32985=DIRECTION('center_axis',(-0.939692620785908,0.,-0.342020143325669));
#32986=DIRECTION('ref_axis',(-0.342020143325669,0.,0.939692620785908));
#32987=DIRECTION('',(0.342020143325669,0.,-0.939692620785908));
#32988=DIRECTION('',(-0.342020143325669,0.,0.939692620785908));
#32989=DIRECTION('',(0.,1.,0.));
#32990=DIRECTION('center_axis',(0.,0.,-1.));
#32991=DIRECTION('ref_axis',(-1.,0.,0.));
#32992=DIRECTION('',(1.,0.,0.));
#32993=DIRECTION('',(-1.,0.,0.));
#32994=DIRECTION('',(0.,1.,0.));
#32995=DIRECTION('center_axis',(0.939692620785909,0.,-0.342020143325667));
#32996=DIRECTION('ref_axis',(-0.342020143325667,0.,-0.939692620785909));
#32997=DIRECTION('',(0.342020143325667,0.,0.939692620785909));
#32998=DIRECTION('',(-0.342020143325667,0.,-0.939692620785909));
#32999=DIRECTION('',(0.,1.,0.));
#33000=DIRECTION('center_axis',(0.,0.,-1.));
#33001=DIRECTION('ref_axis',(-1.,0.,0.));
#33002=DIRECTION('',(1.,0.,0.));
#33003=DIRECTION('',(-1.,0.,0.));
#33004=DIRECTION('',(0.,1.,0.));
#33005=DIRECTION('center_axis',(-0.939692620785908,0.,-0.342020143325669));
#33006=DIRECTION('ref_axis',(-0.342020143325669,0.,0.939692620785908));
#33007=DIRECTION('',(0.342020143325669,0.,-0.939692620785908));
#33008=DIRECTION('',(-0.342020143325669,0.,0.939692620785908));
#33009=DIRECTION('',(0.,1.,0.));
#33010=DIRECTION('center_axis',(0.,0.,-1.));
#33011=DIRECTION('ref_axis',(-1.,0.,0.));
#33012=DIRECTION('',(1.,0.,0.));
#33013=DIRECTION('',(-1.,0.,0.));
#33014=DIRECTION('',(0.,1.,0.));
#33015=DIRECTION('center_axis',(0.939692620785908,0.,-0.342020143325669));
#33016=DIRECTION('ref_axis',(-0.342020143325669,0.,-0.939692620785908));
#33017=DIRECTION('',(0.342020143325669,0.,0.939692620785908));
#33018=DIRECTION('',(-0.342020143325669,0.,-0.939692620785908));
#33019=DIRECTION('',(0.,1.,0.));
#33020=DIRECTION('center_axis',(0.,0.,-1.));
#33021=DIRECTION('ref_axis',(-1.,0.,0.));
#33022=DIRECTION('',(1.,0.,0.));
#33023=DIRECTION('',(-1.,0.,0.));
#33024=DIRECTION('',(0.,1.,0.));
#33025=DIRECTION('center_axis',(-0.939692620785908,0.,-0.342020143325669));
#33026=DIRECTION('ref_axis',(-0.342020143325669,0.,0.939692620785908));
#33027=DIRECTION('',(0.342020143325669,0.,-0.939692620785908));
#33028=DIRECTION('',(-0.342020143325669,0.,0.939692620785908));
#33029=DIRECTION('',(0.,1.,0.));
#33030=DIRECTION('center_axis',(0.,0.,-1.));
#33031=DIRECTION('ref_axis',(-1.,0.,0.));
#33032=DIRECTION('',(1.,0.,0.));
#33033=DIRECTION('',(-1.,0.,0.));
#33034=DIRECTION('',(0.,1.,0.));
#33035=DIRECTION('center_axis',(0.939692620785908,0.,-0.342020143325669));
#33036=DIRECTION('ref_axis',(-0.342020143325669,0.,-0.939692620785908));
#33037=DIRECTION('',(0.342020143325669,0.,0.939692620785908));
#33038=DIRECTION('',(-0.342020143325669,0.,-0.939692620785908));
#33039=DIRECTION('',(0.,1.,0.));
#33040=DIRECTION('center_axis',(0.,0.,-1.));
#33041=DIRECTION('ref_axis',(-1.,0.,0.));
#33042=DIRECTION('',(1.,0.,0.));
#33043=DIRECTION('',(-1.,0.,0.));
#33044=DIRECTION('',(0.,1.,0.));
#33045=DIRECTION('center_axis',(-0.939692620785908,0.,-0.342020143325669));
#33046=DIRECTION('ref_axis',(-0.342020143325669,0.,0.939692620785908));
#33047=DIRECTION('',(0.342020143325669,0.,-0.939692620785908));
#33048=DIRECTION('',(-0.342020143325669,0.,0.939692620785908));
#33049=DIRECTION('',(0.,1.,0.));
#33050=DIRECTION('center_axis',(0.,0.,-1.));
#33051=DIRECTION('ref_axis',(-1.,0.,0.));
#33052=DIRECTION('',(1.,0.,0.));
#33053=DIRECTION('',(-1.,0.,0.));
#33054=DIRECTION('',(0.,1.,0.));
#33055=DIRECTION('center_axis',(0.939692620785908,0.,-0.342020143325669));
#33056=DIRECTION('ref_axis',(-0.342020143325669,0.,-0.939692620785908));
#33057=DIRECTION('',(0.342020143325669,0.,0.939692620785908));
#33058=DIRECTION('',(-0.342020143325669,0.,-0.939692620785908));
#33059=DIRECTION('',(0.,1.,0.));
#33060=DIRECTION('center_axis',(0.,0.,-1.));
#33061=DIRECTION('ref_axis',(-1.,0.,0.));
#33062=DIRECTION('',(1.,0.,0.));
#33063=DIRECTION('',(-1.,0.,0.));
#33064=DIRECTION('',(0.,1.,0.));
#33065=DIRECTION('center_axis',(-0.939692620785909,0.,-0.342020143325667));
#33066=DIRECTION('ref_axis',(-0.342020143325667,0.,0.939692620785909));
#33067=DIRECTION('',(0.342020143325667,0.,-0.939692620785909));
#33068=DIRECTION('',(-0.342020143325667,0.,0.939692620785909));
#33069=DIRECTION('',(0.,1.,0.));
#33070=DIRECTION('center_axis',(0.,0.,-1.));
#33071=DIRECTION('ref_axis',(-1.,0.,0.));
#33072=DIRECTION('',(1.,0.,0.));
#33073=DIRECTION('',(-1.,0.,0.));
#33074=DIRECTION('',(0.,1.,0.));
#33075=DIRECTION('center_axis',(0.939692620785909,0.,-0.342020143325667));
#33076=DIRECTION('ref_axis',(-0.342020143325667,0.,-0.939692620785909));
#33077=DIRECTION('',(0.342020143325667,0.,0.939692620785909));
#33078=DIRECTION('',(-0.342020143325667,0.,-0.939692620785909));
#33079=DIRECTION('',(0.,1.,0.));
#33080=DIRECTION('center_axis',(0.,0.,-1.));
#33081=DIRECTION('ref_axis',(-1.,0.,0.));
#33082=DIRECTION('',(1.,0.,0.));
#33083=DIRECTION('',(-1.,0.,0.));
#33084=DIRECTION('',(0.,1.,0.));
#33085=DIRECTION('center_axis',(-0.939692620785909,0.,-0.342020143325667));
#33086=DIRECTION('ref_axis',(-0.342020143325667,0.,0.939692620785909));
#33087=DIRECTION('',(0.342020143325667,0.,-0.939692620785909));
#33088=DIRECTION('',(-0.342020143325667,0.,0.939692620785909));
#33089=DIRECTION('',(0.,1.,0.));
#33090=DIRECTION('center_axis',(0.,0.,-1.));
#33091=DIRECTION('ref_axis',(-1.,0.,0.));
#33092=DIRECTION('',(1.,0.,0.));
#33093=DIRECTION('',(-1.,0.,0.));
#33094=DIRECTION('',(0.,1.,0.));
#33095=DIRECTION('center_axis',(0.939692620785909,0.,-0.342020143325667));
#33096=DIRECTION('ref_axis',(-0.342020143325667,0.,-0.939692620785909));
#33097=DIRECTION('',(0.342020143325667,0.,0.939692620785909));
#33098=DIRECTION('',(-0.342020143325667,0.,-0.939692620785909));
#33099=DIRECTION('',(0.,1.,0.));
#33100=DIRECTION('center_axis',(0.,0.,-1.));
#33101=DIRECTION('ref_axis',(-1.,0.,0.));
#33102=DIRECTION('',(1.,0.,0.));
#33103=DIRECTION('',(-1.,0.,0.));
#33104=DIRECTION('',(0.,1.,0.));
#33105=DIRECTION('center_axis',(-0.939692620785909,0.,-0.342020143325667));
#33106=DIRECTION('ref_axis',(-0.342020143325667,0.,0.939692620785909));
#33107=DIRECTION('',(0.342020143325667,0.,-0.939692620785909));
#33108=DIRECTION('',(-0.342020143325667,0.,0.939692620785909));
#33109=DIRECTION('',(0.,1.,0.));
#33110=DIRECTION('center_axis',(0.,0.,-1.));
#33111=DIRECTION('ref_axis',(-1.,0.,0.));
#33112=DIRECTION('',(1.,0.,0.));
#33113=DIRECTION('',(-1.,0.,0.));
#33114=DIRECTION('',(0.,1.,0.));
#33115=DIRECTION('center_axis',(0.939692620785908,0.,-0.342020143325671));
#33116=DIRECTION('ref_axis',(-0.342020143325671,0.,-0.939692620785908));
#33117=DIRECTION('',(0.342020143325671,0.,0.939692620785907));
#33118=DIRECTION('',(-0.342020143325671,0.,-0.939692620785907));
#33119=DIRECTION('',(0.,1.,0.));
#33120=DIRECTION('center_axis',(0.,0.,-1.));
#33121=DIRECTION('ref_axis',(-1.,0.,0.));
#33122=DIRECTION('',(1.,0.,0.));
#33123=DIRECTION('',(-1.,0.,0.));
#33124=DIRECTION('',(0.,1.,0.));
#33125=DIRECTION('center_axis',(-0.939692620785908,0.,-0.342020143325671));
#33126=DIRECTION('ref_axis',(-0.342020143325671,0.,0.939692620785908));
#33127=DIRECTION('',(0.342020143325671,0.,-0.939692620785907));
#33128=DIRECTION('',(-0.342020143325671,0.,0.939692620785907));
#33129=DIRECTION('',(0.,1.,0.));
#33130=DIRECTION('center_axis',(0.,0.,-1.));
#33131=DIRECTION('ref_axis',(-1.,0.,0.));
#33132=DIRECTION('',(1.,0.,0.));
#33133=DIRECTION('',(-1.,0.,0.));
#33134=DIRECTION('',(0.,1.,0.));
#33135=DIRECTION('center_axis',(0.939692620785908,0.,-0.342020143325671));
#33136=DIRECTION('ref_axis',(-0.342020143325671,0.,-0.939692620785908));
#33137=DIRECTION('',(0.342020143325671,0.,0.939692620785907));
#33138=DIRECTION('',(-0.342020143325671,0.,-0.939692620785907));
#33139=DIRECTION('',(0.,1.,0.));
#33140=DIRECTION('center_axis',(0.,0.,-1.));
#33141=DIRECTION('ref_axis',(-1.,0.,0.));
#33142=DIRECTION('',(1.,0.,0.));
#33143=DIRECTION('',(-1.,0.,0.));
#33144=DIRECTION('',(0.,1.,0.));
#33145=DIRECTION('center_axis',(-0.939692620785908,0.,-0.342020143325671));
#33146=DIRECTION('ref_axis',(-0.342020143325671,0.,0.939692620785908));
#33147=DIRECTION('',(0.342020143325671,0.,-0.939692620785907));
#33148=DIRECTION('',(-0.342020143325671,0.,0.939692620785907));
#33149=DIRECTION('',(0.,1.,0.));
#33150=DIRECTION('center_axis',(0.,0.,-1.));
#33151=DIRECTION('ref_axis',(-1.,0.,0.));
#33152=DIRECTION('',(1.,0.,0.));
#33153=DIRECTION('',(-1.,0.,0.));
#33154=DIRECTION('',(0.,1.,0.));
#33155=DIRECTION('center_axis',(0.939692620785908,0.,-0.342020143325671));
#33156=DIRECTION('ref_axis',(-0.342020143325671,0.,-0.939692620785908));
#33157=DIRECTION('',(0.342020143325671,0.,0.939692620785907));
#33158=DIRECTION('',(-0.342020143325671,0.,-0.939692620785907));
#33159=DIRECTION('',(0.,1.,0.));
#33160=DIRECTION('center_axis',(0.,0.,-1.));
#33161=DIRECTION('ref_axis',(-1.,0.,0.));
#33162=DIRECTION('',(1.,0.,0.));
#33163=DIRECTION('',(-1.,0.,0.));
#33164=DIRECTION('',(0.,1.,0.));
#33165=DIRECTION('center_axis',(-0.939692620785908,0.,-0.342020143325671));
#33166=DIRECTION('ref_axis',(-0.342020143325671,0.,0.939692620785908));
#33167=DIRECTION('',(0.342020143325671,0.,-0.939692620785907));
#33168=DIRECTION('',(-0.342020143325671,0.,0.939692620785907));
#33169=DIRECTION('',(0.,1.,0.));
#33170=DIRECTION('center_axis',(0.,0.,-1.));
#33171=DIRECTION('ref_axis',(-1.,0.,0.));
#33172=DIRECTION('',(1.,0.,0.));
#33173=DIRECTION('',(-1.,0.,0.));
#33174=DIRECTION('',(0.,1.,0.));
#33175=DIRECTION('center_axis',(0.939692620785909,0.,-0.342020143325667));
#33176=DIRECTION('ref_axis',(-0.342020143325667,0.,-0.939692620785909));
#33177=DIRECTION('',(0.342020143325667,0.,0.939692620785909));
#33178=DIRECTION('',(-0.342020143325667,0.,-0.939692620785909));
#33179=DIRECTION('',(0.,1.,0.));
#33180=DIRECTION('center_axis',(0.,0.,-1.));
#33181=DIRECTION('ref_axis',(-1.,0.,0.));
#33182=DIRECTION('',(1.,0.,0.));
#33183=DIRECTION('',(-1.,0.,0.));
#33184=DIRECTION('',(0.,1.,0.));
#33185=DIRECTION('center_axis',(-0.939692620785909,0.,-0.342020143325667));
#33186=DIRECTION('ref_axis',(-0.342020143325667,0.,0.939692620785909));
#33187=DIRECTION('',(0.342020143325667,0.,-0.939692620785909));
#33188=DIRECTION('',(-0.342020143325667,0.,0.939692620785909));
#33189=DIRECTION('',(0.,1.,0.));
#33190=DIRECTION('center_axis',(0.,0.,-1.));
#33191=DIRECTION('ref_axis',(-1.,0.,0.));
#33192=DIRECTION('',(1.,0.,0.));
#33193=DIRECTION('',(-1.,0.,0.));
#33194=DIRECTION('',(0.,1.,0.));
#33195=DIRECTION('center_axis',(0.939692620785909,0.,-0.342020143325667));
#33196=DIRECTION('ref_axis',(-0.342020143325667,0.,-0.939692620785909));
#33197=DIRECTION('',(0.342020143325667,0.,0.939692620785909));
#33198=DIRECTION('',(-0.342020143325667,0.,-0.939692620785909));
#33199=DIRECTION('',(0.,1.,0.));
#33200=DIRECTION('center_axis',(0.,0.,-1.));
#33201=DIRECTION('ref_axis',(-1.,0.,0.));
#33202=DIRECTION('',(1.,0.,0.));
#33203=DIRECTION('',(-1.,0.,0.));
#33204=DIRECTION('',(0.,1.,0.));
#33205=DIRECTION('center_axis',(-0.939692620785909,0.,-0.342020143325667));
#33206=DIRECTION('ref_axis',(-0.342020143325667,0.,0.939692620785909));
#33207=DIRECTION('',(0.342020143325667,0.,-0.939692620785909));
#33208=DIRECTION('',(-0.342020143325667,0.,0.939692620785909));
#33209=DIRECTION('',(0.,1.,0.));
#33210=DIRECTION('center_axis',(0.,0.,-1.));
#33211=DIRECTION('ref_axis',(-1.,0.,0.));
#33212=DIRECTION('',(1.,0.,0.));
#33213=DIRECTION('',(-1.,0.,0.));
#33214=DIRECTION('',(0.,1.,0.));
#33215=DIRECTION('center_axis',(0.939692620785909,0.,-0.342020143325667));
#33216=DIRECTION('ref_axis',(-0.342020143325667,0.,-0.939692620785909));
#33217=DIRECTION('',(0.342020143325667,0.,0.939692620785909));
#33218=DIRECTION('',(-0.342020143325667,0.,-0.939692620785909));
#33219=DIRECTION('',(0.,1.,0.));
#33220=DIRECTION('center_axis',(0.,0.,-1.));
#33221=DIRECTION('ref_axis',(-1.,0.,0.));
#33222=DIRECTION('',(1.,0.,0.));
#33223=DIRECTION('',(-1.,0.,0.));
#33224=DIRECTION('',(0.,1.,0.));
#33225=DIRECTION('center_axis',(-0.939692620785909,0.,-0.342020143325667));
#33226=DIRECTION('ref_axis',(-0.342020143325667,0.,0.939692620785909));
#33227=DIRECTION('',(0.342020143325667,0.,-0.939692620785909));
#33228=DIRECTION('',(-0.342020143325667,0.,0.939692620785909));
#33229=DIRECTION('',(0.,1.,0.));
#33230=DIRECTION('center_axis',(0.,0.,-1.));
#33231=DIRECTION('ref_axis',(-1.,0.,0.));
#33232=DIRECTION('',(1.,0.,0.));
#33233=DIRECTION('',(-1.,0.,0.));
#33234=DIRECTION('',(0.,1.,0.));
#33235=DIRECTION('center_axis',(0.939692620785908,0.,-0.342020143325671));
#33236=DIRECTION('ref_axis',(-0.342020143325671,0.,-0.939692620785908));
#33237=DIRECTION('',(0.342020143325671,0.,0.939692620785907));
#33238=DIRECTION('',(-0.342020143325671,0.,-0.939692620785907));
#33239=DIRECTION('',(0.,1.,0.));
#33240=DIRECTION('center_axis',(0.,0.,-1.));
#33241=DIRECTION('ref_axis',(-1.,0.,0.));
#33242=DIRECTION('',(1.,0.,0.));
#33243=DIRECTION('',(-1.,0.,0.));
#33244=DIRECTION('',(0.,1.,0.));
#33245=DIRECTION('center_axis',(-0.939692620785908,0.,-0.342020143325671));
#33246=DIRECTION('ref_axis',(-0.342020143325671,0.,0.939692620785908));
#33247=DIRECTION('',(0.342020143325671,0.,-0.939692620785907));
#33248=DIRECTION('',(-0.342020143325671,0.,0.939692620785907));
#33249=DIRECTION('',(0.,1.,0.));
#33250=DIRECTION('center_axis',(0.,0.,-1.));
#33251=DIRECTION('ref_axis',(-1.,0.,0.));
#33252=DIRECTION('',(1.,0.,0.));
#33253=DIRECTION('',(-1.,0.,0.));
#33254=DIRECTION('',(0.,1.,0.));
#33255=DIRECTION('center_axis',(0.939692620785908,0.,-0.342020143325671));
#33256=DIRECTION('ref_axis',(-0.342020143325671,0.,-0.939692620785908));
#33257=DIRECTION('',(0.342020143325671,0.,0.939692620785907));
#33258=DIRECTION('',(-0.342020143325671,0.,-0.939692620785907));
#33259=DIRECTION('',(0.,1.,0.));
#33260=DIRECTION('center_axis',(0.,0.,-1.));
#33261=DIRECTION('ref_axis',(-1.,0.,0.));
#33262=DIRECTION('',(1.,0.,0.));
#33263=DIRECTION('',(-1.,0.,0.));
#33264=DIRECTION('',(0.,1.,0.));
#33265=DIRECTION('center_axis',(-0.939692620785909,0.,-0.342020143325667));
#33266=DIRECTION('ref_axis',(-0.342020143325667,0.,0.939692620785909));
#33267=DIRECTION('',(0.342020143325667,0.,-0.939692620785909));
#33268=DIRECTION('',(-0.342020143325667,0.,0.939692620785909));
#33269=DIRECTION('',(0.,1.,0.));
#33270=DIRECTION('center_axis',(0.,0.,-1.));
#33271=DIRECTION('ref_axis',(-1.,0.,0.));
#33272=DIRECTION('',(1.,0.,0.));
#33273=DIRECTION('',(-1.,0.,0.));
#33274=DIRECTION('',(0.,1.,0.));
#33275=DIRECTION('center_axis',(0.939692620785909,0.,-0.342020143325667));
#33276=DIRECTION('ref_axis',(-0.342020143325667,0.,-0.939692620785909));
#33277=DIRECTION('',(0.342020143325667,0.,0.939692620785909));
#33278=DIRECTION('',(-0.342020143325667,0.,-0.939692620785909));
#33279=DIRECTION('',(0.,1.,0.));
#33280=DIRECTION('center_axis',(0.,0.,-1.));
#33281=DIRECTION('ref_axis',(-1.,0.,0.));
#33282=DIRECTION('',(1.,0.,0.));
#33283=DIRECTION('',(-1.,0.,0.));
#33284=DIRECTION('',(0.,1.,0.));
#33285=DIRECTION('center_axis',(-0.939692620785909,0.,-0.342020143325667));
#33286=DIRECTION('ref_axis',(-0.342020143325667,0.,0.939692620785909));
#33287=DIRECTION('',(0.342020143325667,0.,-0.939692620785909));
#33288=DIRECTION('',(-0.342020143325667,0.,0.939692620785909));
#33289=DIRECTION('',(0.,1.,0.));
#33290=DIRECTION('center_axis',(0.,0.,-1.));
#33291=DIRECTION('ref_axis',(-1.,0.,0.));
#33292=DIRECTION('',(1.,0.,0.));
#33293=DIRECTION('',(-1.,0.,0.));
#33294=DIRECTION('',(0.,1.,0.));
#33295=DIRECTION('center_axis',(0.939692620785909,0.,-0.342020143325667));
#33296=DIRECTION('ref_axis',(-0.342020143325667,0.,-0.939692620785909));
#33297=DIRECTION('',(0.342020143325667,0.,0.939692620785909));
#33298=DIRECTION('',(-0.342020143325667,0.,-0.939692620785909));
#33299=DIRECTION('',(0.,1.,0.));
#33300=DIRECTION('center_axis',(0.,0.,-1.));
#33301=DIRECTION('ref_axis',(-1.,0.,0.));
#33302=DIRECTION('',(1.,0.,0.));
#33303=DIRECTION('',(-1.,0.,0.));
#33304=DIRECTION('',(0.,1.,0.));
#33305=DIRECTION('center_axis',(-0.939692620785911,0.,-0.342020143325663));
#33306=DIRECTION('ref_axis',(-0.342020143325663,0.,0.939692620785911));
#33307=DIRECTION('',(0.342020143325663,0.,-0.939692620785911));
#33308=DIRECTION('',(-0.342020143325663,0.,0.939692620785911));
#33309=DIRECTION('',(0.,1.,0.));
#33310=DIRECTION('center_axis',(0.,0.,-1.));
#33311=DIRECTION('ref_axis',(-1.,0.,0.));
#33312=DIRECTION('',(1.,0.,0.));
#33313=DIRECTION('',(-1.,0.,0.));
#33314=DIRECTION('',(0.,1.,0.));
#33315=DIRECTION('center_axis',(0.939692620785911,0.,-0.342020143325663));
#33316=DIRECTION('ref_axis',(-0.342020143325663,0.,-0.939692620785911));
#33317=DIRECTION('',(0.342020143325663,0.,0.939692620785911));
#33318=DIRECTION('',(-0.342020143325663,0.,-0.939692620785911));
#33319=DIRECTION('',(0.,1.,0.));
#33320=DIRECTION('center_axis',(0.,0.,-1.));
#33321=DIRECTION('ref_axis',(-1.,0.,0.));
#33322=DIRECTION('',(1.,0.,0.));
#33323=DIRECTION('',(-1.,0.,0.));
#33324=DIRECTION('',(0.,1.,0.));
#33325=DIRECTION('center_axis',(-0.939692620785911,0.,-0.342020143325663));
#33326=DIRECTION('ref_axis',(-0.342020143325663,0.,0.939692620785911));
#33327=DIRECTION('',(0.342020143325663,0.,-0.939692620785911));
#33328=DIRECTION('',(-0.342020143325663,0.,0.939692620785911));
#33329=DIRECTION('',(0.,1.,0.));
#33330=DIRECTION('center_axis',(0.,0.,-1.));
#33331=DIRECTION('ref_axis',(-1.,0.,0.));
#33332=DIRECTION('',(1.,0.,0.));
#33333=DIRECTION('',(-1.,0.,0.));
#33334=DIRECTION('',(0.,1.,0.));
#33335=DIRECTION('center_axis',(0.939692620785911,0.,-0.342020143325663));
#33336=DIRECTION('ref_axis',(-0.342020143325663,0.,-0.939692620785911));
#33337=DIRECTION('',(0.342020143325663,0.,0.939692620785911));
#33338=DIRECTION('',(-0.342020143325663,0.,-0.939692620785911));
#33339=DIRECTION('',(0.,1.,0.));
#33340=DIRECTION('center_axis',(0.,0.,-1.));
#33341=DIRECTION('ref_axis',(-1.,0.,0.));
#33342=DIRECTION('',(1.,0.,0.));
#33343=DIRECTION('',(-1.,0.,0.));
#33344=DIRECTION('',(0.,1.,0.));
#33345=DIRECTION('center_axis',(-0.939692620785909,0.,-0.342020143325667));
#33346=DIRECTION('ref_axis',(-0.342020143325667,0.,0.939692620785909));
#33347=DIRECTION('',(0.342020143325667,0.,-0.939692620785909));
#33348=DIRECTION('',(-0.342020143325667,0.,0.939692620785909));
#33349=DIRECTION('',(0.,1.,0.));
#33350=DIRECTION('center_axis',(0.,0.,-1.));
#33351=DIRECTION('ref_axis',(-1.,0.,0.));
#33352=DIRECTION('',(1.,0.,0.));
#33353=DIRECTION('',(-1.,0.,0.));
#33354=DIRECTION('',(0.,1.,0.));
#33355=DIRECTION('center_axis',(0.939692620785909,0.,-0.342020143325667));
#33356=DIRECTION('ref_axis',(-0.342020143325667,0.,-0.939692620785909));
#33357=DIRECTION('',(0.342020143325667,0.,0.939692620785909));
#33358=DIRECTION('',(-0.342020143325667,0.,-0.939692620785909));
#33359=DIRECTION('',(0.,1.,0.));
#33360=DIRECTION('center_axis',(0.,0.,-1.));
#33361=DIRECTION('ref_axis',(-1.,0.,0.));
#33362=DIRECTION('',(1.,0.,0.));
#33363=DIRECTION('',(-1.,0.,0.));
#33364=DIRECTION('',(0.,1.,0.));
#33365=DIRECTION('center_axis',(-0.939692620785909,0.,-0.342020143325667));
#33366=DIRECTION('ref_axis',(-0.342020143325667,0.,0.939692620785909));
#33367=DIRECTION('',(0.342020143325667,0.,-0.939692620785909));
#33368=DIRECTION('',(-0.342020143325667,0.,0.939692620785909));
#33369=DIRECTION('',(0.,1.,0.));
#33370=DIRECTION('center_axis',(0.,0.,-1.));
#33371=DIRECTION('ref_axis',(-1.,0.,0.));
#33372=DIRECTION('',(1.,0.,0.));
#33373=DIRECTION('',(-1.,0.,0.));
#33374=DIRECTION('',(0.,1.,0.));
#33375=DIRECTION('center_axis',(0.939692620785909,0.,-0.342020143325667));
#33376=DIRECTION('ref_axis',(-0.342020143325667,0.,-0.939692620785909));
#33377=DIRECTION('',(0.342020143325667,0.,0.939692620785909));
#33378=DIRECTION('',(-0.342020143325667,0.,-0.939692620785909));
#33379=DIRECTION('',(0.,1.,0.));
#33380=DIRECTION('center_axis',(0.,0.,-1.));
#33381=DIRECTION('ref_axis',(-1.,0.,0.));
#33382=DIRECTION('',(1.,0.,0.));
#33383=DIRECTION('',(-1.,0.,0.));
#33384=DIRECTION('',(0.,1.,0.));
#33385=DIRECTION('center_axis',(-0.939692620785909,0.,-0.342020143325667));
#33386=DIRECTION('ref_axis',(-0.342020143325667,0.,0.939692620785909));
#33387=DIRECTION('',(0.342020143325667,0.,-0.939692620785909));
#33388=DIRECTION('',(-0.342020143325667,0.,0.939692620785909));
#33389=DIRECTION('',(0.,1.,0.));
#33390=DIRECTION('center_axis',(0.,0.,-1.));
#33391=DIRECTION('ref_axis',(-1.,0.,0.));
#33392=DIRECTION('',(1.,0.,0.));
#33393=DIRECTION('',(-1.,0.,0.));
#33394=DIRECTION('',(0.,1.,0.));
#33395=DIRECTION('center_axis',(0.939692620785909,0.,-0.342020143325667));
#33396=DIRECTION('ref_axis',(-0.342020143325667,0.,-0.939692620785909));
#33397=DIRECTION('',(0.342020143325667,0.,0.939692620785909));
#33398=DIRECTION('',(-0.342020143325667,0.,-0.939692620785909));
#33399=DIRECTION('',(0.,1.,0.));
#33400=DIRECTION('center_axis',(0.,0.,-1.));
#33401=DIRECTION('ref_axis',(-1.,0.,0.));
#33402=DIRECTION('',(1.,0.,0.));
#33403=DIRECTION('',(-1.,0.,0.));
#33404=DIRECTION('',(0.,1.,0.));
#33405=DIRECTION('center_axis',(-0.939692620785909,0.,-0.342020143325667));
#33406=DIRECTION('ref_axis',(-0.342020143325667,0.,0.939692620785909));
#33407=DIRECTION('',(0.342020143325667,0.,-0.939692620785909));
#33408=DIRECTION('',(-0.342020143325667,0.,0.939692620785909));
#33409=DIRECTION('',(0.,1.,0.));
#33410=DIRECTION('center_axis',(0.,0.,-1.));
#33411=DIRECTION('ref_axis',(-1.,0.,0.));
#33412=DIRECTION('',(1.,0.,0.));
#33413=DIRECTION('',(-1.,0.,0.));
#33414=DIRECTION('',(0.,1.,0.));
#33415=DIRECTION('center_axis',(0.939692620785909,0.,-0.342020143325667));
#33416=DIRECTION('ref_axis',(-0.342020143325667,0.,-0.939692620785909));
#33417=DIRECTION('',(0.342020143325667,0.,0.939692620785909));
#33418=DIRECTION('',(-0.342020143325667,0.,-0.939692620785909));
#33419=DIRECTION('',(0.,1.,0.));
#33420=DIRECTION('center_axis',(0.,0.,-1.));
#33421=DIRECTION('ref_axis',(-1.,0.,0.));
#33422=DIRECTION('',(1.,0.,0.));
#33423=DIRECTION('',(-1.,0.,0.));
#33424=DIRECTION('',(0.,1.,0.));
#33425=DIRECTION('center_axis',(-0.939692620785909,0.,-0.342020143325667));
#33426=DIRECTION('ref_axis',(-0.342020143325667,0.,0.939692620785909));
#33427=DIRECTION('',(0.342020143325667,0.,-0.939692620785909));
#33428=DIRECTION('',(-0.342020143325667,0.,0.939692620785909));
#33429=DIRECTION('',(0.,1.,0.));
#33430=DIRECTION('center_axis',(0.,0.,-1.));
#33431=DIRECTION('ref_axis',(-1.,0.,0.));
#33432=DIRECTION('',(1.,0.,0.));
#33433=DIRECTION('',(-1.,0.,0.));
#33434=DIRECTION('',(0.,1.,0.));
#33435=DIRECTION('center_axis',(0.939692620785909,0.,-0.342020143325667));
#33436=DIRECTION('ref_axis',(-0.342020143325667,0.,-0.939692620785909));
#33437=DIRECTION('',(0.342020143325667,0.,0.939692620785909));
#33438=DIRECTION('',(-0.342020143325667,0.,-0.939692620785909));
#33439=DIRECTION('center_axis',(0.,1.,0.));
#33440=DIRECTION('ref_axis',(1.,0.,0.));
#33441=DIRECTION('center_axis',(0.,1.,0.));
#33442=DIRECTION('ref_axis',(1.,0.,0.));
#33443=DIRECTION('axis',(0.,0.,1.));
#33444=DIRECTION('refdir',(1.,0.,0.));
#33445=DIRECTION('center_axis',(1.,0.,0.));
#33446=DIRECTION('ref_axis',(0.,0.,-1.));
#33447=DIRECTION('center_axis',(-1.,0.,0.));
#33448=DIRECTION('ref_axis',(0.,0.,-1.));
#33449=DIRECTION('',(0.707106781186548,-8.65956056235493E-17,0.707106781186547));
#33450=DIRECTION('center_axis',(1.,0.,0.));
#33451=DIRECTION('ref_axis',(0.,0.,-1.));
#33452=DIRECTION('center_axis',(1.,0.,0.));
#33453=DIRECTION('ref_axis',(0.,0.,-1.));
#33454=DIRECTION('',(0.,-1.,0.));
#33455=DIRECTION('',(0.,0.,1.));
#33456=DIRECTION('',(0.,1.,0.));
#33457=DIRECTION('',(0.,0.,1.));
#33458=DIRECTION('',(0.,-1.,0.));
#33459=DIRECTION('',(0.,0.,-1.));
#33460=DIRECTION('',(0.,1.,0.));
#33461=DIRECTION('',(0.,0.,1.));
#33462=DIRECTION('center_axis',(1.,0.,0.));
#33463=DIRECTION('ref_axis',(0.,0.,-1.));
#33464=DIRECTION('center_axis',(1.,0.,0.));
#33465=DIRECTION('ref_axis',(0.,0.,-1.));
#33466=DIRECTION('center_axis',(1.,0.,0.));
#33467=DIRECTION('ref_axis',(0.,0.,-1.));
#33468=DIRECTION('center_axis',(1.,0.,0.));
#33469=DIRECTION('ref_axis',(0.,0.,-1.));
#33470=DIRECTION('',(0.,-1.,0.));
#33471=DIRECTION('',(0.,0.,1.));
#33472=DIRECTION('',(0.,1.,0.));
#33473=DIRECTION('',(0.,0.,-1.));
#33474=DIRECTION('',(0.,-1.,0.));
#33475=DIRECTION('',(0.,0.,-1.));
#33476=DIRECTION('',(0.,0.,-1.));
#33477=DIRECTION('',(0.,1.,0.));
#33478=DIRECTION('',(0.,0.,-1.));
#33479=DIRECTION('',(0.,-1.,0.));
#33480=DIRECTION('',(0.,0.,1.));
#33481=DIRECTION('',(0.,1.,0.));
#33482=DIRECTION('center_axis',(1.,0.,0.));
#33483=DIRECTION('ref_axis',(0.,0.,-1.));
#33484=DIRECTION('center_axis',(1.,0.,0.));
#33485=DIRECTION('ref_axis',(0.,0.,-1.));
#33486=DIRECTION('center_axis',(1.,0.,0.));
#33487=DIRECTION('ref_axis',(0.,0.,-1.));
#33488=DIRECTION('center_axis',(-1.,0.,0.));
#33489=DIRECTION('ref_axis',(0.,0.,-1.));
#33490=DIRECTION('',(-1.,0.,0.));
#33491=DIRECTION('center_axis',(1.,0.,0.));
#33492=DIRECTION('ref_axis',(0.,0.,-1.));
#33493=DIRECTION('center_axis',(1.,0.,0.));
#33494=DIRECTION('ref_axis',(0.,0.,-1.));
#33495=DIRECTION('center_axis',(-1.,0.,0.));
#33496=DIRECTION('ref_axis',(0.,0.,-1.));
#33497=DIRECTION('',(0.707106781186548,-8.65956056235493E-17,0.707106781186547));
#33498=DIRECTION('center_axis',(-1.,0.,0.));
#33499=DIRECTION('ref_axis',(0.,0.,-1.));
#33500=DIRECTION('',(-1.,0.,0.));
#33501=DIRECTION('center_axis',(1.,0.,0.));
#33502=DIRECTION('ref_axis',(0.,0.,-1.));
#33503=DIRECTION('center_axis',(1.,0.,0.));
#33504=DIRECTION('ref_axis',(0.,0.,-1.));
#33505=DIRECTION('center_axis',(-1.,0.,0.));
#33506=DIRECTION('ref_axis',(0.,0.,-1.));
#33507=DIRECTION('',(0.707106781186548,-8.65956056235493E-17,0.707106781186547));
#33508=DIRECTION('center_axis',(-1.,0.,0.));
#33509=DIRECTION('ref_axis',(0.,0.,-1.));
#33510=DIRECTION('',(-1.,0.,0.));
#33511=DIRECTION('center_axis',(1.,0.,0.));
#33512=DIRECTION('ref_axis',(0.,0.,-1.));
#33513=DIRECTION('center_axis',(1.,0.,0.));
#33514=DIRECTION('ref_axis',(0.,0.,-1.));
#33515=DIRECTION('center_axis',(-1.,0.,0.));
#33516=DIRECTION('ref_axis',(0.,0.,-1.));
#33517=DIRECTION('',(0.707106781186548,-8.65956056235493E-17,0.707106781186547));
#33518=DIRECTION('center_axis',(-1.,0.,0.));
#33519=DIRECTION('ref_axis',(0.,0.,-1.));
#33520=DIRECTION('',(-1.,0.,0.));
#33521=DIRECTION('center_axis',(1.,0.,0.));
#33522=DIRECTION('ref_axis',(0.,0.,-1.));
#33523=DIRECTION('center_axis',(1.,0.,0.));
#33524=DIRECTION('ref_axis',(0.,0.,-1.));
#33525=DIRECTION('center_axis',(-1.,0.,0.));
#33526=DIRECTION('ref_axis',(0.,0.,-1.));
#33527=DIRECTION('',(0.707106781186548,-8.65956056235493E-17,0.707106781186547));
#33528=DIRECTION('center_axis',(-1.,0.,0.));
#33529=DIRECTION('ref_axis',(0.,0.,-1.));
#33530=DIRECTION('',(-1.,0.,0.));
#33531=DIRECTION('center_axis',(1.,0.,0.));
#33532=DIRECTION('ref_axis',(0.,0.,-1.));
#33533=DIRECTION('center_axis',(1.,0.,0.));
#33534=DIRECTION('ref_axis',(0.,0.,-1.));
#33535=DIRECTION('center_axis',(-1.,0.,0.));
#33536=DIRECTION('ref_axis',(0.,0.,-1.));
#33537=DIRECTION('',(0.707106781186548,-8.65956056235493E-17,0.707106781186547));
#33538=DIRECTION('center_axis',(-1.,0.,0.));
#33539=DIRECTION('ref_axis',(0.,0.,-1.));
#33540=DIRECTION('',(-1.,0.,0.));
#33541=DIRECTION('center_axis',(1.,0.,0.));
#33542=DIRECTION('ref_axis',(0.,0.,-1.));
#33543=DIRECTION('center_axis',(1.,0.,0.));
#33544=DIRECTION('ref_axis',(0.,0.,-1.));
#33545=DIRECTION('center_axis',(-1.,0.,0.));
#33546=DIRECTION('ref_axis',(0.,0.,-1.));
#33547=DIRECTION('',(0.707106781186548,-8.65956056235493E-17,0.707106781186547));
#33548=DIRECTION('center_axis',(-1.,0.,0.));
#33549=DIRECTION('ref_axis',(0.,0.,-1.));
#33550=DIRECTION('',(-1.,0.,0.));
#33551=DIRECTION('center_axis',(1.,0.,0.));
#33552=DIRECTION('ref_axis',(0.,0.,-1.));
#33553=DIRECTION('center_axis',(1.,0.,0.));
#33554=DIRECTION('ref_axis',(0.,0.,-1.));
#33555=DIRECTION('center_axis',(-1.,0.,0.));
#33556=DIRECTION('ref_axis',(0.,0.,-1.));
#33557=DIRECTION('',(0.707106781186548,-8.65956056235493E-17,0.707106781186547));
#33558=DIRECTION('center_axis',(-1.,0.,0.));
#33559=DIRECTION('ref_axis',(0.,0.,-1.));
#33560=DIRECTION('',(-1.,0.,0.));
#33561=DIRECTION('center_axis',(1.,0.,0.));
#33562=DIRECTION('ref_axis',(0.,0.,-1.));
#33563=DIRECTION('center_axis',(0.,1.,0.));
#33564=DIRECTION('ref_axis',(0.,0.,1.));
#33565=DIRECTION('',(0.,0.,1.));
#33566=DIRECTION('',(1.,0.,0.));
#33567=DIRECTION('',(1.,0.,0.));
#33568=DIRECTION('center_axis',(0.,0.,1.));
#33569=DIRECTION('ref_axis',(0.,-1.,0.));
#33570=DIRECTION('',(0.,-1.,0.));
#33571=DIRECTION('',(1.,0.,0.));
#33572=DIRECTION('center_axis',(0.,1.,0.));
#33573=DIRECTION('ref_axis',(0.,0.,1.));
#33574=DIRECTION('',(0.,0.,1.));
#33575=DIRECTION('',(1.,0.,0.));
#33576=DIRECTION('center_axis',(0.,0.,-1.));
#33577=DIRECTION('ref_axis',(0.,1.,0.));
#33578=DIRECTION('',(0.,1.,0.));
#33579=DIRECTION('',(1.,0.,0.));
#33580=DIRECTION('center_axis',(0.,-1.,0.));
#33581=DIRECTION('ref_axis',(0.,0.,-1.));
#33582=DIRECTION('',(0.,0.,-1.));
#33583=DIRECTION('',(1.,0.,0.));
#33584=DIRECTION('center_axis',(0.,0.,1.));
#33585=DIRECTION('ref_axis',(0.,-1.,0.));
#33586=DIRECTION('',(0.,-1.,0.));
#33587=DIRECTION('center_axis',(0.,0.,-1.));
#33588=DIRECTION('ref_axis',(0.,1.,0.));
#33589=DIRECTION('',(0.,1.,0.));
#33590=DIRECTION('',(1.,0.,0.));
#33591=DIRECTION('',(1.,0.,0.));
#33592=DIRECTION('center_axis',(0.,-1.,0.));
#33593=DIRECTION('ref_axis',(0.,0.,-1.));
#33594=DIRECTION('',(0.,0.,-1.));
#33595=DIRECTION('',(1.,0.,0.));
#33596=DIRECTION('center_axis',(0.,0.,1.));
#33597=DIRECTION('ref_axis',(0.,-1.,0.));
#33598=DIRECTION('',(0.,-1.,0.));
#33599=DIRECTION('',(1.,0.,0.));
#33600=DIRECTION('center_axis',(0.,1.,0.));
#33601=DIRECTION('ref_axis',(0.,0.,1.));
#33602=DIRECTION('',(0.,0.,1.));
#33603=DIRECTION('',(1.,0.,0.));
#33604=DIRECTION('center_axis',(0.,0.,-1.));
#33605=DIRECTION('ref_axis',(0.,1.,0.));
#33606=DIRECTION('',(0.,1.,0.));
#33607=DIRECTION('',(1.,0.,0.));
#33608=DIRECTION('center_axis',(0.,1.,0.));
#33609=DIRECTION('ref_axis',(0.,0.,1.));
#33610=DIRECTION('',(0.,0.,1.));
#33611=DIRECTION('center_axis',(0.707106781186545,0.,-0.70710678118655));
#33612=DIRECTION('ref_axis',(-0.70710678118655,0.,-0.707106781186545));
#33613=DIRECTION('',(-0.577350269189627,-0.577350269189627,-0.577350269189623));
#33614=DIRECTION('',(0.,1.,0.));
#33615=DIRECTION('',(-0.577350269189627,-0.577350269189627,-0.577350269189623));
#33616=DIRECTION('center_axis',(0.707106781186548,-0.707106781186548,0.));
#33617=DIRECTION('ref_axis',(0.,0.,-1.));
#33618=DIRECTION('',(-0.577350269189629,-0.577350269189629,0.57735026918962));
#33619=DIRECTION('',(0.,0.,-1.));
#33620=DIRECTION('center_axis',(0.707106781186542,0.,0.707106781186553));
#33621=DIRECTION('ref_axis',(0.707106781186553,0.,-0.707106781186542));
#33622=DIRECTION('',(-0.577350269189629,0.577350269189629,0.57735026918962));
#33623=DIRECTION('',(0.,-1.,0.));
#33624=DIRECTION('center_axis',(0.707106781186548,0.707106781186548,0.));
#33625=DIRECTION('ref_axis',(0.,0.,-1.));
#33626=DIRECTION('',(-0.577350269189629,0.577350269189629,-0.57735026918962));
#33627=DIRECTION('',(0.,0.,1.));
#33628=DIRECTION('center_axis',(0.707106781186542,0.,-0.707106781186553));
#33629=DIRECTION('ref_axis',(-0.707106781186553,0.,-0.707106781186542));
#33630=DIRECTION('',(-0.577350269189629,-0.577350269189629,-0.57735026918962));
#33631=DIRECTION('',(0.,1.,0.));
#33632=DIRECTION('center_axis',(0.707106781186548,-0.707106781186548,0.));
#33633=DIRECTION('ref_axis',(0.,0.,-1.));
#33634=DIRECTION('',(0.,0.,-1.));
#33635=DIRECTION('',(-0.577350269189627,-0.577350269189627,0.577350269189623));
#33636=DIRECTION('center_axis',(0.707106781186545,0.,0.70710678118655));
#33637=DIRECTION('ref_axis',(0.70710678118655,0.,-0.707106781186545));
#33638=DIRECTION('',(0.,-1.,0.));
#33639=DIRECTION('',(-0.577350269189626,-0.577350269189626,0.577350269189626));
#33640=DIRECTION('center_axis',(0.707106781186548,-0.707106781186548,0.));
#33641=DIRECTION('ref_axis',(0.,0.,-1.));
#33642=DIRECTION('',(0.,0.,-1.));
#33643=DIRECTION('center_axis',(0.,-1.,0.));
#33644=DIRECTION('ref_axis',(0.,0.,-1.));
#33645=DIRECTION('',(1.,0.,0.));
#33646=DIRECTION('',(0.,0.,1.));
#33647=DIRECTION('',(1.,0.,0.));
#33648=DIRECTION('center_axis',(0.,0.,1.));
#33649=DIRECTION('ref_axis',(0.,-1.,0.));
#33650=DIRECTION('',(1.,0.,0.));
#33651=DIRECTION('',(0.,1.,0.));
#33652=DIRECTION('center_axis',(0.,-1.,0.));
#33653=DIRECTION('ref_axis',(0.,0.,-1.));
#33654=DIRECTION('',(1.,0.,0.));
#33655=DIRECTION('',(0.,0.,1.));
#33656=DIRECTION('center_axis',(0.,0.,-1.));
#33657=DIRECTION('ref_axis',(0.,1.,0.));
#33658=DIRECTION('',(1.,0.,0.));
#33659=DIRECTION('',(0.,-1.,0.));
#33660=DIRECTION('center_axis',(0.,0.,-1.));
#33661=DIRECTION('ref_axis',(0.,1.,0.));
#33662=DIRECTION('',(0.,-1.,0.));
#33663=DIRECTION('',(1.,0.,0.));
#33664=DIRECTION('center_axis',(0.,-1.,0.));
#33665=DIRECTION('ref_axis',(0.,0.,-1.));
#33666=DIRECTION('',(1.,0.,0.));
#33667=DIRECTION('',(0.,0.,1.));
#33668=DIRECTION('center_axis',(0.,0.,1.));
#33669=DIRECTION('ref_axis',(0.,-1.,0.));
#33670=DIRECTION('',(1.,0.,0.));
#33671=DIRECTION('',(0.,1.,0.));
#33672=DIRECTION('center_axis',(0.,1.,0.));
#33673=DIRECTION('ref_axis',(0.,0.,1.));
#33674=DIRECTION('',(0.,0.,-1.));
#33675=DIRECTION('center_axis',(1.,0.,0.));
#33676=DIRECTION('ref_axis',(0.,0.,-1.));
#33677=DIRECTION('axis',(0.,0.,1.));
#33678=DIRECTION('refdir',(1.,0.,0.));
#33679=DIRECTION('center_axis',(0.,0.,1.));
#33680=DIRECTION('ref_axis',(1.,0.,0.));
#33681=DIRECTION('center_axis',(0.,0.,1.));
#33682=DIRECTION('ref_axis',(1.,0.,0.));
#33683=DIRECTION('',(0.,0.,1.));
#33684=DIRECTION('center_axis',(0.,0.,-1.));
#33685=DIRECTION('ref_axis',(1.,0.,0.));
#33686=DIRECTION('center_axis',(0.,0.,1.));
#33687=DIRECTION('ref_axis',(1.,0.,0.));
#33688=DIRECTION('center_axis',(0.,0.,1.));
#33689=DIRECTION('ref_axis',(1.,0.,0.));
#33690=DIRECTION('',(0.,0.,1.));
#33691=DIRECTION('center_axis',(0.,0.,-1.));
#33692=DIRECTION('ref_axis',(1.,0.,0.));
#33693=DIRECTION('center_axis',(0.,-1.,0.));
#33694=DIRECTION('ref_axis',(1.,0.,0.));
#33695=DIRECTION('center_axis',(0.,1.,0.));
#33696=DIRECTION('ref_axis',(1.,0.,0.));
#33697=DIRECTION('',(-0.70710678118655,-0.707106781186545,-8.65956056235497E-17));
#33698=DIRECTION('center_axis',(0.,-1.,0.));
#33699=DIRECTION('ref_axis',(1.,0.,0.));
#33700=DIRECTION('center_axis',(0.,1.,0.));
#33701=DIRECTION('ref_axis',(1.,0.,0.));
#33702=DIRECTION('',(0.,1.,0.));
#33703=DIRECTION('center_axis',(0.707106781186548,-0.707106781186548,0.));
#33704=DIRECTION('ref_axis',(0.707106781186548,0.707106781186548,0.));
#33705=DIRECTION('center_axis',(0.,1.,0.));
#33706=DIRECTION('ref_axis',(1.,0.,0.));
#33707=DIRECTION('center_axis',(-0.707106781186548,-0.707106781186548,0.));
#33708=DIRECTION('ref_axis',(0.707106781186548,-0.707106781186548,0.));
#33709=DIRECTION('center_axis',(0.,1.,0.));
#33710=DIRECTION('ref_axis',(1.,0.,0.));
#33711=DIRECTION('center_axis',(0.707106781186548,-0.707106781186548,0.));
#33712=DIRECTION('ref_axis',(0.707106781186548,0.707106781186548,0.));
#33713=DIRECTION('center_axis',(0.,-1.,0.));
#33714=DIRECTION('ref_axis',(1.,0.,0.));
#33715=DIRECTION('',(1.,0.,0.));
#33716=DIRECTION('',(0.,0.,1.));
#33717=DIRECTION('',(1.,0.,0.));
#33718=DIRECTION('',(0.,0.,1.));
#33719=DIRECTION('center_axis',(0.,-1.,0.));
#33720=DIRECTION('ref_axis',(1.,0.,0.));
#33721=DIRECTION('center_axis',(0.,1.,0.));
#33722=DIRECTION('ref_axis',(1.,0.,0.));
#33723=DIRECTION('',(-0.70710678118655,-0.707106781186545,-8.65956056235497E-17));
#33724=DIRECTION('center_axis',(0.,-1.,0.));
#33725=DIRECTION('ref_axis',(1.,0.,0.));
#33726=DIRECTION('center_axis',(0.,1.,0.));
#33727=DIRECTION('ref_axis',(1.,0.,0.));
#33728=DIRECTION('',(0.,1.,0.));
#33729=DIRECTION('center_axis',(0.707106781186548,-0.707106781186548,0.));
#33730=DIRECTION('ref_axis',(0.707106781186548,0.707106781186548,0.));
#33731=DIRECTION('center_axis',(0.,1.,0.));
#33732=DIRECTION('ref_axis',(1.,0.,0.));
#33733=DIRECTION('center_axis',(-0.707106781186548,-0.707106781186548,0.));
#33734=DIRECTION('ref_axis',(0.707106781186548,-0.707106781186548,0.));
#33735=DIRECTION('center_axis',(0.,1.,0.));
#33736=DIRECTION('ref_axis',(1.,0.,0.));
#33737=DIRECTION('center_axis',(0.707106781186548,-0.707106781186548,0.));
#33738=DIRECTION('ref_axis',(0.707106781186548,0.707106781186548,0.));
#33739=DIRECTION('center_axis',(0.,-1.,0.));
#33740=DIRECTION('ref_axis',(1.,0.,0.));
#33741=DIRECTION('',(1.,0.,0.));
#33742=DIRECTION('',(0.,0.,1.));
#33743=DIRECTION('',(1.,0.,0.));
#33744=DIRECTION('',(0.,0.,1.));
#33745=DIRECTION('center_axis',(0.,-1.,0.));
#33746=DIRECTION('ref_axis',(1.,0.,0.));
#33747=DIRECTION('center_axis',(0.,-1.,0.));
#33748=DIRECTION('ref_axis',(1.,0.,0.));
#33749=DIRECTION('center_axis',(1.,0.,0.));
#33750=DIRECTION('ref_axis',(0.,0.,-1.));
#33751=DIRECTION('center_axis',(1.,0.,0.));
#33752=DIRECTION('ref_axis',(0.,0.,-1.));
#33753=DIRECTION('',(1.,0.,0.));
#33754=DIRECTION('center_axis',(1.,0.,0.));
#33755=DIRECTION('ref_axis',(0.,0.,-1.));
#33756=DIRECTION('center_axis',(1.,0.,0.));
#33757=DIRECTION('ref_axis',(0.,0.,-1.));
#33758=DIRECTION('center_axis',(0.,-1.,0.));
#33759=DIRECTION('ref_axis',(1.,0.,0.));
#33760=DIRECTION('center_axis',(0.,-1.,0.));
#33761=DIRECTION('ref_axis',(1.,0.,0.));
#33762=DIRECTION('center_axis',(-1.,0.,0.));
#33763=DIRECTION('ref_axis',(0.,0.,-1.));
#33764=DIRECTION('center_axis',(-1.,0.,0.));
#33765=DIRECTION('ref_axis',(0.,0.,-1.));
#33766=DIRECTION('',(-1.,0.,0.));
#33767=DIRECTION('center_axis',(-1.,0.,0.));
#33768=DIRECTION('ref_axis',(0.,0.,-1.));
#33769=DIRECTION('center_axis',(-1.,0.,0.));
#33770=DIRECTION('ref_axis',(0.,0.,-1.));
#33771=DIRECTION('center_axis',(-1.,0.,0.));
#33772=DIRECTION('ref_axis',(0.,0.,-1.));
#33773=DIRECTION('',(-0.707106781186548,8.65956056235493E-17,0.707106781186547));
#33774=DIRECTION('center_axis',(-1.,0.,0.));
#33775=DIRECTION('ref_axis',(0.,0.,-1.));
#33776=DIRECTION('center_axis',(-1.,0.,0.));
#33777=DIRECTION('ref_axis',(0.,-1.,0.));
#33778=DIRECTION('',(0.,-0.707106781186553,0.707106781186542));
#33779=DIRECTION('',(0.,0.,1.));
#33780=DIRECTION('',(0.,0.70710678118655,0.707106781186545));
#33781=DIRECTION('',(0.,-1.,0.));
#33782=DIRECTION('',(0.,-1.,0.));
#33783=DIRECTION('center_axis',(-1.,0.,0.));
#33784=DIRECTION('ref_axis',(0.,1.,0.));
#33785=DIRECTION('',(-0.515038074910058,-0.85716730070211,1.04972719113862E-16));
#33786=DIRECTION('center_axis',(1.,0.,0.));
#33787=DIRECTION('ref_axis',(0.,0.,-1.));
#33788=DIRECTION('',(0.707106781186548,-8.65956056235493E-17,0.707106781186547));
#33789=DIRECTION('center_axis',(1.,0.,0.));
#33790=DIRECTION('ref_axis',(0.,0.,-1.));
#33791=DIRECTION('center_axis',(1.,0.,0.));
#33792=DIRECTION('ref_axis',(0.,1.,0.));
#33793=DIRECTION('',(0.,0.707106781186553,-0.707106781186542));
#33794=DIRECTION('',(0.,1.,0.));
#33795=DIRECTION('',(0.,1.,0.));
#33796=DIRECTION('',(0.,-0.70710678118655,-0.707106781186545));
#33797=DIRECTION('',(0.,0.,1.));
#33798=DIRECTION('center_axis',(1.,0.,0.));
#33799=DIRECTION('ref_axis',(0.,1.,0.));
#33800=DIRECTION('',(0.515038074910058,-0.85716730070211,-1.04972719113862E-16));
#33801=DIRECTION('center_axis',(0.,0.707106781186542,0.707106781186553));
#33802=DIRECTION('ref_axis',(1.,0.,0.));
#33803=DIRECTION('',(1.,0.,0.));
#33804=DIRECTION('',(-1.,0.,0.));
#33805=DIRECTION('center_axis',(0.,1.,0.));
#33806=DIRECTION('ref_axis',(-1.,0.,0.));
#33807=DIRECTION('',(1.,0.,0.));
#33808=DIRECTION('center_axis',(0.,0.707106781186545,-0.70710678118655));
#33809=DIRECTION('ref_axis',(-1.,0.,0.));
#33810=DIRECTION('',(-1.,0.,0.));
#33811=DIRECTION('center_axis',(-1.,0.,0.));
#33812=DIRECTION('ref_axis',(0.,-1.,0.));
#33813=DIRECTION('',(0.,-1.,0.));
#33814=DIRECTION('',(0.,-1.,0.));
#33815=DIRECTION('',(0.,0.,1.));
#33816=DIRECTION('center_axis',(0.,-1.,0.));
#33817=DIRECTION('ref_axis',(1.,0.,0.));
#33818=DIRECTION('',(1.,0.,0.));
#33819=DIRECTION('',(1.,0.,0.));
#33820=DIRECTION('',(0.,0.,1.));
#33821=DIRECTION('center_axis',(1.,0.,0.));
#33822=DIRECTION('ref_axis',(0.,1.,0.));
#33823=DIRECTION('',(0.,1.,0.));
#33824=DIRECTION('',(0.,1.,0.));
#33825=DIRECTION('center_axis',(0.,0.,1.));
#33826=DIRECTION('ref_axis',(1.,0.,0.));
#33827=DIRECTION('center_axis',(0.,0.,1.));
#33828=DIRECTION('ref_axis',(1.,0.,0.));
#33829=DIRECTION('axis',(0.,0.,1.));
#33830=DIRECTION('refdir',(1.,0.,0.));
#33831=DIRECTION('center_axis',(-1.,0.,0.));
#33832=DIRECTION('ref_axis',(0.,0.756725241443425,-0.653733056348224));
#33833=DIRECTION('',(1.,0.,0.));
#33834=DIRECTION('center_axis',(1.,0.,0.));
#33835=DIRECTION('ref_axis',(0.,-2.79741234551221E-14,-1.));
#33836=DIRECTION('center_axis',(-1.,0.,0.));
#33837=DIRECTION('ref_axis',(0.,0.756725241443425,-0.653733056348224));
#33838=DIRECTION('',(1.,0.,0.));
#33839=DIRECTION('center_axis',(-1.,0.,0.));
#33840=DIRECTION('ref_axis',(0.,0.756725241443425,-0.653733056348224));
#33841=DIRECTION('',(1.,0.,0.));
#33842=DIRECTION('center_axis',(-1.,0.,0.));
#33843=DIRECTION('ref_axis',(0.,0.756725241443425,-0.653733056348224));
#33844=DIRECTION('',(1.,0.,0.));
#33845=DIRECTION('center_axis',(-1.,0.,0.));
#33846=DIRECTION('ref_axis',(0.,0.756725241443425,-0.653733056348224));
#33847=DIRECTION('',(1.,0.,0.));
#33848=DIRECTION('center_axis',(-1.,0.,0.));
#33849=DIRECTION('ref_axis',(0.,0.756725241443425,-0.653733056348224));
#33850=DIRECTION('',(1.,0.,0.));
#33851=DIRECTION('center_axis',(-1.,0.,0.));
#33852=DIRECTION('ref_axis',(0.,0.756725241443425,-0.653733056348224));
#33853=DIRECTION('',(1.,0.,0.));
#33854=DIRECTION('center_axis',(-1.,0.,0.));
#33855=DIRECTION('ref_axis',(0.,0.,-1.));
#33856=DIRECTION('center_axis',(1.,0.,0.));
#33857=DIRECTION('ref_axis',(0.,0.,-1.));
#33858=DIRECTION('center_axis',(-1.,0.,0.));
#33859=DIRECTION('ref_axis',(0.,0.,-1.));
#33860=DIRECTION('center_axis',(-1.,0.,0.));
#33861=DIRECTION('ref_axis',(0.,0.961400218503714,-0.275153811278367));
#33862=DIRECTION('center_axis',(-1.,0.,0.));
#33863=DIRECTION('ref_axis',(0.,-2.79741234551221E-14,-1.));
#33864=DIRECTION('center_axis',(1.,0.,0.));
#33865=DIRECTION('ref_axis',(0.,0.,-1.));
#33866=DIRECTION('center_axis',(-1.,0.,0.));
#33867=DIRECTION('ref_axis',(0.,0.,-1.));
#33868=DIRECTION('center_axis',(-1.,0.,0.));
#33869=DIRECTION('ref_axis',(0.,0.,-1.));
#33870=DIRECTION('center_axis',(1.,0.,0.));
#33871=DIRECTION('ref_axis',(0.,0.,-1.));
#33872=DIRECTION('center_axis',(1.,0.,0.));
#33873=DIRECTION('ref_axis',(0.,0.,-1.));
#33874=DIRECTION('center_axis',(1.,0.,0.));
#33875=DIRECTION('ref_axis',(0.,0.,-1.));
#33876=DIRECTION('center_axis',(1.,0.,0.));
#33877=DIRECTION('ref_axis',(0.,0.,-1.));
#33878=DIRECTION('center_axis',(-1.,0.,0.));
#33879=DIRECTION('ref_axis',(0.,0.,-1.));
#33880=DIRECTION('center_axis',(0.,1.,0.));
#33881=DIRECTION('ref_axis',(0.,0.,1.));
#33882=DIRECTION('center_axis',(1.,0.,0.));
#33883=DIRECTION('ref_axis',(0.,0.,-1.));
#33884=DIRECTION('center_axis',(1.,0.,0.));
#33885=DIRECTION('ref_axis',(0.,0.,-1.));
#33886=DIRECTION('center_axis',(1.,0.,0.));
#33887=DIRECTION('ref_axis',(0.,0.,-1.));
#33888=DIRECTION('',(-0.707106781186548,8.65956056235493E-17,-0.707106781186547));
#33889=DIRECTION('center_axis',(1.,0.,0.));
#33890=DIRECTION('ref_axis',(0.,0.,-1.));
#33891=DIRECTION('center_axis',(1.,0.,0.));
#33892=DIRECTION('ref_axis',(0.,0.,-1.));
#33893=DIRECTION('center_axis',(0.,-0.188314866426192,-0.982108706347157));
#33894=DIRECTION('ref_axis',(0.,-0.982108706347157,0.188314866426192));
#33895=DIRECTION('',(1.,0.,0.));
#33896=DIRECTION('',(0.,-0.982108706347157,0.188314866426192));
#33897=DIRECTION('',(-1.,0.,0.));
#33898=DIRECTION('center_axis',(0.,-0.512859050871219,0.858472826558577));
#33899=DIRECTION('ref_axis',(0.,0.858472826558577,0.512859050871219));
#33900=DIRECTION('',(-1.,0.,0.));
#33901=DIRECTION('',(0.,0.858472826558577,0.512859050871219));
#33902=DIRECTION('center_axis',(-1.,0.,0.));
#33903=DIRECTION('ref_axis',(0.,-0.17364817766693,0.984807753012208));
#33904=DIRECTION('center_axis',(-1.,0.,0.));
#33905=DIRECTION('ref_axis',(0.,0.,-1.));
#33906=DIRECTION('center_axis',(-1.,0.,0.));
#33907=DIRECTION('ref_axis',(0.,0.,-1.));
#33908=DIRECTION('center_axis',(1.,0.,0.));
#33909=DIRECTION('ref_axis',(0.,0.,-1.));
#33910=DIRECTION('center_axis',(1.,0.,0.));
#33911=DIRECTION('ref_axis',(0.,0.,-1.));
#33912=DIRECTION('center_axis',(1.,0.,0.));
#33913=DIRECTION('ref_axis',(0.,0.,-1.));
#33914=DIRECTION('center_axis',(1.,0.,0.));
#33915=DIRECTION('ref_axis',(0.,0.,-1.));
#33916=DIRECTION('center_axis',(1.,0.,0.));
#33917=DIRECTION('ref_axis',(0.,0.,-1.));
#33918=DIRECTION('center_axis',(1.,0.,0.));
#33919=DIRECTION('ref_axis',(0.,0.,-1.));
#33920=DIRECTION('center_axis',(1.,0.,0.));
#33921=DIRECTION('ref_axis',(0.,0.,-1.));
#33922=DIRECTION('center_axis',(1.,0.,0.));
#33923=DIRECTION('ref_axis',(0.,0.,-1.));
#33924=DIRECTION('center_axis',(1.,0.,0.));
#33925=DIRECTION('ref_axis',(0.,0.,-1.));
#33926=DIRECTION('center_axis',(1.,0.,0.));
#33927=DIRECTION('ref_axis',(0.,0.,-1.));
#33928=DIRECTION('center_axis',(1.,0.,0.));
#33929=DIRECTION('ref_axis',(0.,0.,-1.));
#33930=DIRECTION('center_axis',(1.,0.,0.));
#33931=DIRECTION('ref_axis',(0.,0.,-1.));
#33932=DIRECTION('center_axis',(1.,0.,0.));
#33933=DIRECTION('ref_axis',(0.,0.,-1.));
#33934=DIRECTION('center_axis',(1.,0.,0.));
#33935=DIRECTION('ref_axis',(0.,0.,-1.));
#33936=DIRECTION('center_axis',(1.,0.,0.));
#33937=DIRECTION('ref_axis',(0.,0.,-1.));
#33938=DIRECTION('center_axis',(1.,0.,0.));
#33939=DIRECTION('ref_axis',(0.,0.,-1.));
#33940=DIRECTION('center_axis',(1.,0.,0.));
#33941=DIRECTION('ref_axis',(0.,0.,-1.));
#33942=DIRECTION('center_axis',(1.,0.,0.));
#33943=DIRECTION('ref_axis',(0.,0.,-1.));
#33944=DIRECTION('center_axis',(1.,0.,0.));
#33945=DIRECTION('ref_axis',(0.,0.,-1.));
#33946=DIRECTION('center_axis',(1.,0.,0.));
#33947=DIRECTION('ref_axis',(0.,0.,-1.));
#33948=DIRECTION('center_axis',(1.,0.,0.));
#33949=DIRECTION('ref_axis',(0.,0.,-1.));
#33950=DIRECTION('center_axis',(1.,0.,0.));
#33951=DIRECTION('ref_axis',(0.,0.,-1.));
#33952=DIRECTION('center_axis',(1.,0.,0.));
#33953=DIRECTION('ref_axis',(0.,0.,-1.));
#33954=DIRECTION('center_axis',(1.,0.,0.));
#33955=DIRECTION('ref_axis',(0.,0.,-1.));
#33956=DIRECTION('center_axis',(1.,0.,0.));
#33957=DIRECTION('ref_axis',(0.,0.,-1.));
#33958=DIRECTION('center_axis',(1.,0.,0.));
#33959=DIRECTION('ref_axis',(0.,0.,-1.));
#33960=DIRECTION('center_axis',(1.,0.,0.));
#33961=DIRECTION('ref_axis',(0.,0.,-1.));
#33962=DIRECTION('center_axis',(1.,0.,0.));
#33963=DIRECTION('ref_axis',(0.,0.,-1.));
#33964=DIRECTION('center_axis',(1.,0.,0.));
#33965=DIRECTION('ref_axis',(0.,0.,-1.));
#33966=DIRECTION('center_axis',(1.,0.,0.));
#33967=DIRECTION('ref_axis',(0.,0.,-1.));
#33968=DIRECTION('center_axis',(1.,0.,0.));
#33969=DIRECTION('ref_axis',(0.,0.,-1.));
#33970=DIRECTION('center_axis',(1.,0.,0.));
#33971=DIRECTION('ref_axis',(0.,0.,-1.));
#33972=DIRECTION('center_axis',(1.,0.,0.));
#33973=DIRECTION('ref_axis',(0.,0.,-1.));
#33974=DIRECTION('center_axis',(1.,0.,0.));
#33975=DIRECTION('ref_axis',(0.,0.,-1.));
#33976=DIRECTION('center_axis',(1.,0.,0.));
#33977=DIRECTION('ref_axis',(0.,0.,-1.));
#33978=DIRECTION('center_axis',(1.,0.,0.));
#33979=DIRECTION('ref_axis',(0.,0.,-1.));
#33980=DIRECTION('',(0.707106781186545,-8.65956056235496E-17,-0.70710678118655));
#33981=DIRECTION('center_axis',(-1.,0.,0.));
#33982=DIRECTION('ref_axis',(0.,0.,-1.));
#33983=DIRECTION('center_axis',(0.,-0.0149125533359619,-0.999888801693969));
#33984=DIRECTION('ref_axis',(0.,-0.999888801693969,0.0149125533359619));
#33985=DIRECTION('',(1.,0.,0.));
#33986=DIRECTION('',(0.,-0.999888801693969,0.0149125533359619));
#33987=DIRECTION('',(-1.,0.,0.));
#33988=DIRECTION('center_axis',(0.,-0.654139811408935,0.756373655761412));
#33989=DIRECTION('ref_axis',(0.,0.756373655761412,0.654139811408935));
#33990=DIRECTION('',(-1.,0.,0.));
#33991=DIRECTION('',(0.,0.756373655761412,0.654139811408935));
#33992=DIRECTION('center_axis',(-1.,0.,0.));
#33993=DIRECTION('ref_axis',(0.,-0.342020143325669,0.939692620785908));
#33994=DIRECTION('center_axis',(-1.,0.,0.));
#33995=DIRECTION('ref_axis',(0.,0.,-1.));
#33996=DIRECTION('center_axis',(0.,0.158942870141265,-0.987287781769458));
#33997=DIRECTION('ref_axis',(0.,-0.987287781769458,-0.158942870141265));
#33998=DIRECTION('',(1.,0.,0.));
#33999=DIRECTION('',(0.,-0.987287781769458,-0.158942870141265));
#34000=DIRECTION('',(-1.,0.,0.));
#34001=DIRECTION('center_axis',(0.,-0.775544864787706,0.631292454177475));
#34002=DIRECTION('ref_axis',(0.,0.631292454177475,0.775544864787706));
#34003=DIRECTION('',(-1.,0.,0.));
#34004=DIRECTION('',(0.,0.631292454177475,0.775544864787706));
#34005=DIRECTION('center_axis',(-1.,0.,0.));
#34006=DIRECTION('ref_axis',(0.,-0.5,0.866025403784438));
#34007=DIRECTION('center_axis',(-1.,0.,0.));
#34008=DIRECTION('ref_axis',(0.,0.,-1.));
#34009=DIRECTION('center_axis',(0.,0.327968894938223,-0.944688522187605));
#34010=DIRECTION('ref_axis',(0.,-0.944688522187605,-0.327968894938223));
#34011=DIRECTION('',(1.,0.,0.));
#34012=DIRECTION('',(0.,-0.944688522187605,-0.327968894938223));
#34013=DIRECTION('',(-1.,0.,0.));
#34014=DIRECTION('center_axis',(0.,-0.87338537989454,0.48702975082275));
#34015=DIRECTION('ref_axis',(0.,0.48702975082275,0.87338537989454));
#34016=DIRECTION('',(-1.,0.,0.));
#34017=DIRECTION('',(0.,0.48702975082275,0.87338537989454));
#34018=DIRECTION('center_axis',(-1.,0.,0.));
#34019=DIRECTION('ref_axis',(0.,-0.64278760968654,0.766044443118978));
#34020=DIRECTION('center_axis',(-1.,0.,0.));
#34021=DIRECTION('ref_axis',(0.,0.,-1.));
#34022=DIRECTION('center_axis',(0.,0.487029750822751,-0.87338537989454));
#34023=DIRECTION('ref_axis',(0.,-0.87338537989454,-0.487029750822751));
#34024=DIRECTION('',(1.,0.,0.));
#34025=DIRECTION('',(0.,-0.87338537989454,-0.487029750822751));
#34026=DIRECTION('',(-1.,0.,0.));
#34027=DIRECTION('center_axis',(0.,-0.944688522187605,0.327968894938222));
#34028=DIRECTION('ref_axis',(0.,0.327968894938222,0.944688522187605));
#34029=DIRECTION('',(-1.,0.,0.));
#34030=DIRECTION('',(0.,0.327968894938222,0.944688522187605));
#34031=DIRECTION('center_axis',(-1.,0.,0.));
#34032=DIRECTION('ref_axis',(0.,-0.766044443118978,0.642787609686539));
#34033=DIRECTION('center_axis',(-1.,0.,0.));
#34034=DIRECTION('ref_axis',(0.,0.,-1.));
#34035=DIRECTION('center_axis',(0.,0.631292454177475,-0.775544864787706));
#34036=DIRECTION('ref_axis',(0.,-0.775544864787706,-0.631292454177475));
#34037=DIRECTION('',(1.,0.,0.));
#34038=DIRECTION('',(0.,-0.775544864787705,-0.631292454177475));
#34039=DIRECTION('',(-1.,0.,0.));
#34040=DIRECTION('center_axis',(0.,-0.987287781769458,0.158942870141265));
#34041=DIRECTION('ref_axis',(0.,0.158942870141265,0.987287781769458));
#34042=DIRECTION('',(-1.,0.,0.));
#34043=DIRECTION('',(0.,0.158942870141265,0.987287781769458));
#34044=DIRECTION('center_axis',(-1.,0.,0.));
#34045=DIRECTION('ref_axis',(0.,-0.866025403784439,0.5));
#34046=DIRECTION('center_axis',(-1.,0.,0.));
#34047=DIRECTION('ref_axis',(0.,0.,-1.));
#34048=DIRECTION('center_axis',(0.,0.756373655761413,-0.654139811408934));
#34049=DIRECTION('ref_axis',(0.,-0.654139811408934,-0.756373655761413));
#34050=DIRECTION('',(1.,0.,0.));
#34051=DIRECTION('',(0.,-0.654139811408934,-0.756373655761413));
#34052=DIRECTION('',(-1.,0.,0.));
#34053=DIRECTION('center_axis',(0.,-0.999888801693969,-0.0149125533359631));
#34054=DIRECTION('ref_axis',(0.,-0.0149125533359631,0.999888801693969));
#34055=DIRECTION('',(-1.,0.,0.));
#34056=DIRECTION('',(0.,-0.0149125533359631,0.999888801693969));
#34057=DIRECTION('center_axis',(-1.,0.,0.));
#34058=DIRECTION('ref_axis',(0.,-0.939692620785909,0.342020143325668));
#34059=DIRECTION('center_axis',(-1.,0.,0.));
#34060=DIRECTION('ref_axis',(0.,0.,-1.));
#34061=DIRECTION('center_axis',(0.,0.858472826558577,-0.512859050871218));
#34062=DIRECTION('ref_axis',(0.,-0.512859050871218,-0.858472826558577));
#34063=DIRECTION('',(1.,0.,0.));
#34064=DIRECTION('',(0.,-0.512859050871218,-0.858472826558577));
#34065=DIRECTION('',(-1.,0.,0.));
#34066=DIRECTION('center_axis',(0.,-0.982108706347157,-0.188314866426193));
#34067=DIRECTION('ref_axis',(0.,-0.188314866426193,0.982108706347157));
#34068=DIRECTION('',(-1.,0.,0.));
#34069=DIRECTION('',(0.,-0.188314866426193,0.982108706347156));
#34070=DIRECTION('center_axis',(-1.,0.,0.));
#34071=DIRECTION('ref_axis',(0.,-0.984807753012208,0.17364817766693));
#34072=DIRECTION('center_axis',(-1.,0.,0.));
#34073=DIRECTION('ref_axis',(0.,0.,-1.));
#34074=DIRECTION('center_axis',(0.,0.93448773492897,-0.355995327591983));
#34075=DIRECTION('ref_axis',(0.,-0.355995327591983,-0.93448773492897));
#34076=DIRECTION('',(1.,0.,0.));
#34077=DIRECTION('',(0.,-0.355995327591983,-0.93448773492897));
#34078=DIRECTION('',(-1.,0.,0.));
#34079=DIRECTION('center_axis',(0.,-0.93448773492897,-0.355995327591983));
#34080=DIRECTION('ref_axis',(0.,-0.355995327591983,0.93448773492897));
#34081=DIRECTION('',(-1.,0.,0.));
#34082=DIRECTION('',(0.,-0.355995327591983,0.93448773492897));
#34083=DIRECTION('center_axis',(-1.,0.,0.));
#34084=DIRECTION('ref_axis',(0.,-1.,-1.83697019872103E-16));
#34085=DIRECTION('center_axis',(-1.,0.,0.));
#34086=DIRECTION('ref_axis',(0.,0.,-1.));
#34087=DIRECTION('center_axis',(-1.,0.,0.));
#34088=DIRECTION('ref_axis',(0.,0.,-1.));
#34089=DIRECTION('center_axis',(0.,0.982108706347157,-0.188314866426193));
#34090=DIRECTION('ref_axis',(0.,-0.188314866426193,-0.982108706347156));
#34091=DIRECTION('',(1.,0.,0.));
#34092=DIRECTION('',(0.,-0.188314866426193,-0.982108706347156));
#34093=DIRECTION('',(-1.,0.,0.));
#34094=DIRECTION('center_axis',(0.,-0.858472826558577,-0.512859050871219));
#34095=DIRECTION('ref_axis',(0.,-0.512859050871219,0.858472826558577));
#34096=DIRECTION('',(-1.,0.,0.));
#34097=DIRECTION('',(0.,-0.512859050871219,0.858472826558577));
#34098=DIRECTION('center_axis',(-1.,0.,0.));
#34099=DIRECTION('ref_axis',(0.,-0.984807753012208,-0.17364817766693));
#34100=DIRECTION('center_axis',(-1.,0.,0.));
#34101=DIRECTION('ref_axis',(0.,0.,-1.));
#34102=DIRECTION('center_axis',(0.,0.99988880169397,-0.014912553335962));
#34103=DIRECTION('ref_axis',(0.,-0.014912553335962,-0.99988880169397));
#34104=DIRECTION('',(1.,0.,0.));
#34105=DIRECTION('',(0.,-0.014912553335962,-0.999888801693969));
#34106=DIRECTION('',(-1.,0.,0.));
#34107=DIRECTION('center_axis',(0.,-0.756373655761412,-0.654139811408935));
#34108=DIRECTION('ref_axis',(0.,-0.654139811408935,0.756373655761412));
#34109=DIRECTION('',(-1.,0.,0.));
#34110=DIRECTION('',(0.,-0.654139811408935,0.756373655761412));
#34111=DIRECTION('center_axis',(-1.,0.,0.));
#34112=DIRECTION('ref_axis',(0.,-0.939692620785908,-0.342020143325669));
#34113=DIRECTION('center_axis',(-1.,0.,0.));
#34114=DIRECTION('ref_axis',(0.,0.,-1.));
#34115=DIRECTION('center_axis',(0.,0.987287781769458,0.158942870141265));
#34116=DIRECTION('ref_axis',(0.,0.158942870141265,-0.987287781769458));
#34117=DIRECTION('',(1.,0.,0.));
#34118=DIRECTION('',(0.,0.158942870141265,-0.987287781769458));
#34119=DIRECTION('',(-1.,0.,0.));
#34120=DIRECTION('center_axis',(0.,-0.631292454177475,-0.775544864787706));
#34121=DIRECTION('ref_axis',(0.,-0.775544864787706,0.631292454177475));
#34122=DIRECTION('',(-1.,0.,0.));
#34123=DIRECTION('',(0.,-0.775544864787706,0.631292454177475));
#34124=DIRECTION('center_axis',(-1.,0.,0.));
#34125=DIRECTION('ref_axis',(0.,-0.866025403784438,-0.5));
#34126=DIRECTION('center_axis',(-1.,0.,0.));
#34127=DIRECTION('ref_axis',(0.,0.,-1.));
#34128=DIRECTION('center_axis',(0.,0.944688522187605,0.327968894938222));
#34129=DIRECTION('ref_axis',(0.,0.327968894938222,-0.944688522187605));
#34130=DIRECTION('',(1.,0.,0.));
#34131=DIRECTION('',(0.,0.327968894938222,-0.944688522187605));
#34132=DIRECTION('',(-1.,0.,0.));
#34133=DIRECTION('center_axis',(0.,-0.487029750822751,-0.87338537989454));
#34134=DIRECTION('ref_axis',(0.,-0.87338537989454,0.487029750822751));
#34135=DIRECTION('',(-1.,0.,0.));
#34136=DIRECTION('',(0.,-0.87338537989454,0.487029750822751));
#34137=DIRECTION('center_axis',(-1.,0.,0.));
#34138=DIRECTION('ref_axis',(0.,-0.766044443118978,-0.642787609686539));
#34139=DIRECTION('center_axis',(-1.,0.,0.));
#34140=DIRECTION('ref_axis',(0.,0.,-1.));
#34141=DIRECTION('center_axis',(0.,0.87338537989454,0.487029750822751));
#34142=DIRECTION('ref_axis',(0.,0.487029750822751,-0.87338537989454));
#34143=DIRECTION('',(1.,0.,0.));
#34144=DIRECTION('',(0.,0.487029750822751,-0.87338537989454));
#34145=DIRECTION('',(-1.,0.,0.));
#34146=DIRECTION('center_axis',(0.,-0.327968894938222,-0.944688522187605));
#34147=DIRECTION('ref_axis',(0.,-0.944688522187605,0.327968894938222));
#34148=DIRECTION('',(-1.,0.,0.));
#34149=DIRECTION('',(0.,-0.944688522187605,0.327968894938222));
#34150=DIRECTION('center_axis',(-1.,0.,0.));
#34151=DIRECTION('ref_axis',(0.,-0.642787609686539,-0.766044443118978));
#34152=DIRECTION('center_axis',(-1.,0.,0.));
#34153=DIRECTION('ref_axis',(0.,0.,-1.));
#34154=DIRECTION('center_axis',(0.,0.775544864787705,0.631292454177475));
#34155=DIRECTION('ref_axis',(0.,0.631292454177475,-0.775544864787705));
#34156=DIRECTION('',(1.,0.,0.));
#34157=DIRECTION('',(0.,0.631292454177475,-0.775544864787705));
#34158=DIRECTION('',(-1.,0.,0.));
#34159=DIRECTION('center_axis',(0.,-0.158942870141264,-0.987287781769458));
#34160=DIRECTION('ref_axis',(0.,-0.987287781769458,0.158942870141264));
#34161=DIRECTION('',(-1.,0.,0.));
#34162=DIRECTION('',(0.,-0.987287781769458,0.158942870141264));
#34163=DIRECTION('center_axis',(-1.,0.,0.));
#34164=DIRECTION('ref_axis',(0.,-0.5,-0.866025403784439));
#34165=DIRECTION('center_axis',(-1.,0.,0.));
#34166=DIRECTION('ref_axis',(0.,0.,-1.));
#34167=DIRECTION('center_axis',(0.,0.654139811408934,0.756373655761413));
#34168=DIRECTION('ref_axis',(0.,0.756373655761413,-0.654139811408934));
#34169=DIRECTION('',(1.,0.,0.));
#34170=DIRECTION('',(0.,0.756373655761413,-0.654139811408934));
#34171=DIRECTION('',(-1.,0.,0.));
#34172=DIRECTION('center_axis',(0.,0.0149125533359627,-0.99988880169397));
#34173=DIRECTION('ref_axis',(0.,-0.99988880169397,-0.0149125533359627));
#34174=DIRECTION('',(-1.,0.,0.));
#34175=DIRECTION('',(0.,-0.999888801693969,-0.0149125533359627));
#34176=DIRECTION('center_axis',(-1.,0.,0.));
#34177=DIRECTION('ref_axis',(0.,-0.342020143325669,-0.939692620785908));
#34178=DIRECTION('center_axis',(-1.,0.,0.));
#34179=DIRECTION('ref_axis',(0.,0.,-1.));
#34180=DIRECTION('center_axis',(0.,0.512859050871218,0.858472826558577));
#34181=DIRECTION('ref_axis',(0.,0.858472826558577,-0.512859050871218));
#34182=DIRECTION('',(1.,0.,0.));
#34183=DIRECTION('',(0.,0.858472826558577,-0.512859050871218));
#34184=DIRECTION('',(-1.,0.,0.));
#34185=DIRECTION('center_axis',(0.,0.188314866426193,-0.982108706347157));
#34186=DIRECTION('ref_axis',(0.,-0.982108706347157,-0.188314866426193));
#34187=DIRECTION('',(-1.,0.,0.));
#34188=DIRECTION('',(0.,-0.982108706347156,-0.188314866426193));
#34189=DIRECTION('center_axis',(-1.,0.,0.));
#34190=DIRECTION('ref_axis',(0.,-0.17364817766693,-0.984807753012208));
#34191=DIRECTION('center_axis',(-1.,0.,0.));
#34192=DIRECTION('ref_axis',(0.,0.,-1.));
#34193=DIRECTION('center_axis',(0.,0.355995327591983,0.93448773492897));
#34194=DIRECTION('ref_axis',(0.,0.93448773492897,-0.355995327591983));
#34195=DIRECTION('',(1.,0.,0.));
#34196=DIRECTION('',(0.,0.93448773492897,-0.355995327591983));
#34197=DIRECTION('',(-1.,0.,0.));
#34198=DIRECTION('center_axis',(0.,0.355995327591983,-0.93448773492897));
#34199=DIRECTION('ref_axis',(0.,-0.93448773492897,-0.355995327591983));
#34200=DIRECTION('',(-1.,0.,0.));
#34201=DIRECTION('',(0.,-0.93448773492897,-0.355995327591983));
#34202=DIRECTION('center_axis',(-1.,0.,0.));
#34203=DIRECTION('ref_axis',(0.,1.22464679914735E-16,-1.));
#34204=DIRECTION('center_axis',(-1.,0.,0.));
#34205=DIRECTION('ref_axis',(0.,0.,-1.));
#34206=DIRECTION('center_axis',(0.,0.188314866426192,0.982108706347157));
#34207=DIRECTION('ref_axis',(0.,0.982108706347157,-0.188314866426192));
#34208=DIRECTION('',(1.,0.,0.));
#34209=DIRECTION('',(0.,0.982108706347157,-0.188314866426192));
#34210=DIRECTION('',(-1.,0.,0.));
#34211=DIRECTION('center_axis',(0.,0.512859050871219,-0.858472826558577));
#34212=DIRECTION('ref_axis',(0.,-0.858472826558577,-0.512859050871219));
#34213=DIRECTION('',(-1.,0.,0.));
#34214=DIRECTION('',(0.,-0.858472826558577,-0.512859050871219));
#34215=DIRECTION('center_axis',(-1.,0.,0.));
#34216=DIRECTION('ref_axis',(0.,0.173648177666931,-0.984807753012208));
#34217=DIRECTION('center_axis',(-1.,0.,0.));
#34218=DIRECTION('ref_axis',(0.,0.,-1.));
#34219=DIRECTION('center_axis',(0.,0.0149125533359624,0.99988880169397));
#34220=DIRECTION('ref_axis',(0.,0.99988880169397,-0.0149125533359624));
#34221=DIRECTION('',(1.,0.,0.));
#34222=DIRECTION('',(0.,0.999888801693969,-0.0149125533359624));
#34223=DIRECTION('',(-1.,0.,0.));
#34224=DIRECTION('center_axis',(0.,0.654139811408934,-0.756373655761413));
#34225=DIRECTION('ref_axis',(0.,-0.756373655761413,-0.654139811408935));
#34226=DIRECTION('',(-1.,0.,0.));
#34227=DIRECTION('',(0.,-0.756373655761413,-0.654139811408934));
#34228=DIRECTION('center_axis',(-1.,0.,0.));
#34229=DIRECTION('ref_axis',(0.,0.342020143325669,-0.939692620785908));
#34230=DIRECTION('center_axis',(-1.,0.,0.));
#34231=DIRECTION('ref_axis',(0.,0.,-1.));
#34232=DIRECTION('center_axis',(0.,-0.158942870141264,0.987287781769458));
#34233=DIRECTION('ref_axis',(0.,0.987287781769458,0.158942870141264));
#34234=DIRECTION('',(1.,0.,0.));
#34235=DIRECTION('',(0.,0.987287781769458,0.158942870141264));
#34236=DIRECTION('',(-1.,0.,0.));
#34237=DIRECTION('center_axis',(0.,0.775544864787705,-0.631292454177475));
#34238=DIRECTION('ref_axis',(0.,-0.631292454177475,-0.775544864787705));
#34239=DIRECTION('',(-1.,0.,0.));
#34240=DIRECTION('',(0.,-0.631292454177475,-0.775544864787705));
#34241=DIRECTION('center_axis',(-1.,0.,0.));
#34242=DIRECTION('ref_axis',(0.,0.5,-0.866025403784439));
#34243=DIRECTION('center_axis',(-1.,0.,0.));
#34244=DIRECTION('ref_axis',(0.,0.,-1.));
#34245=DIRECTION('center_axis',(0.,-0.327968894938222,0.944688522187605));
#34246=DIRECTION('ref_axis',(0.,0.944688522187605,0.327968894938222));
#34247=DIRECTION('',(1.,0.,0.));
#34248=DIRECTION('',(0.,0.944688522187605,0.327968894938222));
#34249=DIRECTION('',(-1.,0.,0.));
#34250=DIRECTION('center_axis',(0.,0.87338537989454,-0.487029750822751));
#34251=DIRECTION('ref_axis',(0.,-0.487029750822751,-0.87338537989454));
#34252=DIRECTION('',(-1.,0.,0.));
#34253=DIRECTION('',(0.,-0.487029750822751,-0.87338537989454));
#34254=DIRECTION('center_axis',(-1.,0.,0.));
#34255=DIRECTION('ref_axis',(0.,0.642787609686539,-0.766044443118978));
#34256=DIRECTION('center_axis',(-1.,0.,0.));
#34257=DIRECTION('ref_axis',(0.,0.,-1.));
#34258=DIRECTION('center_axis',(0.,-0.487029750822751,0.87338537989454));
#34259=DIRECTION('ref_axis',(0.,0.87338537989454,0.487029750822751));
#34260=DIRECTION('',(1.,0.,0.));
#34261=DIRECTION('',(0.,0.87338537989454,0.487029750822751));
#34262=DIRECTION('',(-1.,0.,0.));
#34263=DIRECTION('center_axis',(0.,0.944688522187605,-0.327968894938222));
#34264=DIRECTION('ref_axis',(0.,-0.327968894938222,-0.944688522187605));
#34265=DIRECTION('',(-1.,0.,0.));
#34266=DIRECTION('',(0.,-0.327968894938222,-0.944688522187605));
#34267=DIRECTION('center_axis',(-1.,0.,0.));
#34268=DIRECTION('ref_axis',(0.,0.766044443118978,-0.642787609686539));
#34269=DIRECTION('center_axis',(-1.,0.,0.));
#34270=DIRECTION('ref_axis',(0.,0.,-1.));
#34271=DIRECTION('center_axis',(0.,-0.631292454177475,0.775544864787705));
#34272=DIRECTION('ref_axis',(0.,0.775544864787705,0.631292454177475));
#34273=DIRECTION('',(1.,0.,0.));
#34274=DIRECTION('',(0.,0.775544864787705,0.631292454177475));
#34275=DIRECTION('',(-1.,0.,0.));
#34276=DIRECTION('center_axis',(0.,0.987287781769458,-0.158942870141264));
#34277=DIRECTION('ref_axis',(0.,-0.158942870141264,-0.987287781769458));
#34278=DIRECTION('',(-1.,0.,0.));
#34279=DIRECTION('',(0.,-0.158942870141264,-0.987287781769458));
#34280=DIRECTION('center_axis',(-1.,0.,0.));
#34281=DIRECTION('ref_axis',(0.,0.866025403784439,-0.5));
#34282=DIRECTION('center_axis',(-1.,0.,0.));
#34283=DIRECTION('ref_axis',(0.,0.,-1.));
#34284=DIRECTION('center_axis',(0.,-0.756373655761413,0.654139811408934));
#34285=DIRECTION('ref_axis',(0.,0.654139811408934,0.756373655761413));
#34286=DIRECTION('',(1.,0.,0.));
#34287=DIRECTION('',(0.,0.654139811408934,0.756373655761413));
#34288=DIRECTION('',(-1.,0.,0.));
#34289=DIRECTION('center_axis',(0.,0.99988880169397,0.0149125533359626));
#34290=DIRECTION('ref_axis',(0.,0.0149125533359626,-0.99988880169397));
#34291=DIRECTION('',(-1.,0.,0.));
#34292=DIRECTION('',(0.,0.0149125533359626,-0.999888801693969));
#34293=DIRECTION('center_axis',(-1.,0.,0.));
#34294=DIRECTION('ref_axis',(0.,0.939692620785908,-0.342020143325669));
#34295=DIRECTION('center_axis',(-1.,0.,0.));
#34296=DIRECTION('ref_axis',(0.,0.,-1.));
#34297=DIRECTION('center_axis',(0.,-0.858472826558577,0.512859050871219));
#34298=DIRECTION('ref_axis',(0.,0.512859050871219,0.858472826558577));
#34299=DIRECTION('',(1.,0.,0.));
#34300=DIRECTION('',(0.,0.512859050871219,0.858472826558577));
#34301=DIRECTION('',(-1.,0.,0.));
#34302=DIRECTION('center_axis',(0.,0.982108706347157,0.188314866426193));
#34303=DIRECTION('ref_axis',(0.,0.188314866426193,-0.982108706347156));
#34304=DIRECTION('',(-1.,0.,0.));
#34305=DIRECTION('',(0.,0.188314866426193,-0.982108706347156));
#34306=DIRECTION('center_axis',(-1.,0.,0.));
#34307=DIRECTION('ref_axis',(0.,0.984807753012208,-0.17364817766693));
#34308=DIRECTION('center_axis',(-1.,0.,0.));
#34309=DIRECTION('ref_axis',(0.,0.,-1.));
#34310=DIRECTION('center_axis',(0.,-0.93448773492897,0.355995327591983));
#34311=DIRECTION('ref_axis',(0.,0.355995327591983,0.93448773492897));
#34312=DIRECTION('',(1.,0.,0.));
#34313=DIRECTION('',(0.,0.355995327591983,0.93448773492897));
#34314=DIRECTION('',(-1.,0.,0.));
#34315=DIRECTION('center_axis',(0.,0.93448773492897,0.355995327591983));
#34316=DIRECTION('ref_axis',(0.,0.355995327591983,-0.93448773492897));
#34317=DIRECTION('',(-1.,0.,0.));
#34318=DIRECTION('',(0.,0.355995327591983,-0.93448773492897));
#34319=DIRECTION('center_axis',(-1.,0.,0.));
#34320=DIRECTION('ref_axis',(0.,1.,6.12323399573677E-17));
#34321=DIRECTION('center_axis',(-1.,0.,0.));
#34322=DIRECTION('ref_axis',(0.,0.,-1.));
#34323=DIRECTION('center_axis',(0.,-0.982108706347157,0.188314866426192));
#34324=DIRECTION('ref_axis',(0.,0.188314866426192,0.982108706347157));
#34325=DIRECTION('',(1.,0.,0.));
#34326=DIRECTION('',(0.,0.188314866426192,0.982108706347157));
#34327=DIRECTION('',(-1.,0.,0.));
#34328=DIRECTION('center_axis',(0.,0.858472826558577,0.512859050871219));
#34329=DIRECTION('ref_axis',(0.,0.512859050871219,-0.858472826558577));
#34330=DIRECTION('',(-1.,0.,0.));
#34331=DIRECTION('',(0.,0.512859050871219,-0.858472826558577));
#34332=DIRECTION('center_axis',(-1.,0.,0.));
#34333=DIRECTION('ref_axis',(0.,0.984807753012208,0.17364817766693));
#34334=DIRECTION('center_axis',(-1.,0.,0.));
#34335=DIRECTION('ref_axis',(0.,0.,-1.));
#34336=DIRECTION('center_axis',(0.,-0.99988880169397,0.0149125533359625));
#34337=DIRECTION('ref_axis',(0.,0.0149125533359625,0.99988880169397));
#34338=DIRECTION('',(1.,0.,0.));
#34339=DIRECTION('',(0.,0.0149125533359625,0.99988880169397));
#34340=DIRECTION('',(-1.,0.,0.));
#34341=DIRECTION('center_axis',(0.,0.756373655761413,0.654139811408934));
#34342=DIRECTION('ref_axis',(0.,0.654139811408935,-0.756373655761413));
#34343=DIRECTION('',(-1.,0.,0.));
#34344=DIRECTION('',(0.,0.654139811408934,-0.756373655761413));
#34345=DIRECTION('center_axis',(-1.,0.,0.));
#34346=DIRECTION('ref_axis',(0.,0.939692620785908,0.342020143325669));
#34347=DIRECTION('center_axis',(-1.,0.,0.));
#34348=DIRECTION('ref_axis',(0.,0.,-1.));
#34349=DIRECTION('center_axis',(0.,-0.987287781769458,-0.158942870141265));
#34350=DIRECTION('ref_axis',(0.,-0.158942870141265,0.987287781769458));
#34351=DIRECTION('',(1.,0.,0.));
#34352=DIRECTION('',(0.,-0.158942870141265,0.987287781769458));
#34353=DIRECTION('',(-1.,0.,0.));
#34354=DIRECTION('center_axis',(0.,0.631292454177475,0.775544864787706));
#34355=DIRECTION('ref_axis',(0.,0.775544864787706,-0.631292454177475));
#34356=DIRECTION('',(-1.,0.,0.));
#34357=DIRECTION('',(0.,0.775544864787705,-0.631292454177475));
#34358=DIRECTION('center_axis',(-1.,0.,0.));
#34359=DIRECTION('ref_axis',(0.,0.866025403784439,0.5));
#34360=DIRECTION('center_axis',(-1.,0.,0.));
#34361=DIRECTION('ref_axis',(0.,0.,-1.));
#34362=DIRECTION('center_axis',(0.,-0.944688522187605,-0.327968894938222));
#34363=DIRECTION('ref_axis',(0.,-0.327968894938222,0.944688522187605));
#34364=DIRECTION('',(1.,0.,0.));
#34365=DIRECTION('',(0.,-0.327968894938222,0.944688522187605));
#34366=DIRECTION('',(-1.,0.,0.));
#34367=DIRECTION('center_axis',(0.,0.487029750822751,0.87338537989454));
#34368=DIRECTION('ref_axis',(0.,0.87338537989454,-0.487029750822751));
#34369=DIRECTION('',(-1.,0.,0.));
#34370=DIRECTION('',(0.,0.87338537989454,-0.487029750822751));
#34371=DIRECTION('center_axis',(-1.,0.,0.));
#34372=DIRECTION('ref_axis',(0.,0.766044443118978,0.642787609686539));
#34373=DIRECTION('center_axis',(-1.,0.,0.));
#34374=DIRECTION('ref_axis',(0.,0.,-1.));
#34375=DIRECTION('center_axis',(0.,-0.87338537989454,-0.487029750822751));
#34376=DIRECTION('ref_axis',(0.,-0.487029750822751,0.87338537989454));
#34377=DIRECTION('',(1.,0.,0.));
#34378=DIRECTION('',(0.,-0.487029750822751,0.87338537989454));
#34379=DIRECTION('',(-1.,0.,0.));
#34380=DIRECTION('center_axis',(0.,0.327968894938222,0.944688522187605));
#34381=DIRECTION('ref_axis',(0.,0.944688522187605,-0.327968894938222));
#34382=DIRECTION('',(-1.,0.,0.));
#34383=DIRECTION('',(0.,0.944688522187605,-0.327968894938222));
#34384=DIRECTION('center_axis',(-1.,0.,0.));
#34385=DIRECTION('ref_axis',(0.,0.642787609686539,0.766044443118978));
#34386=DIRECTION('center_axis',(-1.,0.,0.));
#34387=DIRECTION('ref_axis',(0.,0.,-1.));
#34388=DIRECTION('center_axis',(0.,-0.775544864787705,-0.631292454177475));
#34389=DIRECTION('ref_axis',(0.,-0.631292454177475,0.775544864787705));
#34390=DIRECTION('',(1.,0.,0.));
#34391=DIRECTION('',(0.,-0.631292454177475,0.775544864787705));
#34392=DIRECTION('',(-1.,0.,0.));
#34393=DIRECTION('center_axis',(0.,0.158942870141264,0.987287781769458));
#34394=DIRECTION('ref_axis',(0.,0.987287781769458,-0.158942870141264));
#34395=DIRECTION('',(-1.,0.,0.));
#34396=DIRECTION('',(0.,0.987287781769458,-0.158942870141264));
#34397=DIRECTION('center_axis',(-1.,0.,0.));
#34398=DIRECTION('ref_axis',(0.,0.5,0.866025403784439));
#34399=DIRECTION('center_axis',(-1.,0.,0.));
#34400=DIRECTION('ref_axis',(0.,0.,-1.));
#34401=DIRECTION('center_axis',(0.,-0.654139811408934,-0.756373655761413));
#34402=DIRECTION('ref_axis',(0.,-0.756373655761413,0.654139811408934));
#34403=DIRECTION('',(1.,0.,0.));
#34404=DIRECTION('',(0.,-0.756373655761413,0.654139811408934));
#34405=DIRECTION('',(-1.,0.,0.));
#34406=DIRECTION('center_axis',(0.,-0.0149125533359626,0.99988880169397));
#34407=DIRECTION('ref_axis',(0.,0.99988880169397,0.0149125533359626));
#34408=DIRECTION('',(-1.,0.,0.));
#34409=DIRECTION('',(0.,0.999888801693969,0.0149125533359626));
#34410=DIRECTION('center_axis',(-1.,0.,0.));
#34411=DIRECTION('ref_axis',(0.,0.342020143325669,0.939692620785908));
#34412=DIRECTION('center_axis',(-1.,0.,0.));
#34413=DIRECTION('ref_axis',(0.,0.,-1.));
#34414=DIRECTION('center_axis',(0.,-0.512859050871219,-0.858472826558577));
#34415=DIRECTION('ref_axis',(0.,-0.858472826558577,0.512859050871219));
#34416=DIRECTION('',(1.,0.,0.));
#34417=DIRECTION('',(0.,-0.858472826558577,0.512859050871219));
#34418=DIRECTION('',(-1.,0.,0.));
#34419=DIRECTION('center_axis',(0.,-0.188314866426193,0.982108706347157));
#34420=DIRECTION('ref_axis',(0.,0.982108706347156,0.188314866426193));
#34421=DIRECTION('',(-1.,0.,0.));
#34422=DIRECTION('',(0.,0.982108706347156,0.188314866426193));
#34423=DIRECTION('center_axis',(-1.,0.,0.));
#34424=DIRECTION('ref_axis',(0.,0.17364817766693,0.984807753012208));
#34425=DIRECTION('center_axis',(-1.,0.,0.));
#34426=DIRECTION('ref_axis',(0.,0.,-1.));
#34427=DIRECTION('center_axis',(0.,-0.355995327591983,-0.93448773492897));
#34428=DIRECTION('ref_axis',(0.,-0.93448773492897,0.355995327591983));
#34429=DIRECTION('',(1.,0.,0.));
#34430=DIRECTION('',(0.,-0.93448773492897,0.355995327591983));
#34431=DIRECTION('',(-1.,0.,0.));
#34432=DIRECTION('center_axis',(0.,-0.355995327591983,0.93448773492897));
#34433=DIRECTION('ref_axis',(0.,0.93448773492897,0.355995327591983));
#34434=DIRECTION('',(-1.,0.,0.));
#34435=DIRECTION('',(0.,0.93448773492897,0.355995327591983));
#34436=DIRECTION('center_axis',(-1.,0.,0.));
#34437=DIRECTION('ref_axis',(0.,0.,1.));
#34438=DIRECTION('center_axis',(-1.,0.,0.));
#34439=DIRECTION('ref_axis',(0.,0.,-1.));
#34440=DIRECTION('center_axis',(1.,0.,0.));
#34441=DIRECTION('ref_axis',(0.,0.,-1.));
#34442=DIRECTION('',(-1.,0.,0.));
#34443=DIRECTION('center_axis',(1.,0.,0.));
#34444=DIRECTION('ref_axis',(0.,0.,-1.));
#34445=DIRECTION('',(0.,0.499999999999998,-0.86602540378444));
#34446=DIRECTION('',(0.,-0.499999999999999,-0.866025403784439));
#34447=DIRECTION('',(0.,-1.,0.));
#34448=DIRECTION('',(0.,-0.500000000000003,0.866025403784437));
#34449=DIRECTION('',(0.,0.500000000000002,0.866025403784437));
#34450=DIRECTION('',(0.,1.,0.));
#34451=DIRECTION('center_axis',(1.,0.,0.));
#34452=DIRECTION('ref_axis',(0.,0.,-1.));
#34453=DIRECTION('',(0.,0.499999999999998,-0.86602540378444));
#34454=DIRECTION('center_axis',(1.,0.,0.));
#34455=DIRECTION('ref_axis',(0.,0.,-1.));
#34456=DIRECTION('center_axis',(1.,0.,0.));
#34457=DIRECTION('ref_axis',(0.,0.,-1.));
#34458=DIRECTION('',(0.,-0.499999999999999,-0.866025403784439));
#34459=DIRECTION('center_axis',(1.,0.,0.));
#34460=DIRECTION('ref_axis',(0.,0.,-1.));
#34461=DIRECTION('center_axis',(1.,0.,0.));
#34462=DIRECTION('ref_axis',(0.,0.,-1.));
#34463=DIRECTION('',(0.,-1.,0.));
#34464=DIRECTION('center_axis',(1.,0.,0.));
#34465=DIRECTION('ref_axis',(0.,0.,-1.));
#34466=DIRECTION('center_axis',(1.,0.,0.));
#34467=DIRECTION('ref_axis',(0.,0.,-1.));
#34468=DIRECTION('',(0.,-0.500000000000003,0.866025403784437));
#34469=DIRECTION('center_axis',(1.,0.,0.));
#34470=DIRECTION('ref_axis',(0.,0.,-1.));
#34471=DIRECTION('center_axis',(1.,0.,0.));
#34472=DIRECTION('ref_axis',(0.,0.,-1.));
#34473=DIRECTION('',(0.,0.500000000000002,0.866025403784437));
#34474=DIRECTION('center_axis',(1.,0.,0.));
#34475=DIRECTION('ref_axis',(0.,0.,-1.));
#34476=DIRECTION('center_axis',(1.,0.,0.));
#34477=DIRECTION('ref_axis',(0.,0.,-1.));
#34478=DIRECTION('',(0.,1.,0.));
#34479=DIRECTION('center_axis',(1.,0.,0.));
#34480=DIRECTION('ref_axis',(0.,0.,-1.));
#34481=DIRECTION('center_axis',(1.,0.,0.));
#34482=DIRECTION('ref_axis',(0.,1.,0.));
#34483=DIRECTION('',(0.515038074910058,-0.85716730070211,-1.04972719113862E-16));
#34484=DIRECTION('center_axis',(0.,0.86602540378444,0.499999999999998));
#34485=DIRECTION('ref_axis',(0.,0.499999999999998,-0.86602540378444));
#34486=DIRECTION('',(-1.,0.,0.));
#34487=DIRECTION('',(-1.,0.,0.));
#34488=DIRECTION('center_axis',(0.,0.,1.));
#34489=DIRECTION('ref_axis',(0.,1.,0.));
#34490=DIRECTION('',(-1.,0.,0.));
#34491=DIRECTION('center_axis',(0.,-0.866025403784437,0.500000000000002));
#34492=DIRECTION('ref_axis',(0.,0.500000000000002,0.866025403784437));
#34493=DIRECTION('',(-1.,0.,0.));
#34494=DIRECTION('center_axis',(0.,-0.866025403784437,-0.500000000000003));
#34495=DIRECTION('ref_axis',(0.,-0.500000000000003,0.866025403784437));
#34496=DIRECTION('',(-1.,0.,0.));
#34497=DIRECTION('center_axis',(0.,0.,-1.));
#34498=DIRECTION('ref_axis',(0.,-1.,0.));
#34499=DIRECTION('',(-1.,0.,0.));
#34500=DIRECTION('center_axis',(0.,0.866025403784439,-0.499999999999999));
#34501=DIRECTION('ref_axis',(0.,-0.499999999999999,-0.866025403784439));
#34502=DIRECTION('axis',(0.,0.,1.));
#34503=DIRECTION('refdir',(1.,0.,0.));
#34504=DIRECTION('center_axis',(0.,-1.,0.));
#34505=DIRECTION('ref_axis',(0.653826602794498,0.,-0.756644416802375));
#34506=DIRECTION('',(0.,1.,0.));
#34507=DIRECTION('center_axis',(0.,1.,0.));
#34508=DIRECTION('ref_axis',(1.,0.,6.03192037001069E-14));
#34509=DIRECTION('center_axis',(0.,-1.,0.));
#34510=DIRECTION('ref_axis',(0.653826602794498,0.,-0.756644416802375));
#34511=DIRECTION('',(0.,1.,0.));
#34512=DIRECTION('center_axis',(0.,-1.,0.));
#34513=DIRECTION('ref_axis',(0.653826602794498,0.,-0.756644416802375));
#34514=DIRECTION('',(0.,1.,0.));
#34515=DIRECTION('center_axis',(0.,-1.,0.));
#34516=DIRECTION('ref_axis',(0.653826602794498,0.,-0.756644416802375));
#34517=DIRECTION('',(0.,1.,0.));
#34518=DIRECTION('center_axis',(0.,-1.,0.));
#34519=DIRECTION('ref_axis',(0.653826602794498,0.,-0.756644416802375));
#34520=DIRECTION('',(0.,1.,0.));
#34521=DIRECTION('center_axis',(0.,-1.,0.));
#34522=DIRECTION('ref_axis',(0.653826602794498,0.,-0.756644416802375));
#34523=DIRECTION('',(0.,1.,0.));
#34524=DIRECTION('center_axis',(0.,-1.,0.));
#34525=DIRECTION('ref_axis',(0.653826602794498,0.,-0.756644416802375));
#34526=DIRECTION('',(0.,1.,0.));
#34527=DIRECTION('center_axis',(0.,-1.,0.));
#34528=DIRECTION('ref_axis',(0.653826602794498,0.,-0.756644416802375));
#34529=DIRECTION('',(0.,1.,0.));
#34530=DIRECTION('center_axis',(0.,-1.,0.));
#34531=DIRECTION('ref_axis',(0.653826602794498,0.,-0.756644416802375));
#34532=DIRECTION('',(0.,1.,0.));
#34533=DIRECTION('center_axis',(0.,-1.,0.));
#34534=DIRECTION('ref_axis',(1.,0.,0.));
#34535=DIRECTION('center_axis',(0.,1.,0.));
#34536=DIRECTION('ref_axis',(1.,0.,0.));
#34537=DIRECTION('center_axis',(0.,-1.,0.));
#34538=DIRECTION('ref_axis',(1.,0.,0.));
#34539=DIRECTION('center_axis',(0.,-1.,0.));
#34540=DIRECTION('ref_axis',(0.279895837868924,0.,-0.960030374490127));
#34541=DIRECTION('center_axis',(0.,-1.,0.));
#34542=DIRECTION('ref_axis',(1.,0.,6.03192037001069E-14));
#34543=DIRECTION('center_axis',(0.,1.,0.));
#34544=DIRECTION('ref_axis',(0.,0.,1.));
#34545=DIRECTION('center_axis',(0.,-1.,0.));
#34546=DIRECTION('ref_axis',(1.,0.,0.));
#34547=DIRECTION('center_axis',(0.,-1.,0.));
#34548=DIRECTION('ref_axis',(1.,0.,0.));
#34549=DIRECTION('center_axis',(0.,1.,0.));
#34550=DIRECTION('ref_axis',(0.,0.,1.));
#34551=DIRECTION('center_axis',(0.,1.,0.));
#34552=DIRECTION('ref_axis',(1.,0.,0.));
#34553=DIRECTION('center_axis',(0.,1.,0.));
#34554=DIRECTION('ref_axis',(1.,0.,0.));
#34555=DIRECTION('center_axis',(0.,1.,0.));
#34556=DIRECTION('ref_axis',(0.,0.,1.));
#34557=DIRECTION('center_axis',(0.,-1.,0.));
#34558=DIRECTION('ref_axis',(1.,0.,0.));
#34559=DIRECTION('center_axis',(1.,0.,0.));
#34560=DIRECTION('ref_axis',(0.,0.,-1.));
#34561=DIRECTION('center_axis',(0.,1.,0.));
#34562=DIRECTION('ref_axis',(1.,0.,0.));
#34563=DIRECTION('center_axis',(0.,1.,0.));
#34564=DIRECTION('ref_axis',(1.,0.,0.));
#34565=DIRECTION('center_axis',(0.,1.,0.));
#34566=DIRECTION('ref_axis',(1.,0.,0.));
#34567=DIRECTION('',(0.707106781186545,-0.70710678118655,-8.6595605623549E-17));
#34568=DIRECTION('center_axis',(0.,1.,0.));
#34569=DIRECTION('ref_axis',(1.,0.,0.));
#34570=DIRECTION('center_axis',(0.,1.,0.));
#34571=DIRECTION('ref_axis',(1.,0.,0.));
#34572=DIRECTION('center_axis',(-0.188314866426195,0.,0.982108706347156));
#34573=DIRECTION('ref_axis',(-0.982108706347156,0.,-0.188314866426195));
#34574=DIRECTION('',(0.,1.,0.));
#34575=DIRECTION('',(-0.982108706347156,0.,-0.188314866426195));
#34576=DIRECTION('',(0.,-1.,0.));
#34577=DIRECTION('center_axis',(-0.512859050871223,0.,-0.858472826558574));
#34578=DIRECTION('ref_axis',(0.858472826558574,0.,-0.512859050871223));
#34579=DIRECTION('',(0.,-1.,0.));
#34580=DIRECTION('',(0.858472826558574,0.,-0.512859050871223));
#34581=DIRECTION('center_axis',(0.,-1.,0.));
#34582=DIRECTION('ref_axis',(-0.17364817766693,0.,-0.984807753012208));
#34583=DIRECTION('center_axis',(0.,-1.,0.));
#34584=DIRECTION('ref_axis',(1.,0.,0.));
#34585=DIRECTION('center_axis',(0.,-1.,0.));
#34586=DIRECTION('ref_axis',(1.,0.,0.));
#34587=DIRECTION('center_axis',(0.,1.,0.));
#34588=DIRECTION('ref_axis',(1.,0.,0.));
#34589=DIRECTION('center_axis',(0.,1.,0.));
#34590=DIRECTION('ref_axis',(1.,0.,0.));
#34591=DIRECTION('center_axis',(0.,1.,0.));
#34592=DIRECTION('ref_axis',(1.,0.,0.));
#34593=DIRECTION('center_axis',(0.,1.,0.));
#34594=DIRECTION('ref_axis',(1.,0.,0.));
#34595=DIRECTION('center_axis',(0.,1.,0.));
#34596=DIRECTION('ref_axis',(1.,0.,0.));
#34597=DIRECTION('center_axis',(0.,1.,0.));
#34598=DIRECTION('ref_axis',(1.,0.,0.));
#34599=DIRECTION('center_axis',(0.,1.,0.));
#34600=DIRECTION('ref_axis',(1.,0.,0.));
#34601=DIRECTION('center_axis',(0.,1.,0.));
#34602=DIRECTION('ref_axis',(1.,0.,0.));
#34603=DIRECTION('center_axis',(0.,1.,0.));
#34604=DIRECTION('ref_axis',(1.,0.,0.));
#34605=DIRECTION('center_axis',(0.,1.,0.));
#34606=DIRECTION('ref_axis',(1.,0.,0.));
#34607=DIRECTION('center_axis',(0.,1.,0.));
#34608=DIRECTION('ref_axis',(1.,0.,0.));
#34609=DIRECTION('center_axis',(0.,1.,0.));
#34610=DIRECTION('ref_axis',(1.,0.,0.));
#34611=DIRECTION('center_axis',(0.,1.,0.));
#34612=DIRECTION('ref_axis',(1.,0.,0.));
#34613=DIRECTION('center_axis',(0.,1.,0.));
#34614=DIRECTION('ref_axis',(1.,0.,0.));
#34615=DIRECTION('center_axis',(0.,1.,0.));
#34616=DIRECTION('ref_axis',(1.,0.,0.));
#34617=DIRECTION('center_axis',(0.,1.,0.));
#34618=DIRECTION('ref_axis',(1.,0.,0.));
#34619=DIRECTION('center_axis',(0.,1.,0.));
#34620=DIRECTION('ref_axis',(1.,0.,0.));
#34621=DIRECTION('center_axis',(0.,1.,0.));
#34622=DIRECTION('ref_axis',(1.,0.,0.));
#34623=DIRECTION('center_axis',(0.,1.,0.));
#34624=DIRECTION('ref_axis',(1.,0.,0.));
#34625=DIRECTION('center_axis',(0.,1.,0.));
#34626=DIRECTION('ref_axis',(1.,0.,0.));
#34627=DIRECTION('center_axis',(0.,1.,0.));
#34628=DIRECTION('ref_axis',(1.,0.,0.));
#34629=DIRECTION('center_axis',(0.,1.,0.));
#34630=DIRECTION('ref_axis',(1.,0.,0.));
#34631=DIRECTION('center_axis',(0.,1.,0.));
#34632=DIRECTION('ref_axis',(1.,0.,0.));
#34633=DIRECTION('center_axis',(0.,1.,0.));
#34634=DIRECTION('ref_axis',(1.,0.,0.));
#34635=DIRECTION('center_axis',(0.,1.,0.));
#34636=DIRECTION('ref_axis',(1.,0.,0.));
#34637=DIRECTION('center_axis',(0.,1.,0.));
#34638=DIRECTION('ref_axis',(1.,0.,0.));
#34639=DIRECTION('center_axis',(0.,1.,0.));
#34640=DIRECTION('ref_axis',(1.,0.,0.));
#34641=DIRECTION('center_axis',(0.,1.,0.));
#34642=DIRECTION('ref_axis',(1.,0.,0.));
#34643=DIRECTION('center_axis',(0.,1.,0.));
#34644=DIRECTION('ref_axis',(1.,0.,0.));
#34645=DIRECTION('center_axis',(0.,1.,0.));
#34646=DIRECTION('ref_axis',(1.,0.,0.));
#34647=DIRECTION('center_axis',(0.,1.,0.));
#34648=DIRECTION('ref_axis',(1.,0.,0.));
#34649=DIRECTION('center_axis',(0.,1.,0.));
#34650=DIRECTION('ref_axis',(1.,0.,0.));
#34651=DIRECTION('center_axis',(0.,1.,0.));
#34652=DIRECTION('ref_axis',(1.,0.,0.));
#34653=DIRECTION('center_axis',(0.,1.,0.));
#34654=DIRECTION('ref_axis',(1.,0.,0.));
#34655=DIRECTION('center_axis',(0.,1.,0.));
#34656=DIRECTION('ref_axis',(1.,0.,0.));
#34657=DIRECTION('center_axis',(0.,1.,0.));
#34658=DIRECTION('ref_axis',(1.,0.,0.));
#34659=DIRECTION('',(0.707106781186545,0.70710678118655,8.6595605623549E-17));
#34660=DIRECTION('center_axis',(0.,-1.,0.));
#34661=DIRECTION('ref_axis',(1.,0.,0.));
#34662=DIRECTION('center_axis',(-0.0149125533359648,0.,0.999888801693969));
#34663=DIRECTION('ref_axis',(-0.999888801693969,0.,-0.0149125533359648));
#34664=DIRECTION('',(0.,1.,0.));
#34665=DIRECTION('',(-0.999888801693969,0.,-0.0149125533359648));
#34666=DIRECTION('',(0.,-1.,0.));
#34667=DIRECTION('center_axis',(-0.654139811408939,0.,-0.756373655761409));
#34668=DIRECTION('ref_axis',(0.756373655761409,0.,-0.654139811408939));
#34669=DIRECTION('',(0.,-1.,0.));
#34670=DIRECTION('',(0.756373655761409,0.,-0.654139811408939));
#34671=DIRECTION('center_axis',(0.,-1.,0.));
#34672=DIRECTION('ref_axis',(-0.342020143325669,0.,-0.939692620785908));
#34673=DIRECTION('center_axis',(0.,-1.,0.));
#34674=DIRECTION('ref_axis',(1.,0.,0.));
#34675=DIRECTION('center_axis',(0.158942870141262,0.,0.987287781769459));
#34676=DIRECTION('ref_axis',(-0.987287781769459,0.,0.158942870141262));
#34677=DIRECTION('',(0.,1.,0.));
#34678=DIRECTION('',(-0.987287781769459,0.,0.158942870141262));
#34679=DIRECTION('',(0.,-1.,0.));
#34680=DIRECTION('center_axis',(-0.775544864787709,0.,-0.631292454177471));
#34681=DIRECTION('ref_axis',(0.631292454177471,0.,-0.775544864787709));
#34682=DIRECTION('',(0.,-1.,0.));
#34683=DIRECTION('',(0.631292454177471,0.,-0.775544864787709));
#34684=DIRECTION('center_axis',(0.,-1.,0.));
#34685=DIRECTION('ref_axis',(-0.5,0.,-0.866025403784438));
#34686=DIRECTION('center_axis',(0.,-1.,0.));
#34687=DIRECTION('ref_axis',(1.,0.,0.));
#34688=DIRECTION('center_axis',(0.32796889493822,0.,0.944688522187606));
#34689=DIRECTION('ref_axis',(-0.944688522187606,0.,0.32796889493822));
#34690=DIRECTION('',(0.,1.,0.));
#34691=DIRECTION('',(-0.944688522187606,0.,0.32796889493822));
#34692=DIRECTION('',(0.,-1.,0.));
#34693=DIRECTION('center_axis',(-0.873385379894542,0.,-0.487029750822746));
#34694=DIRECTION('ref_axis',(0.487029750822746,0.,-0.873385379894542));
#34695=DIRECTION('',(0.,-1.,0.));
#34696=DIRECTION('',(0.487029750822746,0.,-0.873385379894542));
#34697=DIRECTION('center_axis',(0.,-1.,0.));
#34698=DIRECTION('ref_axis',(-0.64278760968654,0.,-0.766044443118978));
#34699=DIRECTION('center_axis',(0.,-1.,0.));
#34700=DIRECTION('ref_axis',(1.,0.,0.));
#34701=DIRECTION('center_axis',(0.487029750822748,0.,0.873385379894541));
#34702=DIRECTION('ref_axis',(-0.873385379894541,0.,0.487029750822748));
#34703=DIRECTION('',(0.,1.,0.));
#34704=DIRECTION('',(-0.873385379894541,0.,0.487029750822748));
#34705=DIRECTION('',(0.,-1.,0.));
#34706=DIRECTION('center_axis',(-0.944688522187607,0.,-0.327968894938217));
#34707=DIRECTION('ref_axis',(0.327968894938217,0.,-0.944688522187607));
#34708=DIRECTION('',(0.,-1.,0.));
#34709=DIRECTION('',(0.327968894938217,0.,-0.944688522187607));
#34710=DIRECTION('center_axis',(0.,-1.,0.));
#34711=DIRECTION('ref_axis',(-0.766044443118978,0.,-0.642787609686539));
#34712=DIRECTION('center_axis',(0.,-1.,0.));
#34713=DIRECTION('ref_axis',(1.,0.,0.));
#34714=DIRECTION('center_axis',(0.631292454177473,0.,0.775544864787707));
#34715=DIRECTION('ref_axis',(-0.775544864787707,0.,0.631292454177473));
#34716=DIRECTION('',(0.,1.,0.));
#34717=DIRECTION('',(-0.775544864787707,0.,0.631292454177473));
#34718=DIRECTION('',(0.,-1.,0.));
#34719=DIRECTION('center_axis',(-0.987287781769459,0.,-0.158942870141259));
#34720=DIRECTION('ref_axis',(0.158942870141259,0.,-0.987287781769459));
#34721=DIRECTION('',(0.,-1.,0.));
#34722=DIRECTION('',(0.158942870141259,0.,-0.987287781769459));
#34723=DIRECTION('center_axis',(0.,-1.,0.));
#34724=DIRECTION('ref_axis',(-0.866025403784439,0.,-0.5));
#34725=DIRECTION('center_axis',(0.,-1.,0.));
#34726=DIRECTION('ref_axis',(1.,0.,0.));
#34727=DIRECTION('center_axis',(0.756373655761411,0.,0.654139811408936));
#34728=DIRECTION('ref_axis',(-0.654139811408936,0.,0.756373655761411));
#34729=DIRECTION('',(0.,1.,0.));
#34730=DIRECTION('',(-0.654139811408936,0.,0.756373655761411));
#34731=DIRECTION('',(0.,-1.,0.));
#34732=DIRECTION('center_axis',(-0.999888801693969,0.,0.0149125533359685));
#34733=DIRECTION('ref_axis',(-0.0149125533359685,0.,-0.999888801693969));
#34734=DIRECTION('',(0.,-1.,0.));
#34735=DIRECTION('',(-0.0149125533359685,0.,-0.999888801693969));
#34736=DIRECTION('center_axis',(0.,-1.,0.));
#34737=DIRECTION('ref_axis',(-0.939692620785909,0.,-0.342020143325668));
#34738=DIRECTION('center_axis',(0.,-1.,0.));
#34739=DIRECTION('ref_axis',(1.,0.,0.));
#34740=DIRECTION('center_axis',(0.858472826558576,0.,0.512859050871221));
#34741=DIRECTION('ref_axis',(-0.512859050871221,0.,0.858472826558576));
#34742=DIRECTION('',(0.,1.,0.));
#34743=DIRECTION('',(-0.512859050871221,0.,0.858472826558576));
#34744=DIRECTION('',(0.,-1.,0.));
#34745=DIRECTION('center_axis',(-0.982108706347156,0.,0.188314866426198));
#34746=DIRECTION('ref_axis',(-0.188314866426198,0.,-0.982108706347155));
#34747=DIRECTION('',(0.,-1.,0.));
#34748=DIRECTION('',(-0.188314866426198,0.,-0.982108706347155));
#34749=DIRECTION('center_axis',(0.,-1.,0.));
#34750=DIRECTION('ref_axis',(-0.984807753012208,0.,-0.17364817766693));
#34751=DIRECTION('center_axis',(0.,-1.,0.));
#34752=DIRECTION('ref_axis',(1.,0.,0.));
#34753=DIRECTION('center_axis',(0.934487734928969,0.,0.355995327591985));
#34754=DIRECTION('ref_axis',(-0.355995327591985,0.,0.934487734928969));
#34755=DIRECTION('',(0.,1.,0.));
#34756=DIRECTION('',(-0.355995327591985,0.,0.934487734928969));
#34757=DIRECTION('',(0.,-1.,0.));
#34758=DIRECTION('center_axis',(-0.934487734928968,0.,0.355995327591988));
#34759=DIRECTION('ref_axis',(-0.355995327591988,0.,-0.934487734928968));
#34760=DIRECTION('',(0.,-1.,0.));
#34761=DIRECTION('',(-0.355995327591988,0.,-0.934487734928968));
#34762=DIRECTION('center_axis',(0.,-1.,0.));
#34763=DIRECTION('ref_axis',(-1.,0.,1.83697019872103E-16));
#34764=DIRECTION('center_axis',(0.,-1.,0.));
#34765=DIRECTION('ref_axis',(1.,0.,0.));
#34766=DIRECTION('center_axis',(0.982108706347156,0.,0.188314866426195));
#34767=DIRECTION('ref_axis',(-0.188314866426195,0.,0.982108706347156));
#34768=DIRECTION('',(0.,1.,0.));
#34769=DIRECTION('',(-0.188314866426195,0.,0.982108706347156));
#34770=DIRECTION('',(0.,-1.,0.));
#34771=DIRECTION('center_axis',(-0.858472826558574,0.,0.512859050871223));
#34772=DIRECTION('ref_axis',(-0.512859050871223,0.,-0.858472826558574));
#34773=DIRECTION('',(0.,-1.,0.));
#34774=DIRECTION('',(-0.512859050871223,0.,-0.858472826558574));
#34775=DIRECTION('center_axis',(0.,-1.,0.));
#34776=DIRECTION('ref_axis',(-0.984807753012208,0.,0.17364817766693));
#34777=DIRECTION('center_axis',(0.,-1.,0.));
#34778=DIRECTION('ref_axis',(1.,0.,0.));
#34779=DIRECTION('center_axis',(0.999888801693969,0.,0.0149125533359649));
#34780=DIRECTION('ref_axis',(-0.0149125533359649,0.,0.999888801693969));
#34781=DIRECTION('',(0.,1.,0.));
#34782=DIRECTION('',(-0.0149125533359649,0.,0.999888801693969));
#34783=DIRECTION('',(0.,-1.,0.));
#34784=DIRECTION('center_axis',(-0.756373655761409,0.,0.654139811408939));
#34785=DIRECTION('ref_axis',(-0.654139811408939,0.,-0.756373655761409));
#34786=DIRECTION('',(0.,-1.,0.));
#34787=DIRECTION('',(-0.654139811408939,0.,-0.756373655761409));
#34788=DIRECTION('center_axis',(0.,-1.,0.));
#34789=DIRECTION('ref_axis',(-0.939692620785908,0.,0.342020143325669));
#34790=DIRECTION('center_axis',(0.,-1.,0.));
#34791=DIRECTION('ref_axis',(1.,0.,0.));
#34792=DIRECTION('center_axis',(0.987287781769459,0.,-0.158942870141262));
#34793=DIRECTION('ref_axis',(0.158942870141262,0.,0.987287781769459));
#34794=DIRECTION('',(0.,1.,0.));
#34795=DIRECTION('',(0.158942870141262,0.,0.987287781769459));
#34796=DIRECTION('',(0.,-1.,0.));
#34797=DIRECTION('center_axis',(-0.631292454177471,0.,0.775544864787709));
#34798=DIRECTION('ref_axis',(-0.775544864787709,0.,-0.631292454177471));
#34799=DIRECTION('',(0.,-1.,0.));
#34800=DIRECTION('',(-0.775544864787709,0.,-0.631292454177471));
#34801=DIRECTION('center_axis',(0.,-1.,0.));
#34802=DIRECTION('ref_axis',(-0.866025403784438,0.,0.5));
#34803=DIRECTION('center_axis',(0.,-1.,0.));
#34804=DIRECTION('ref_axis',(1.,0.,0.));
#34805=DIRECTION('center_axis',(0.944688522187606,0.,-0.32796889493822));
#34806=DIRECTION('ref_axis',(0.32796889493822,0.,0.944688522187606));
#34807=DIRECTION('',(0.,1.,0.));
#34808=DIRECTION('',(0.32796889493822,0.,0.944688522187606));
#34809=DIRECTION('',(0.,-1.,0.));
#34810=DIRECTION('center_axis',(-0.487029750822746,0.,0.873385379894542));
#34811=DIRECTION('ref_axis',(-0.873385379894542,0.,-0.487029750822746));
#34812=DIRECTION('',(0.,-1.,0.));
#34813=DIRECTION('',(-0.873385379894542,0.,-0.487029750822746));
#34814=DIRECTION('center_axis',(0.,-1.,0.));
#34815=DIRECTION('ref_axis',(-0.766044443118978,0.,0.642787609686539));
#34816=DIRECTION('center_axis',(0.,-1.,0.));
#34817=DIRECTION('ref_axis',(1.,0.,0.));
#34818=DIRECTION('center_axis',(0.873385379894541,0.,-0.487029750822748));
#34819=DIRECTION('ref_axis',(0.487029750822748,0.,0.873385379894541));
#34820=DIRECTION('',(0.,1.,0.));
#34821=DIRECTION('',(0.487029750822748,0.,0.873385379894541));
#34822=DIRECTION('',(0.,-1.,0.));
#34823=DIRECTION('center_axis',(-0.327968894938217,0.,0.944688522187607));
#34824=DIRECTION('ref_axis',(-0.944688522187607,0.,-0.327968894938217));
#34825=DIRECTION('',(0.,-1.,0.));
#34826=DIRECTION('',(-0.944688522187607,0.,-0.327968894938217));
#34827=DIRECTION('center_axis',(0.,-1.,0.));
#34828=DIRECTION('ref_axis',(-0.642787609686539,0.,0.766044443118978));
#34829=DIRECTION('center_axis',(0.,-1.,0.));
#34830=DIRECTION('ref_axis',(1.,0.,0.));
#34831=DIRECTION('center_axis',(0.775544864787707,0.,-0.631292454177473));
#34832=DIRECTION('ref_axis',(0.631292454177473,0.,0.775544864787707));
#34833=DIRECTION('',(0.,1.,0.));
#34834=DIRECTION('',(0.631292454177473,0.,0.775544864787707));
#34835=DIRECTION('',(0.,-1.,0.));
#34836=DIRECTION('center_axis',(-0.158942870141259,0.,0.987287781769459));
#34837=DIRECTION('ref_axis',(-0.987287781769459,0.,-0.158942870141259));
#34838=DIRECTION('',(0.,-1.,0.));
#34839=DIRECTION('',(-0.987287781769459,0.,-0.158942870141259));
#34840=DIRECTION('center_axis',(0.,-1.,0.));
#34841=DIRECTION('ref_axis',(-0.5,0.,0.866025403784439));
#34842=DIRECTION('center_axis',(0.,-1.,0.));
#34843=DIRECTION('ref_axis',(1.,0.,0.));
#34844=DIRECTION('center_axis',(0.654139811408936,0.,-0.756373655761411));
#34845=DIRECTION('ref_axis',(0.756373655761411,0.,0.654139811408936));
#34846=DIRECTION('',(0.,1.,0.));
#34847=DIRECTION('',(0.75637365576141,0.,0.654139811408937));
#34848=DIRECTION('',(0.,-1.,0.));
#34849=DIRECTION('center_axis',(0.014912553335968,0.,0.999888801693969));
#34850=DIRECTION('ref_axis',(-0.999888801693969,0.,0.014912553335968));
#34851=DIRECTION('',(0.,-1.,0.));
#34852=DIRECTION('',(-0.999888801693969,0.,0.014912553335968));
#34853=DIRECTION('center_axis',(0.,-1.,0.));
#34854=DIRECTION('ref_axis',(-0.342020143325669,0.,0.939692620785908));
#34855=DIRECTION('center_axis',(0.,-1.,0.));
#34856=DIRECTION('ref_axis',(1.,0.,0.));
#34857=DIRECTION('center_axis',(0.512859050871221,0.,-0.858472826558576));
#34858=DIRECTION('ref_axis',(0.858472826558576,0.,0.512859050871221));
#34859=DIRECTION('',(0.,1.,0.));
#34860=DIRECTION('',(0.858472826558576,0.,0.512859050871221));
#34861=DIRECTION('',(0.,-1.,0.));
#34862=DIRECTION('center_axis',(0.188314866426198,0.,0.982108706347156));
#34863=DIRECTION('ref_axis',(-0.982108706347156,0.,0.188314866426198));
#34864=DIRECTION('',(0.,-1.,0.));
#34865=DIRECTION('',(-0.982108706347155,0.,0.188314866426198));
#34866=DIRECTION('center_axis',(0.,-1.,0.));
#34867=DIRECTION('ref_axis',(-0.17364817766693,0.,0.984807753012208));
#34868=DIRECTION('center_axis',(0.,-1.,0.));
#34869=DIRECTION('ref_axis',(1.,0.,0.));
#34870=DIRECTION('center_axis',(0.355995327591986,0.,-0.934487734928969));
#34871=DIRECTION('ref_axis',(0.934487734928969,0.,0.355995327591986));
#34872=DIRECTION('',(0.,1.,0.));
#34873=DIRECTION('',(0.934487734928969,0.,0.355995327591986));
#34874=DIRECTION('',(0.,-1.,0.));
#34875=DIRECTION('center_axis',(0.355995327591988,0.,0.934487734928968));
#34876=DIRECTION('ref_axis',(-0.934487734928968,0.,0.355995327591988));
#34877=DIRECTION('',(0.,-1.,0.));
#34878=DIRECTION('',(-0.934487734928968,0.,0.355995327591988));
#34879=DIRECTION('center_axis',(0.,-1.,0.));
#34880=DIRECTION('ref_axis',(1.22464679914735E-16,0.,1.));
#34881=DIRECTION('center_axis',(0.,-1.,0.));
#34882=DIRECTION('ref_axis',(1.,0.,0.));
#34883=DIRECTION('center_axis',(0.,-1.,0.));
#34884=DIRECTION('ref_axis',(1.,0.,0.));
#34885=DIRECTION('center_axis',(0.188314866426195,0.,-0.982108706347156));
#34886=DIRECTION('ref_axis',(0.982108706347156,0.,0.188314866426195));
#34887=DIRECTION('',(0.,1.,0.));
#34888=DIRECTION('',(0.982108706347156,0.,0.188314866426195));
#34889=DIRECTION('',(0.,-1.,0.));
#34890=DIRECTION('center_axis',(0.512859050871224,0.,0.858472826558574));
#34891=DIRECTION('ref_axis',(-0.858472826558574,0.,0.512859050871224));
#34892=DIRECTION('',(0.,-1.,0.));
#34893=DIRECTION('',(-0.858472826558574,0.,0.512859050871224));
#34894=DIRECTION('center_axis',(0.,-1.,0.));
#34895=DIRECTION('ref_axis',(0.173648177666931,0.,0.984807753012208));
#34896=DIRECTION('center_axis',(0.,-1.,0.));
#34897=DIRECTION('ref_axis',(1.,0.,0.));
#34898=DIRECTION('center_axis',(0.0149125533359654,0.,-0.999888801693969));
#34899=DIRECTION('ref_axis',(0.999888801693969,0.,0.0149125533359654));
#34900=DIRECTION('',(0.,1.,0.));
#34901=DIRECTION('',(0.999888801693969,0.,0.0149125533359654));
#34902=DIRECTION('',(0.,-1.,0.));
#34903=DIRECTION('center_axis',(0.654139811408939,0.,0.756373655761409));
#34904=DIRECTION('ref_axis',(-0.756373655761409,0.,0.654139811408939));
#34905=DIRECTION('',(0.,-1.,0.));
#34906=DIRECTION('',(-0.756373655761409,0.,0.654139811408938));
#34907=DIRECTION('center_axis',(0.,-1.,0.));
#34908=DIRECTION('ref_axis',(0.342020143325669,0.,0.939692620785908));
#34909=DIRECTION('center_axis',(0.,-1.,0.));
#34910=DIRECTION('ref_axis',(1.,0.,0.));
#34911=DIRECTION('center_axis',(-0.158942870141261,0.,-0.987287781769459));
#34912=DIRECTION('ref_axis',(0.987287781769459,0.,-0.158942870141261));
#34913=DIRECTION('',(0.,1.,0.));
#34914=DIRECTION('',(0.987287781769459,0.,-0.158942870141261));
#34915=DIRECTION('',(0.,-1.,0.));
#34916=DIRECTION('center_axis',(0.775544864787709,0.,0.631292454177471));
#34917=DIRECTION('ref_axis',(-0.631292454177471,0.,0.775544864787709));
#34918=DIRECTION('',(0.,-1.,0.));
#34919=DIRECTION('',(-0.631292454177471,0.,0.775544864787709));
#34920=DIRECTION('center_axis',(0.,-1.,0.));
#34921=DIRECTION('ref_axis',(0.5,0.,0.866025403784439));
#34922=DIRECTION('center_axis',(0.,-1.,0.));
#34923=DIRECTION('ref_axis',(1.,0.,0.));
#34924=DIRECTION('center_axis',(-0.32796889493822,0.,-0.944688522187606));
#34925=DIRECTION('ref_axis',(0.944688522187606,0.,-0.32796889493822));
#34926=DIRECTION('',(0.,1.,0.));
#34927=DIRECTION('',(0.944688522187606,0.,-0.32796889493822));
#34928=DIRECTION('',(0.,-1.,0.));
#34929=DIRECTION('center_axis',(0.873385379894542,0.,0.487029750822746));
#34930=DIRECTION('ref_axis',(-0.487029750822746,0.,0.873385379894542));
#34931=DIRECTION('',(0.,-1.,0.));
#34932=DIRECTION('',(-0.487029750822746,0.,0.873385379894542));
#34933=DIRECTION('center_axis',(0.,-1.,0.));
#34934=DIRECTION('ref_axis',(0.642787609686539,0.,0.766044443118978));
#34935=DIRECTION('center_axis',(0.,-1.,0.));
#34936=DIRECTION('ref_axis',(1.,0.,0.));
#34937=DIRECTION('center_axis',(-0.487029750822748,0.,-0.873385379894541));
#34938=DIRECTION('ref_axis',(0.873385379894541,0.,-0.487029750822748));
#34939=DIRECTION('',(0.,1.,0.));
#34940=DIRECTION('',(0.873385379894541,0.,-0.487029750822748));
#34941=DIRECTION('',(0.,-1.,0.));
#34942=DIRECTION('center_axis',(0.944688522187607,0.,0.327968894938217));
#34943=DIRECTION('ref_axis',(-0.327968894938217,0.,0.944688522187607));
#34944=DIRECTION('',(0.,-1.,0.));
#34945=DIRECTION('',(-0.327968894938217,0.,0.944688522187607));
#34946=DIRECTION('center_axis',(0.,-1.,0.));
#34947=DIRECTION('ref_axis',(0.766044443118978,0.,0.642787609686539));
#34948=DIRECTION('center_axis',(0.,-1.,0.));
#34949=DIRECTION('ref_axis',(1.,0.,0.));
#34950=DIRECTION('center_axis',(-0.631292454177473,0.,-0.775544864787707));
#34951=DIRECTION('ref_axis',(0.775544864787707,0.,-0.631292454177473));
#34952=DIRECTION('',(0.,1.,0.));
#34953=DIRECTION('',(0.775544864787707,0.,-0.631292454177473));
#34954=DIRECTION('',(0.,-1.,0.));
#34955=DIRECTION('center_axis',(0.987287781769459,0.,0.158942870141259));
#34956=DIRECTION('ref_axis',(-0.158942870141259,0.,0.987287781769459));
#34957=DIRECTION('',(0.,-1.,0.));
#34958=DIRECTION('',(-0.158942870141259,0.,0.987287781769459));
#34959=DIRECTION('center_axis',(0.,-1.,0.));
#34960=DIRECTION('ref_axis',(0.866025403784439,0.,0.5));
#34961=DIRECTION('center_axis',(0.,-1.,0.));
#34962=DIRECTION('ref_axis',(1.,0.,0.));
#34963=DIRECTION('center_axis',(-0.756373655761411,0.,-0.654139811408937));
#34964=DIRECTION('ref_axis',(0.654139811408937,0.,-0.756373655761411));
#34965=DIRECTION('',(0.,1.,0.));
#34966=DIRECTION('',(0.654139811408937,0.,-0.75637365576141));
#34967=DIRECTION('',(0.,-1.,0.));
#34968=DIRECTION('center_axis',(0.999888801693969,0.,-0.014912553335968));
#34969=DIRECTION('ref_axis',(0.014912553335968,0.,0.999888801693969));
#34970=DIRECTION('',(0.,-1.,0.));
#34971=DIRECTION('',(0.014912553335968,0.,0.999888801693969));
#34972=DIRECTION('center_axis',(0.,-1.,0.));
#34973=DIRECTION('ref_axis',(0.939692620785908,0.,0.342020143325669));
#34974=DIRECTION('center_axis',(0.,-1.,0.));
#34975=DIRECTION('ref_axis',(1.,0.,0.));
#34976=DIRECTION('center_axis',(-0.858472826558576,0.,-0.512859050871221));
#34977=DIRECTION('ref_axis',(0.512859050871221,0.,-0.858472826558576));
#34978=DIRECTION('',(0.,1.,0.));
#34979=DIRECTION('',(0.512859050871221,0.,-0.858472826558576));
#34980=DIRECTION('',(0.,-1.,0.));
#34981=DIRECTION('center_axis',(0.982108706347156,0.,-0.188314866426198));
#34982=DIRECTION('ref_axis',(0.188314866426198,0.,0.982108706347155));
#34983=DIRECTION('',(0.,-1.,0.));
#34984=DIRECTION('',(0.188314866426198,0.,0.982108706347156));
#34985=DIRECTION('center_axis',(0.,-1.,0.));
#34986=DIRECTION('ref_axis',(0.984807753012208,0.,0.17364817766693));
#34987=DIRECTION('center_axis',(0.,-1.,0.));
#34988=DIRECTION('ref_axis',(1.,0.,0.));
#34989=DIRECTION('center_axis',(-0.934487734928969,0.,-0.355995327591986));
#34990=DIRECTION('ref_axis',(0.355995327591986,0.,-0.934487734928969));
#34991=DIRECTION('',(0.,1.,0.));
#34992=DIRECTION('',(0.355995327591986,0.,-0.934487734928969));
#34993=DIRECTION('',(0.,-1.,0.));
#34994=DIRECTION('center_axis',(0.934487734928968,0.,-0.355995327591988));
#34995=DIRECTION('ref_axis',(0.355995327591988,0.,0.934487734928968));
#34996=DIRECTION('',(0.,-1.,0.));
#34997=DIRECTION('',(0.355995327591988,0.,0.934487734928968));
#34998=DIRECTION('center_axis',(0.,-1.,0.));
#34999=DIRECTION('ref_axis',(1.,0.,-6.12323399573677E-17));
#35000=DIRECTION('center_axis',(0.,-1.,0.));
#35001=DIRECTION('ref_axis',(1.,0.,0.));
#35002=DIRECTION('center_axis',(-0.982108706347156,0.,-0.188314866426195));
#35003=DIRECTION('ref_axis',(0.188314866426195,0.,-0.982108706347156));
#35004=DIRECTION('',(0.,1.,0.));
#35005=DIRECTION('',(0.188314866426195,0.,-0.982108706347156));
#35006=DIRECTION('',(0.,-1.,0.));
#35007=DIRECTION('center_axis',(0.858472826558574,0.,-0.512859050871223));
#35008=DIRECTION('ref_axis',(0.512859050871223,0.,0.858472826558574));
#35009=DIRECTION('',(0.,-1.,0.));
#35010=DIRECTION('',(0.512859050871223,0.,0.858472826558574));
#35011=DIRECTION('center_axis',(0.,-1.,0.));
#35012=DIRECTION('ref_axis',(0.984807753012208,0.,-0.17364817766693));
#35013=DIRECTION('center_axis',(0.,-1.,0.));
#35014=DIRECTION('ref_axis',(1.,0.,0.));
#35015=DIRECTION('center_axis',(-0.999888801693969,0.,-0.0149125533359654));
#35016=DIRECTION('ref_axis',(0.0149125533359654,0.,-0.999888801693969));
#35017=DIRECTION('',(0.,1.,0.));
#35018=DIRECTION('',(0.0149125533359654,0.,-0.999888801693969));
#35019=DIRECTION('',(0.,-1.,0.));
#35020=DIRECTION('center_axis',(0.756373655761409,0.,-0.654139811408938));
#35021=DIRECTION('ref_axis',(0.654139811408938,0.,0.756373655761409));
#35022=DIRECTION('',(0.,-1.,0.));
#35023=DIRECTION('',(0.654139811408938,0.,0.756373655761409));
#35024=DIRECTION('center_axis',(0.,-1.,0.));
#35025=DIRECTION('ref_axis',(0.939692620785908,0.,-0.342020143325669));
#35026=DIRECTION('center_axis',(0.,-1.,0.));
#35027=DIRECTION('ref_axis',(1.,0.,0.));
#35028=DIRECTION('center_axis',(-0.987287781769459,0.,0.158942870141262));
#35029=DIRECTION('ref_axis',(-0.158942870141262,0.,-0.987287781769459));
#35030=DIRECTION('',(0.,1.,0.));
#35031=DIRECTION('',(-0.158942870141262,0.,-0.987287781769459));
#35032=DIRECTION('',(0.,-1.,0.));
#35033=DIRECTION('center_axis',(0.631292454177471,0.,-0.775544864787709));
#35034=DIRECTION('ref_axis',(0.775544864787709,0.,0.631292454177471));
#35035=DIRECTION('',(0.,-1.,0.));
#35036=DIRECTION('',(0.775544864787709,0.,0.631292454177471));
#35037=DIRECTION('center_axis',(0.,-1.,0.));
#35038=DIRECTION('ref_axis',(0.866025403784439,0.,-0.5));
#35039=DIRECTION('center_axis',(0.,-1.,0.));
#35040=DIRECTION('ref_axis',(1.,0.,0.));
#35041=DIRECTION('center_axis',(-0.944688522187606,0.,0.32796889493822));
#35042=DIRECTION('ref_axis',(-0.32796889493822,0.,-0.944688522187606));
#35043=DIRECTION('',(0.,1.,0.));
#35044=DIRECTION('',(-0.32796889493822,0.,-0.944688522187606));
#35045=DIRECTION('',(0.,-1.,0.));
#35046=DIRECTION('center_axis',(0.487029750822746,0.,-0.873385379894542));
#35047=DIRECTION('ref_axis',(0.873385379894542,0.,0.487029750822746));
#35048=DIRECTION('',(0.,-1.,0.));
#35049=DIRECTION('',(0.873385379894542,0.,0.487029750822746));
#35050=DIRECTION('center_axis',(0.,-1.,0.));
#35051=DIRECTION('ref_axis',(0.766044443118978,0.,-0.642787609686539));
#35052=DIRECTION('center_axis',(0.,-1.,0.));
#35053=DIRECTION('ref_axis',(1.,0.,0.));
#35054=DIRECTION('center_axis',(-0.873385379894541,0.,0.487029750822748));
#35055=DIRECTION('ref_axis',(-0.487029750822748,0.,-0.873385379894541));
#35056=DIRECTION('',(0.,1.,0.));
#35057=DIRECTION('',(-0.487029750822748,0.,-0.873385379894541));
#35058=DIRECTION('',(0.,-1.,0.));
#35059=DIRECTION('center_axis',(0.327968894938217,0.,-0.944688522187607));
#35060=DIRECTION('ref_axis',(0.944688522187607,0.,0.327968894938217));
#35061=DIRECTION('',(0.,-1.,0.));
#35062=DIRECTION('',(0.944688522187607,0.,0.327968894938217));
#35063=DIRECTION('center_axis',(0.,-1.,0.));
#35064=DIRECTION('ref_axis',(0.642787609686539,0.,-0.766044443118978));
#35065=DIRECTION('center_axis',(0.,-1.,0.));
#35066=DIRECTION('ref_axis',(1.,0.,0.));
#35067=DIRECTION('center_axis',(-0.775544864787707,0.,0.631292454177473));
#35068=DIRECTION('ref_axis',(-0.631292454177473,0.,-0.775544864787707));
#35069=DIRECTION('',(0.,1.,0.));
#35070=DIRECTION('',(-0.631292454177473,0.,-0.775544864787707));
#35071=DIRECTION('',(0.,-1.,0.));
#35072=DIRECTION('center_axis',(0.158942870141259,0.,-0.987287781769459));
#35073=DIRECTION('ref_axis',(0.987287781769459,0.,0.158942870141259));
#35074=DIRECTION('',(0.,-1.,0.));
#35075=DIRECTION('',(0.987287781769459,0.,0.158942870141259));
#35076=DIRECTION('center_axis',(0.,-1.,0.));
#35077=DIRECTION('ref_axis',(0.5,0.,-0.866025403784439));
#35078=DIRECTION('center_axis',(0.,-1.,0.));
#35079=DIRECTION('ref_axis',(1.,0.,0.));
#35080=DIRECTION('center_axis',(-0.654139811408937,0.,0.756373655761411));
#35081=DIRECTION('ref_axis',(-0.756373655761411,0.,-0.654139811408937));
#35082=DIRECTION('',(0.,1.,0.));
#35083=DIRECTION('',(-0.75637365576141,0.,-0.654139811408937));
#35084=DIRECTION('',(0.,-1.,0.));
#35085=DIRECTION('center_axis',(-0.014912553335968,0.,-0.999888801693969));
#35086=DIRECTION('ref_axis',(0.999888801693969,0.,-0.014912553335968));
#35087=DIRECTION('',(0.,-1.,0.));
#35088=DIRECTION('',(0.999888801693969,0.,-0.014912553335968));
#35089=DIRECTION('center_axis',(0.,-1.,0.));
#35090=DIRECTION('ref_axis',(0.342020143325669,0.,-0.939692620785908));
#35091=DIRECTION('center_axis',(0.,-1.,0.));
#35092=DIRECTION('ref_axis',(1.,0.,0.));
#35093=DIRECTION('center_axis',(-0.512859050871221,0.,0.858472826558576));
#35094=DIRECTION('ref_axis',(-0.858472826558576,0.,-0.512859050871221));
#35095=DIRECTION('',(0.,1.,0.));
#35096=DIRECTION('',(-0.858472826558576,0.,-0.512859050871221));
#35097=DIRECTION('',(0.,-1.,0.));
#35098=DIRECTION('center_axis',(-0.188314866426198,0.,-0.982108706347156));
#35099=DIRECTION('ref_axis',(0.982108706347156,0.,-0.188314866426198));
#35100=DIRECTION('',(0.,-1.,0.));
#35101=DIRECTION('',(0.982108706347155,0.,-0.188314866426198));
#35102=DIRECTION('center_axis',(0.,-1.,0.));
#35103=DIRECTION('ref_axis',(0.17364817766693,0.,-0.984807753012208));
#35104=DIRECTION('center_axis',(0.,-1.,0.));
#35105=DIRECTION('ref_axis',(1.,0.,0.));
#35106=DIRECTION('center_axis',(-0.355995327591986,0.,0.934487734928969));
#35107=DIRECTION('ref_axis',(-0.934487734928969,0.,-0.355995327591986));
#35108=DIRECTION('',(0.,1.,0.));
#35109=DIRECTION('',(-0.934487734928969,0.,-0.355995327591986));
#35110=DIRECTION('',(0.,-1.,0.));
#35111=DIRECTION('center_axis',(-0.355995327591988,0.,-0.934487734928968));
#35112=DIRECTION('ref_axis',(0.934487734928968,0.,-0.355995327591988));
#35113=DIRECTION('',(0.,-1.,0.));
#35114=DIRECTION('',(0.934487734928968,0.,-0.355995327591988));
#35115=DIRECTION('center_axis',(0.,-1.,0.));
#35116=DIRECTION('ref_axis',(0.,0.,-1.));
#35117=DIRECTION('center_axis',(0.,-1.,0.));
#35118=DIRECTION('ref_axis',(1.,0.,0.));
#35119=DIRECTION('center_axis',(0.,1.,0.));
#35120=DIRECTION('ref_axis',(1.,0.,0.));
#35121=DIRECTION('',(0.,-1.,0.));
#35122=DIRECTION('center_axis',(0.,1.,0.));
#35123=DIRECTION('ref_axis',(1.,0.,0.));
#35124=DIRECTION('',(0.5,0.,-0.866025403784439));
#35125=DIRECTION('',(1.,0.,0.));
#35126=DIRECTION('',(0.5,0.,0.866025403784439));
#35127=DIRECTION('',(-0.5,0.,0.866025403784439));
#35128=DIRECTION('',(-1.,0.,0.));
#35129=DIRECTION('',(-0.5,0.,-0.866025403784439));
#35130=DIRECTION('center_axis',(0.,1.,0.));
#35131=DIRECTION('ref_axis',(0.,0.,1.));
#35132=DIRECTION('',(0.5,0.,-0.866025403784439));
#35133=DIRECTION('center_axis',(0.,-1.,0.));
#35134=DIRECTION('ref_axis',(1.,0.,0.));
#35135=DIRECTION('center_axis',(0.,1.,0.));
#35136=DIRECTION('ref_axis',(0.,0.,1.));
#35137=DIRECTION('',(1.,0.,0.));
#35138=DIRECTION('center_axis',(0.,-1.,0.));
#35139=DIRECTION('ref_axis',(1.,0.,0.));
#35140=DIRECTION('center_axis',(0.,1.,0.));
#35141=DIRECTION('ref_axis',(0.,0.,1.));
#35142=DIRECTION('',(0.5,0.,0.866025403784439));
#35143=DIRECTION('center_axis',(0.,-1.,0.));
#35144=DIRECTION('ref_axis',(1.,0.,0.));
#35145=DIRECTION('center_axis',(0.,1.,0.));
#35146=DIRECTION('ref_axis',(0.,0.,1.));
#35147=DIRECTION('',(-0.5,0.,0.866025403784439));
#35148=DIRECTION('center_axis',(0.,-1.,0.));
#35149=DIRECTION('ref_axis',(1.,0.,0.));
#35150=DIRECTION('center_axis',(0.,1.,0.));
#35151=DIRECTION('ref_axis',(0.,0.,1.));
#35152=DIRECTION('',(-1.,0.,0.));
#35153=DIRECTION('center_axis',(0.,-1.,0.));
#35154=DIRECTION('ref_axis',(1.,0.,0.));
#35155=DIRECTION('center_axis',(0.,1.,0.));
#35156=DIRECTION('ref_axis',(0.,0.,1.));
#35157=DIRECTION('',(-0.5,0.,-0.866025403784439));
#35158=DIRECTION('center_axis',(0.,-1.,0.));
#35159=DIRECTION('ref_axis',(1.,0.,0.));
#35160=DIRECTION('center_axis',(0.,1.,0.));
#35161=DIRECTION('ref_axis',(1.,0.,0.));
#35162=DIRECTION('',(-0.85716730070211,0.515038074910058,1.04972719113862E-16));
#35163=DIRECTION('center_axis',(-0.866025403784439,0.,-0.5));
#35164=DIRECTION('ref_axis',(0.5,0.,-0.866025403784439));
#35165=DIRECTION('',(0.,-1.,0.));
#35166=DIRECTION('',(0.,-1.,0.));
#35167=DIRECTION('center_axis',(-0.866025403784439,0.,0.5));
#35168=DIRECTION('ref_axis',(-0.5,0.,-0.866025403784439));
#35169=DIRECTION('',(0.,-1.,0.));
#35170=DIRECTION('center_axis',(0.,0.,1.));
#35171=DIRECTION('ref_axis',(-1.,0.,0.));
#35172=DIRECTION('',(0.,-1.,0.));
#35173=DIRECTION('center_axis',(0.866025403784439,0.,0.5));
#35174=DIRECTION('ref_axis',(-0.5,0.,0.866025403784439));
#35175=DIRECTION('',(0.,-1.,0.));
#35176=DIRECTION('center_axis',(0.866025403784439,0.,-0.5));
#35177=DIRECTION('ref_axis',(0.5,0.,0.866025403784439));
#35178=DIRECTION('',(0.,-1.,0.));
#35179=DIRECTION('center_axis',(0.,0.,-1.));
#35180=DIRECTION('ref_axis',(1.,0.,0.));
#35181=DIRECTION('axis',(0.,0.,1.));
#35182=DIRECTION('refdir',(1.,0.,0.));
#35183=DIRECTION('center_axis',(0.,-1.,0.));
#35184=DIRECTION('ref_axis',(0.653824539037156,0.,-0.756646200117896));
#35185=DIRECTION('',(0.,1.,0.));
#35186=DIRECTION('center_axis',(0.,1.,0.));
#35187=DIRECTION('ref_axis',(1.,0.,1.17141641968325E-13));
#35188=DIRECTION('center_axis',(0.,-1.,0.));
#35189=DIRECTION('ref_axis',(0.653824539037156,0.,-0.756646200117896));
#35190=DIRECTION('',(0.,1.,0.));
#35191=DIRECTION('center_axis',(0.,-1.,0.));
#35192=DIRECTION('ref_axis',(0.653824539037156,0.,-0.756646200117896));
#35193=DIRECTION('',(0.,1.,0.));
#35194=DIRECTION('center_axis',(0.,-1.,0.));
#35195=DIRECTION('ref_axis',(0.653824539037156,0.,-0.756646200117896));
#35196=DIRECTION('',(0.,1.,0.));
#35197=DIRECTION('center_axis',(0.,-1.,0.));
#35198=DIRECTION('ref_axis',(0.653824539037156,0.,-0.756646200117896));
#35199=DIRECTION('',(0.,1.,0.));
#35200=DIRECTION('center_axis',(0.,-1.,0.));
#35201=DIRECTION('ref_axis',(0.653824539037156,0.,-0.756646200117896));
#35202=DIRECTION('',(0.,1.,0.));
#35203=DIRECTION('center_axis',(0.,-1.,0.));
#35204=DIRECTION('ref_axis',(0.653824539037156,0.,-0.756646200117896));
#35205=DIRECTION('',(0.,1.,0.));
#35206=DIRECTION('center_axis',(0.,-1.,0.));
#35207=DIRECTION('ref_axis',(0.653824539037156,0.,-0.756646200117896));
#35208=DIRECTION('',(0.,1.,0.));
#35209=DIRECTION('center_axis',(0.,-1.,0.));
#35210=DIRECTION('ref_axis',(0.653824539037156,0.,-0.756646200117896));
#35211=DIRECTION('',(0.,1.,0.));
#35212=DIRECTION('center_axis',(0.,-1.,0.));
#35213=DIRECTION('ref_axis',(0.653824539037156,0.,-0.756646200117896));
#35214=DIRECTION('',(0.,1.,0.));
#35215=DIRECTION('center_axis',(0.,-1.,0.));
#35216=DIRECTION('ref_axis',(0.653824539037156,0.,-0.756646200117896));
#35217=DIRECTION('',(0.,1.,0.));
#35218=DIRECTION('center_axis',(0.,-1.,0.));
#35219=DIRECTION('ref_axis',(0.653824539037156,0.,-0.756646200117896));
#35220=DIRECTION('',(0.,1.,0.));
#35221=DIRECTION('center_axis',(0.,-1.,0.));
#35222=DIRECTION('ref_axis',(0.653824539037156,0.,-0.756646200117896));
#35223=DIRECTION('',(0.,1.,0.));
#35224=DIRECTION('center_axis',(0.,-1.,0.));
#35225=DIRECTION('ref_axis',(0.653824539037156,0.,-0.756646200117896));
#35226=DIRECTION('',(0.,1.,0.));
#35227=DIRECTION('center_axis',(0.,-1.,0.));
#35228=DIRECTION('ref_axis',(0.653824539037156,0.,-0.756646200117896));
#35229=DIRECTION('',(0.,1.,0.));
#35230=DIRECTION('center_axis',(0.,-1.,0.));
#35231=DIRECTION('ref_axis',(0.653824539037156,0.,-0.756646200117896));
#35232=DIRECTION('',(0.,1.,0.));
#35233=DIRECTION('center_axis',(0.,-1.,0.));
#35234=DIRECTION('ref_axis',(0.653824539037156,0.,-0.756646200117896));
#35235=DIRECTION('',(0.,1.,0.));
#35236=DIRECTION('center_axis',(0.,-1.,0.));
#35237=DIRECTION('ref_axis',(0.653824539037156,0.,-0.756646200117896));
#35238=DIRECTION('',(0.,1.,0.));
#35239=DIRECTION('center_axis',(0.,-1.,0.));
#35240=DIRECTION('ref_axis',(0.653824539037156,0.,-0.756646200117896));
#35241=DIRECTION('',(0.,1.,0.));
#35242=DIRECTION('center_axis',(0.,-1.,0.));
#35243=DIRECTION('ref_axis',(1.,0.,0.));
#35244=DIRECTION('center_axis',(0.,1.,0.));
#35245=DIRECTION('ref_axis',(1.,0.,0.));
#35246=DIRECTION('center_axis',(0.,-1.,0.));
#35247=DIRECTION('ref_axis',(1.,0.,0.));
#35248=DIRECTION('center_axis',(0.,-1.,0.));
#35249=DIRECTION('ref_axis',(0.653824539037156,0.,-0.756646200117896));
#35250=DIRECTION('center_axis',(0.,-1.,0.));
#35251=DIRECTION('ref_axis',(1.,0.,1.17141641968325E-13));
#35252=DIRECTION('center_axis',(0.,1.,0.));
#35253=DIRECTION('ref_axis',(0.,0.,1.));
#35254=DIRECTION('center_axis',(0.,-1.,0.));
#35255=DIRECTION('ref_axis',(1.,0.,0.));
#35256=DIRECTION('center_axis',(0.,-1.,0.));
#35257=DIRECTION('ref_axis',(1.,0.,0.));
#35258=DIRECTION('center_axis',(0.,1.,0.));
#35259=DIRECTION('ref_axis',(0.,0.,1.));
#35260=DIRECTION('center_axis',(0.,1.,0.));
#35261=DIRECTION('ref_axis',(1.,0.,0.));
#35262=DIRECTION('center_axis',(0.,1.,0.));
#35263=DIRECTION('ref_axis',(1.,0.,0.));
#35264=DIRECTION('center_axis',(0.,1.,0.));
#35265=DIRECTION('ref_axis',(0.,0.,1.));
#35266=DIRECTION('center_axis',(0.,-1.,0.));
#35267=DIRECTION('ref_axis',(1.,0.,0.));
#35268=DIRECTION('center_axis',(1.,0.,0.));
#35269=DIRECTION('ref_axis',(0.,0.,-1.));
#35270=DIRECTION('center_axis',(0.,1.,0.));
#35271=DIRECTION('ref_axis',(1.,0.,0.));
#35272=DIRECTION('center_axis',(0.,1.,0.));
#35273=DIRECTION('ref_axis',(1.,0.,0.));
#35274=DIRECTION('center_axis',(0.,1.,0.));
#35275=DIRECTION('ref_axis',(1.,0.,0.));
#35276=DIRECTION('',(0.707106781186547,-0.707106781186548,-8.65956056235493E-17));
#35277=DIRECTION('center_axis',(0.,1.,0.));
#35278=DIRECTION('ref_axis',(1.,0.,0.));
#35279=DIRECTION('center_axis',(0.,1.,0.));
#35280=DIRECTION('ref_axis',(1.,0.,0.));
#35281=DIRECTION('center_axis',(-0.188314866426199,0.,0.982108706347155));
#35282=DIRECTION('ref_axis',(-0.982108706347155,0.,-0.188314866426199));
#35283=DIRECTION('',(0.,1.,0.));
#35284=DIRECTION('',(-0.982108706347155,0.,-0.188314866426199));
#35285=DIRECTION('',(0.,-1.,0.));
#35286=DIRECTION('center_axis',(-0.512859050871225,0.,-0.858472826558573));
#35287=DIRECTION('ref_axis',(0.858472826558573,0.,-0.512859050871225));
#35288=DIRECTION('',(0.,-1.,0.));
#35289=DIRECTION('',(0.858472826558573,0.,-0.512859050871225));
#35290=DIRECTION('center_axis',(0.,-1.,0.));
#35291=DIRECTION('ref_axis',(-0.17364817766693,0.,-0.984807753012208));
#35292=DIRECTION('center_axis',(0.,-1.,0.));
#35293=DIRECTION('ref_axis',(1.,0.,0.));
#35294=DIRECTION('center_axis',(0.,-1.,0.));
#35295=DIRECTION('ref_axis',(1.,0.,0.));
#35296=DIRECTION('center_axis',(0.,1.,0.));
#35297=DIRECTION('ref_axis',(1.,0.,0.));
#35298=DIRECTION('center_axis',(0.,1.,0.));
#35299=DIRECTION('ref_axis',(1.,0.,0.));
#35300=DIRECTION('center_axis',(0.,1.,0.));
#35301=DIRECTION('ref_axis',(1.,0.,0.));
#35302=DIRECTION('center_axis',(0.,1.,0.));
#35303=DIRECTION('ref_axis',(1.,0.,0.));
#35304=DIRECTION('center_axis',(0.,1.,0.));
#35305=DIRECTION('ref_axis',(1.,0.,0.));
#35306=DIRECTION('center_axis',(0.,1.,0.));
#35307=DIRECTION('ref_axis',(1.,0.,0.));
#35308=DIRECTION('center_axis',(0.,1.,0.));
#35309=DIRECTION('ref_axis',(1.,0.,0.));
#35310=DIRECTION('center_axis',(0.,1.,0.));
#35311=DIRECTION('ref_axis',(1.,0.,0.));
#35312=DIRECTION('center_axis',(0.,1.,0.));
#35313=DIRECTION('ref_axis',(1.,0.,0.));
#35314=DIRECTION('center_axis',(0.,1.,0.));
#35315=DIRECTION('ref_axis',(1.,0.,0.));
#35316=DIRECTION('center_axis',(0.,1.,0.));
#35317=DIRECTION('ref_axis',(1.,0.,0.));
#35318=DIRECTION('center_axis',(0.,1.,0.));
#35319=DIRECTION('ref_axis',(1.,0.,0.));
#35320=DIRECTION('center_axis',(0.,1.,0.));
#35321=DIRECTION('ref_axis',(1.,0.,0.));
#35322=DIRECTION('center_axis',(0.,1.,0.));
#35323=DIRECTION('ref_axis',(1.,0.,0.));
#35324=DIRECTION('center_axis',(0.,1.,0.));
#35325=DIRECTION('ref_axis',(1.,0.,0.));
#35326=DIRECTION('center_axis',(0.,1.,0.));
#35327=DIRECTION('ref_axis',(1.,0.,0.));
#35328=DIRECTION('center_axis',(0.,1.,0.));
#35329=DIRECTION('ref_axis',(1.,0.,0.));
#35330=DIRECTION('center_axis',(0.,1.,0.));
#35331=DIRECTION('ref_axis',(1.,0.,0.));
#35332=DIRECTION('center_axis',(0.,1.,0.));
#35333=DIRECTION('ref_axis',(1.,0.,0.));
#35334=DIRECTION('center_axis',(0.,1.,0.));
#35335=DIRECTION('ref_axis',(1.,0.,0.));
#35336=DIRECTION('center_axis',(0.,1.,0.));
#35337=DIRECTION('ref_axis',(1.,0.,0.));
#35338=DIRECTION('center_axis',(0.,1.,0.));
#35339=DIRECTION('ref_axis',(1.,0.,0.));
#35340=DIRECTION('center_axis',(0.,1.,0.));
#35341=DIRECTION('ref_axis',(1.,0.,0.));
#35342=DIRECTION('center_axis',(0.,1.,0.));
#35343=DIRECTION('ref_axis',(1.,0.,0.));
#35344=DIRECTION('center_axis',(0.,1.,0.));
#35345=DIRECTION('ref_axis',(1.,0.,0.));
#35346=DIRECTION('center_axis',(0.,1.,0.));
#35347=DIRECTION('ref_axis',(1.,0.,0.));
#35348=DIRECTION('center_axis',(0.,1.,0.));
#35349=DIRECTION('ref_axis',(1.,0.,0.));
#35350=DIRECTION('center_axis',(0.,1.,0.));
#35351=DIRECTION('ref_axis',(1.,0.,0.));
#35352=DIRECTION('center_axis',(0.,1.,0.));
#35353=DIRECTION('ref_axis',(1.,0.,0.));
#35354=DIRECTION('center_axis',(0.,1.,0.));
#35355=DIRECTION('ref_axis',(1.,0.,0.));
#35356=DIRECTION('center_axis',(0.,1.,0.));
#35357=DIRECTION('ref_axis',(1.,0.,0.));
#35358=DIRECTION('center_axis',(0.,1.,0.));
#35359=DIRECTION('ref_axis',(1.,0.,0.));
#35360=DIRECTION('center_axis',(0.,1.,0.));
#35361=DIRECTION('ref_axis',(1.,0.,0.));
#35362=DIRECTION('center_axis',(0.,1.,0.));
#35363=DIRECTION('ref_axis',(1.,0.,0.));
#35364=DIRECTION('center_axis',(0.,1.,0.));
#35365=DIRECTION('ref_axis',(1.,0.,0.));
#35366=DIRECTION('center_axis',(0.,1.,0.));
#35367=DIRECTION('ref_axis',(1.,0.,0.));
#35368=DIRECTION('',(0.707106781186537,0.707106781186558,8.65956056235481E-17));
#35369=DIRECTION('center_axis',(0.,-1.,0.));
#35370=DIRECTION('ref_axis',(1.,0.,0.));
#35371=DIRECTION('center_axis',(-0.0149125533359689,0.,0.999888801693969));
#35372=DIRECTION('ref_axis',(-0.999888801693969,0.,-0.0149125533359689));
#35373=DIRECTION('',(0.,1.,0.));
#35374=DIRECTION('',(-0.999888801693969,0.,-0.0149125533359689));
#35375=DIRECTION('',(0.,-1.,0.));
#35376=DIRECTION('center_axis',(-0.65413981140894,0.,-0.756373655761408));
#35377=DIRECTION('ref_axis',(0.756373655761408,0.,-0.65413981140894));
#35378=DIRECTION('',(0.,-1.,0.));
#35379=DIRECTION('',(0.756373655761408,0.,-0.65413981140894));
#35380=DIRECTION('center_axis',(0.,-1.,0.));
#35381=DIRECTION('ref_axis',(-0.342020143325669,0.,-0.939692620785908));
#35382=DIRECTION('center_axis',(0.,-1.,0.));
#35383=DIRECTION('ref_axis',(1.,0.,0.));
#35384=DIRECTION('center_axis',(0.158942870141258,0.,0.987287781769459));
#35385=DIRECTION('ref_axis',(-0.987287781769459,0.,0.158942870141258));
#35386=DIRECTION('',(0.,1.,0.));
#35387=DIRECTION('',(-0.987287781769459,0.,0.158942870141258));
#35388=DIRECTION('',(0.,-1.,0.));
#35389=DIRECTION('center_axis',(-0.77554486478771,0.,-0.631292454177469));
#35390=DIRECTION('ref_axis',(0.631292454177469,0.,-0.77554486478771));
#35391=DIRECTION('',(0.,-1.,0.));
#35392=DIRECTION('',(0.631292454177469,0.,-0.77554486478771));
#35393=DIRECTION('center_axis',(0.,-1.,0.));
#35394=DIRECTION('ref_axis',(-0.5,0.,-0.866025403784438));
#35395=DIRECTION('center_axis',(0.,-1.,0.));
#35396=DIRECTION('ref_axis',(1.,0.,0.));
#35397=DIRECTION('center_axis',(0.327968894938216,0.,0.944688522187607));
#35398=DIRECTION('ref_axis',(-0.944688522187607,0.,0.327968894938216));
#35399=DIRECTION('',(0.,1.,0.));
#35400=DIRECTION('',(-0.944688522187607,0.,0.327968894938216));
#35401=DIRECTION('',(0.,-1.,0.));
#35402=DIRECTION('center_axis',(-0.873385379894543,0.,-0.487029750822744));
#35403=DIRECTION('ref_axis',(0.487029750822744,0.,-0.873385379894543));
#35404=DIRECTION('',(0.,-1.,0.));
#35405=DIRECTION('',(0.487029750822744,0.,-0.873385379894543));
#35406=DIRECTION('center_axis',(0.,-1.,0.));
#35407=DIRECTION('ref_axis',(-0.64278760968654,0.,-0.766044443118978));
#35408=DIRECTION('center_axis',(0.,-1.,0.));
#35409=DIRECTION('ref_axis',(1.,0.,0.));
#35410=DIRECTION('center_axis',(0.487029750822745,0.,0.873385379894543));
#35411=DIRECTION('ref_axis',(-0.873385379894543,0.,0.487029750822745));
#35412=DIRECTION('',(0.,1.,0.));
#35413=DIRECTION('',(-0.873385379894543,0.,0.487029750822745));
#35414=DIRECTION('',(0.,-1.,0.));
#35415=DIRECTION('center_axis',(-0.944688522187607,0.,-0.327968894938216));
#35416=DIRECTION('ref_axis',(0.327968894938216,0.,-0.944688522187607));
#35417=DIRECTION('',(0.,-1.,0.));
#35418=DIRECTION('',(0.327968894938216,0.,-0.944688522187607));
#35419=DIRECTION('center_axis',(0.,-1.,0.));
#35420=DIRECTION('ref_axis',(-0.766044443118978,0.,-0.642787609686539));
#35421=DIRECTION('center_axis',(0.,-1.,0.));
#35422=DIRECTION('ref_axis',(1.,0.,0.));
#35423=DIRECTION('center_axis',(0.63129245417747,0.,0.77554486478771));
#35424=DIRECTION('ref_axis',(-0.77554486478771,0.,0.63129245417747));
#35425=DIRECTION('',(0.,1.,0.));
#35426=DIRECTION('',(-0.77554486478771,0.,0.63129245417747));
#35427=DIRECTION('',(0.,-1.,0.));
#35428=DIRECTION('center_axis',(-0.987287781769459,0.,-0.158942870141258));
#35429=DIRECTION('ref_axis',(0.158942870141258,0.,-0.987287781769459));
#35430=DIRECTION('',(0.,-1.,0.));
#35431=DIRECTION('',(0.158942870141258,0.,-0.987287781769459));
#35432=DIRECTION('center_axis',(0.,-1.,0.));
#35433=DIRECTION('ref_axis',(-0.866025403784439,0.,-0.5));
#35434=DIRECTION('center_axis',(0.,-1.,0.));
#35435=DIRECTION('ref_axis',(1.,0.,0.));
#35436=DIRECTION('center_axis',(0.756373655761408,0.,0.654139811408939));
#35437=DIRECTION('ref_axis',(-0.654139811408939,0.,0.756373655761408));
#35438=DIRECTION('',(0.,1.,0.));
#35439=DIRECTION('',(-0.654139811408939,0.,0.756373655761408));
#35440=DIRECTION('',(0.,-1.,0.));
#35441=DIRECTION('center_axis',(-0.999888801693969,0.,0.0149125533359702));
#35442=DIRECTION('ref_axis',(-0.0149125533359702,0.,-0.999888801693969));
#35443=DIRECTION('',(0.,-1.,0.));
#35444=DIRECTION('',(-0.0149125533359701,0.,-0.999888801693969));
#35445=DIRECTION('center_axis',(0.,-1.,0.));
#35446=DIRECTION('ref_axis',(-0.939692620785909,0.,-0.342020143325668));
#35447=DIRECTION('center_axis',(0.,-1.,0.));
#35448=DIRECTION('ref_axis',(1.,0.,0.));
#35449=DIRECTION('center_axis',(0.858472826558574,0.,0.512859050871224));
#35450=DIRECTION('ref_axis',(-0.512859050871224,0.,0.858472826558574));
#35451=DIRECTION('',(0.,1.,0.));
#35452=DIRECTION('',(-0.512859050871224,0.,0.858472826558574));
#35453=DIRECTION('',(0.,-1.,0.));
#35454=DIRECTION('center_axis',(-0.982108706347155,0.,0.1883148664262));
#35455=DIRECTION('ref_axis',(-0.1883148664262,0.,-0.982108706347155));
#35456=DIRECTION('',(0.,-1.,0.));
#35457=DIRECTION('',(-0.1883148664262,0.,-0.982108706347155));
#35458=DIRECTION('center_axis',(0.,-1.,0.));
#35459=DIRECTION('ref_axis',(-0.984807753012208,0.,-0.17364817766693));
#35460=DIRECTION('center_axis',(0.,-1.,0.));
#35461=DIRECTION('ref_axis',(1.,0.,0.));
#35462=DIRECTION('center_axis',(0.934487734928968,0.,0.355995327591989));
#35463=DIRECTION('ref_axis',(-0.355995327591989,0.,0.934487734928968));
#35464=DIRECTION('',(0.,1.,0.));
#35465=DIRECTION('',(-0.355995327591989,0.,0.934487734928968));
#35466=DIRECTION('',(0.,-1.,0.));
#35467=DIRECTION('center_axis',(-0.934487734928967,0.,0.35599532759199));
#35468=DIRECTION('ref_axis',(-0.35599532759199,0.,-0.934487734928967));
#35469=DIRECTION('',(0.,-1.,0.));
#35470=DIRECTION('',(-0.35599532759199,0.,-0.934487734928967));
#35471=DIRECTION('center_axis',(0.,-1.,0.));
#35472=DIRECTION('ref_axis',(-1.,0.,1.83697019872103E-16));
#35473=DIRECTION('center_axis',(0.,-1.,0.));
#35474=DIRECTION('ref_axis',(1.,0.,0.));
#35475=DIRECTION('center_axis',(0.982108706347155,0.,0.188314866426199));
#35476=DIRECTION('ref_axis',(-0.188314866426199,0.,0.982108706347155));
#35477=DIRECTION('',(0.,1.,0.));
#35478=DIRECTION('',(-0.188314866426199,0.,0.982108706347155));
#35479=DIRECTION('',(0.,-1.,0.));
#35480=DIRECTION('center_axis',(-0.858472826558574,0.,0.512859050871225));
#35481=DIRECTION('ref_axis',(-0.512859050871225,0.,-0.858472826558573));
#35482=DIRECTION('',(0.,-1.,0.));
#35483=DIRECTION('',(-0.512859050871225,0.,-0.858472826558573));
#35484=DIRECTION('center_axis',(0.,-1.,0.));
#35485=DIRECTION('ref_axis',(-0.984807753012208,0.,0.17364817766693));
#35486=DIRECTION('center_axis',(0.,-1.,0.));
#35487=DIRECTION('ref_axis',(1.,0.,0.));
#35488=DIRECTION('center_axis',(0.999888801693969,0.,0.0149125533359689));
#35489=DIRECTION('ref_axis',(-0.0149125533359689,0.,0.999888801693969));
#35490=DIRECTION('',(0.,1.,0.));
#35491=DIRECTION('',(-0.0149125533359689,0.,0.999888801693969));
#35492=DIRECTION('',(0.,-1.,0.));
#35493=DIRECTION('center_axis',(-0.756373655761408,0.,0.65413981140894));
#35494=DIRECTION('ref_axis',(-0.65413981140894,0.,-0.756373655761408));
#35495=DIRECTION('',(0.,-1.,0.));
#35496=DIRECTION('',(-0.65413981140894,0.,-0.756373655761408));
#35497=DIRECTION('center_axis',(0.,-1.,0.));
#35498=DIRECTION('ref_axis',(-0.939692620785908,0.,0.342020143325669));
#35499=DIRECTION('center_axis',(0.,-1.,0.));
#35500=DIRECTION('ref_axis',(1.,0.,0.));
#35501=DIRECTION('center_axis',(0.987287781769459,0.,-0.158942870141258));
#35502=DIRECTION('ref_axis',(0.158942870141258,0.,0.987287781769459));
#35503=DIRECTION('',(0.,1.,0.));
#35504=DIRECTION('',(0.158942870141258,0.,0.987287781769459));
#35505=DIRECTION('',(0.,-1.,0.));
#35506=DIRECTION('center_axis',(-0.631292454177469,0.,0.77554486478771));
#35507=DIRECTION('ref_axis',(-0.77554486478771,0.,-0.631292454177469));
#35508=DIRECTION('',(0.,-1.,0.));
#35509=DIRECTION('',(-0.77554486478771,0.,-0.631292454177469));
#35510=DIRECTION('center_axis',(0.,-1.,0.));
#35511=DIRECTION('ref_axis',(-0.866025403784438,0.,0.5));
#35512=DIRECTION('center_axis',(0.,-1.,0.));
#35513=DIRECTION('ref_axis',(1.,0.,0.));
#35514=DIRECTION('center_axis',(0.944688522187607,0.,-0.327968894938216));
#35515=DIRECTION('ref_axis',(0.327968894938216,0.,0.944688522187607));
#35516=DIRECTION('',(0.,1.,0.));
#35517=DIRECTION('',(0.327968894938216,0.,0.944688522187607));
#35518=DIRECTION('',(0.,-1.,0.));
#35519=DIRECTION('center_axis',(-0.487029750822744,0.,0.873385379894543));
#35520=DIRECTION('ref_axis',(-0.873385379894543,0.,-0.487029750822744));
#35521=DIRECTION('',(0.,-1.,0.));
#35522=DIRECTION('',(-0.873385379894543,0.,-0.487029750822744));
#35523=DIRECTION('center_axis',(0.,-1.,0.));
#35524=DIRECTION('ref_axis',(-0.766044443118978,0.,0.642787609686539));
#35525=DIRECTION('center_axis',(0.,-1.,0.));
#35526=DIRECTION('ref_axis',(1.,0.,0.));
#35527=DIRECTION('center_axis',(0.873385379894543,0.,-0.487029750822745));
#35528=DIRECTION('ref_axis',(0.487029750822745,0.,0.873385379894543));
#35529=DIRECTION('',(0.,1.,0.));
#35530=DIRECTION('',(0.487029750822745,0.,0.873385379894543));
#35531=DIRECTION('',(0.,-1.,0.));
#35532=DIRECTION('center_axis',(-0.327968894938216,0.,0.944688522187607));
#35533=DIRECTION('ref_axis',(-0.944688522187607,0.,-0.327968894938216));
#35534=DIRECTION('',(0.,-1.,0.));
#35535=DIRECTION('',(-0.944688522187607,0.,-0.327968894938216));
#35536=DIRECTION('center_axis',(0.,-1.,0.));
#35537=DIRECTION('ref_axis',(-0.642787609686539,0.,0.766044443118978));
#35538=DIRECTION('center_axis',(0.,-1.,0.));
#35539=DIRECTION('ref_axis',(1.,0.,0.));
#35540=DIRECTION('center_axis',(0.77554486478771,0.,-0.63129245417747));
#35541=DIRECTION('ref_axis',(0.63129245417747,0.,0.77554486478771));
#35542=DIRECTION('',(0.,1.,0.));
#35543=DIRECTION('',(0.63129245417747,0.,0.77554486478771));
#35544=DIRECTION('',(0.,-1.,0.));
#35545=DIRECTION('center_axis',(-0.158942870141257,0.,0.987287781769459));
#35546=DIRECTION('ref_axis',(-0.987287781769459,0.,-0.158942870141257));
#35547=DIRECTION('',(0.,-1.,0.));
#35548=DIRECTION('',(-0.987287781769459,0.,-0.158942870141257));
#35549=DIRECTION('center_axis',(0.,-1.,0.));
#35550=DIRECTION('ref_axis',(-0.5,0.,0.866025403784439));
#35551=DIRECTION('center_axis',(0.,-1.,0.));
#35552=DIRECTION('ref_axis',(1.,0.,0.));
#35553=DIRECTION('center_axis',(0.65413981140894,0.,-0.756373655761408));
#35554=DIRECTION('ref_axis',(0.756373655761408,0.,0.65413981140894));
#35555=DIRECTION('',(0.,1.,0.));
#35556=DIRECTION('',(0.756373655761408,0.,0.65413981140894));
#35557=DIRECTION('',(0.,-1.,0.));
#35558=DIRECTION('center_axis',(0.0149125533359697,0.,0.999888801693969));
#35559=DIRECTION('ref_axis',(-0.999888801693969,0.,0.0149125533359697));
#35560=DIRECTION('',(0.,-1.,0.));
#35561=DIRECTION('',(-0.999888801693969,0.,0.0149125533359697));
#35562=DIRECTION('center_axis',(0.,-1.,0.));
#35563=DIRECTION('ref_axis',(-0.342020143325669,0.,0.939692620785908));
#35564=DIRECTION('center_axis',(0.,-1.,0.));
#35565=DIRECTION('ref_axis',(1.,0.,0.));
#35566=DIRECTION('center_axis',(0.512859050871225,0.,-0.858472826558573));
#35567=DIRECTION('ref_axis',(0.858472826558573,0.,0.512859050871225));
#35568=DIRECTION('',(0.,1.,0.));
#35569=DIRECTION('',(0.858472826558574,0.,0.512859050871224));
#35570=DIRECTION('',(0.,-1.,0.));
#35571=DIRECTION('center_axis',(0.1883148664262,0.,0.982108706347155));
#35572=DIRECTION('ref_axis',(-0.982108706347155,0.,0.1883148664262));
#35573=DIRECTION('',(0.,-1.,0.));
#35574=DIRECTION('',(-0.982108706347155,0.,0.1883148664262));
#35575=DIRECTION('center_axis',(0.,-1.,0.));
#35576=DIRECTION('ref_axis',(-0.17364817766693,0.,0.984807753012208));
#35577=DIRECTION('center_axis',(0.,-1.,0.));
#35578=DIRECTION('ref_axis',(1.,0.,0.));
#35579=DIRECTION('center_axis',(0.355995327591989,0.,-0.934487734928968));
#35580=DIRECTION('ref_axis',(0.934487734928968,0.,0.355995327591989));
#35581=DIRECTION('',(0.,1.,0.));
#35582=DIRECTION('',(0.934487734928968,0.,0.355995327591989));
#35583=DIRECTION('',(0.,-1.,0.));
#35584=DIRECTION('center_axis',(0.35599532759199,0.,0.934487734928967));
#35585=DIRECTION('ref_axis',(-0.934487734928967,0.,0.35599532759199));
#35586=DIRECTION('',(0.,-1.,0.));
#35587=DIRECTION('',(-0.934487734928967,0.,0.35599532759199));
#35588=DIRECTION('center_axis',(0.,-1.,0.));
#35589=DIRECTION('ref_axis',(1.22464679914735E-16,0.,1.));
#35590=DIRECTION('center_axis',(0.,-1.,0.));
#35591=DIRECTION('ref_axis',(1.,0.,0.));
#35592=DIRECTION('center_axis',(0.,-1.,0.));
#35593=DIRECTION('ref_axis',(1.,0.,0.));
#35594=DIRECTION('center_axis',(0.188314866426199,0.,-0.982108706347155));
#35595=DIRECTION('ref_axis',(0.982108706347155,0.,0.188314866426199));
#35596=DIRECTION('',(0.,1.,0.));
#35597=DIRECTION('',(0.982108706347155,0.,0.188314866426199));
#35598=DIRECTION('',(0.,-1.,0.));
#35599=DIRECTION('center_axis',(0.512859050871225,0.,0.858472826558573));
#35600=DIRECTION('ref_axis',(-0.858472826558573,0.,0.512859050871225));
#35601=DIRECTION('',(0.,-1.,0.));
#35602=DIRECTION('',(-0.858472826558573,0.,0.512859050871225));
#35603=DIRECTION('center_axis',(0.,-1.,0.));
#35604=DIRECTION('ref_axis',(0.173648177666931,0.,0.984807753012208));
#35605=DIRECTION('center_axis',(0.,-1.,0.));
#35606=DIRECTION('ref_axis',(1.,0.,0.));
#35607=DIRECTION('center_axis',(0.0149125533359694,0.,-0.999888801693969));
#35608=DIRECTION('ref_axis',(0.999888801693969,0.,0.0149125533359694));
#35609=DIRECTION('',(0.,1.,0.));
#35610=DIRECTION('',(0.999888801693969,0.,0.0149125533359694));
#35611=DIRECTION('',(0.,-1.,0.));
#35612=DIRECTION('center_axis',(0.65413981140894,0.,0.756373655761408));
#35613=DIRECTION('ref_axis',(-0.756373655761408,0.,0.65413981140894));
#35614=DIRECTION('',(0.,-1.,0.));
#35615=DIRECTION('',(-0.756373655761408,0.,0.65413981140894));
#35616=DIRECTION('center_axis',(0.,-1.,0.));
#35617=DIRECTION('ref_axis',(0.342020143325669,0.,0.939692620785908));
#35618=DIRECTION('center_axis',(0.,-1.,0.));
#35619=DIRECTION('ref_axis',(1.,0.,0.));
#35620=DIRECTION('center_axis',(-0.158942870141257,0.,-0.987287781769459));
#35621=DIRECTION('ref_axis',(0.987287781769459,0.,-0.158942870141257));
#35622=DIRECTION('',(0.,1.,0.));
#35623=DIRECTION('',(0.987287781769459,0.,-0.158942870141257));
#35624=DIRECTION('',(0.,-1.,0.));
#35625=DIRECTION('center_axis',(0.77554486478771,0.,0.63129245417747));
#35626=DIRECTION('ref_axis',(-0.63129245417747,0.,0.77554486478771));
#35627=DIRECTION('',(0.,-1.,0.));
#35628=DIRECTION('',(-0.63129245417747,0.,0.77554486478771));
#35629=DIRECTION('center_axis',(0.,-1.,0.));
#35630=DIRECTION('ref_axis',(0.5,0.,0.866025403784439));
#35631=DIRECTION('center_axis',(0.,-1.,0.));
#35632=DIRECTION('ref_axis',(1.,0.,0.));
#35633=DIRECTION('center_axis',(-0.327968894938216,0.,-0.944688522187607));
#35634=DIRECTION('ref_axis',(0.944688522187607,0.,-0.327968894938216));
#35635=DIRECTION('',(0.,1.,0.));
#35636=DIRECTION('',(0.944688522187607,0.,-0.327968894938216));
#35637=DIRECTION('',(0.,-1.,0.));
#35638=DIRECTION('center_axis',(0.873385379894543,0.,0.487029750822744));
#35639=DIRECTION('ref_axis',(-0.487029750822744,0.,0.873385379894543));
#35640=DIRECTION('',(0.,-1.,0.));
#35641=DIRECTION('',(-0.487029750822744,0.,0.873385379894543));
#35642=DIRECTION('center_axis',(0.,-1.,0.));
#35643=DIRECTION('ref_axis',(0.642787609686539,0.,0.766044443118978));
#35644=DIRECTION('center_axis',(0.,-1.,0.));
#35645=DIRECTION('ref_axis',(1.,0.,0.));
#35646=DIRECTION('center_axis',(-0.487029750822745,0.,-0.873385379894543));
#35647=DIRECTION('ref_axis',(0.873385379894543,0.,-0.487029750822745));
#35648=DIRECTION('',(0.,1.,0.));
#35649=DIRECTION('',(0.873385379894543,0.,-0.487029750822745));
#35650=DIRECTION('',(0.,-1.,0.));
#35651=DIRECTION('center_axis',(0.944688522187607,0.,0.327968894938216));
#35652=DIRECTION('ref_axis',(-0.327968894938216,0.,0.944688522187607));
#35653=DIRECTION('',(0.,-1.,0.));
#35654=DIRECTION('',(-0.327968894938216,0.,0.944688522187607));
#35655=DIRECTION('center_axis',(0.,-1.,0.));
#35656=DIRECTION('ref_axis',(0.766044443118978,0.,0.642787609686539));
#35657=DIRECTION('center_axis',(0.,-1.,0.));
#35658=DIRECTION('ref_axis',(1.,0.,0.));
#35659=DIRECTION('center_axis',(-0.63129245417747,0.,-0.77554486478771));
#35660=DIRECTION('ref_axis',(0.77554486478771,0.,-0.63129245417747));
#35661=DIRECTION('',(0.,1.,0.));
#35662=DIRECTION('',(0.77554486478771,0.,-0.63129245417747));
#35663=DIRECTION('',(0.,-1.,0.));
#35664=DIRECTION('center_axis',(0.987287781769459,0.,0.158942870141257));
#35665=DIRECTION('ref_axis',(-0.158942870141257,0.,0.987287781769459));
#35666=DIRECTION('',(0.,-1.,0.));
#35667=DIRECTION('',(-0.158942870141257,0.,0.987287781769459));
#35668=DIRECTION('center_axis',(0.,-1.,0.));
#35669=DIRECTION('ref_axis',(0.866025403784439,0.,0.5));
#35670=DIRECTION('center_axis',(0.,-1.,0.));
#35671=DIRECTION('ref_axis',(1.,0.,0.));
#35672=DIRECTION('center_axis',(-0.756373655761408,0.,-0.65413981140894));
#35673=DIRECTION('ref_axis',(0.65413981140894,0.,-0.756373655761408));
#35674=DIRECTION('',(0.,1.,0.));
#35675=DIRECTION('',(0.65413981140894,0.,-0.756373655761408));
#35676=DIRECTION('',(0.,-1.,0.));
#35677=DIRECTION('center_axis',(0.999888801693969,0.,-0.0149125533359696));
#35678=DIRECTION('ref_axis',(0.0149125533359696,0.,0.999888801693969));
#35679=DIRECTION('',(0.,-1.,0.));
#35680=DIRECTION('',(0.0149125533359696,0.,0.999888801693969));
#35681=DIRECTION('center_axis',(0.,-1.,0.));
#35682=DIRECTION('ref_axis',(0.939692620785908,0.,0.342020143325669));
#35683=DIRECTION('center_axis',(0.,-1.,0.));
#35684=DIRECTION('ref_axis',(1.,0.,0.));
#35685=DIRECTION('center_axis',(-0.858472826558574,0.,-0.512859050871225));
#35686=DIRECTION('ref_axis',(0.512859050871225,0.,-0.858472826558573));
#35687=DIRECTION('',(0.,1.,0.));
#35688=DIRECTION('',(0.512859050871225,0.,-0.858472826558573));
#35689=DIRECTION('',(0.,-1.,0.));
#35690=DIRECTION('center_axis',(0.982108706347155,0.,-0.188314866426199));
#35691=DIRECTION('ref_axis',(0.188314866426199,0.,0.982108706347155));
#35692=DIRECTION('',(0.,-1.,0.));
#35693=DIRECTION('',(0.188314866426199,0.,0.982108706347155));
#35694=DIRECTION('center_axis',(0.,-1.,0.));
#35695=DIRECTION('ref_axis',(0.984807753012208,0.,0.17364817766693));
#35696=DIRECTION('center_axis',(0.,-1.,0.));
#35697=DIRECTION('ref_axis',(1.,0.,0.));
#35698=DIRECTION('center_axis',(-0.934487734928968,0.,-0.355995327591989));
#35699=DIRECTION('ref_axis',(0.355995327591989,0.,-0.934487734928968));
#35700=DIRECTION('',(0.,1.,0.));
#35701=DIRECTION('',(0.355995327591989,0.,-0.934487734928968));
#35702=DIRECTION('',(0.,-1.,0.));
#35703=DIRECTION('center_axis',(0.934487734928967,0.,-0.35599532759199));
#35704=DIRECTION('ref_axis',(0.35599532759199,0.,0.934487734928967));
#35705=DIRECTION('',(0.,-1.,0.));
#35706=DIRECTION('',(0.355995327591989,0.,0.934487734928968));
#35707=DIRECTION('center_axis',(0.,-1.,0.));
#35708=DIRECTION('ref_axis',(1.,0.,-6.12323399573677E-17));
#35709=DIRECTION('center_axis',(0.,-1.,0.));
#35710=DIRECTION('ref_axis',(1.,0.,0.));
#35711=DIRECTION('center_axis',(-0.982108706347155,0.,-0.188314866426199));
#35712=DIRECTION('ref_axis',(0.188314866426199,0.,-0.982108706347155));
#35713=DIRECTION('',(0.,1.,0.));
#35714=DIRECTION('',(0.188314866426199,0.,-0.982108706347155));
#35715=DIRECTION('',(0.,-1.,0.));
#35716=DIRECTION('center_axis',(0.858472826558573,0.,-0.512859050871225));
#35717=DIRECTION('ref_axis',(0.512859050871225,0.,0.858472826558573));
#35718=DIRECTION('',(0.,-1.,0.));
#35719=DIRECTION('',(0.512859050871225,0.,0.858472826558573));
#35720=DIRECTION('center_axis',(0.,-1.,0.));
#35721=DIRECTION('ref_axis',(0.984807753012208,0.,-0.17364817766693));
#35722=DIRECTION('center_axis',(0.,-1.,0.));
#35723=DIRECTION('ref_axis',(1.,0.,0.));
#35724=DIRECTION('center_axis',(-0.999888801693969,0.,-0.0149125533359695));
#35725=DIRECTION('ref_axis',(0.0149125533359695,0.,-0.999888801693969));
#35726=DIRECTION('',(0.,1.,0.));
#35727=DIRECTION('',(0.0149125533359695,0.,-0.999888801693969));
#35728=DIRECTION('',(0.,-1.,0.));
#35729=DIRECTION('center_axis',(0.756373655761408,0.,-0.65413981140894));
#35730=DIRECTION('ref_axis',(0.65413981140894,0.,0.756373655761408));
#35731=DIRECTION('',(0.,-1.,0.));
#35732=DIRECTION('',(0.65413981140894,0.,0.756373655761408));
#35733=DIRECTION('center_axis',(0.,-1.,0.));
#35734=DIRECTION('ref_axis',(0.939692620785908,0.,-0.342020143325669));
#35735=DIRECTION('center_axis',(0.,-1.,0.));
#35736=DIRECTION('ref_axis',(1.,0.,0.));
#35737=DIRECTION('center_axis',(-0.987287781769459,0.,0.158942870141258));
#35738=DIRECTION('ref_axis',(-0.158942870141258,0.,-0.987287781769459));
#35739=DIRECTION('',(0.,1.,0.));
#35740=DIRECTION('',(-0.158942870141258,0.,-0.987287781769459));
#35741=DIRECTION('',(0.,-1.,0.));
#35742=DIRECTION('center_axis',(0.63129245417747,0.,-0.77554486478771));
#35743=DIRECTION('ref_axis',(0.77554486478771,0.,0.63129245417747));
#35744=DIRECTION('',(0.,-1.,0.));
#35745=DIRECTION('',(0.77554486478771,0.,0.63129245417747));
#35746=DIRECTION('center_axis',(0.,-1.,0.));
#35747=DIRECTION('ref_axis',(0.866025403784439,0.,-0.5));
#35748=DIRECTION('center_axis',(0.,-1.,0.));
#35749=DIRECTION('ref_axis',(1.,0.,0.));
#35750=DIRECTION('center_axis',(-0.944688522187607,0.,0.327968894938216));
#35751=DIRECTION('ref_axis',(-0.327968894938216,0.,-0.944688522187607));
#35752=DIRECTION('',(0.,1.,0.));
#35753=DIRECTION('',(-0.327968894938216,0.,-0.944688522187607));
#35754=DIRECTION('',(0.,-1.,0.));
#35755=DIRECTION('center_axis',(0.487029750822745,0.,-0.873385379894543));
#35756=DIRECTION('ref_axis',(0.873385379894543,0.,0.487029750822745));
#35757=DIRECTION('',(0.,-1.,0.));
#35758=DIRECTION('',(0.873385379894543,0.,0.487029750822745));
#35759=DIRECTION('center_axis',(0.,-1.,0.));
#35760=DIRECTION('ref_axis',(0.766044443118978,0.,-0.642787609686539));
#35761=DIRECTION('center_axis',(0.,-1.,0.));
#35762=DIRECTION('ref_axis',(1.,0.,0.));
#35763=DIRECTION('center_axis',(-0.873385379894543,0.,0.487029750822745));
#35764=DIRECTION('ref_axis',(-0.487029750822745,0.,-0.873385379894543));
#35765=DIRECTION('',(0.,1.,0.));
#35766=DIRECTION('',(-0.487029750822745,0.,-0.873385379894543));
#35767=DIRECTION('',(0.,-1.,0.));
#35768=DIRECTION('center_axis',(0.327968894938216,0.,-0.944688522187607));
#35769=DIRECTION('ref_axis',(0.944688522187607,0.,0.327968894938216));
#35770=DIRECTION('',(0.,-1.,0.));
#35771=DIRECTION('',(0.944688522187607,0.,0.327968894938216));
#35772=DIRECTION('center_axis',(0.,-1.,0.));
#35773=DIRECTION('ref_axis',(0.642787609686539,0.,-0.766044443118978));
#35774=DIRECTION('center_axis',(0.,-1.,0.));
#35775=DIRECTION('ref_axis',(1.,0.,0.));
#35776=DIRECTION('center_axis',(-0.77554486478771,0.,0.63129245417747));
#35777=DIRECTION('ref_axis',(-0.63129245417747,0.,-0.77554486478771));
#35778=DIRECTION('',(0.,1.,0.));
#35779=DIRECTION('',(-0.63129245417747,0.,-0.77554486478771));
#35780=DIRECTION('',(0.,-1.,0.));
#35781=DIRECTION('center_axis',(0.158942870141257,0.,-0.987287781769459));
#35782=DIRECTION('ref_axis',(0.987287781769459,0.,0.158942870141257));
#35783=DIRECTION('',(0.,-1.,0.));
#35784=DIRECTION('',(0.987287781769459,0.,0.158942870141257));
#35785=DIRECTION('center_axis',(0.,-1.,0.));
#35786=DIRECTION('ref_axis',(0.5,0.,-0.866025403784439));
#35787=DIRECTION('center_axis',(0.,-1.,0.));
#35788=DIRECTION('ref_axis',(1.,0.,0.));
#35789=DIRECTION('center_axis',(-0.65413981140894,0.,0.756373655761408));
#35790=DIRECTION('ref_axis',(-0.756373655761408,0.,-0.65413981140894));
#35791=DIRECTION('',(0.,1.,0.));
#35792=DIRECTION('',(-0.756373655761408,0.,-0.65413981140894));
#35793=DIRECTION('',(0.,-1.,0.));
#35794=DIRECTION('center_axis',(-0.0149125533359696,0.,-0.999888801693969));
#35795=DIRECTION('ref_axis',(0.999888801693969,0.,-0.0149125533359696));
#35796=DIRECTION('',(0.,-1.,0.));
#35797=DIRECTION('',(0.999888801693969,0.,-0.0149125533359696));
#35798=DIRECTION('center_axis',(0.,-1.,0.));
#35799=DIRECTION('ref_axis',(0.342020143325669,0.,-0.939692620785908));
#35800=DIRECTION('center_axis',(0.,-1.,0.));
#35801=DIRECTION('ref_axis',(1.,0.,0.));
#35802=DIRECTION('center_axis',(-0.512859050871225,0.,0.858472826558573));
#35803=DIRECTION('ref_axis',(-0.858472826558573,0.,-0.512859050871225));
#35804=DIRECTION('',(0.,1.,0.));
#35805=DIRECTION('',(-0.858472826558573,0.,-0.512859050871225));
#35806=DIRECTION('',(0.,-1.,0.));
#35807=DIRECTION('center_axis',(-0.188314866426199,0.,-0.982108706347155));
#35808=DIRECTION('ref_axis',(0.982108706347155,0.,-0.188314866426199));
#35809=DIRECTION('',(0.,-1.,0.));
#35810=DIRECTION('',(0.982108706347155,0.,-0.188314866426199));
#35811=DIRECTION('center_axis',(0.,-1.,0.));
#35812=DIRECTION('ref_axis',(0.17364817766693,0.,-0.984807753012208));
#35813=DIRECTION('center_axis',(0.,-1.,0.));
#35814=DIRECTION('ref_axis',(1.,0.,0.));
#35815=DIRECTION('center_axis',(-0.355995327591989,0.,0.934487734928968));
#35816=DIRECTION('ref_axis',(-0.934487734928968,0.,-0.355995327591989));
#35817=DIRECTION('',(0.,1.,0.));
#35818=DIRECTION('',(-0.934487734928968,0.,-0.355995327591989));
#35819=DIRECTION('',(0.,-1.,0.));
#35820=DIRECTION('center_axis',(-0.355995327591989,0.,-0.934487734928968));
#35821=DIRECTION('ref_axis',(0.934487734928968,0.,-0.355995327591989));
#35822=DIRECTION('',(0.,-1.,0.));
#35823=DIRECTION('',(0.934487734928968,0.,-0.355995327591989));
#35824=DIRECTION('center_axis',(0.,-1.,0.));
#35825=DIRECTION('ref_axis',(0.,0.,-1.));
#35826=DIRECTION('center_axis',(0.,-1.,0.));
#35827=DIRECTION('ref_axis',(1.,0.,0.));
#35828=DIRECTION('center_axis',(0.,1.,0.));
#35829=DIRECTION('ref_axis',(1.,0.,0.));
#35830=DIRECTION('',(0.,-1.,0.));
#35831=DIRECTION('center_axis',(0.,1.,0.));
#35832=DIRECTION('ref_axis',(1.,0.,0.));
#35833=DIRECTION('',(0.499999999999998,0.,-0.86602540378444));
#35834=DIRECTION('',(1.,0.,0.));
#35835=DIRECTION('',(0.500000000000006,0.,0.866025403784435));
#35836=DIRECTION('',(-0.500000000000006,0.,0.866025403784435));
#35837=DIRECTION('',(-1.,0.,0.));
#35838=DIRECTION('',(-0.499999999999998,0.,-0.86602540378444));
#35839=DIRECTION('center_axis',(0.,1.,0.));
#35840=DIRECTION('ref_axis',(0.,0.,1.));
#35841=DIRECTION('',(0.499999999999998,0.,-0.86602540378444));
#35842=DIRECTION('center_axis',(0.,-1.,0.));
#35843=DIRECTION('ref_axis',(1.,0.,0.));
#35844=DIRECTION('center_axis',(0.,1.,0.));
#35845=DIRECTION('ref_axis',(0.,0.,1.));
#35846=DIRECTION('',(1.,0.,0.));
#35847=DIRECTION('center_axis',(0.,-1.,0.));
#35848=DIRECTION('ref_axis',(1.,0.,0.));
#35849=DIRECTION('center_axis',(0.,1.,0.));
#35850=DIRECTION('ref_axis',(0.,0.,1.));
#35851=DIRECTION('',(0.500000000000006,0.,0.866025403784435));
#35852=DIRECTION('center_axis',(0.,-1.,0.));
#35853=DIRECTION('ref_axis',(1.,0.,0.));
#35854=DIRECTION('center_axis',(0.,1.,0.));
#35855=DIRECTION('ref_axis',(0.,0.,1.));
#35856=DIRECTION('',(-0.500000000000006,0.,0.866025403784435));
#35857=DIRECTION('center_axis',(0.,-1.,0.));
#35858=DIRECTION('ref_axis',(1.,0.,0.));
#35859=DIRECTION('center_axis',(0.,1.,0.));
#35860=DIRECTION('ref_axis',(0.,0.,1.));
#35861=DIRECTION('',(-1.,0.,0.));
#35862=DIRECTION('center_axis',(0.,-1.,0.));
#35863=DIRECTION('ref_axis',(1.,0.,0.));
#35864=DIRECTION('center_axis',(0.,1.,0.));
#35865=DIRECTION('ref_axis',(0.,0.,1.));
#35866=DIRECTION('',(-0.499999999999998,0.,-0.86602540378444));
#35867=DIRECTION('center_axis',(0.,-1.,0.));
#35868=DIRECTION('ref_axis',(1.,0.,0.));
#35869=DIRECTION('center_axis',(0.,1.,0.));
#35870=DIRECTION('ref_axis',(1.,0.,0.));
#35871=DIRECTION('',(-0.857167300702115,0.515038074910049,1.04972719113862E-16));
#35872=DIRECTION('center_axis',(-0.86602540378444,0.,-0.499999999999998));
#35873=DIRECTION('ref_axis',(0.499999999999998,0.,-0.86602540378444));
#35874=DIRECTION('',(0.,-1.,0.));
#35875=DIRECTION('',(0.,-1.,0.));
#35876=DIRECTION('center_axis',(-0.86602540378444,0.,0.499999999999998));
#35877=DIRECTION('ref_axis',(-0.499999999999998,0.,-0.86602540378444));
#35878=DIRECTION('',(0.,-1.,0.));
#35879=DIRECTION('center_axis',(0.,0.,1.));
#35880=DIRECTION('ref_axis',(-1.,0.,0.));
#35881=DIRECTION('',(0.,-1.,0.));
#35882=DIRECTION('center_axis',(0.866025403784435,0.,0.500000000000006));
#35883=DIRECTION('ref_axis',(-0.500000000000006,0.,0.866025403784435));
#35884=DIRECTION('',(0.,-1.,0.));
#35885=DIRECTION('center_axis',(0.866025403784435,0.,-0.500000000000006));
#35886=DIRECTION('ref_axis',(0.500000000000006,0.,0.866025403784435));
#35887=DIRECTION('',(0.,-1.,0.));
#35888=DIRECTION('center_axis',(0.,0.,-1.));
#35889=DIRECTION('ref_axis',(1.,0.,0.));
#35890=DIRECTION('axis',(0.,0.,1.));
#35891=DIRECTION('refdir',(1.,0.,0.));
#35892=DIRECTION('center_axis',(0.,1.,0.));
#35893=DIRECTION('ref_axis',(1.,0.,0.));
#35894=DIRECTION('center_axis',(0.,-1.,0.));
#35895=DIRECTION('ref_axis',(1.,0.,0.));
#35896=DIRECTION('',(-0.707106781186579,0.707106781186516,8.65956056235532E-17));
#35897=DIRECTION('center_axis',(0.,-1.,0.));
#35898=DIRECTION('ref_axis',(1.,0.,0.));
#35899=DIRECTION('center_axis',(0.,1.,0.));
#35900=DIRECTION('ref_axis',(0.,0.,1.));
#35901=DIRECTION('center_axis',(0.,-1.,0.));
#35902=DIRECTION('ref_axis',(1.,0.,0.));
#35903=DIRECTION('center_axis',(0.,-1.,0.));
#35904=DIRECTION('ref_axis',(1.,0.,0.));
#35905=DIRECTION('center_axis',(0.,-1.,0.));
#35906=DIRECTION('ref_axis',(1.,0.,0.));
#35907=DIRECTION('',(0.,1.,0.));
#35908=DIRECTION('center_axis',(0.,1.,0.));
#35909=DIRECTION('ref_axis',(1.,0.,0.));
#35910=DIRECTION('',(0.707106781186568,-0.707106781186526,-8.65956056235519E-17));
#35911=DIRECTION('center_axis',(0.,-1.,0.));
#35912=DIRECTION('ref_axis',(1.,0.,0.));
#35913=DIRECTION('center_axis',(0.,-1.,0.));
#35914=DIRECTION('ref_axis',(0.,0.,-1.));
#35915=DIRECTION('center_axis',(0.,-1.,0.));
#35916=DIRECTION('ref_axis',(1.,0.,0.));
#35917=DIRECTION('center_axis',(0.,-1.,0.));
#35918=DIRECTION('ref_axis',(1.,0.,0.));
#35919=DIRECTION('',(0.,-1.,0.));
#35920=DIRECTION('axis',(0.,0.,1.));
#35921=DIRECTION('refdir',(1.,0.,0.));
#35922=DIRECTION('center_axis',(0.,1.,0.));
#35923=DIRECTION('ref_axis',(1.,0.,0.));
#35924=DIRECTION('center_axis',(0.,-1.,0.));
#35925=DIRECTION('ref_axis',(1.,0.,0.));
#35926=DIRECTION('',(-0.707106781186547,0.707106781186548,8.65956056235493E-17));
#35927=DIRECTION('center_axis',(0.,1.,0.));
#35928=DIRECTION('ref_axis',(1.,0.,0.));
#35929=DIRECTION('center_axis',(0.,-1.,0.));
#35930=DIRECTION('ref_axis',(1.,0.,0.));
#35931=DIRECTION('',(0.,-1.,0.));
#35932=DIRECTION('center_axis',(0.,1.,0.));
#35933=DIRECTION('ref_axis',(1.,0.,0.));
#35934=DIRECTION('center_axis',(0.,1.,0.));
#35935=DIRECTION('ref_axis',(0.,0.,1.));
#35936=DIRECTION('center_axis',(0.,1.,0.));
#35937=DIRECTION('ref_axis',(1.,0.,0.));
#35938=DIRECTION('center_axis',(0.,-1.,0.));
#35939=DIRECTION('ref_axis',(1.,0.,0.));
#35940=DIRECTION('center_axis',(0.,-1.,0.));
#35941=DIRECTION('ref_axis',(1.,0.,0.));
#35942=DIRECTION('',(0.,1.,0.));
#35943=DIRECTION('center_axis',(0.,1.,0.));
#35944=DIRECTION('ref_axis',(1.,0.,0.));
#35945=DIRECTION('center_axis',(0.,1.,0.));
#35946=DIRECTION('ref_axis',(1.,0.,0.));
#35947=DIRECTION('',(0.707106781186532,-0.707106781186563,-8.65956056235474E-17));
#35948=DIRECTION('center_axis',(0.,-1.,0.));
#35949=DIRECTION('ref_axis',(1.,0.,0.));
#35950=DIRECTION('center_axis',(0.,-1.,0.));
#35951=DIRECTION('ref_axis',(0.,0.,-1.));
#35952=DIRECTION('center_axis',(0.,-1.,0.));
#35953=DIRECTION('ref_axis',(1.,0.,0.));
#35954=DIRECTION('center_axis',(0.,-1.,0.));
#35955=DIRECTION('ref_axis',(1.,0.,0.));
#35956=DIRECTION('center_axis',(0.,-1.,0.));
#35957=DIRECTION('ref_axis',(1.,0.,0.));
#35958=DIRECTION('',(0.,-1.,0.));
#35959=DIRECTION('center_axis',(0.,1.,0.));
#35960=DIRECTION('ref_axis',(1.,0.,0.));
#35961=DIRECTION('center_axis',(0.,-1.,0.));
#35962=DIRECTION('ref_axis',(1.,0.,0.));
#35963=DIRECTION('',(0.866025403784435,0.500000000000007,1.0605752387249E-16));
#35964=DIRECTION('center_axis',(-0.866025403784439,0.,0.5));
#35965=DIRECTION('ref_axis',(0.5,0.,0.866025403784439));
#35966=DIRECTION('',(0.,1.,0.));
#35967=DIRECTION('',(-0.5,0.,-0.866025403784439));
#35968=DIRECTION('',(0.,1.,0.));
#35969=DIRECTION('center_axis',(-0.866025403784439,0.,-0.5));
#35970=DIRECTION('ref_axis',(-0.5,0.,0.866025403784439));
#35971=DIRECTION('',(0.,1.,0.));
#35972=DIRECTION('',(0.5,0.,-0.866025403784438));
#35973=DIRECTION('center_axis',(-2.42263015607378E-16,0.,-1.));
#35974=DIRECTION('ref_axis',(-1.,0.,2.42263015607378E-16));
#35975=DIRECTION('',(0.,1.,0.));
#35976=DIRECTION('',(1.,0.,-2.42263015607378E-16));
#35977=DIRECTION('center_axis',(0.86602540378444,0.,-0.499999999999997));
#35978=DIRECTION('ref_axis',(-0.499999999999997,0.,-0.86602540378444));
#35979=DIRECTION('',(0.,1.,0.));
#35980=DIRECTION('',(0.499999999999997,0.,0.86602540378444));
#35981=DIRECTION('center_axis',(0.86602540378444,0.,0.499999999999997));
#35982=DIRECTION('ref_axis',(0.499999999999997,0.,-0.86602540378444));
#35983=DIRECTION('',(0.,1.,0.));
#35984=DIRECTION('',(-0.499999999999997,0.,0.86602540378444));
#35985=DIRECTION('center_axis',(0.,0.,1.));
#35986=DIRECTION('ref_axis',(1.,0.,0.));
#35987=DIRECTION('',(-1.,0.,0.));
#35988=DIRECTION('center_axis',(0.,1.,0.));
#35989=DIRECTION('ref_axis',(1.,0.,0.));
#35990=DIRECTION('',(0.,0.,1.));
#35991=DIRECTION('',(1.,0.,0.));
#35992=DIRECTION('',(0.,0.,1.));
#35993=DIRECTION('',(1.,0.,0.));
#35994=DIRECTION('',(0.,0.,1.));
#35995=DIRECTION('',(1.,0.,0.));
#35996=DIRECTION('',(0.,0.,1.));
#35997=DIRECTION('',(1.,0.,0.));
#35998=DIRECTION('',(0.,0.,1.));
#35999=DIRECTION('',(1.,0.,0.));
#36000=DIRECTION('',(0.,0.,1.));
#36001=DIRECTION('',(1.,0.,0.));
#36002=DIRECTION('',(0.,0.,1.));
#36003=DIRECTION('',(1.,0.,0.));
#36004=DIRECTION('',(0.,0.,1.));
#36005=DIRECTION('',(1.,0.,0.));
#36006=DIRECTION('',(0.,0.,1.));
#36007=DIRECTION('',(1.,0.,0.));
#36008=DIRECTION('',(0.,0.,1.));
#36009=DIRECTION('',(1.,0.,0.));
#36010=DIRECTION('',(0.,0.,1.));
#36011=DIRECTION('',(1.,0.,0.));
#36012=DIRECTION('',(0.,0.,1.));
#36013=DIRECTION('',(1.,0.,0.));
#36014=DIRECTION('',(0.,0.,1.));
#36015=DIRECTION('',(1.,0.,0.));
#36016=DIRECTION('',(0.,0.,1.));
#36017=DIRECTION('',(1.,0.,0.));
#36018=DIRECTION('',(1.22464679914735E-16,0.,-1.));
#36019=DIRECTION('',(-1.,0.,-1.22464679914735E-16));
#36020=DIRECTION('',(1.22464679914735E-16,0.,-1.));
#36021=DIRECTION('',(-1.,0.,-1.22464679914735E-16));
#36022=DIRECTION('',(1.22464679914735E-16,0.,-1.));
#36023=DIRECTION('',(-1.,0.,-1.22464679914735E-16));
#36024=DIRECTION('',(1.22464679914735E-16,0.,-1.));
#36025=DIRECTION('',(-1.,0.,-1.22464679914735E-16));
#36026=DIRECTION('',(0.,0.,1.));
#36027=DIRECTION('',(1.,0.,0.));
#36028=DIRECTION('',(0.,0.,-1.));
#36029=DIRECTION('',(-1.,0.,0.));
#36030=DIRECTION('',(0.,0.,-1.));
#36031=DIRECTION('',(-1.,0.,0.));
#36032=DIRECTION('',(0.,0.,1.));
#36033=DIRECTION('',(1.,0.,0.));
#36034=DIRECTION('',(0.,0.,1.));
#36035=DIRECTION('',(1.,0.,0.));
#36036=DIRECTION('',(0.,0.,-1.));
#36037=DIRECTION('',(-1.,0.,0.));
#36038=DIRECTION('',(0.,0.,-1.));
#36039=DIRECTION('',(-1.,0.,0.));
#36040=DIRECTION('',(0.,0.,1.));
#36041=DIRECTION('',(0.,-1.,0.));
#36042=DIRECTION('',(0.,0.,1.));
#36043=DIRECTION('',(0.,-1.,0.));
#36044=DIRECTION('',(0.,0.,1.));
#36045=DIRECTION('',(0.,-1.,0.));
#36046=DIRECTION('',(0.,0.,1.));
#36047=DIRECTION('',(0.,-1.,0.));
#36048=DIRECTION('',(0.,0.,1.));
#36049=DIRECTION('',(1.,0.,0.));
#36050=DIRECTION('',(0.,0.,1.));
#36051=DIRECTION('',(1.,0.,0.));
#36052=DIRECTION('',(0.,0.,1.));
#36053=DIRECTION('',(1.,0.,0.));
#36054=DIRECTION('',(0.,0.,1.));
#36055=DIRECTION('',(1.,0.,0.));
#36056=DIRECTION('',(0.,0.,1.));
#36057=DIRECTION('',(1.,0.,0.));
#36058=DIRECTION('',(0.,0.,1.));
#36059=DIRECTION('',(1.,0.,0.));
#36060=DIRECTION('',(0.,0.,1.));
#36061=DIRECTION('',(1.,0.,0.));
#36062=DIRECTION('',(0.,0.,1.));
#36063=DIRECTION('',(1.,0.,0.));
#36064=DIRECTION('',(0.,0.,1.));
#36065=DIRECTION('',(1.,0.,0.));
#36066=DIRECTION('',(0.,0.,-1.));
#36067=DIRECTION('',(1.,0.,0.));
#36068=DIRECTION('',(0.,0.,-1.));
#36069=DIRECTION('',(1.,0.,0.));
#36070=DIRECTION('',(0.,0.,-1.));
#36071=DIRECTION('',(1.,0.,0.));
#36072=DIRECTION('',(0.,0.,-1.));
#36073=DIRECTION('',(1.,0.,0.));
#36074=DIRECTION('',(0.,0.,1.));
#36075=DIRECTION('',(1.,0.,0.));
#36076=DIRECTION('',(0.,0.,1.));
#36077=DIRECTION('',(1.,0.,0.));
#36078=DIRECTION('',(0.,0.,1.));
#36079=DIRECTION('',(1.,0.,0.));
#36080=CARTESIAN_POINT('',(0.,0.,0.));
#36081=CARTESIAN_POINT('',(0.,0.,0.));
#36082=CARTESIAN_POINT('Origin',(-16.614,71.6454,-13.47));
#36083=CARTESIAN_POINT('',(-16.464,71.6454,-11.6675));
#36084=CARTESIAN_POINT('Origin',(-16.464,71.6454,-13.47));
#36085=CARTESIAN_POINT('',(-16.764,71.6454,-11.3675));
#36086=CARTESIAN_POINT('',(-16.614,71.6454,-11.5175));
#36087=CARTESIAN_POINT('Origin',(-16.764,71.6454,-13.47));
#36088=CARTESIAN_POINT('Origin',(-16.764,71.6454,-13.47));
#36089=CARTESIAN_POINT('',(-8.964,71.6454,-11.6675));
#36090=CARTESIAN_POINT('',(-16.764,71.6454,-11.6675));
#36091=CARTESIAN_POINT('',(-8.964,69.8429,-13.47));
#36092=CARTESIAN_POINT('Origin',(-8.964,71.6454,-13.47));
#36093=CARTESIAN_POINT('Origin',(-8.964,71.6454,-13.47));
#36094=CARTESIAN_POINT('Origin',(-16.764,68.4704,-16.51));
#36095=CARTESIAN_POINT('',(-16.764,74.4204,-16.51));
#36096=CARTESIAN_POINT('',(-16.764,74.4204,-8.13));
#36097=CARTESIAN_POINT('',(-16.764,74.4204,-8.255));
#36098=CARTESIAN_POINT('',(-16.764,68.4704,-16.51));
#36099=CARTESIAN_POINT('',(-16.764,68.4704,-16.51));
#36100=CARTESIAN_POINT('',(-16.764,68.4704,-8.13));
#36101=CARTESIAN_POINT('',(-16.764,68.4704,16.51));
#36102=CARTESIAN_POINT('',(-16.764,68.4704,-8.13));
#36103=CARTESIAN_POINT('Origin',(-16.614,71.6454,13.47));
#36104=CARTESIAN_POINT('',(-16.464,71.6454,15.2725));
#36105=CARTESIAN_POINT('Origin',(-16.464,71.6454,13.47));
#36106=CARTESIAN_POINT('',(-16.764,71.6454,15.5725));
#36107=CARTESIAN_POINT('',(-16.614,71.6454,15.4225));
#36108=CARTESIAN_POINT('Origin',(-16.764,71.6454,13.47));
#36109=CARTESIAN_POINT('Origin',(-16.764,71.6454,13.47));
#36110=CARTESIAN_POINT('',(-8.964,71.6454,15.2725));
#36111=CARTESIAN_POINT('',(-16.764,71.6454,15.2725));
#36112=CARTESIAN_POINT('',(-8.96400000000001,69.8429,13.47));
#36113=CARTESIAN_POINT('Origin',(-8.964,71.6454,13.47));
#36114=CARTESIAN_POINT('Origin',(-8.964,71.6454,13.47));
#36115=CARTESIAN_POINT('Origin',(-16.764,68.4704,-16.51));
#36116=CARTESIAN_POINT('',(-16.764,74.4204,8.13));
#36117=CARTESIAN_POINT('',(-16.764,74.4204,16.51));
#36118=CARTESIAN_POINT('',(-16.764,74.4204,-8.255));
#36119=CARTESIAN_POINT('',(-16.764,68.4704,8.13));
#36120=CARTESIAN_POINT('',(-16.764,68.4704,8.13));
#36121=CARTESIAN_POINT('',(-16.764,68.4704,16.51));
#36122=CARTESIAN_POINT('',(-16.764,68.4704,16.51));
#36123=CARTESIAN_POINT('',(-16.764,68.4704,16.51));
#36124=CARTESIAN_POINT('Origin',(-8.964,71.6454,-13.47));
#36125=CARTESIAN_POINT('',(-7.88094873420282,71.6454,-13.47));
#36126=CARTESIAN_POINT('',(-8.964,69.8429,-13.47));
#36127=CARTESIAN_POINT('Origin',(-8.964,71.6454,13.47));
#36128=CARTESIAN_POINT('',(-7.88094873420282,71.6454,13.47));
#36129=CARTESIAN_POINT('',(-8.964,69.8429,13.47));
#36130=CARTESIAN_POINT('Origin',(16.614,71.6454,-13.47));
#36131=CARTESIAN_POINT('',(16.464,71.6454,-11.6675));
#36132=CARTESIAN_POINT('Origin',(16.464,71.6454,-13.47));
#36133=CARTESIAN_POINT('',(16.764,71.6454,-11.3675));
#36134=CARTESIAN_POINT('',(16.614,71.6454,-11.5175));
#36135=CARTESIAN_POINT('Origin',(16.764,71.6454,-13.47));
#36136=CARTESIAN_POINT('Origin',(16.764,71.6454,-13.47));
#36137=CARTESIAN_POINT('',(8.964,71.6454,-11.6675));
#36138=CARTESIAN_POINT('',(16.764,71.6454,-11.6675));
#36139=CARTESIAN_POINT('',(8.964,69.8429,-13.47));
#36140=CARTESIAN_POINT('Origin',(8.964,71.6454,-13.47));
#36141=CARTESIAN_POINT('Origin',(8.964,71.6454,-13.47));
#36142=CARTESIAN_POINT('Origin',(16.764,68.4704,16.51));
#36143=CARTESIAN_POINT('',(16.764,74.4204,-8.13));
#36144=CARTESIAN_POINT('',(16.764,74.4204,-16.51));
#36145=CARTESIAN_POINT('',(16.764,74.4204,8.255));
#36146=CARTESIAN_POINT('',(16.764,68.4704,-8.13));
#36147=CARTESIAN_POINT('',(16.764,68.4704,-8.13));
#36148=CARTESIAN_POINT('',(16.764,68.4704,-16.51));
#36149=CARTESIAN_POINT('',(16.764,68.4704,-16.51));
#36150=CARTESIAN_POINT('',(16.764,68.4704,-16.51));
#36151=CARTESIAN_POINT('Origin',(16.614,71.6454,13.47));
#36152=CARTESIAN_POINT('',(16.464,71.6454,15.2725));
#36153=CARTESIAN_POINT('Origin',(16.464,71.6454,13.47));
#36154=CARTESIAN_POINT('',(16.764,71.6454,15.5725));
#36155=CARTESIAN_POINT('',(16.614,71.6454,15.4225));
#36156=CARTESIAN_POINT('Origin',(16.764,71.6454,13.47));
#36157=CARTESIAN_POINT('Origin',(16.764,71.6454,13.47));
#36158=CARTESIAN_POINT('',(8.964,71.6454,15.2725));
#36159=CARTESIAN_POINT('',(16.764,71.6454,15.2725));
#36160=CARTESIAN_POINT('',(8.964,69.8429,13.47));
#36161=CARTESIAN_POINT('Origin',(8.964,71.6454,13.47));
#36162=CARTESIAN_POINT('Origin',(8.964,71.6454,13.47));
#36163=CARTESIAN_POINT('Origin',(16.764,68.4704,16.51));
#36164=CARTESIAN_POINT('',(16.764,74.4204,16.51));
#36165=CARTESIAN_POINT('',(16.764,74.4204,8.13));
#36166=CARTESIAN_POINT('',(16.764,74.4204,8.255));
#36167=CARTESIAN_POINT('',(16.764,68.4704,16.51));
#36168=CARTESIAN_POINT('',(16.764,68.4704,16.51));
#36169=CARTESIAN_POINT('',(16.764,68.4704,8.13));
#36170=CARTESIAN_POINT('',(16.764,68.4704,-16.51));
#36171=CARTESIAN_POINT('',(16.764,68.4704,8.13));
#36172=CARTESIAN_POINT('Origin',(8.42247436710141,71.6454,-13.47));
#36173=CARTESIAN_POINT('',(7.88094873420282,71.6454,-13.47));
#36174=CARTESIAN_POINT('',(8.42247436710141,70.74415,-13.47));
#36175=CARTESIAN_POINT('Origin',(8.42247436710141,71.6454,13.47));
#36176=CARTESIAN_POINT('',(7.88094873420282,71.6454,13.47));
#36177=CARTESIAN_POINT('',(8.42247436710141,70.74415,13.47));
#36178=CARTESIAN_POINT('Origin',(6.91,74.8204,-6.91));
#36179=CARTESIAN_POINT('',(5.132,74.8204,-6.91));
#36180=CARTESIAN_POINT('Origin',(6.91,74.8204,-6.91));
#36181=CARTESIAN_POINT('',(5.132,68.4704,-6.91));
#36182=CARTESIAN_POINT('',(5.132,74.8204,-6.91));
#36183=CARTESIAN_POINT('Origin',(6.91,68.4704,-6.91));
#36184=CARTESIAN_POINT('Origin',(-6.91,74.8204,6.91));
#36185=CARTESIAN_POINT('',(-8.688,74.8204,6.91));
#36186=CARTESIAN_POINT('Origin',(-6.91,74.8204,6.91));
#36187=CARTESIAN_POINT('',(-8.688,68.4704,6.91));
#36188=CARTESIAN_POINT('',(-8.688,74.8204,6.91));
#36189=CARTESIAN_POINT('Origin',(-6.91,68.4704,6.91));
#36190=CARTESIAN_POINT('Origin',(6.91,74.8204,6.91));
#36191=CARTESIAN_POINT('',(5.132,74.8204,6.91));
#36192=CARTESIAN_POINT('Origin',(6.91,74.8204,6.91));
#36193=CARTESIAN_POINT('',(5.132,68.4704,6.91));
#36194=CARTESIAN_POINT('',(5.132,74.8204,6.91));
#36195=CARTESIAN_POINT('Origin',(6.91,68.4704,6.91));
#36196=CARTESIAN_POINT('Origin',(-6.91,74.8204,-6.91));
#36197=CARTESIAN_POINT('',(-8.688,74.8204,-6.91));
#36198=CARTESIAN_POINT('Origin',(-6.91,74.8204,-6.91));
#36199=CARTESIAN_POINT('',(-8.688,68.4704,-6.91));
#36200=CARTESIAN_POINT('',(-8.688,74.8204,-6.91));
#36201=CARTESIAN_POINT('Origin',(-6.91,68.4704,-6.91));
#36202=CARTESIAN_POINT('Origin',(-9.78,74.6704,0.));
#36203=CARTESIAN_POINT('',(-11.5825,74.5204,-2.2074258554631E-16));
#36204=CARTESIAN_POINT('Origin',(-9.78,74.5204,0.));
#36205=CARTESIAN_POINT('',(-11.8825,74.8204,2.57481989520731E-16));
#36206=CARTESIAN_POINT('',(-11.7325,74.6704,2.39112287533521E-16));
#36207=CARTESIAN_POINT('Origin',(-9.78,74.8204,0.));
#36208=CARTESIAN_POINT('Origin',(0.,74.8204,0.));
#36209=CARTESIAN_POINT('',(6.61825063159195,74.8204,-13.57));
#36210=CARTESIAN_POINT('',(8.25290409693848,74.8204,-16.11));
#36211=CARTESIAN_POINT('',(2.62042490592468,74.8204,-7.35799387242471));
#36212=CARTESIAN_POINT('',(-6.61825063159195,74.8204,-13.57));
#36213=CARTESIAN_POINT('',(-3.2,74.8204,-13.57));
#36214=CARTESIAN_POINT('',(-8.25290409693848,74.8204,-16.11));
#36215=CARTESIAN_POINT('',(-3.59542490592468,74.8204,-8.87299387242471));
#36216=CARTESIAN_POINT('',(-16.364,74.8204,-16.11));
#36217=CARTESIAN_POINT('',(8.382,74.8204,-16.11));
#36218=CARTESIAN_POINT('',(-16.364,74.8204,-8.53));
#36219=CARTESIAN_POINT('',(-16.364,74.8204,-8.255));
#36220=CARTESIAN_POINT('',(-13.07,74.8204,-8.53));
#36221=CARTESIAN_POINT('',(-6.735,74.8204,-8.53));
#36222=CARTESIAN_POINT('',(-13.07,74.8204,8.53));
#36223=CARTESIAN_POINT('',(-13.07,74.8204,4.065));
#36224=CARTESIAN_POINT('',(-16.364,74.8204,8.53));
#36225=CARTESIAN_POINT('',(-9.,74.8204,8.53));
#36226=CARTESIAN_POINT('',(-16.364,74.8204,16.11));
#36227=CARTESIAN_POINT('',(-16.364,74.8204,-8.255));
#36228=CARTESIAN_POINT('',(-8.25290409693848,74.8204,16.11));
#36229=CARTESIAN_POINT('',(-8.382,74.8204,16.11));
#36230=CARTESIAN_POINT('',(-6.61825063159195,74.8204,13.57));
#36231=CARTESIAN_POINT('',(-2.62042490592468,74.8204,7.35799387242471));
#36232=CARTESIAN_POINT('',(6.61825063159195,74.8204,13.57));
#36233=CARTESIAN_POINT('',(3.2,74.8204,13.57));
#36234=CARTESIAN_POINT('',(8.25290409693848,74.8204,16.11));
#36235=CARTESIAN_POINT('',(3.59542490592468,74.8204,8.87299387242471));
#36236=CARTESIAN_POINT('',(16.364,74.8204,16.11));
#36237=CARTESIAN_POINT('',(-8.382,74.8204,16.11));
#36238=CARTESIAN_POINT('',(16.364,74.8204,8.53));
#36239=CARTESIAN_POINT('',(16.364,74.8204,8.255));
#36240=CARTESIAN_POINT('',(13.07,74.8204,8.53));
#36241=CARTESIAN_POINT('',(6.735,74.8204,8.53));
#36242=CARTESIAN_POINT('',(13.07,74.8204,-8.53));
#36243=CARTESIAN_POINT('',(13.07,74.8204,-4.065));
#36244=CARTESIAN_POINT('',(16.364,74.8204,-8.53));
#36245=CARTESIAN_POINT('',(9.,74.8204,-8.53));
#36246=CARTESIAN_POINT('',(16.364,74.8204,-16.11));
#36247=CARTESIAN_POINT('',(16.364,74.8204,8.255));
#36248=CARTESIAN_POINT('',(8.382,74.8204,-16.11));
#36249=CARTESIAN_POINT('',(-2.1025,74.8204,-9.78));
#36250=CARTESIAN_POINT('Origin',(0.,74.8204,-9.78));
#36251=CARTESIAN_POINT('',(-6.763,74.8204,8.28228630263355E-16));
#36252=CARTESIAN_POINT('Origin',(0.,74.8204,0.));
#36253=CARTESIAN_POINT('',(7.6775,74.8204,2.57481989520731E-16));
#36254=CARTESIAN_POINT('Origin',(9.78,74.8204,0.));
#36255=CARTESIAN_POINT('',(-2.1025,74.8204,9.78));
#36256=CARTESIAN_POINT('Origin',(0.,74.8204,9.78));
#36257=CARTESIAN_POINT('Origin',(-9.78,74.8204,0.));
#36258=CARTESIAN_POINT('',(-11.5825,68.4704,2.2074258554631E-16));
#36259=CARTESIAN_POINT('',(-11.5825,74.8204,-2.2074258554631E-16));
#36260=CARTESIAN_POINT('Origin',(-9.78,68.4704,0.));
#36261=CARTESIAN_POINT('Origin',(0.,74.6704,9.78));
#36262=CARTESIAN_POINT('',(-1.8025,74.5204,9.78));
#36263=CARTESIAN_POINT('Origin',(0.,74.5204,9.78));
#36264=CARTESIAN_POINT('',(-1.9525,74.6704,9.78));
#36265=CARTESIAN_POINT('Origin',(0.,74.8204,9.78));
#36266=CARTESIAN_POINT('',(-1.8025,68.4704,9.78));
#36267=CARTESIAN_POINT('',(-1.8025,74.8204,9.78));
#36268=CARTESIAN_POINT('Origin',(0.,68.4704,9.78));
#36269=CARTESIAN_POINT('Origin',(0.,74.6704,-9.78));
#36270=CARTESIAN_POINT('',(-1.8025,74.5204,-9.78));
#36271=CARTESIAN_POINT('Origin',(0.,74.5204,-9.78));
#36272=CARTESIAN_POINT('',(-1.9525,74.6704,-9.78));
#36273=CARTESIAN_POINT('Origin',(0.,74.8204,-9.78));
#36274=CARTESIAN_POINT('',(-1.8025,68.4704,-9.78));
#36275=CARTESIAN_POINT('',(-1.8025,74.8204,-9.78));
#36276=CARTESIAN_POINT('Origin',(0.,68.4704,-9.78));
#36277=CARTESIAN_POINT('Origin',(9.78,74.6704,0.));
#36278=CARTESIAN_POINT('',(7.9775,74.5204,-2.2074258554631E-16));
#36279=CARTESIAN_POINT('Origin',(9.78,74.5204,0.));
#36280=CARTESIAN_POINT('',(7.8275,74.6704,2.39112287533521E-16));
#36281=CARTESIAN_POINT('Origin',(9.78,74.8204,0.));
#36282=CARTESIAN_POINT('',(7.9775,68.4704,2.2074258554631E-16));
#36283=CARTESIAN_POINT('',(7.9775,74.8204,-2.2074258554631E-16));
#36284=CARTESIAN_POINT('Origin',(9.78,68.4704,0.));
#36285=CARTESIAN_POINT('Origin',(0.,74.6204,0.));
#36286=CARTESIAN_POINT('',(-6.363,74.4204,-7.79242758297461E-16));
#36287=CARTESIAN_POINT('Origin',(0.,74.4204,0.));
#36288=CARTESIAN_POINT('',(-6.563,74.6204,8.03735694280408E-16));
#36289=CARTESIAN_POINT('Origin',(0.,74.8204,0.));
#36290=CARTESIAN_POINT('',(-6.363,68.4704,7.79242758297461E-16));
#36291=CARTESIAN_POINT('',(-6.363,74.8204,-7.79242758297461E-16));
#36292=CARTESIAN_POINT('Origin',(0.,68.4704,0.));
#36293=CARTESIAN_POINT('Origin',(-2.45224333470364,74.6204,7.46622953707191));
#36294=CARTESIAN_POINT('',(-8.03465346534654,74.4204,16.51));
#36295=CARTESIAN_POINT('',(-8.25290409693848,74.8204,16.11));
#36296=CARTESIAN_POINT('',(-6.4,74.4204,13.97));
#36297=CARTESIAN_POINT('',(-2.2840617634826,74.4204,7.57446520171912));
#36298=CARTESIAN_POINT('',(-6.4,74.4204,13.97));
#36299=CARTESIAN_POINT('Origin',(-8.382,74.6204,16.31));
#36300=CARTESIAN_POINT('',(-16.364,74.8204,16.11));
#36301=CARTESIAN_POINT('',(-8.382,74.4204,16.51));
#36302=CARTESIAN_POINT('Origin',(-16.564,74.6204,-8.255));
#36303=CARTESIAN_POINT('',(-16.364,74.8204,8.53));
#36304=CARTESIAN_POINT('Origin',(13.27,74.6204,-4.065));
#36305=CARTESIAN_POINT('',(13.47,74.4204,8.13));
#36306=CARTESIAN_POINT('',(13.47,74.4204,-8.13));
#36307=CARTESIAN_POINT('',(13.47,74.4204,-4.065));
#36308=CARTESIAN_POINT('',(13.47,74.4204,-8.13));
#36309=CARTESIAN_POINT('',(13.07,74.8204,8.53));
#36310=CARTESIAN_POINT('Origin',(-9.,74.6204,8.33));
#36311=CARTESIAN_POINT('',(-13.47,74.4204,8.13));
#36312=CARTESIAN_POINT('',(-13.07,74.8204,8.53));
#36313=CARTESIAN_POINT('',(-9.,74.4204,8.13));
#36314=CARTESIAN_POINT('Origin',(-6.735,74.6204,-8.33));
#36315=CARTESIAN_POINT('',(-16.364,74.8204,-8.53));
#36316=CARTESIAN_POINT('',(-13.47,74.4204,-8.13));
#36317=CARTESIAN_POINT('',(-6.735,74.4204,-8.13));
#36318=CARTESIAN_POINT('',(-13.47,74.4204,-8.13));
#36319=CARTESIAN_POINT('Origin',(-16.564,74.6204,-8.255));
#36320=CARTESIAN_POINT('',(-16.364,74.8204,-16.11));
#36321=CARTESIAN_POINT('Origin',(2.45224333470364,74.6204,-7.46622953707191));
#36322=CARTESIAN_POINT('',(8.03465346534654,74.4204,-16.51));
#36323=CARTESIAN_POINT('',(6.4,74.4204,-13.97));
#36324=CARTESIAN_POINT('',(2.2840617634826,74.4204,-7.57446520171912));
#36325=CARTESIAN_POINT('',(6.4,74.4204,-13.97));
#36326=CARTESIAN_POINT('',(8.25290409693848,74.8204,-16.11));
#36327=CARTESIAN_POINT('Origin',(8.382,74.6204,-16.31));
#36328=CARTESIAN_POINT('',(-8.03465346534654,74.4204,-16.51));
#36329=CARTESIAN_POINT('',(-8.25290409693848,74.8204,-16.11));
#36330=CARTESIAN_POINT('',(8.382,74.4204,-16.51));
#36331=CARTESIAN_POINT('Origin',(-3.2,74.6204,-13.77));
#36332=CARTESIAN_POINT('',(-6.4,74.4204,-13.97));
#36333=CARTESIAN_POINT('',(-3.2,74.4204,-13.97));
#36334=CARTESIAN_POINT('',(-6.4,74.4204,-13.97));
#36335=CARTESIAN_POINT('Origin',(-3.42724333470364,74.6204,-8.98122953707191));
#36336=CARTESIAN_POINT('',(-3.2590617634826,74.4204,-9.08946520171912));
#36337=CARTESIAN_POINT('Origin',(8.382,74.6204,-16.31));
#36338=CARTESIAN_POINT('',(8.382,74.4204,-16.51));
#36339=CARTESIAN_POINT('',(16.364,74.8204,-16.11));
#36340=CARTESIAN_POINT('Origin',(16.564,74.6204,8.255));
#36341=CARTESIAN_POINT('',(16.364,74.8204,-8.53));
#36342=CARTESIAN_POINT('Origin',(-13.27,74.6204,4.065));
#36343=CARTESIAN_POINT('',(-13.47,74.4204,4.065));
#36344=CARTESIAN_POINT('Origin',(9.,74.6204,-8.33));
#36345=CARTESIAN_POINT('',(9.,74.4204,-8.13));
#36346=CARTESIAN_POINT('Origin',(6.735,74.6204,8.33));
#36347=CARTESIAN_POINT('',(6.735,74.4204,8.13));
#36348=CARTESIAN_POINT('',(16.364,74.8204,8.53));
#36349=CARTESIAN_POINT('Origin',(16.564,74.6204,8.255));
#36350=CARTESIAN_POINT('',(16.364,74.8204,16.11));
#36351=CARTESIAN_POINT('Origin',(-8.382,74.6204,16.31));
#36352=CARTESIAN_POINT('',(8.03465346534654,74.4204,16.51));
#36353=CARTESIAN_POINT('',(-8.382,74.4204,16.51));
#36354=CARTESIAN_POINT('',(8.25290409693848,74.8204,16.11));
#36355=CARTESIAN_POINT('Origin',(3.2,74.6204,13.77));
#36356=CARTESIAN_POINT('',(6.4,74.4204,13.97));
#36357=CARTESIAN_POINT('',(3.2,74.4204,13.97));
#36358=CARTESIAN_POINT('',(6.4,74.4204,13.97));
#36359=CARTESIAN_POINT('Origin',(3.42724333470364,74.6204,8.98122953707191));
#36360=CARTESIAN_POINT('',(3.2590617634826,74.4204,9.08946520171912));
#36361=CARTESIAN_POINT('Origin',(-16.764,68.4704,16.51));
#36362=CARTESIAN_POINT('',(-8.03465346534653,68.4704,16.51));
#36363=CARTESIAN_POINT('',(16.764,68.4704,16.51));
#36364=CARTESIAN_POINT('',(-8.03465346534654,68.4704,16.51));
#36365=CARTESIAN_POINT('Origin',(-18.,68.4704,8.13));
#36366=CARTESIAN_POINT('',(-13.47,68.4704,8.13));
#36367=CARTESIAN_POINT('',(-13.47,68.4704,8.13));
#36368=CARTESIAN_POINT('',(-9.,68.4704,8.13));
#36369=CARTESIAN_POINT('Origin',(-13.47,68.4704,8.13));
#36370=CARTESIAN_POINT('',(-13.47,68.4704,-8.13));
#36371=CARTESIAN_POINT('',(-13.47,68.4704,-8.13));
#36372=CARTESIAN_POINT('',(-13.47,68.4704,4.065));
#36373=CARTESIAN_POINT('Origin',(-13.47,68.4704,-8.13));
#36374=CARTESIAN_POINT('',(-6.735,68.4704,-8.13));
#36375=CARTESIAN_POINT('Origin',(16.764,68.4704,-16.51));
#36376=CARTESIAN_POINT('',(-8.03465346534654,68.4704,-16.51));
#36377=CARTESIAN_POINT('',(-8.03465346534654,68.4704,-16.51));
#36378=CARTESIAN_POINT('',(-16.764,68.4704,-16.51));
#36379=CARTESIAN_POINT('Origin',(-8.35,68.4704,-17.));
#36380=CARTESIAN_POINT('',(-6.4,68.4704,-13.97));
#36381=CARTESIAN_POINT('',(-6.4,68.4704,-13.97));
#36382=CARTESIAN_POINT('',(-3.2590617634826,68.4704,-9.08946520171912));
#36383=CARTESIAN_POINT('Origin',(-6.4,68.4704,-13.97));
#36384=CARTESIAN_POINT('',(6.4,68.4704,-13.97));
#36385=CARTESIAN_POINT('',(6.4,68.4704,-13.97));
#36386=CARTESIAN_POINT('',(-3.2,68.4704,-13.97));
#36387=CARTESIAN_POINT('Origin',(6.4,68.4704,-13.97));
#36388=CARTESIAN_POINT('',(8.03465346534653,68.4704,-16.51));
#36389=CARTESIAN_POINT('',(8.03465346534654,68.4704,-16.51));
#36390=CARTESIAN_POINT('',(2.2840617634826,68.4704,-7.57446520171912));
#36391=CARTESIAN_POINT('Origin',(8.35,68.4704,17.));
#36392=CARTESIAN_POINT('',(6.4,68.4704,13.97));
#36393=CARTESIAN_POINT('',(6.4,68.4704,13.97));
#36394=CARTESIAN_POINT('',(8.03465346534654,68.4704,16.51));
#36395=CARTESIAN_POINT('',(3.2590617634826,68.4704,9.08946520171912));
#36396=CARTESIAN_POINT('',(8.03465346534654,68.4704,16.51));
#36397=CARTESIAN_POINT('Origin',(-6.4,68.4704,13.97));
#36398=CARTESIAN_POINT('',(-6.4,68.4704,13.97));
#36399=CARTESIAN_POINT('',(-2.2840617634826,68.4704,7.57446520171912));
#36400=CARTESIAN_POINT('',(-6.4,68.4704,13.97));
#36401=CARTESIAN_POINT('Origin',(6.4,68.4704,13.97));
#36402=CARTESIAN_POINT('',(3.2,68.4704,13.97));
#36403=CARTESIAN_POINT('Origin',(16.764,68.4704,-16.51));
#36404=CARTESIAN_POINT('',(-16.764,68.4704,-16.51));
#36405=CARTESIAN_POINT('Origin',(-16.764,68.4704,16.51));
#36406=CARTESIAN_POINT('',(16.764,68.4704,16.51));
#36407=CARTESIAN_POINT('Origin',(0.,68.4704,0.));
#36408=CARTESIAN_POINT('',(13.47,68.4704,-8.13));
#36409=CARTESIAN_POINT('',(9.,68.4704,-8.13));
#36410=CARTESIAN_POINT('',(13.47,68.4704,8.13));
#36411=CARTESIAN_POINT('',(13.47,68.4704,-4.065));
#36412=CARTESIAN_POINT('',(6.735,68.4704,8.13));
#36413=CARTESIAN_POINT('Origin',(13.47,68.4704,-8.13));
#36414=CARTESIAN_POINT('',(13.47,68.4704,8.13));
#36415=CARTESIAN_POINT('',(13.47,68.4704,-8.13));
#36416=CARTESIAN_POINT('Origin',(18.,68.4704,-8.13));
#36417=CARTESIAN_POINT('Origin',(13.47,68.4704,8.13));
#36418=CARTESIAN_POINT('',(0.,0.,0.));
#36419=CARTESIAN_POINT('Origin',(13.47,36.061,18.29));
#36420=CARTESIAN_POINT('',(11.692,36.186,18.29));
#36421=CARTESIAN_POINT('Origin',(13.47,36.186,18.29));
#36422=CARTESIAN_POINT('',(11.442,35.936,18.29));
#36423=CARTESIAN_POINT('',(11.567,36.061,18.29));
#36424=CARTESIAN_POINT('Origin',(13.47,35.936,18.29));
#36425=CARTESIAN_POINT('Origin',(15.68,35.936,0.));
#36426=CARTESIAN_POINT('',(17.28,35.936,-17.65));
#36427=CARTESIAN_POINT('',(52.11,35.936,-17.65));
#36428=CARTESIAN_POINT('',(-20.75,35.936,-17.65));
#36429=CARTESIAN_POINT('',(55.3,35.936,-14.46));
#36430=CARTESIAN_POINT('Origin',(52.11,35.936,-14.46));
#36431=CARTESIAN_POINT('',(55.3,35.936,14.46));
#36432=CARTESIAN_POINT('',(55.3,35.936,-14.46));
#36433=CARTESIAN_POINT('',(52.11,35.936,17.65));
#36434=CARTESIAN_POINT('Origin',(52.11,35.936,14.46));
#36435=CARTESIAN_POINT('',(17.28,35.936,17.65));
#36436=CARTESIAN_POINT('',(52.11,35.936,17.65));
#36437=CARTESIAN_POINT('',(17.28,35.936,21.46));
#36438=CARTESIAN_POINT('',(17.28,35.936,17.));
#36439=CARTESIAN_POINT('',(9.66,35.936,21.46));
#36440=CARTESIAN_POINT('',(17.28,35.936,21.46));
#36441=CARTESIAN_POINT('',(9.66,35.936,17.65));
#36442=CARTESIAN_POINT('',(9.66,35.936,21.46));
#36443=CARTESIAN_POINT('',(-9.66,35.936,17.65));
#36444=CARTESIAN_POINT('',(52.11,35.936,17.65));
#36445=CARTESIAN_POINT('',(-9.66,35.936,21.46));
#36446=CARTESIAN_POINT('',(-9.66,35.936,17.));
#36447=CARTESIAN_POINT('',(-17.28,35.936,21.46));
#36448=CARTESIAN_POINT('',(-9.66,35.936,21.46));
#36449=CARTESIAN_POINT('',(-17.28,35.936,17.65));
#36450=CARTESIAN_POINT('',(-17.28,35.936,21.46));
#36451=CARTESIAN_POINT('',(-20.75,35.936,17.65));
#36452=CARTESIAN_POINT('',(52.11,35.936,17.65));
#36453=CARTESIAN_POINT('',(-23.94,35.936,14.46));
#36454=CARTESIAN_POINT('Origin',(-20.75,35.936,14.46));
#36455=CARTESIAN_POINT('',(-23.94,35.936,-14.46));
#36456=CARTESIAN_POINT('',(-23.94,35.936,14.46));
#36457=CARTESIAN_POINT('',(-20.75,35.936,-17.65));
#36458=CARTESIAN_POINT('Origin',(-20.75,35.936,-14.46));
#36459=CARTESIAN_POINT('',(-17.28,35.936,-17.65));
#36460=CARTESIAN_POINT('',(-20.75,35.936,-17.65));
#36461=CARTESIAN_POINT('',(-17.28,35.936,-21.46));
#36462=CARTESIAN_POINT('',(-17.28,35.936,-21.46));
#36463=CARTESIAN_POINT('',(-9.66,35.936,-21.46));
#36464=CARTESIAN_POINT('',(-9.66,35.936,-21.46));
#36465=CARTESIAN_POINT('',(-9.66,35.936,-17.65));
#36466=CARTESIAN_POINT('',(-9.66,35.936,-17.));
#36467=CARTESIAN_POINT('',(9.66,35.936,-17.65));
#36468=CARTESIAN_POINT('',(-20.75,35.936,-17.65));
#36469=CARTESIAN_POINT('',(9.66,35.936,-21.46));
#36470=CARTESIAN_POINT('',(9.66,35.936,-21.46));
#36471=CARTESIAN_POINT('',(17.28,35.936,-21.46));
#36472=CARTESIAN_POINT('',(17.28,35.936,-21.46));
#36473=CARTESIAN_POINT('',(17.28,35.936,-17.));
#36474=CARTESIAN_POINT('',(-15.498,35.936,-18.29));
#36475=CARTESIAN_POINT('Origin',(-13.47,35.936,-18.29));
#36476=CARTESIAN_POINT('',(11.442,35.936,-18.29));
#36477=CARTESIAN_POINT('Origin',(13.47,35.936,-18.29));
#36478=CARTESIAN_POINT('',(47.5375,35.936,-7.87));
#36479=CARTESIAN_POINT('Origin',(49.34,35.936,-7.87));
#36480=CARTESIAN_POINT('',(-19.7825,35.936,7.87));
#36481=CARTESIAN_POINT('Origin',(-17.98,35.936,7.87));
#36482=CARTESIAN_POINT('',(-19.7825,35.936,-7.87));
#36483=CARTESIAN_POINT('Origin',(-17.98,35.936,-7.87));
#36484=CARTESIAN_POINT('',(47.5375,35.936,7.87));
#36485=CARTESIAN_POINT('Origin',(49.34,35.936,7.87));
#36486=CARTESIAN_POINT('',(49.65,35.936,-2.475));
#36487=CARTESIAN_POINT('',(45.52,35.936,-2.475));
#36488=CARTESIAN_POINT('',(32.665,35.936,-2.475));
#36489=CARTESIAN_POINT('',(45.52,35.936,-13.68));
#36490=CARTESIAN_POINT('',(45.52,35.936,6.84));
#36491=CARTESIAN_POINT('',(44.72,35.936,-14.48));
#36492=CARTESIAN_POINT('Origin',(44.72,35.936,-13.68));
#36493=CARTESIAN_POINT('',(-13.36,35.936,-14.48));
#36494=CARTESIAN_POINT('',(30.2,35.936,-14.48));
#36495=CARTESIAN_POINT('',(-14.16,35.936,-13.68));
#36496=CARTESIAN_POINT('Origin',(-13.36,35.936,-13.68));
#36497=CARTESIAN_POINT('',(-14.16,35.936,-2.475));
#36498=CARTESIAN_POINT('',(-14.16,35.936,-6.84));
#36499=CARTESIAN_POINT('',(-18.29,35.936,-2.475));
#36500=CARTESIAN_POINT('',(0.765,35.936,-2.475));
#36501=CARTESIAN_POINT('',(-18.29,35.936,2.475));
#36502=CARTESIAN_POINT('Origin',(-18.29,35.936,0.));
#36503=CARTESIAN_POINT('',(-14.16,35.936,2.475));
#36504=CARTESIAN_POINT('',(-1.305,35.936,2.475));
#36505=CARTESIAN_POINT('',(-14.16,35.936,13.68));
#36506=CARTESIAN_POINT('',(-14.16,35.936,-6.84));
#36507=CARTESIAN_POINT('',(-13.36,35.936,14.48));
#36508=CARTESIAN_POINT('Origin',(-13.36,35.936,13.68));
#36509=CARTESIAN_POINT('',(44.72,35.936,14.48));
#36510=CARTESIAN_POINT('',(1.16,35.936,14.48));
#36511=CARTESIAN_POINT('',(45.52,35.936,13.68));
#36512=CARTESIAN_POINT('Origin',(44.72,35.936,13.68));
#36513=CARTESIAN_POINT('',(45.52,35.936,2.475));
#36514=CARTESIAN_POINT('',(45.52,35.936,6.84));
#36515=CARTESIAN_POINT('',(49.65,35.936,2.475));
#36516=CARTESIAN_POINT('',(30.595,35.936,2.475));
#36517=CARTESIAN_POINT('Origin',(49.65,35.936,0.));
#36518=CARTESIAN_POINT('',(-15.498,35.936,18.29));
#36519=CARTESIAN_POINT('Origin',(-13.47,35.936,18.29));
#36520=CARTESIAN_POINT('Origin',(13.47,39.116,18.29));
#36521=CARTESIAN_POINT('',(11.692,39.116,18.29));
#36522=CARTESIAN_POINT('Origin',(13.47,39.116,18.29));
#36523=CARTESIAN_POINT('',(11.692,39.116,18.29));
#36524=CARTESIAN_POINT('Origin',(-13.47,36.061,-18.29));
#36525=CARTESIAN_POINT('',(-15.248,36.186,-18.29));
#36526=CARTESIAN_POINT('Origin',(-13.47,36.186,-18.29));
#36527=CARTESIAN_POINT('',(-15.373,36.061,-18.29));
#36528=CARTESIAN_POINT('Origin',(-13.47,39.116,-18.29));
#36529=CARTESIAN_POINT('',(-15.248,39.116,-18.29));
#36530=CARTESIAN_POINT('Origin',(-13.47,39.116,-18.29));
#36531=CARTESIAN_POINT('',(-15.248,39.116,-18.29));
#36532=CARTESIAN_POINT('Origin',(-13.47,36.061,18.29));
#36533=CARTESIAN_POINT('',(-15.248,36.186,18.29));
#36534=CARTESIAN_POINT('Origin',(-13.47,36.186,18.29));
#36535=CARTESIAN_POINT('',(-15.373,36.061,18.29));
#36536=CARTESIAN_POINT('Origin',(-13.47,39.116,18.29));
#36537=CARTESIAN_POINT('',(-15.248,39.116,18.29));
#36538=CARTESIAN_POINT('Origin',(-13.47,39.116,18.29));
#36539=CARTESIAN_POINT('',(-15.248,39.116,18.29));
#36540=CARTESIAN_POINT('Origin',(13.47,36.061,-18.29));
#36541=CARTESIAN_POINT('',(11.692,36.186,-18.29));
#36542=CARTESIAN_POINT('Origin',(13.47,36.186,-18.29));
#36543=CARTESIAN_POINT('',(11.567,36.061,-18.29));
#36544=CARTESIAN_POINT('Origin',(13.47,39.116,-18.29));
#36545=CARTESIAN_POINT('',(11.692,39.116,-18.29));
#36546=CARTESIAN_POINT('Origin',(13.47,39.116,-18.29));
#36547=CARTESIAN_POINT('',(11.692,39.116,-18.29));
#36548=CARTESIAN_POINT('Origin',(49.34,38.966,7.87));
#36549=CARTESIAN_POINT('',(47.5375,38.816,7.87));
#36550=CARTESIAN_POINT('Origin',(49.34,38.816,7.87));
#36551=CARTESIAN_POINT('',(47.2375,39.116,7.87));
#36552=CARTESIAN_POINT('',(47.3875,38.966,7.87));
#36553=CARTESIAN_POINT('Origin',(49.34,39.116,7.87));
#36554=CARTESIAN_POINT('Origin',(15.68,39.116,0.));
#36555=CARTESIAN_POINT('',(52.11,39.116,17.35));
#36556=CARTESIAN_POINT('',(16.98,39.116,17.35));
#36557=CARTESIAN_POINT('',(-2.535,39.116,17.35));
#36558=CARTESIAN_POINT('',(55.,39.116,14.46));
#36559=CARTESIAN_POINT('Origin',(52.11,39.116,14.46));
#36560=CARTESIAN_POINT('',(55.,39.116,-14.46));
#36561=CARTESIAN_POINT('',(55.,39.116,7.23));
#36562=CARTESIAN_POINT('',(52.11,39.116,-17.35));
#36563=CARTESIAN_POINT('Origin',(52.11,39.116,-14.46));
#36564=CARTESIAN_POINT('',(16.98,39.116,-17.35));
#36565=CARTESIAN_POINT('',(33.895,39.116,-17.35));
#36566=CARTESIAN_POINT('',(16.98,39.116,-21.16));
#36567=CARTESIAN_POINT('',(16.98,39.116,-8.5));
#36568=CARTESIAN_POINT('',(9.96,39.116,-21.16));
#36569=CARTESIAN_POINT('',(16.48,39.116,-21.16));
#36570=CARTESIAN_POINT('',(9.96,39.116,-17.35));
#36571=CARTESIAN_POINT('',(9.96,39.116,-10.73));
#36572=CARTESIAN_POINT('',(-9.96,39.116,-17.35));
#36573=CARTESIAN_POINT('',(33.895,39.116,-17.35));
#36574=CARTESIAN_POINT('',(-9.96,39.116,-21.16));
#36575=CARTESIAN_POINT('',(-9.96,39.116,-8.5));
#36576=CARTESIAN_POINT('',(-16.98,39.116,-21.16));
#36577=CARTESIAN_POINT('',(3.01,39.116,-21.16));
#36578=CARTESIAN_POINT('',(-16.98,39.116,-17.35));
#36579=CARTESIAN_POINT('',(-16.98,39.116,-10.73));
#36580=CARTESIAN_POINT('',(-20.75,39.116,-17.35));
#36581=CARTESIAN_POINT('',(33.895,39.116,-17.35));
#36582=CARTESIAN_POINT('',(-23.64,39.116,-14.46));
#36583=CARTESIAN_POINT('Origin',(-20.75,39.116,-14.46));
#36584=CARTESIAN_POINT('',(-23.64,39.116,14.46));
#36585=CARTESIAN_POINT('',(-23.64,39.116,-7.23));
#36586=CARTESIAN_POINT('',(-20.75,39.116,17.35));
#36587=CARTESIAN_POINT('Origin',(-20.75,39.116,14.46));
#36588=CARTESIAN_POINT('',(-16.98,39.116,17.35));
#36589=CARTESIAN_POINT('',(-2.535,39.116,17.35));
#36590=CARTESIAN_POINT('',(-16.98,39.116,21.16));
#36591=CARTESIAN_POINT('',(-16.98,39.116,8.5));
#36592=CARTESIAN_POINT('',(-9.96,39.116,21.16));
#36593=CARTESIAN_POINT('',(-0.800000000000002,39.116,21.16));
#36594=CARTESIAN_POINT('',(-9.96,39.116,17.35));
#36595=CARTESIAN_POINT('',(-9.96,39.116,10.73));
#36596=CARTESIAN_POINT('',(9.96,39.116,17.35));
#36597=CARTESIAN_POINT('',(-2.535,39.116,17.35));
#36598=CARTESIAN_POINT('',(9.96,39.116,21.16));
#36599=CARTESIAN_POINT('',(9.96,39.116,8.5));
#36600=CARTESIAN_POINT('',(16.98,39.116,21.16));
#36601=CARTESIAN_POINT('',(12.67,39.116,21.16));
#36602=CARTESIAN_POINT('',(16.98,39.116,10.73));
#36603=CARTESIAN_POINT('',(-20.0825,39.116,7.87));
#36604=CARTESIAN_POINT('Origin',(-17.98,39.116,7.87));
#36605=CARTESIAN_POINT('',(-14.46,39.116,-13.68));
#36606=CARTESIAN_POINT('',(-14.46,39.116,-2.775));
#36607=CARTESIAN_POINT('',(-14.46,39.116,-6.84));
#36608=CARTESIAN_POINT('',(-13.36,39.116,-14.78));
#36609=CARTESIAN_POINT('Origin',(-13.36,39.116,-13.68));
#36610=CARTESIAN_POINT('',(44.72,39.116,-14.78));
#36611=CARTESIAN_POINT('',(30.2,39.116,-14.78));
#36612=CARTESIAN_POINT('',(45.82,39.116,-13.68));
#36613=CARTESIAN_POINT('Origin',(44.72,39.116,-13.68));
#36614=CARTESIAN_POINT('',(45.82,39.116,-2.775));
#36615=CARTESIAN_POINT('',(45.82,39.116,6.84));
#36616=CARTESIAN_POINT('',(49.65,39.116,-2.775));
#36617=CARTESIAN_POINT('',(32.665,39.116,-2.775));
#36618=CARTESIAN_POINT('',(49.65,39.116,2.775));
#36619=CARTESIAN_POINT('Origin',(49.65,39.116,0.));
#36620=CARTESIAN_POINT('',(45.82,39.116,2.775));
#36621=CARTESIAN_POINT('',(30.595,39.116,2.775));
#36622=CARTESIAN_POINT('',(45.82,39.116,13.68));
#36623=CARTESIAN_POINT('',(45.82,39.116,6.84));
#36624=CARTESIAN_POINT('',(44.72,39.116,14.78));
#36625=CARTESIAN_POINT('Origin',(44.72,39.116,13.68));
#36626=CARTESIAN_POINT('',(-13.36,39.116,14.78));
#36627=CARTESIAN_POINT('',(1.16,39.116,14.78));
#36628=CARTESIAN_POINT('',(-14.46,39.116,13.68));
#36629=CARTESIAN_POINT('Origin',(-13.36,39.116,13.68));
#36630=CARTESIAN_POINT('',(-14.46,39.116,2.775));
#36631=CARTESIAN_POINT('',(-14.46,39.116,-6.84));
#36632=CARTESIAN_POINT('',(-18.29,39.116,2.775));
#36633=CARTESIAN_POINT('',(-1.305,39.116,2.775));
#36634=CARTESIAN_POINT('',(-18.29,39.116,-2.775));
#36635=CARTESIAN_POINT('Origin',(-18.29,39.116,0.));
#36636=CARTESIAN_POINT('',(0.765,39.116,-2.775));
#36637=CARTESIAN_POINT('',(47.2375,39.116,-7.87));
#36638=CARTESIAN_POINT('Origin',(49.34,39.116,-7.87));
#36639=CARTESIAN_POINT('',(-20.0825,39.116,-7.87));
#36640=CARTESIAN_POINT('Origin',(-17.98,39.116,-7.87));
#36641=CARTESIAN_POINT('Origin',(49.34,39.116,7.87));
#36642=CARTESIAN_POINT('',(47.5375,39.116,7.87));
#36643=CARTESIAN_POINT('Origin',(-17.98,38.966,-7.87));
#36644=CARTESIAN_POINT('',(-19.7825,38.816,-7.87));
#36645=CARTESIAN_POINT('Origin',(-17.98,38.816,-7.87));
#36646=CARTESIAN_POINT('',(-19.9325,38.966,-7.87));
#36647=CARTESIAN_POINT('Origin',(-17.98,39.116,-7.87));
#36648=CARTESIAN_POINT('',(-19.7825,39.116,-7.87));
#36649=CARTESIAN_POINT('Origin',(-17.98,38.966,7.87));
#36650=CARTESIAN_POINT('',(-19.7825,38.816,7.87));
#36651=CARTESIAN_POINT('Origin',(-17.98,38.816,7.87));
#36652=CARTESIAN_POINT('',(-19.9325,38.966,7.87));
#36653=CARTESIAN_POINT('Origin',(-17.98,39.116,7.87));
#36654=CARTESIAN_POINT('',(-19.7825,39.116,7.87));
#36655=CARTESIAN_POINT('Origin',(49.34,38.966,-7.87));
#36656=CARTESIAN_POINT('',(47.5375,38.816,-7.87));
#36657=CARTESIAN_POINT('Origin',(49.34,38.816,-7.87));
#36658=CARTESIAN_POINT('',(47.3875,38.966,-7.87));
#36659=CARTESIAN_POINT('Origin',(49.34,39.116,-7.87));
#36660=CARTESIAN_POINT('',(47.5375,39.116,-7.87));
#36661=CARTESIAN_POINT('Origin',(-2.535,38.966,17.5));
#36662=CARTESIAN_POINT('',(-9.66,38.816,17.65));
#36663=CARTESIAN_POINT('',(-9.96,39.116,17.35));
#36664=CARTESIAN_POINT('',(9.66,38.816,17.65));
#36665=CARTESIAN_POINT('',(-2.535,38.816,17.65));
#36666=CARTESIAN_POINT('',(9.96,39.116,17.35));
#36667=CARTESIAN_POINT('Origin',(-9.81,38.966,10.73));
#36668=CARTESIAN_POINT('',(-9.66,38.816,21.46));
#36669=CARTESIAN_POINT('',(-9.96,39.116,21.16));
#36670=CARTESIAN_POINT('',(-9.66,38.816,10.73));
#36671=CARTESIAN_POINT('Origin',(-0.800000000000002,38.966,21.31));
#36672=CARTESIAN_POINT('',(-17.28,38.816,21.46));
#36673=CARTESIAN_POINT('',(-16.98,39.116,21.16));
#36674=CARTESIAN_POINT('',(-0.800000000000002,38.816,21.46));
#36675=CARTESIAN_POINT('Origin',(-17.13,38.966,8.5));
#36676=CARTESIAN_POINT('',(-17.28,38.816,17.65));
#36677=CARTESIAN_POINT('',(-16.98,39.116,17.35));
#36678=CARTESIAN_POINT('',(-17.28,38.816,8.5));
#36679=CARTESIAN_POINT('Origin',(33.895,38.966,-17.5));
#36680=CARTESIAN_POINT('',(-17.28,38.816,-17.65));
#36681=CARTESIAN_POINT('',(-20.75,38.816,-17.65));
#36682=CARTESIAN_POINT('',(33.895,38.816,-17.65));
#36683=CARTESIAN_POINT('',(-20.75,38.816,-17.65));
#36684=CARTESIAN_POINT('',(-16.98,39.116,-17.35));
#36685=CARTESIAN_POINT('Origin',(-17.13,38.966,-10.73));
#36686=CARTESIAN_POINT('',(-17.28,38.816,-21.46));
#36687=CARTESIAN_POINT('',(-16.98,39.116,-21.16));
#36688=CARTESIAN_POINT('',(-17.28,38.816,-10.73));
#36689=CARTESIAN_POINT('Origin',(3.01,38.966,-21.31));
#36690=CARTESIAN_POINT('',(-9.66,38.816,-21.46));
#36691=CARTESIAN_POINT('',(-9.96,39.116,-21.16));
#36692=CARTESIAN_POINT('',(3.01,38.816,-21.46));
#36693=CARTESIAN_POINT('Origin',(-9.81,38.966,-8.5));
#36694=CARTESIAN_POINT('',(-9.66,38.816,-17.65));
#36695=CARTESIAN_POINT('',(-9.96,39.116,-17.35));
#36696=CARTESIAN_POINT('',(-9.66,38.816,-8.5));
#36697=CARTESIAN_POINT('Origin',(33.895,38.966,-17.5));
#36698=CARTESIAN_POINT('',(9.66,38.816,-17.65));
#36699=CARTESIAN_POINT('',(9.96,39.116,-17.35));
#36700=CARTESIAN_POINT('',(33.895,38.816,-17.65));
#36701=CARTESIAN_POINT('Origin',(9.81,38.966,-10.73));
#36702=CARTESIAN_POINT('',(9.66,38.816,-21.46));
#36703=CARTESIAN_POINT('',(9.66,38.816,-10.73));
#36704=CARTESIAN_POINT('',(9.96,39.116,-21.16));
#36705=CARTESIAN_POINT('Origin',(16.48,38.966,-21.31));
#36706=CARTESIAN_POINT('',(17.28,38.816,-21.46));
#36707=CARTESIAN_POINT('',(16.48,38.816,-21.46));
#36708=CARTESIAN_POINT('',(16.98,39.116,-21.16));
#36709=CARTESIAN_POINT('Origin',(17.13,38.966,-8.5));
#36710=CARTESIAN_POINT('',(17.28,38.816,-17.65));
#36711=CARTESIAN_POINT('',(17.28,38.816,-8.5));
#36712=CARTESIAN_POINT('',(16.98,39.116,-17.35));
#36713=CARTESIAN_POINT('Origin',(-2.535,38.966,17.5));
#36714=CARTESIAN_POINT('',(17.28,38.816,17.65));
#36715=CARTESIAN_POINT('',(52.11,38.816,17.65));
#36716=CARTESIAN_POINT('',(-2.535,38.816,17.65));
#36717=CARTESIAN_POINT('',(52.11,38.816,17.65));
#36718=CARTESIAN_POINT('',(16.98,39.116,17.35));
#36719=CARTESIAN_POINT('Origin',(52.11,38.966,14.46));
#36720=CARTESIAN_POINT('',(55.3,38.816,14.46));
#36721=CARTESIAN_POINT('',(55.3,38.816,14.46));
#36722=CARTESIAN_POINT('Origin',(52.11,38.816,14.46));
#36723=CARTESIAN_POINT('Origin',(55.15,38.966,7.23));
#36724=CARTESIAN_POINT('',(55.3,38.816,-14.46));
#36725=CARTESIAN_POINT('',(55.3,38.816,-14.46));
#36726=CARTESIAN_POINT('',(55.3,38.816,7.23));
#36727=CARTESIAN_POINT('Origin',(52.11,38.966,-14.46));
#36728=CARTESIAN_POINT('',(52.11,38.816,-17.65));
#36729=CARTESIAN_POINT('',(52.11,38.816,-17.65));
#36730=CARTESIAN_POINT('Origin',(52.11,38.816,-14.46));
#36731=CARTESIAN_POINT('Origin',(33.895,38.966,-17.5));
#36732=CARTESIAN_POINT('',(33.895,38.816,-17.65));
#36733=CARTESIAN_POINT('Origin',(-20.75,38.966,-14.46));
#36734=CARTESIAN_POINT('',(-23.94,38.816,-14.46));
#36735=CARTESIAN_POINT('',(-23.94,38.816,-14.46));
#36736=CARTESIAN_POINT('Origin',(-20.75,38.816,-14.46));
#36737=CARTESIAN_POINT('Origin',(-23.79,38.966,-7.23));
#36738=CARTESIAN_POINT('',(-23.94,38.816,14.46));
#36739=CARTESIAN_POINT('',(-23.94,38.816,14.46));
#36740=CARTESIAN_POINT('',(-23.94,38.816,-7.23));
#36741=CARTESIAN_POINT('Origin',(-20.75,38.966,14.46));
#36742=CARTESIAN_POINT('',(-20.75,38.816,17.65));
#36743=CARTESIAN_POINT('',(-20.75,38.816,17.65));
#36744=CARTESIAN_POINT('Origin',(-20.75,38.816,14.46));
#36745=CARTESIAN_POINT('Origin',(-2.535,38.966,17.5));
#36746=CARTESIAN_POINT('',(-2.535,38.816,17.65));
#36747=CARTESIAN_POINT('Origin',(17.13,38.966,10.73));
#36748=CARTESIAN_POINT('',(17.28,38.816,21.46));
#36749=CARTESIAN_POINT('',(17.28,38.816,10.73));
#36750=CARTESIAN_POINT('',(16.98,39.116,21.16));
#36751=CARTESIAN_POINT('Origin',(12.67,38.966,21.31));
#36752=CARTESIAN_POINT('',(9.66,38.816,21.46));
#36753=CARTESIAN_POINT('',(12.67,38.816,21.46));
#36754=CARTESIAN_POINT('',(9.96,39.116,21.16));
#36755=CARTESIAN_POINT('Origin',(9.81,38.966,8.5));
#36756=CARTESIAN_POINT('',(9.66,38.816,8.5));
#36757=CARTESIAN_POINT('Origin',(-17.28,35.936,-21.46));
#36758=CARTESIAN_POINT('',(-17.28,35.936,-21.46));
#36759=CARTESIAN_POINT('',(-17.28,35.936,-17.65));
#36760=CARTESIAN_POINT('Origin',(-9.66,35.936,-21.46));
#36761=CARTESIAN_POINT('',(-9.66,35.936,-21.46));
#36762=CARTESIAN_POINT('Origin',(-9.66,35.936,-17.));
#36763=CARTESIAN_POINT('',(-9.66,35.936,-17.65));
#36764=CARTESIAN_POINT('Origin',(52.11,35.936,-17.65));
#36765=CARTESIAN_POINT('',(9.66,35.936,-17.65));
#36766=CARTESIAN_POINT('Origin',(9.66,35.936,-21.46));
#36767=CARTESIAN_POINT('',(9.66,35.936,-21.46));
#36768=CARTESIAN_POINT('Origin',(17.28,35.936,-21.46));
#36769=CARTESIAN_POINT('',(17.28,35.936,-21.46));
#36770=CARTESIAN_POINT('Origin',(17.28,35.936,-17.));
#36771=CARTESIAN_POINT('',(17.28,35.936,-17.65));
#36772=CARTESIAN_POINT('Origin',(52.11,35.936,-17.65));
#36773=CARTESIAN_POINT('',(52.11,35.936,-17.65));
#36774=CARTESIAN_POINT('Origin',(52.11,35.936,-14.46));
#36775=CARTESIAN_POINT('',(55.3,35.936,-14.46));
#36776=CARTESIAN_POINT('Origin',(55.3,35.936,14.46));
#36777=CARTESIAN_POINT('',(55.3,35.936,14.46));
#36778=CARTESIAN_POINT('Origin',(52.11,35.936,14.46));
#36779=CARTESIAN_POINT('',(52.11,35.936,17.65));
#36780=CARTESIAN_POINT('Origin',(-20.75,35.936,17.65));
#36781=CARTESIAN_POINT('',(17.28,35.936,17.65));
#36782=CARTESIAN_POINT('Origin',(-1.305,38.966,2.625));
#36783=CARTESIAN_POINT('',(-14.16,38.816,2.475));
#36784=CARTESIAN_POINT('',(-18.29,38.816,2.475));
#36785=CARTESIAN_POINT('',(-1.305,38.816,2.475));
#36786=CARTESIAN_POINT('',(-18.29,38.816,2.475));
#36787=CARTESIAN_POINT('',(-14.46,39.116,2.775));
#36788=CARTESIAN_POINT('Origin',(45.67,38.966,6.84));
#36789=CARTESIAN_POINT('',(45.52,38.816,2.475));
#36790=CARTESIAN_POINT('',(45.52,38.816,13.68));
#36791=CARTESIAN_POINT('',(45.52,38.816,6.84));
#36792=CARTESIAN_POINT('',(45.52,38.816,13.68));
#36793=CARTESIAN_POINT('',(45.82,39.116,2.775));
#36794=CARTESIAN_POINT('Origin',(32.665,38.966,-2.625));
#36795=CARTESIAN_POINT('',(45.52,38.816,-2.475));
#36796=CARTESIAN_POINT('',(49.65,38.816,-2.475));
#36797=CARTESIAN_POINT('',(32.665,38.816,-2.475));
#36798=CARTESIAN_POINT('',(49.65,38.816,-2.475));
#36799=CARTESIAN_POINT('',(45.82,39.116,-2.775));
#36800=CARTESIAN_POINT('Origin',(49.65,38.966,0.));
#36801=CARTESIAN_POINT('',(49.65,38.816,2.475));
#36802=CARTESIAN_POINT('',(49.65,38.816,2.475));
#36803=CARTESIAN_POINT('Origin',(49.65,38.816,0.));
#36804=CARTESIAN_POINT('Origin',(30.595,38.966,2.625));
#36805=CARTESIAN_POINT('',(30.595,38.816,2.475));
#36806=CARTESIAN_POINT('Origin',(-14.31,38.966,-6.84));
#36807=CARTESIAN_POINT('',(-14.16,38.816,-2.475));
#36808=CARTESIAN_POINT('',(-14.16,38.816,-13.68));
#36809=CARTESIAN_POINT('',(-14.16,38.816,-6.84));
#36810=CARTESIAN_POINT('',(-14.16,38.816,-13.68));
#36811=CARTESIAN_POINT('',(-14.46,39.116,-2.775));
#36812=CARTESIAN_POINT('Origin',(-13.36,38.966,-13.68));
#36813=CARTESIAN_POINT('',(-13.36,38.816,-14.48));
#36814=CARTESIAN_POINT('',(-13.36,38.816,-14.48));
#36815=CARTESIAN_POINT('Origin',(-13.36,38.816,-13.68));
#36816=CARTESIAN_POINT('Origin',(30.2,38.966,-14.63));
#36817=CARTESIAN_POINT('',(44.72,38.816,-14.48));
#36818=CARTESIAN_POINT('',(44.72,38.816,-14.48));
#36819=CARTESIAN_POINT('',(30.2,38.816,-14.48));
#36820=CARTESIAN_POINT('Origin',(44.72,38.966,-13.68));
#36821=CARTESIAN_POINT('',(45.52,38.816,-13.68));
#36822=CARTESIAN_POINT('',(45.52,38.816,-13.68));
#36823=CARTESIAN_POINT('Origin',(44.72,38.816,-13.68));
#36824=CARTESIAN_POINT('Origin',(45.67,38.966,6.84));
#36825=CARTESIAN_POINT('',(45.52,38.816,6.84));
#36826=CARTESIAN_POINT('Origin',(44.72,38.966,13.68));
#36827=CARTESIAN_POINT('',(44.72,38.816,14.48));
#36828=CARTESIAN_POINT('',(44.72,38.816,14.48));
#36829=CARTESIAN_POINT('Origin',(44.72,38.816,13.68));
#36830=CARTESIAN_POINT('Origin',(1.16,38.966,14.63));
#36831=CARTESIAN_POINT('',(-13.36,38.816,14.48));
#36832=CARTESIAN_POINT('',(-13.36,38.816,14.48));
#36833=CARTESIAN_POINT('',(1.16,38.816,14.48));
#36834=CARTESIAN_POINT('Origin',(-13.36,38.966,13.68));
#36835=CARTESIAN_POINT('',(-14.16,38.816,13.68));
#36836=CARTESIAN_POINT('',(-14.16,38.816,13.68));
#36837=CARTESIAN_POINT('Origin',(-13.36,38.816,13.68));
#36838=CARTESIAN_POINT('Origin',(-14.31,38.966,-6.84));
#36839=CARTESIAN_POINT('',(-14.16,38.816,-6.84));
#36840=CARTESIAN_POINT('Origin',(-18.29,38.966,0.));
#36841=CARTESIAN_POINT('',(-18.29,38.816,-2.475));
#36842=CARTESIAN_POINT('',(-18.29,38.816,-2.475));
#36843=CARTESIAN_POINT('Origin',(-18.29,38.816,0.));
#36844=CARTESIAN_POINT('Origin',(0.765,38.966,-2.625));
#36845=CARTESIAN_POINT('',(0.765,38.816,-2.475));
#36846=CARTESIAN_POINT('Origin',(45.51,35.936,2.475));
#36847=CARTESIAN_POINT('',(49.65,35.936,2.475));
#36848=CARTESIAN_POINT('',(45.52,35.936,2.475));
#36849=CARTESIAN_POINT('Origin',(49.65,35.936,0.));
#36850=CARTESIAN_POINT('',(49.65,35.936,-2.475));
#36851=CARTESIAN_POINT('Origin',(49.65,35.936,-2.475));
#36852=CARTESIAN_POINT('',(45.52,35.936,-2.475));
#36853=CARTESIAN_POINT('Origin',(45.52,35.936,13.68));
#36854=CARTESIAN_POINT('',(45.52,35.936,-13.68));
#36855=CARTESIAN_POINT('Origin',(44.72,35.936,-13.68));
#36856=CARTESIAN_POINT('',(44.72,35.936,-14.48));
#36857=CARTESIAN_POINT('Origin',(44.72,35.936,-14.48));
#36858=CARTESIAN_POINT('',(-13.36,35.936,-14.48));
#36859=CARTESIAN_POINT('Origin',(-13.36,35.936,-13.68));
#36860=CARTESIAN_POINT('',(-14.16,35.936,-13.68));
#36861=CARTESIAN_POINT('Origin',(-14.16,35.936,-13.68));
#36862=CARTESIAN_POINT('',(-14.16,35.936,-2.475));
#36863=CARTESIAN_POINT('Origin',(-14.15,35.936,-2.475));
#36864=CARTESIAN_POINT('',(-18.29,35.936,-2.475));
#36865=CARTESIAN_POINT('Origin',(-18.29,35.936,2.475));
#36866=CARTESIAN_POINT('',(-14.16,35.936,2.475));
#36867=CARTESIAN_POINT('',(-18.29,35.936,2.475));
#36868=CARTESIAN_POINT('Origin',(-18.29,35.936,0.));
#36869=CARTESIAN_POINT('Origin',(45.52,35.936,13.68));
#36870=CARTESIAN_POINT('',(45.52,35.936,13.68));
#36871=CARTESIAN_POINT('Origin',(-14.16,35.936,-13.68));
#36872=CARTESIAN_POINT('',(-14.16,35.936,13.68));
#36873=CARTESIAN_POINT('Origin',(44.72,35.936,13.68));
#36874=CARTESIAN_POINT('',(44.72,35.936,14.48));
#36875=CARTESIAN_POINT('Origin',(-13.36,35.936,14.48));
#36876=CARTESIAN_POINT('',(-13.36,35.936,14.48));
#36877=CARTESIAN_POINT('Origin',(-13.36,35.936,13.68));
#36878=CARTESIAN_POINT('Origin',(17.28,35.936,21.46));
#36879=CARTESIAN_POINT('',(17.28,35.936,21.46));
#36880=CARTESIAN_POINT('Origin',(9.66,35.936,17.));
#36881=CARTESIAN_POINT('',(9.66,35.936,17.65));
#36882=CARTESIAN_POINT('',(9.66,35.936,21.46));
#36883=CARTESIAN_POINT('Origin',(9.66,35.936,21.46));
#36884=CARTESIAN_POINT('Origin',(-20.75,35.936,17.65));
#36885=CARTESIAN_POINT('',(-9.66,35.936,17.65));
#36886=CARTESIAN_POINT('Origin',(-17.28,35.936,17.));
#36887=CARTESIAN_POINT('',(-17.28,35.936,17.65));
#36888=CARTESIAN_POINT('',(-17.28,35.936,21.46));
#36889=CARTESIAN_POINT('Origin',(-9.66,35.936,21.46));
#36890=CARTESIAN_POINT('',(-9.66,35.936,21.46));
#36891=CARTESIAN_POINT('Origin',(-17.28,35.936,21.46));
#36892=CARTESIAN_POINT('Origin',(-20.75,35.936,17.65));
#36893=CARTESIAN_POINT('',(-20.75,35.936,17.65));
#36894=CARTESIAN_POINT('Origin',(-20.75,35.936,14.46));
#36895=CARTESIAN_POINT('',(-23.94,35.936,14.46));
#36896=CARTESIAN_POINT('Origin',(-23.94,35.936,-14.46));
#36897=CARTESIAN_POINT('',(-23.94,35.936,-14.46));
#36898=CARTESIAN_POINT('Origin',(-20.75,35.936,-14.46));
#36899=CARTESIAN_POINT('',(-20.75,35.936,-17.65));
#36900=CARTESIAN_POINT('Origin',(52.11,35.936,-17.65));
#36901=CARTESIAN_POINT('',(0.,0.,0.));
#36902=CARTESIAN_POINT('Origin',(-13.82,8.,0.));
#36903=CARTESIAN_POINT('',(-17.82,8.,2.5));
#36904=CARTESIAN_POINT('Origin',(-17.82,8.,0.));
#36905=CARTESIAN_POINT('',(-13.82,8.,2.5));
#36906=CARTESIAN_POINT('',(-13.82,8.,2.5));
#36907=CARTESIAN_POINT('Origin',(-13.82,8.,0.));
#36908=CARTESIAN_POINT('Origin',(-17.82,8.,0.));
#36909=CARTESIAN_POINT('Origin',(49.34,41.616,-7.87));
#36910=CARTESIAN_POINT('',(47.34,41.616,-7.87));
#36911=CARTESIAN_POINT('Origin',(49.34,41.616,-7.87));
#36912=CARTESIAN_POINT('',(47.34,39.116,-7.87));
#36913=CARTESIAN_POINT('',(47.34,41.616,-7.87));
#36914=CARTESIAN_POINT('Origin',(49.34,39.116,-7.87));
#36915=CARTESIAN_POINT('Origin',(-17.98,41.616,7.87));
#36916=CARTESIAN_POINT('',(-19.98,41.616,7.87));
#36917=CARTESIAN_POINT('Origin',(-17.98,41.616,7.87));
#36918=CARTESIAN_POINT('',(-19.98,39.116,7.87));
#36919=CARTESIAN_POINT('',(-19.98,41.616,7.87));
#36920=CARTESIAN_POINT('Origin',(-17.98,39.116,7.87));
#36921=CARTESIAN_POINT('Origin',(-17.98,41.616,-7.87));
#36922=CARTESIAN_POINT('',(-19.98,41.616,-7.87));
#36923=CARTESIAN_POINT('Origin',(-17.98,41.616,-7.87));
#36924=CARTESIAN_POINT('',(-19.98,39.116,-7.87));
#36925=CARTESIAN_POINT('',(-19.98,41.616,-7.87));
#36926=CARTESIAN_POINT('Origin',(-17.98,39.116,-7.87));
#36927=CARTESIAN_POINT('Origin',(49.34,41.616,7.87));
#36928=CARTESIAN_POINT('',(47.34,41.616,7.87));
#36929=CARTESIAN_POINT('Origin',(49.34,41.616,7.87));
#36930=CARTESIAN_POINT('',(47.34,39.116,7.87));
#36931=CARTESIAN_POINT('',(47.34,41.616,7.87));
#36932=CARTESIAN_POINT('Origin',(49.34,39.116,7.87));
#36933=CARTESIAN_POINT('Origin',(0.,53.835,0.));
#36934=CARTESIAN_POINT('',(-1.55,53.735,-1.8982025386784E-16));
#36935=CARTESIAN_POINT('Origin',(0.,53.735,0.));
#36936=CARTESIAN_POINT('',(-1.75,53.935,2.14313189850787E-16));
#36937=CARTESIAN_POINT('',(-1.65,53.835,2.02066721859313E-16));
#36938=CARTESIAN_POINT('Origin',(0.,53.935,0.));
#36939=CARTESIAN_POINT('Origin',(0.,53.935,0.));
#36940=CARTESIAN_POINT('',(-1.55,47.935,-1.8982025386784E-16));
#36941=CARTESIAN_POINT('',(-1.55,53.935,-1.8982025386784E-16));
#36942=CARTESIAN_POINT('Origin',(0.,47.935,0.));
#36943=CARTESIAN_POINT('Origin',(2.955,53.935,0.));
#36944=CARTESIAN_POINT('',(-2.955,53.935,-3.61883129148043E-16));
#36945=CARTESIAN_POINT('Origin',(0.,53.935,0.));
#36946=CARTESIAN_POINT('Origin',(0.,47.935,0.));
#36947=CARTESIAN_POINT('',(0.,47.0036660405073,0.));
#36948=CARTESIAN_POINT('',(-1.55,47.935,1.8982025386784E-16));
#36949=CARTESIAN_POINT('Origin',(0.,51.0675,0.));
#36950=CARTESIAN_POINT('',(-3.255,49.,-3.98622533122464E-16));
#36951=CARTESIAN_POINT('Origin',(0.,49.,0.));
#36952=CARTESIAN_POINT('',(-3.255,53.635,-3.98622533122464E-16));
#36953=CARTESIAN_POINT('',(-3.255,51.0675,-3.98622533122464E-16));
#36954=CARTESIAN_POINT('Origin',(0.,53.635,0.));
#36955=CARTESIAN_POINT('Origin',(0.,53.785,0.));
#36956=CARTESIAN_POINT('',(-3.105,53.785,-3.80252831135253E-16));
#36957=CARTESIAN_POINT('Origin',(0.,47.6,0.));
#36958=CARTESIAN_POINT('',(-5.5,47.,-6.73555739531044E-16));
#36959=CARTESIAN_POINT('Origin',(0.,47.,0.));
#36960=CARTESIAN_POINT('',(-5.5,48.7,-6.73555739531044E-16));
#36961=CARTESIAN_POINT('',(-5.5,47.6,-6.73555739531044E-16));
#36962=CARTESIAN_POINT('Origin',(0.,48.7,0.));
#36963=CARTESIAN_POINT('Origin',(5.2,49.,0.));
#36964=CARTESIAN_POINT('',(-5.2,49.,-6.36816335556623E-16));
#36965=CARTESIAN_POINT('Origin',(0.,49.,0.));
#36966=CARTESIAN_POINT('Origin',(0.,48.85,0.));
#36967=CARTESIAN_POINT('',(-5.35,48.85,-6.55186037543834E-16));
#36968=CARTESIAN_POINT('Origin',(44.98,41.616,12.5));
#36969=CARTESIAN_POINT('',(44.98,41.616,-12.5));
#36970=CARTESIAN_POINT('',(44.98,41.616,12.5));
#36971=CARTESIAN_POINT('',(44.98,41.616,6.25));
#36972=CARTESIAN_POINT('',(44.98,47.,-12.5));
#36973=CARTESIAN_POINT('',(44.98,41.616,-12.5));
#36974=CARTESIAN_POINT('',(44.98,47.,12.5));
#36975=CARTESIAN_POINT('',(44.98,47.,-12.5));
#36976=CARTESIAN_POINT('',(44.98,41.616,12.5));
#36977=CARTESIAN_POINT('Origin',(43.48,41.616,12.5));
#36978=CARTESIAN_POINT('',(43.48,41.616,14.));
#36979=CARTESIAN_POINT('Origin',(43.48,41.616,12.5));
#36980=CARTESIAN_POINT('',(43.48,47.,14.));
#36981=CARTESIAN_POINT('Origin',(43.48,47.,12.5));
#36982=CARTESIAN_POINT('',(43.48,41.616,14.));
#36983=CARTESIAN_POINT('Origin',(-12.12,41.616,12.5));
#36984=CARTESIAN_POINT('',(-12.12,41.616,14.));
#36985=CARTESIAN_POINT('',(-13.62,41.616,12.5));
#36986=CARTESIAN_POINT('Origin',(-12.12,41.616,12.5));
#36987=CARTESIAN_POINT('',(-12.12,47.,14.));
#36988=CARTESIAN_POINT('',(-12.12,41.616,14.));
#36989=CARTESIAN_POINT('',(-13.62,47.,12.5));
#36990=CARTESIAN_POINT('Origin',(-12.12,47.,12.5));
#36991=CARTESIAN_POINT('',(-13.62,41.616,12.5));
#36992=CARTESIAN_POINT('Origin',(-13.62,41.616,-12.5));
#36993=CARTESIAN_POINT('',(-13.62,41.616,-12.5));
#36994=CARTESIAN_POINT('',(-13.62,41.616,-6.25));
#36995=CARTESIAN_POINT('',(-13.62,47.,-12.5));
#36996=CARTESIAN_POINT('',(-13.62,47.,12.5));
#36997=CARTESIAN_POINT('',(-13.62,41.616,-12.5));
#36998=CARTESIAN_POINT('Origin',(-12.12,41.616,-12.5));
#36999=CARTESIAN_POINT('',(-12.12,41.616,-14.));
#37000=CARTESIAN_POINT('Origin',(-12.12,41.616,-12.5));
#37001=CARTESIAN_POINT('',(-12.12,47.,-14.));
#37002=CARTESIAN_POINT('Origin',(-12.12,47.,-12.5));
#37003=CARTESIAN_POINT('',(-12.12,41.616,-14.));
#37004=CARTESIAN_POINT('Origin',(43.48,41.616,-12.5));
#37005=CARTESIAN_POINT('',(43.48,41.616,-14.));
#37006=CARTESIAN_POINT('Origin',(43.48,41.616,-12.5));
#37007=CARTESIAN_POINT('',(43.48,47.,-14.));
#37008=CARTESIAN_POINT('',(43.48,41.616,-14.));
#37009=CARTESIAN_POINT('Origin',(43.48,47.,-12.5));
#37010=CARTESIAN_POINT('Origin',(15.68,47.,0.));
#37011=CARTESIAN_POINT('',(-12.12,47.,-14.));
#37012=CARTESIAN_POINT('',(43.48,47.,14.));
#37013=CARTESIAN_POINT('Origin',(15.68,41.616,-2.22044604925031E-15));
#37014=CARTESIAN_POINT('',(51.68,41.616,14.));
#37015=CARTESIAN_POINT('',(51.68,41.616,14.));
#37016=CARTESIAN_POINT('',(52.68,41.616,13.));
#37017=CARTESIAN_POINT('Origin',(51.68,41.616,13.));
#37018=CARTESIAN_POINT('',(52.68,41.616,-13.));
#37019=CARTESIAN_POINT('',(52.68,41.616,-13.));
#37020=CARTESIAN_POINT('',(51.68,41.616,-14.));
#37021=CARTESIAN_POINT('Origin',(51.68,41.616,-13.));
#37022=CARTESIAN_POINT('',(-20.32,41.616,-14.));
#37023=CARTESIAN_POINT('Origin',(15.68,41.616,-2.22044604925031E-15));
#37024=CARTESIAN_POINT('',(-20.32,41.616,-14.));
#37025=CARTESIAN_POINT('',(-20.32,41.616,-14.));
#37026=CARTESIAN_POINT('',(-21.32,41.616,-13.));
#37027=CARTESIAN_POINT('Origin',(-20.32,41.616,-13.));
#37028=CARTESIAN_POINT('',(-21.32,41.616,13.));
#37029=CARTESIAN_POINT('',(-21.32,41.616,13.));
#37030=CARTESIAN_POINT('',(-20.32,41.616,14.));
#37031=CARTESIAN_POINT('Origin',(-20.32,41.616,13.));
#37032=CARTESIAN_POINT('',(51.68,41.616,14.));
#37033=CARTESIAN_POINT('Origin',(15.68,39.116,-2.22044604925031E-15));
#37034=CARTESIAN_POINT('',(44.6998039027186,39.116,14.));
#37035=CARTESIAN_POINT('',(45.18,39.116,12.9));
#37036=CARTESIAN_POINT('Origin',(43.68,39.116,12.9));
#37037=CARTESIAN_POINT('',(45.18,39.116,-12.9));
#37038=CARTESIAN_POINT('',(45.18,39.116,-12.9));
#37039=CARTESIAN_POINT('',(44.6998039027186,39.116,-14.));
#37040=CARTESIAN_POINT('Origin',(43.68,39.116,-12.9));
#37041=CARTESIAN_POINT('',(51.68,39.116,-14.));
#37042=CARTESIAN_POINT('',(-20.32,39.116,-14.));
#37043=CARTESIAN_POINT('',(52.68,39.116,-13.));
#37044=CARTESIAN_POINT('Origin',(51.68,39.116,-13.));
#37045=CARTESIAN_POINT('',(52.68,39.116,13.));
#37046=CARTESIAN_POINT('',(52.68,39.116,-13.));
#37047=CARTESIAN_POINT('',(51.68,39.116,14.));
#37048=CARTESIAN_POINT('Origin',(51.68,39.116,13.));
#37049=CARTESIAN_POINT('',(51.68,39.116,14.));
#37050=CARTESIAN_POINT('Origin',(52.68,39.116,13.));
#37051=CARTESIAN_POINT('',(52.68,39.116,-13.));
#37052=CARTESIAN_POINT('',(52.68,39.116,13.));
#37053=CARTESIAN_POINT('Origin',(51.68,39.116,13.));
#37054=CARTESIAN_POINT('',(51.68,39.116,14.));
#37055=CARTESIAN_POINT('Origin',(-20.32,39.116,14.));
#37056=CARTESIAN_POINT('',(-20.32,39.116,14.));
#37057=CARTESIAN_POINT('',(-20.32,39.116,14.));
#37058=CARTESIAN_POINT('',(-13.3398039027186,39.116,14.));
#37059=CARTESIAN_POINT('',(51.68,39.116,14.));
#37060=CARTESIAN_POINT('',(-2.32,39.116,14.));
#37061=CARTESIAN_POINT('Origin',(-20.32,39.116,13.));
#37062=CARTESIAN_POINT('',(-21.32,39.116,13.));
#37063=CARTESIAN_POINT('Origin',(-20.32,39.116,13.));
#37064=CARTESIAN_POINT('',(-21.32,39.116,13.));
#37065=CARTESIAN_POINT('Origin',(-21.32,39.116,-13.));
#37066=CARTESIAN_POINT('',(-21.32,39.116,-13.));
#37067=CARTESIAN_POINT('',(-21.32,39.116,13.));
#37068=CARTESIAN_POINT('',(-21.32,39.116,-13.));
#37069=CARTESIAN_POINT('Origin',(-20.32,39.116,-13.));
#37070=CARTESIAN_POINT('',(-20.32,39.116,-14.));
#37071=CARTESIAN_POINT('Origin',(-20.32,39.116,-13.));
#37072=CARTESIAN_POINT('',(-20.32,39.116,-14.));
#37073=CARTESIAN_POINT('Origin',(51.68,39.116,-14.));
#37074=CARTESIAN_POINT('',(-13.3398039027186,39.116,-14.));
#37075=CARTESIAN_POINT('',(-20.32,39.116,-14.));
#37076=CARTESIAN_POINT('',(51.68,39.116,-14.));
#37077=CARTESIAN_POINT('',(33.68,39.116,-14.));
#37078=CARTESIAN_POINT('Origin',(51.68,39.116,-13.));
#37079=CARTESIAN_POINT('Origin',(15.68,39.116,-2.22044604925031E-15));
#37080=CARTESIAN_POINT('',(-13.82,39.116,12.9));
#37081=CARTESIAN_POINT('Origin',(-12.32,39.116,12.9));
#37082=CARTESIAN_POINT('',(-13.82,39.116,-12.9));
#37083=CARTESIAN_POINT('Origin',(-12.32,39.116,-12.9));
#37084=CARTESIAN_POINT('',(-13.82,39.116,12.9));
#37085=CARTESIAN_POINT('Origin',(15.68,39.116,0.));
#37086=CARTESIAN_POINT('',(43.68,39.116,-14.4));
#37087=CARTESIAN_POINT('Origin',(43.68,39.116,-12.9));
#37088=CARTESIAN_POINT('',(-12.32,39.116,-14.4));
#37089=CARTESIAN_POINT('',(-12.32,39.116,-14.4));
#37090=CARTESIAN_POINT('Origin',(-12.32,39.116,-12.9));
#37091=CARTESIAN_POINT('Origin',(45.18,0.,12.9));
#37092=CARTESIAN_POINT('',(45.18,0.,-12.9));
#37093=CARTESIAN_POINT('',(45.18,0.,12.9));
#37094=CARTESIAN_POINT('',(45.18,0.,-12.9));
#37095=CARTESIAN_POINT('',(45.18,0.,-12.9));
#37096=CARTESIAN_POINT('',(45.18,0.,12.9));
#37097=CARTESIAN_POINT('Origin',(43.68,0.,12.9));
#37098=CARTESIAN_POINT('',(43.68,0.,14.4));
#37099=CARTESIAN_POINT('Origin',(43.68,0.,12.9));
#37100=CARTESIAN_POINT('',(43.68,39.116,14.4));
#37101=CARTESIAN_POINT('Origin',(43.68,39.116,12.9));
#37102=CARTESIAN_POINT('',(43.68,0.,14.4));
#37103=CARTESIAN_POINT('Origin',(-12.32,0.,14.4));
#37104=CARTESIAN_POINT('',(-12.32,0.,14.4));
#37105=CARTESIAN_POINT('',(43.68,0.,14.4));
#37106=CARTESIAN_POINT('',(-12.32,39.116,14.4));
#37107=CARTESIAN_POINT('',(43.68,39.116,14.4));
#37108=CARTESIAN_POINT('',(-12.32,0.,14.4));
#37109=CARTESIAN_POINT('Origin',(-12.32,0.,12.9));
#37110=CARTESIAN_POINT('',(-13.82,0.,12.9));
#37111=CARTESIAN_POINT('Origin',(-12.32,0.,12.9));
#37112=CARTESIAN_POINT('Origin',(-12.32,39.116,12.9));
#37113=CARTESIAN_POINT('',(-13.82,0.,12.9));
#37114=CARTESIAN_POINT('Origin',(-13.82,0.,-12.9));
#37115=CARTESIAN_POINT('',(-13.82,0.,-12.9));
#37116=CARTESIAN_POINT('',(-13.82,0.,12.9));
#37117=CARTESIAN_POINT('',(-13.82,0.,-12.9));
#37118=CARTESIAN_POINT('Origin',(-12.32,0.,-12.9));
#37119=CARTESIAN_POINT('',(-12.32,0.,-14.4));
#37120=CARTESIAN_POINT('Origin',(-12.32,0.,-12.9));
#37121=CARTESIAN_POINT('',(-12.32,0.,-14.4));
#37122=CARTESIAN_POINT('Origin',(43.68,0.,-14.4));
#37123=CARTESIAN_POINT('',(43.68,0.,-14.4));
#37124=CARTESIAN_POINT('',(-12.32,0.,-14.4));
#37125=CARTESIAN_POINT('',(43.68,0.,-14.4));
#37126=CARTESIAN_POINT('Origin',(43.68,0.,-12.9));
#37127=CARTESIAN_POINT('Origin',(43.68,0.,-12.9));
#37128=CARTESIAN_POINT('Origin',(15.68,39.116,0.));
#37129=CARTESIAN_POINT('Origin',(15.68,0.,0.));
#37130=CARTESIAN_POINT('',(0.,0.,0.));
#37131=CARTESIAN_POINT('Origin',(1.66039107437149,57.495,5.73138421404289));
#37132=CARTESIAN_POINT('',(1.4909173120086,51.145,5.1463899549833));
#37133=CARTESIAN_POINT('',(1.4909173120086,57.495,5.1463899549833));
#37134=CARTESIAN_POINT('',(1.4909173120086,54.32,5.1463899549833));
#37135=CARTESIAN_POINT('',(1.66039107437149,51.145,5.73138421404289));
#37136=CARTESIAN_POINT('',(1.66039107437149,51.145,5.73138421404289));
#37137=CARTESIAN_POINT('',(1.66039107437149,57.495,5.73138421404289));
#37138=CARTESIAN_POINT('',(1.66039107437149,57.495,5.73138421404289));
#37139=CARTESIAN_POINT('',(1.66039107437149,57.495,5.73138421404289));
#37140=CARTESIAN_POINT('Origin',(6.23660068148934E-13,57.495,1.50456066262064E-12));
#37141=CARTESIAN_POINT('',(2.50394540602693,57.495,6.6908141061934));
#37142=CARTESIAN_POINT('',(2.96056324982543,57.495,6.5016768024705));
#37143=CARTESIAN_POINT('Origin',(6.23660068148934E-13,57.495,1.50456066262064E-12));
#37144=CARTESIAN_POINT('',(2.50394540602693,51.145,6.6908141061934));
#37145=CARTESIAN_POINT('',(2.50394540602693,57.495,6.6908141061934));
#37146=CARTESIAN_POINT('',(2.96056324982543,51.145,6.5016768024705));
#37147=CARTESIAN_POINT('Origin',(6.23660068148934E-13,51.145,1.50456066262064E-12));
#37148=CARTESIAN_POINT('',(2.96056324982543,57.495,6.5016768024705));
#37149=CARTESIAN_POINT('Ctrl Pts',(2.87862685522557,57.495,5.22677443144495));
#37150=CARTESIAN_POINT('Ctrl Pts',(2.87862685522557,49.875,5.22677443144495));
#37151=CARTESIAN_POINT('Ctrl Pts',(2.88043681055508,57.495,5.23024117954544));
#37152=CARTESIAN_POINT('Ctrl Pts',(2.88043681055508,49.875,5.23024117954544));
#37153=CARTESIAN_POINT('Ctrl Pts',(2.88406558980908,57.495,5.2374521593957));
#37154=CARTESIAN_POINT('Ctrl Pts',(2.88406558980908,49.875,5.2374521593957));
#37155=CARTESIAN_POINT('Ctrl Pts',(2.88953536864324,57.495,5.24910109063627));
#37156=CARTESIAN_POINT('Ctrl Pts',(2.88953536864324,49.875,5.24910109063627));
#37157=CARTESIAN_POINT('Ctrl Pts',(2.8968816873652,57.495,5.26630084561717));
#37158=CARTESIAN_POINT('Ctrl Pts',(2.8968816873652,49.875,5.26630084561717));
#37159=CARTESIAN_POINT('Ctrl Pts',(2.90614521320845,57.495,5.29057828960674));
#37160=CARTESIAN_POINT('Ctrl Pts',(2.90614521320845,49.875,5.29057828960674));
#37161=CARTESIAN_POINT('Ctrl Pts',(2.91546314862894,57.495,5.31759510370885));
#37162=CARTESIAN_POINT('Ctrl Pts',(2.91546314862894,49.875,5.31759510370885));
#37163=CARTESIAN_POINT('Ctrl Pts',(2.92478335875772,57.495,5.34725389048201));
#37164=CARTESIAN_POINT('Ctrl Pts',(2.92478335875772,49.875,5.34725389048201));
#37165=CARTESIAN_POINT('Ctrl Pts',(2.93401523982667,57.495,5.37936310952306));
#37166=CARTESIAN_POINT('Ctrl Pts',(2.93401523982667,49.875,5.37936310952306));
#37167=CARTESIAN_POINT('Ctrl Pts',(2.94303247002252,57.495,5.41364129622042));
#37168=CARTESIAN_POINT('Ctrl Pts',(2.94303247002252,49.875,5.41364129622042));
#37169=CARTESIAN_POINT('Ctrl Pts',(2.95169462080126,57.495,5.44977003302479));
#37170=CARTESIAN_POINT('Ctrl Pts',(2.95169462080126,49.875,5.44977003302479));
#37171=CARTESIAN_POINT('Ctrl Pts',(2.95986479289849,57.495,5.48743586913294));
#37172=CARTESIAN_POINT('Ctrl Pts',(2.95986479289849,49.875,5.48743586913294));
#37173=CARTESIAN_POINT('Ctrl Pts',(2.96742703426686,57.495,5.52637191504897));
#37174=CARTESIAN_POINT('Ctrl Pts',(2.96742703426686,49.875,5.52637191504897));
#37175=CARTESIAN_POINT('Ctrl Pts',(2.97430877025614,57.495,5.56641026634754));
#37176=CARTESIAN_POINT('Ctrl Pts',(2.97430877025614,49.875,5.56641026634754));
#37177=CARTESIAN_POINT('Ctrl Pts',(2.98047914221006,57.495,5.60747882861056));
#37178=CARTESIAN_POINT('Ctrl Pts',(2.98047914221006,49.875,5.60747882861056));
#37179=CARTESIAN_POINT('Ctrl Pts',(2.98593308820276,57.495,5.64956501668965));
#37180=CARTESIAN_POINT('Ctrl Pts',(2.98593308820276,49.875,5.64956501668965));
#37181=CARTESIAN_POINT('Ctrl Pts',(2.99067972442542,57.495,5.6926888242775));
#37182=CARTESIAN_POINT('Ctrl Pts',(2.99067972442542,49.875,5.6926888242775));
#37183=CARTESIAN_POINT('Ctrl Pts',(2.99473015701059,57.495,5.73687442119609));
#37184=CARTESIAN_POINT('Ctrl Pts',(2.99473015701059,49.875,5.73687442119609));
#37185=CARTESIAN_POINT('Ctrl Pts',(2.99808342690941,57.495,5.78211642456377));
#37186=CARTESIAN_POINT('Ctrl Pts',(2.99808342690941,49.875,5.78211642456377));
#37187=CARTESIAN_POINT('Ctrl Pts',(3.00072490941926,57.495,5.82837721216371));
#37188=CARTESIAN_POINT('Ctrl Pts',(3.00072490941926,49.875,5.82837721216371));
#37189=CARTESIAN_POINT('Ctrl Pts',(3.00263159433907,57.495,5.87560110342618));
#37190=CARTESIAN_POINT('Ctrl Pts',(3.00263159433907,49.875,5.87560110342618));
#37191=CARTESIAN_POINT('Ctrl Pts',(3.00377540211876,57.495,5.92372322806235));
#37192=CARTESIAN_POINT('Ctrl Pts',(3.00377540211876,49.875,5.92372322806235));
#37193=CARTESIAN_POINT('Ctrl Pts',(3.00412716938112,57.495,5.97267956506957));
#37194=CARTESIAN_POINT('Ctrl Pts',(3.00412716938112,49.875,5.97267956506957));
#37195=CARTESIAN_POINT('Ctrl Pts',(3.0036611362189,57.495,6.02241806591682));
#37196=CARTESIAN_POINT('Ctrl Pts',(3.0036611362189,49.875,6.02241806591682));
#37197=CARTESIAN_POINT('Ctrl Pts',(3.00235671375976,57.495,6.07290162599645));
#37198=CARTESIAN_POINT('Ctrl Pts',(3.00235671375976,49.875,6.07290162599645));
#37199=CARTESIAN_POINT('Ctrl Pts',(3.00019778316116,57.495,6.12410381716763));
#37200=CARTESIAN_POINT('Ctrl Pts',(3.00019778316116,49.875,6.12410381716763));
#37201=CARTESIAN_POINT('Ctrl Pts',(2.99717295692923,57.495,6.17600655789219));
#37202=CARTESIAN_POINT('Ctrl Pts',(2.99717295692923,49.875,6.17600655789219));
#37203=CARTESIAN_POINT('Ctrl Pts',(2.9932755486881,57.495,6.22859706400143));
#37204=CARTESIAN_POINT('Ctrl Pts',(2.9932755486881,49.875,6.22859706400143));
#37205=CARTESIAN_POINT('Ctrl Pts',(2.98850417352762,57.495,6.28186459845025));
#37206=CARTESIAN_POINT('Ctrl Pts',(2.98850417352762,49.875,6.28186459845025));
#37207=CARTESIAN_POINT('Ctrl Pts',(2.98286238364848,57.495,6.33579850967655));
#37208=CARTESIAN_POINT('Ctrl Pts',(2.98286238364848,49.875,6.33579850967655));
#37209=CARTESIAN_POINT('Ctrl Pts',(2.97635619664327,57.495,6.39038953466525));
#37210=CARTESIAN_POINT('Ctrl Pts',(2.97635619664327,49.875,6.39038953466525));
#37211=CARTESIAN_POINT('Ctrl Pts',(2.97046502832938,57.495,6.43458214159119));
#37212=CARTESIAN_POINT('Ctrl Pts',(2.97046502832938,49.875,6.43458214159119));
#37213=CARTESIAN_POINT('Ctrl Pts',(2.96566304810545,57.495,6.4680168144459));
#37214=CARTESIAN_POINT('Ctrl Pts',(2.96566304810545,49.875,6.4680168144459));
#37215=CARTESIAN_POINT('Ctrl Pts',(2.96229154623624,57.495,6.49043534784125));
#37216=CARTESIAN_POINT('Ctrl Pts',(2.96229154623624,49.875,6.49043534784125));
#37217=CARTESIAN_POINT('Ctrl Pts',(2.96056324982543,57.495,6.5016768024705));
#37218=CARTESIAN_POINT('Ctrl Pts',(2.96056324982543,49.875,6.5016768024705));
#37219=CARTESIAN_POINT('',(2.87862685522557,57.495,5.22677443144495));
#37220=CARTESIAN_POINT('Ctrl Pts',(2.87862685522557,57.495,5.22677443144495));
#37221=CARTESIAN_POINT('Ctrl Pts',(2.88043681055508,57.495,5.23024117954544));
#37222=CARTESIAN_POINT('Ctrl Pts',(2.88406558980908,57.495,5.2374521593957));
#37223=CARTESIAN_POINT('Ctrl Pts',(2.88953536864324,57.495,5.24910109063627));
#37224=CARTESIAN_POINT('Ctrl Pts',(2.8968816873652,57.495,5.26630084561717));
#37225=CARTESIAN_POINT('Ctrl Pts',(2.90614521320845,57.495,5.29057828960674));
#37226=CARTESIAN_POINT('Ctrl Pts',(2.91546314862894,57.495,5.31759510370885));
#37227=CARTESIAN_POINT('Ctrl Pts',(2.92478335875772,57.495,5.34725389048201));
#37228=CARTESIAN_POINT('Ctrl Pts',(2.93401523982667,57.495,5.37936310952306));
#37229=CARTESIAN_POINT('Ctrl Pts',(2.94303247002252,57.495,5.41364129622042));
#37230=CARTESIAN_POINT('Ctrl Pts',(2.95169462080126,57.495,5.44977003302479));
#37231=CARTESIAN_POINT('Ctrl Pts',(2.95986479289849,57.495,5.48743586913294));
#37232=CARTESIAN_POINT('Ctrl Pts',(2.96742703426686,57.495,5.52637191504897));
#37233=CARTESIAN_POINT('Ctrl Pts',(2.97430877025614,57.495,5.56641026634754));
#37234=CARTESIAN_POINT('Ctrl Pts',(2.98047914221006,57.495,5.60747882861056));
#37235=CARTESIAN_POINT('Ctrl Pts',(2.98593308820276,57.495,5.64956501668965));
#37236=CARTESIAN_POINT('Ctrl Pts',(2.99067972442542,57.495,5.6926888242775));
#37237=CARTESIAN_POINT('Ctrl Pts',(2.99473015701059,57.495,5.73687442119609));
#37238=CARTESIAN_POINT('Ctrl Pts',(2.99808342690941,57.495,5.78211642456377));
#37239=CARTESIAN_POINT('Ctrl Pts',(3.00072490941926,57.495,5.82837721216371));
#37240=CARTESIAN_POINT('Ctrl Pts',(3.00263159433907,57.495,5.87560110342618));
#37241=CARTESIAN_POINT('Ctrl Pts',(3.00377540211876,57.495,5.92372322806235));
#37242=CARTESIAN_POINT('Ctrl Pts',(3.00412716938112,57.495,5.97267956506957));
#37243=CARTESIAN_POINT('Ctrl Pts',(3.0036611362189,57.495,6.02241806591682));
#37244=CARTESIAN_POINT('Ctrl Pts',(3.00235671375976,57.495,6.07290162599645));
#37245=CARTESIAN_POINT('Ctrl Pts',(3.00019778316116,57.495,6.12410381716763));
#37246=CARTESIAN_POINT('Ctrl Pts',(2.99717295692923,57.495,6.17600655789219));
#37247=CARTESIAN_POINT('Ctrl Pts',(2.9932755486881,57.495,6.22859706400143));
#37248=CARTESIAN_POINT('Ctrl Pts',(2.98850417352762,57.495,6.28186459845025));
#37249=CARTESIAN_POINT('Ctrl Pts',(2.98286238364848,57.495,6.33579850967655));
#37250=CARTESIAN_POINT('Ctrl Pts',(2.97635619664327,57.495,6.39038953466525));
#37251=CARTESIAN_POINT('Ctrl Pts',(2.97046502832938,57.495,6.43458214159119));
#37252=CARTESIAN_POINT('Ctrl Pts',(2.96566304810545,57.495,6.4680168144459));
#37253=CARTESIAN_POINT('Ctrl Pts',(2.96229154623624,57.495,6.49043534784125));
#37254=CARTESIAN_POINT('Ctrl Pts',(2.96056324982543,57.495,6.5016768024705));
#37255=CARTESIAN_POINT('',(2.87862685522557,51.145,5.22677443144495));
#37256=CARTESIAN_POINT('Ctrl Pts',(2.87862685522557,51.145,5.22677443144495));
#37257=CARTESIAN_POINT('Ctrl Pts',(2.88043681055508,51.145,5.23024117954544));
#37258=CARTESIAN_POINT('Ctrl Pts',(2.88406558980908,51.145,5.2374521593957));
#37259=CARTESIAN_POINT('Ctrl Pts',(2.88953536864324,51.145,5.24910109063627));
#37260=CARTESIAN_POINT('Ctrl Pts',(2.8968816873652,51.145,5.26630084561717));
#37261=CARTESIAN_POINT('Ctrl Pts',(2.90614521320845,51.145,5.29057828960674));
#37262=CARTESIAN_POINT('Ctrl Pts',(2.91546314862894,51.145,5.31759510370885));
#37263=CARTESIAN_POINT('Ctrl Pts',(2.92478335875772,51.145,5.34725389048201));
#37264=CARTESIAN_POINT('Ctrl Pts',(2.93401523982667,51.145,5.37936310952306));
#37265=CARTESIAN_POINT('Ctrl Pts',(2.94303247002252,51.145,5.41364129622042));
#37266=CARTESIAN_POINT('Ctrl Pts',(2.95169462080126,51.145,5.44977003302479));
#37267=CARTESIAN_POINT('Ctrl Pts',(2.95986479289849,51.145,5.48743586913294));
#37268=CARTESIAN_POINT('Ctrl Pts',(2.96742703426686,51.145,5.52637191504897));
#37269=CARTESIAN_POINT('Ctrl Pts',(2.97430877025614,51.145,5.56641026634754));
#37270=CARTESIAN_POINT('Ctrl Pts',(2.98047914221006,51.145,5.60747882861056));
#37271=CARTESIAN_POINT('Ctrl Pts',(2.98593308820276,51.145,5.64956501668965));
#37272=CARTESIAN_POINT('Ctrl Pts',(2.99067972442542,51.145,5.6926888242775));
#37273=CARTESIAN_POINT('Ctrl Pts',(2.99473015701059,51.145,5.73687442119609));
#37274=CARTESIAN_POINT('Ctrl Pts',(2.99808342690941,51.145,5.78211642456377));
#37275=CARTESIAN_POINT('Ctrl Pts',(3.00072490941926,51.145,5.82837721216371));
#37276=CARTESIAN_POINT('Ctrl Pts',(3.00263159433907,51.145,5.87560110342618));
#37277=CARTESIAN_POINT('Ctrl Pts',(3.00377540211876,51.145,5.92372322806235));
#37278=CARTESIAN_POINT('Ctrl Pts',(3.00412716938112,51.145,5.97267956506957));
#37279=CARTESIAN_POINT('Ctrl Pts',(3.0036611362189,51.145,6.02241806591682));
#37280=CARTESIAN_POINT('Ctrl Pts',(3.00235671375976,51.145,6.07290162599645));
#37281=CARTESIAN_POINT('Ctrl Pts',(3.00019778316116,51.145,6.12410381716763));
#37282=CARTESIAN_POINT('Ctrl Pts',(2.99717295692923,51.145,6.17600655789219));
#37283=CARTESIAN_POINT('Ctrl Pts',(2.9932755486881,51.145,6.22859706400143));
#37284=CARTESIAN_POINT('Ctrl Pts',(2.98850417352762,51.145,6.28186459845025));
#37285=CARTESIAN_POINT('Ctrl Pts',(2.98286238364848,51.145,6.33579850967655));
#37286=CARTESIAN_POINT('Ctrl Pts',(2.97635619664327,51.145,6.39038953466525));
#37287=CARTESIAN_POINT('Ctrl Pts',(2.97046502832938,51.145,6.43458214159119));
#37288=CARTESIAN_POINT('Ctrl Pts',(2.96566304810545,51.145,6.4680168144459));
#37289=CARTESIAN_POINT('Ctrl Pts',(2.96229154623624,51.145,6.49043534784125));
#37290=CARTESIAN_POINT('Ctrl Pts',(2.96056324982543,51.145,6.5016768024705));
#37291=CARTESIAN_POINT('',(2.87862685522557,57.495,5.22677443144495));
#37292=CARTESIAN_POINT('Origin',(2.51244640654327,57.495,4.56189402049717));
#37293=CARTESIAN_POINT('',(2.58480949428933,57.495,4.69328497730872));
#37294=CARTESIAN_POINT('',(2.58480949428933,51.145,4.69328497730872));
#37295=CARTESIAN_POINT('',(2.58480949428933,54.32,4.69328497730872));
#37296=CARTESIAN_POINT('',(2.51244640654327,57.495,4.56189402049717));
#37297=CARTESIAN_POINT('',(2.51244640654327,51.145,4.56189402049717));
#37298=CARTESIAN_POINT('Ctrl Pts',(2.50394540602693,57.495,6.6908141061934));
#37299=CARTESIAN_POINT('Ctrl Pts',(2.50394540602693,49.875,6.6908141061934));
#37300=CARTESIAN_POINT('Ctrl Pts',(2.49477440711623,57.495,6.6840872875067));
#37301=CARTESIAN_POINT('Ctrl Pts',(2.49477440711623,49.875,6.6840872875067));
#37302=CARTESIAN_POINT('Ctrl Pts',(2.47653809829367,57.495,6.67061900235319));
#37303=CARTESIAN_POINT('Ctrl Pts',(2.47653809829367,49.875,6.67061900235319));
#37304=CARTESIAN_POINT('Ctrl Pts',(2.44950070161195,57.495,6.65037263123044));
#37305=CARTESIAN_POINT('Ctrl Pts',(2.44950070161195,49.875,6.65037263123044));
#37306=CARTESIAN_POINT('Ctrl Pts',(2.41408612451248,57.495,6.62328942425873));
#37307=CARTESIAN_POINT('Ctrl Pts',(2.41408612451248,49.875,6.62328942425873));
#37308=CARTESIAN_POINT('Ctrl Pts',(2.37088387159998,57.495,6.58928830924832));
#37309=CARTESIAN_POINT('Ctrl Pts',(2.37088387159998,49.875,6.58928830924832));
#37310=CARTESIAN_POINT('Ctrl Pts',(2.32875748935431,57.495,6.55514062276576));
#37311=CARTESIAN_POINT('Ctrl Pts',(2.32875748935431,49.875,6.55514062276576));
#37312=CARTESIAN_POINT('Ctrl Pts',(2.28771778279682,57.495,6.52084865967131));
#37313=CARTESIAN_POINT('Ctrl Pts',(2.28771778279682,49.875,6.52084865967131));
#37314=CARTESIAN_POINT('Ctrl Pts',(2.24777479550452,57.495,6.48641743997165));
#37315=CARTESIAN_POINT('Ctrl Pts',(2.24777479550452,49.875,6.48641743997165));
#37316=CARTESIAN_POINT('Ctrl Pts',(2.20893514043546,57.495,6.45185553518355));
#37317=CARTESIAN_POINT('Ctrl Pts',(2.20893514043546,49.875,6.45185553518355));
#37318=CARTESIAN_POINT('Ctrl Pts',(2.17120312938033,57.495,6.41717671306116));
#37319=CARTESIAN_POINT('Ctrl Pts',(2.17120312938033,49.875,6.41717671306116));
#37320=CARTESIAN_POINT('Ctrl Pts',(2.13458349574322,57.495,6.38240181135686));
#37321=CARTESIAN_POINT('Ctrl Pts',(2.13458349574322,49.875,6.38240181135686));
#37322=CARTESIAN_POINT('Ctrl Pts',(2.09908352929886,57.495,6.34756091533109));
#37323=CARTESIAN_POINT('Ctrl Pts',(2.09908352929886,49.875,6.34756091533109));
#37324=CARTESIAN_POINT('Ctrl Pts',(2.06471490843566,57.495,6.31269482043472));
#37325=CARTESIAN_POINT('Ctrl Pts',(2.06471490843566,49.875,6.31269482043472));
#37326=CARTESIAN_POINT('Ctrl Pts',(2.03149622201774,57.495,6.27785854554207));
#37327=CARTESIAN_POINT('Ctrl Pts',(2.03149622201774,49.875,6.27785854554207));
#37328=CARTESIAN_POINT('Ctrl Pts',(1.99945211810842,57.495,6.24311798195999));
#37329=CARTESIAN_POINT('Ctrl Pts',(1.99945211810842,49.875,6.24311798195999));
#37330=CARTESIAN_POINT('Ctrl Pts',(1.96860861168855,57.495,6.20853885514991));
#37331=CARTESIAN_POINT('Ctrl Pts',(1.96860861168855,49.875,6.20853885514991));
#37332=CARTESIAN_POINT('Ctrl Pts',(1.93898880419739,57.495,6.17417680788948));
#37333=CARTESIAN_POINT('Ctrl Pts',(1.93898880419739,49.875,6.17417680788948));
#37334=CARTESIAN_POINT('Ctrl Pts',(1.91060895733316,57.495,6.14006878432979));
#37335=CARTESIAN_POINT('Ctrl Pts',(1.91060895733316,49.875,6.14006878432979));
#37336=CARTESIAN_POINT('Ctrl Pts',(1.88347219921808,57.495,6.10621926889293));
#37337=CARTESIAN_POINT('Ctrl Pts',(1.88347219921808,49.875,6.10621926889293));
#37338=CARTESIAN_POINT('Ctrl Pts',(1.85756929242873,57.495,6.07260331771223));
#37339=CARTESIAN_POINT('Ctrl Pts',(1.85756929242873,49.875,6.07260331771223));
#37340=CARTESIAN_POINT('Ctrl Pts',(1.83289254541003,57.495,6.03920034699142));
#37341=CARTESIAN_POINT('Ctrl Pts',(1.83289254541003,49.875,6.03920034699142));
#37342=CARTESIAN_POINT('Ctrl Pts',(1.80944727788364,57.495,6.00602283509636));
#37343=CARTESIAN_POINT('Ctrl Pts',(1.80944727788364,49.875,6.00602283509636));
#37344=CARTESIAN_POINT('Ctrl Pts',(1.78726264793637,57.495,5.97314358084405));
#37345=CARTESIAN_POINT('Ctrl Pts',(1.78726264793637,49.875,5.97314358084405));
#37346=CARTESIAN_POINT('Ctrl Pts',(1.76640606389863,57.495,5.94073262861954));
#37347=CARTESIAN_POINT('Ctrl Pts',(1.76640606389863,49.875,5.94073262861954));
#37348=CARTESIAN_POINT('Ctrl Pts',(1.74698425466385,57.495,5.90906068827417));
#37349=CARTESIAN_POINT('Ctrl Pts',(1.74698425466385,49.875,5.90906068827417));
#37350=CARTESIAN_POINT('Ctrl Pts',(1.72912206102238,57.495,5.87844620539466));
#37351=CARTESIAN_POINT('Ctrl Pts',(1.72912206102238,49.875,5.87844620539466));
#37352=CARTESIAN_POINT('Ctrl Pts',(1.71294534020682,57.495,5.84921363316514));
#37353=CARTESIAN_POINT('Ctrl Pts',(1.71294534020682,49.875,5.84921363316514));
#37354=CARTESIAN_POINT('Ctrl Pts',(1.69856379474193,57.495,5.8216513201319));
#37355=CARTESIAN_POINT('Ctrl Pts',(1.69856379474193,49.875,5.8216513201319));
#37356=CARTESIAN_POINT('Ctrl Pts',(1.68604879760681,57.495,5.79595877235173));
#37357=CARTESIAN_POINT('Ctrl Pts',(1.68604879760681,49.875,5.79595877235173));
#37358=CARTESIAN_POINT('Ctrl Pts',(1.67543235427339,57.495,5.77224172513534));
#37359=CARTESIAN_POINT('Ctrl Pts',(1.67543235427339,49.875,5.77224172513534));
#37360=CARTESIAN_POINT('Ctrl Pts',(1.6684649226767,57.495,5.75488502996854));
#37361=CARTESIAN_POINT('Ctrl Pts',(1.6684649226767,49.875,5.75488502996854));
#37362=CARTESIAN_POINT('Ctrl Pts',(1.66409560210811,57.495,5.74278027398956));
#37363=CARTESIAN_POINT('Ctrl Pts',(1.66409560210811,49.875,5.74278027398956));
#37364=CARTESIAN_POINT('Ctrl Pts',(1.66156260377489,57.495,5.73511540682054));
#37365=CARTESIAN_POINT('Ctrl Pts',(1.66156260377489,49.875,5.73511540682054));
#37366=CARTESIAN_POINT('Ctrl Pts',(1.66039107437149,57.495,5.73138421404289));
#37367=CARTESIAN_POINT('Ctrl Pts',(1.66039107437149,49.875,5.73138421404289));
#37368=CARTESIAN_POINT('Ctrl Pts',(1.66039107437149,57.495,5.73138421404289));
#37369=CARTESIAN_POINT('Ctrl Pts',(1.66156260377489,57.495,5.73511540682054));
#37370=CARTESIAN_POINT('Ctrl Pts',(1.66409560210811,57.495,5.74278027398956));
#37371=CARTESIAN_POINT('Ctrl Pts',(1.6684649226767,57.495,5.75488502996854));
#37372=CARTESIAN_POINT('Ctrl Pts',(1.67543235427339,57.495,5.77224172513534));
#37373=CARTESIAN_POINT('Ctrl Pts',(1.68604879760681,57.495,5.79595877235173));
#37374=CARTESIAN_POINT('Ctrl Pts',(1.69856379474193,57.495,5.8216513201319));
#37375=CARTESIAN_POINT('Ctrl Pts',(1.71294534020682,57.495,5.84921363316514));
#37376=CARTESIAN_POINT('Ctrl Pts',(1.72912206102238,57.495,5.87844620539466));
#37377=CARTESIAN_POINT('Ctrl Pts',(1.74698425466385,57.495,5.90906068827417));
#37378=CARTESIAN_POINT('Ctrl Pts',(1.76640606389863,57.495,5.94073262861954));
#37379=CARTESIAN_POINT('Ctrl Pts',(1.78726264793637,57.495,5.97314358084405));
#37380=CARTESIAN_POINT('Ctrl Pts',(1.80944727788364,57.495,6.00602283509636));
#37381=CARTESIAN_POINT('Ctrl Pts',(1.83289254541003,57.495,6.03920034699142));
#37382=CARTESIAN_POINT('Ctrl Pts',(1.85756929242873,57.495,6.07260331771223));
#37383=CARTESIAN_POINT('Ctrl Pts',(1.88347219921808,57.495,6.10621926889293));
#37384=CARTESIAN_POINT('Ctrl Pts',(1.91060895733316,57.495,6.14006878432979));
#37385=CARTESIAN_POINT('Ctrl Pts',(1.93898880419739,57.495,6.17417680788948));
#37386=CARTESIAN_POINT('Ctrl Pts',(1.96860861168855,57.495,6.20853885514991));
#37387=CARTESIAN_POINT('Ctrl Pts',(1.99945211810842,57.495,6.24311798195999));
#37388=CARTESIAN_POINT('Ctrl Pts',(2.03149622201774,57.495,6.27785854554207));
#37389=CARTESIAN_POINT('Ctrl Pts',(2.06471490843566,57.495,6.31269482043472));
#37390=CARTESIAN_POINT('Ctrl Pts',(2.09908352929886,57.495,6.34756091533109));
#37391=CARTESIAN_POINT('Ctrl Pts',(2.13458349574322,57.495,6.38240181135686));
#37392=CARTESIAN_POINT('Ctrl Pts',(2.17120312938033,57.495,6.41717671306116));
#37393=CARTESIAN_POINT('Ctrl Pts',(2.20893514043546,57.495,6.45185553518355));
#37394=CARTESIAN_POINT('Ctrl Pts',(2.24777479550452,57.495,6.48641743997165));
#37395=CARTESIAN_POINT('Ctrl Pts',(2.28771778279682,57.495,6.52084865967131));
#37396=CARTESIAN_POINT('Ctrl Pts',(2.32875748935431,57.495,6.55514062276576));
#37397=CARTESIAN_POINT('Ctrl Pts',(2.37088387159998,57.495,6.58928830924832));
#37398=CARTESIAN_POINT('Ctrl Pts',(2.41408612451248,57.495,6.62328942425873));
#37399=CARTESIAN_POINT('Ctrl Pts',(2.44950070161195,57.495,6.65037263123044));
#37400=CARTESIAN_POINT('Ctrl Pts',(2.47653809829367,57.495,6.67061900235319));
#37401=CARTESIAN_POINT('Ctrl Pts',(2.49477440711623,57.495,6.6840872875067));
#37402=CARTESIAN_POINT('Ctrl Pts',(2.50394540602693,57.495,6.6908141061934));
#37403=CARTESIAN_POINT('Ctrl Pts',(2.50394540602693,51.145,6.6908141061934));
#37404=CARTESIAN_POINT('Ctrl Pts',(2.49477440711623,51.145,6.6840872875067));
#37405=CARTESIAN_POINT('Ctrl Pts',(2.47653809829367,51.145,6.67061900235319));
#37406=CARTESIAN_POINT('Ctrl Pts',(2.44950070161195,51.145,6.65037263123044));
#37407=CARTESIAN_POINT('Ctrl Pts',(2.41408612451248,51.145,6.62328942425873));
#37408=CARTESIAN_POINT('Ctrl Pts',(2.37088387159998,51.145,6.58928830924832));
#37409=CARTESIAN_POINT('Ctrl Pts',(2.32875748935431,51.145,6.55514062276576));
#37410=CARTESIAN_POINT('Ctrl Pts',(2.28771778279682,51.145,6.52084865967131));
#37411=CARTESIAN_POINT('Ctrl Pts',(2.24777479550452,51.145,6.48641743997165));
#37412=CARTESIAN_POINT('Ctrl Pts',(2.20893514043546,51.145,6.45185553518355));
#37413=CARTESIAN_POINT('Ctrl Pts',(2.17120312938033,51.145,6.41717671306116));
#37414=CARTESIAN_POINT('Ctrl Pts',(2.13458349574322,51.145,6.38240181135686));
#37415=CARTESIAN_POINT('Ctrl Pts',(2.09908352929886,51.145,6.34756091533109));
#37416=CARTESIAN_POINT('Ctrl Pts',(2.06471490843566,51.145,6.31269482043472));
#37417=CARTESIAN_POINT('Ctrl Pts',(2.03149622201774,51.145,6.27785854554207));
#37418=CARTESIAN_POINT('Ctrl Pts',(1.99945211810842,51.145,6.24311798195999));
#37419=CARTESIAN_POINT('Ctrl Pts',(1.96860861168855,51.145,6.20853885514991));
#37420=CARTESIAN_POINT('Ctrl Pts',(1.93898880419739,51.145,6.17417680788948));
#37421=CARTESIAN_POINT('Ctrl Pts',(1.91060895733316,51.145,6.14006878432979));
#37422=CARTESIAN_POINT('Ctrl Pts',(1.88347219921808,51.145,6.10621926889293));
#37423=CARTESIAN_POINT('Ctrl Pts',(1.85756929242873,51.145,6.07260331771223));
#37424=CARTESIAN_POINT('Ctrl Pts',(1.83289254541003,51.145,6.03920034699142));
#37425=CARTESIAN_POINT('Ctrl Pts',(1.80944727788364,51.145,6.00602283509636));
#37426=CARTESIAN_POINT('Ctrl Pts',(1.78726264793637,51.145,5.97314358084405));
#37427=CARTESIAN_POINT('Ctrl Pts',(1.76640606389863,51.145,5.94073262861954));
#37428=CARTESIAN_POINT('Ctrl Pts',(1.74698425466385,51.145,5.90906068827417));
#37429=CARTESIAN_POINT('Ctrl Pts',(1.72912206102238,51.145,5.87844620539466));
#37430=CARTESIAN_POINT('Ctrl Pts',(1.71294534020682,51.145,5.84921363316514));
#37431=CARTESIAN_POINT('Ctrl Pts',(1.69856379474193,51.145,5.8216513201319));
#37432=CARTESIAN_POINT('Ctrl Pts',(1.68604879760681,51.145,5.79595877235173));
#37433=CARTESIAN_POINT('Ctrl Pts',(1.67543235427339,51.145,5.77224172513534));
#37434=CARTESIAN_POINT('Ctrl Pts',(1.6684649226767,51.145,5.75488502996854));
#37435=CARTESIAN_POINT('Ctrl Pts',(1.66409560210811,51.145,5.74278027398956));
#37436=CARTESIAN_POINT('Ctrl Pts',(1.66156260377489,51.145,5.73511540682054));
#37437=CARTESIAN_POINT('Ctrl Pts',(1.66039107437149,51.145,5.73138421404289));
#37438=CARTESIAN_POINT('Origin',(5.358,57.495,0.));
#37439=CARTESIAN_POINT('',(3.34686616149372,57.495,4.18409499139877));
#37440=CARTESIAN_POINT('Origin',(0.,57.495,0.));
#37441=CARTESIAN_POINT('',(3.72730711280926,57.495,4.65970441290367));
#37442=CARTESIAN_POINT('',(3.72730711280926,57.495,4.65970441290367));
#37443=CARTESIAN_POINT('',(4.87380761862879,57.495,5.22328778611671));
#37444=CARTESIAN_POINT('Ctrl Pts',(3.72730711280926,57.495,4.65970441290367));
#37445=CARTESIAN_POINT('Ctrl Pts',(3.72981733050578,57.495,4.66270326064959));
#37446=CARTESIAN_POINT('Ctrl Pts',(3.73509073349858,57.495,4.66881533805013));
#37447=CARTESIAN_POINT('Ctrl Pts',(3.74375974890886,57.495,4.67832660775287));
#37448=CARTESIAN_POINT('Ctrl Pts',(3.75683893603616,57.495,4.69169578253132));
#37449=CARTESIAN_POINT('Ctrl Pts',(3.77572337177431,57.495,4.7095447400518));
#37450=CARTESIAN_POINT('Ctrl Pts',(3.7971178338476,57.495,4.72849227702426));
#37451=CARTESIAN_POINT('Ctrl Pts',(3.82095228990397,57.495,4.74845295472312));
#37452=CARTESIAN_POINT('Ctrl Pts',(3.84708445224627,57.495,4.76926976684252));
#37453=CARTESIAN_POINT('Ctrl Pts',(3.8753026227458,57.495,4.79071829540103));
#37454=CARTESIAN_POINT('Ctrl Pts',(3.90536636162318,57.495,4.81254694822034));
#37455=CARTESIAN_POINT('Ctrl Pts',(3.93703846717724,57.495,4.83450929444279));
#37456=CARTESIAN_POINT('Ctrl Pts',(3.97011673859274,57.495,4.85639607415676));
#37457=CARTESIAN_POINT('Ctrl Pts',(4.00447382552396,57.495,4.87807598288654));
#37458=CARTESIAN_POINT('Ctrl Pts',(4.04005493051012,57.495,4.89949292161185));
#37459=CARTESIAN_POINT('Ctrl Pts',(4.07685036350539,57.495,4.92063739759521));
#37460=CARTESIAN_POINT('Ctrl Pts',(4.11487510765791,57.495,4.94152548435402));
#37461=CARTESIAN_POINT('Ctrl Pts',(4.15414724283858,57.495,4.96217669200723));
#37462=CARTESIAN_POINT('Ctrl Pts',(4.1946621629253,57.495,4.98258807456961));
#37463=CARTESIAN_POINT('Ctrl Pts',(4.23639070615337,57.495,5.00273172317863));
#37464=CARTESIAN_POINT('Ctrl Pts',(4.27929023600674,57.495,5.02256507114894));
#37465=CARTESIAN_POINT('Ctrl Pts',(4.3233115657319,57.495,5.04203735157412));
#37466=CARTESIAN_POINT('Ctrl Pts',(4.36840670797617,57.495,5.06109712122989));
#37467=CARTESIAN_POINT('Ctrl Pts',(4.41453743405677,57.495,5.07970066295468));
#37468=CARTESIAN_POINT('Ctrl Pts',(4.46167734280651,57.495,5.09781475579217));
#37469=CARTESIAN_POINT('Ctrl Pts',(4.50980818622101,57.495,5.11541439426204));
#37470=CARTESIAN_POINT('Ctrl Pts',(4.5589176169425,57.495,5.13248213818666));
#37471=CARTESIAN_POINT('Ctrl Pts',(4.60899638270439,57.495,5.14900691787064));
#37472=CARTESIAN_POINT('Ctrl Pts',(4.66003509375265,57.495,5.16498334493456));
#37473=CARTESIAN_POINT('Ctrl Pts',(4.71202254995864,57.495,5.18041062500752));
#37474=CARTESIAN_POINT('Ctrl Pts',(4.7649478905793,57.495,5.19529077281773));
#37475=CARTESIAN_POINT('Ctrl Pts',(4.80803098811744,57.495,5.20675982149348));
#37476=CARTESIAN_POINT('Ctrl Pts',(4.84075823631826,57.495,5.21511826561704));
#37477=CARTESIAN_POINT('Ctrl Pts',(4.86276047837859,57.495,5.2205826053545));
#37478=CARTESIAN_POINT('Ctrl Pts',(4.87380761862879,57.495,5.22328778611671));
#37479=CARTESIAN_POINT('',(5.22328778611671,57.495,4.87380761862879));
#37480=CARTESIAN_POINT('Origin',(1.15195721078055E-12,57.495,1.15136842610855E-12));
#37481=CARTESIAN_POINT('',(4.65970441290368,57.495,3.72730711280926));
#37482=CARTESIAN_POINT('Ctrl Pts',(4.65970441290368,57.495,3.72730711280926));
#37483=CARTESIAN_POINT('Ctrl Pts',(4.66270326064961,57.495,3.72981733050576));
#37484=CARTESIAN_POINT('Ctrl Pts',(4.6688153380502,57.495,3.73509073349854));
#37485=CARTESIAN_POINT('Ctrl Pts',(4.67832660775297,57.495,3.7437597489088));
#37486=CARTESIAN_POINT('Ctrl Pts',(4.69169578253142,57.495,3.7568389360361));
#37487=CARTESIAN_POINT('Ctrl Pts',(4.70954474005187,57.495,3.77572337177426));
#37488=CARTESIAN_POINT('Ctrl Pts',(4.72849227702429,57.495,3.79711783384759));
#37489=CARTESIAN_POINT('Ctrl Pts',(4.74845295472311,57.495,3.82095228990398));
#37490=CARTESIAN_POINT('Ctrl Pts',(4.76926976684248,57.495,3.84708445224628));
#37491=CARTESIAN_POINT('Ctrl Pts',(4.79071829540097,57.495,3.87530262274579));
#37492=CARTESIAN_POINT('Ctrl Pts',(4.81254694822028,57.495,3.90536636162316));
#37493=CARTESIAN_POINT('Ctrl Pts',(4.83450929444277,57.495,3.93703846717723));
#37494=CARTESIAN_POINT('Ctrl Pts',(4.85639607415679,57.495,3.97011673859275));
#37495=CARTESIAN_POINT('Ctrl Pts',(4.87807598288661,57.495,4.00447382552398));
#37496=CARTESIAN_POINT('Ctrl Pts',(4.89949292161193,57.495,4.04005493051016));
#37497=CARTESIAN_POINT('Ctrl Pts',(4.92063739759527,57.495,4.07685036350543));
#37498=CARTESIAN_POINT('Ctrl Pts',(4.94152548435404,57.495,4.11487510765792));
#37499=CARTESIAN_POINT('Ctrl Pts',(4.9621766920072,57.495,4.15414724283855));
#37500=CARTESIAN_POINT('Ctrl Pts',(4.98258807456953,57.495,4.19466216292523));
#37501=CARTESIAN_POINT('Ctrl Pts',(5.00273172317852,57.495,4.23639070615327));
#37502=CARTESIAN_POINT('Ctrl Pts',(5.02256507114883,57.495,4.27929023600664));
#37503=CARTESIAN_POINT('Ctrl Pts',(5.04203735157409,57.495,4.32331156573186));
#37504=CARTESIAN_POINT('Ctrl Pts',(5.06109712122993,57.495,4.36840670797621));
#37505=CARTESIAN_POINT('Ctrl Pts',(5.07970066295481,57.495,4.41453743405689));
#37506=CARTESIAN_POINT('Ctrl Pts',(5.09781475579234,57.495,4.46167734280668));
#37507=CARTESIAN_POINT('Ctrl Pts',(5.11541439426219,57.495,4.50980818622117));
#37508=CARTESIAN_POINT('Ctrl Pts',(5.13248213818673,57.495,4.55891761694258));
#37509=CARTESIAN_POINT('Ctrl Pts',(5.14900691787061,57.495,4.60899638270436));
#37510=CARTESIAN_POINT('Ctrl Pts',(5.16498334493441,57.495,4.66003509375248));
#37511=CARTESIAN_POINT('Ctrl Pts',(5.1804106250073,57.495,4.71202254995837));
#37512=CARTESIAN_POINT('Ctrl Pts',(5.1952907728175,57.495,4.764947890579));
#37513=CARTESIAN_POINT('Ctrl Pts',(5.2067598214933,57.495,4.8080309881172));
#37514=CARTESIAN_POINT('Ctrl Pts',(5.21511826561693,57.495,4.84075823631811));
#37515=CARTESIAN_POINT('Ctrl Pts',(5.22058260535447,57.495,4.86276047837853));
#37516=CARTESIAN_POINT('Ctrl Pts',(5.22328778611671,57.495,4.87380761862879));
#37517=CARTESIAN_POINT('',(4.18409499139877,57.495,3.34686616149372));
#37518=CARTESIAN_POINT('',(4.06695907338649,57.495,3.25316890053365));
#37519=CARTESIAN_POINT('',(4.69328497730872,57.495,2.58480949428933));
#37520=CARTESIAN_POINT('Origin',(0.,57.495,0.));
#37521=CARTESIAN_POINT('',(5.22677443144495,57.495,2.87862685522557));
#37522=CARTESIAN_POINT('',(5.22677443144495,57.495,2.87862685522557));
#37523=CARTESIAN_POINT('',(6.50167680247051,57.495,2.96056324982543));
#37524=CARTESIAN_POINT('Ctrl Pts',(5.22677443144495,57.495,2.87862685522557));
#37525=CARTESIAN_POINT('Ctrl Pts',(5.23024117954545,57.495,2.88043681055505));
#37526=CARTESIAN_POINT('Ctrl Pts',(5.23745215939571,57.495,2.88406558980901));
#37527=CARTESIAN_POINT('Ctrl Pts',(5.24910109063628,57.495,2.88953536864313));
#37528=CARTESIAN_POINT('Ctrl Pts',(5.26630084561719,57.495,2.89688168736508));
#37529=CARTESIAN_POINT('Ctrl Pts',(5.29057828960676,57.495,2.90614521320837));
#37530=CARTESIAN_POINT('Ctrl Pts',(5.31759510370885,57.495,2.91546314862892));
#37531=CARTESIAN_POINT('Ctrl Pts',(5.34725389048201,57.495,2.92478335875774));
#37532=CARTESIAN_POINT('Ctrl Pts',(5.37936310952307,57.495,2.93401523982671));
#37533=CARTESIAN_POINT('Ctrl Pts',(5.41364129622045,57.495,2.94303247002258));
#37534=CARTESIAN_POINT('Ctrl Pts',(5.44977003302482,57.495,2.95169462080131));
#37535=CARTESIAN_POINT('Ctrl Pts',(5.48743586913296,57.495,2.9598647928985));
#37536=CARTESIAN_POINT('Ctrl Pts',(5.52637191504895,57.495,2.96742703426683));
#37537=CARTESIAN_POINT('Ctrl Pts',(5.56641026634749,57.495,2.97430877025609));
#37538=CARTESIAN_POINT('Ctrl Pts',(5.60747882861049,57.495,2.98047914221));
#37539=CARTESIAN_POINT('Ctrl Pts',(5.64956501668959,57.495,2.98593308820271));
#37540=CARTESIAN_POINT('Ctrl Pts',(5.69268882427748,57.495,2.9906797244254));
#37541=CARTESIAN_POINT('Ctrl Pts',(5.73687442119613,57.495,2.9947301570106));
#37542=CARTESIAN_POINT('Ctrl Pts',(5.78211642456387,57.495,2.99808342690946));
#37543=CARTESIAN_POINT('Ctrl Pts',(5.82837721216385,57.495,3.00072490941932));
#37544=CARTESIAN_POINT('Ctrl Pts',(5.87560110342631,57.495,3.00263159433912));
#37545=CARTESIAN_POINT('Ctrl Pts',(5.9237232280624,57.495,3.00377540211878));
#37546=CARTESIAN_POINT('Ctrl Pts',(5.97267956506952,57.495,3.00412716938109));
#37547=CARTESIAN_POINT('Ctrl Pts',(6.02241806591666,57.495,3.00366113621883));
#37548=CARTESIAN_POINT('Ctrl Pts',(6.07290162599622,57.495,3.00235671375967));
#37549=CARTESIAN_POINT('Ctrl Pts',(6.12410381716742,57.495,3.00019778316108));
#37550=CARTESIAN_POINT('Ctrl Pts',(6.17600655789209,57.495,2.99717295692919));
#37551=CARTESIAN_POINT('Ctrl Pts',(6.22859706400147,57.495,2.99327554868811));
#37552=CARTESIAN_POINT('Ctrl Pts',(6.28186459845047,57.495,2.98850417352769));
#37553=CARTESIAN_POINT('Ctrl Pts',(6.33579850967689,57.495,2.98286238364858));
#37554=CARTESIAN_POINT('Ctrl Pts',(6.39038953466561,57.495,2.97635619664337));
#37555=CARTESIAN_POINT('Ctrl Pts',(6.43458214159149,57.495,2.97046502832946));
#37556=CARTESIAN_POINT('Ctrl Pts',(6.46801681444607,57.495,2.9656630481055));
#37557=CARTESIAN_POINT('Ctrl Pts',(6.49043534784131,57.495,2.96229154623625));
#37558=CARTESIAN_POINT('Ctrl Pts',(6.50167680247051,57.495,2.96056324982543));
#37559=CARTESIAN_POINT('',(6.69081410619341,57.495,2.50394540602692));
#37560=CARTESIAN_POINT('Origin',(1.50487931058895E-12,57.495,6.22890783902203E-13));
#37561=CARTESIAN_POINT('',(5.73138421404289,57.495,1.66039107437148));
#37562=CARTESIAN_POINT('Ctrl Pts',(5.73138421404289,57.495,1.66039107437148));
#37563=CARTESIAN_POINT('Ctrl Pts',(5.73511540682056,57.495,1.66156260377487));
#37564=CARTESIAN_POINT('Ctrl Pts',(5.7427802739896,57.495,1.66409560210805));
#37565=CARTESIAN_POINT('Ctrl Pts',(5.75488502996861,57.495,1.6684649226766));
#37566=CARTESIAN_POINT('Ctrl Pts',(5.77224172513541,57.495,1.67543235427329));
#37567=CARTESIAN_POINT('Ctrl Pts',(5.79595877235177,57.495,1.68604879760674));
#37568=CARTESIAN_POINT('Ctrl Pts',(5.82165132013192,57.495,1.69856379474191));
#37569=CARTESIAN_POINT('Ctrl Pts',(5.84921363316513,57.495,1.71294534020683));
#37570=CARTESIAN_POINT('Ctrl Pts',(5.87844620539462,57.495,1.72912206102241));
#37571=CARTESIAN_POINT('Ctrl Pts',(5.90906068827411,57.495,1.74698425466387));
#37572=CARTESIAN_POINT('Ctrl Pts',(5.94073262861949,57.495,1.76640606389864));
#37573=CARTESIAN_POINT('Ctrl Pts',(5.97314358084403,57.495,1.78726264793637));
#37574=CARTESIAN_POINT('Ctrl Pts',(6.0060228350964,57.495,1.80944727788364));
#37575=CARTESIAN_POINT('Ctrl Pts',(6.03920034699149,57.495,1.83289254541003));
#37576=CARTESIAN_POINT('Ctrl Pts',(6.07260331771232,57.495,1.85756929242874));
#37577=CARTESIAN_POINT('Ctrl Pts',(6.10621926889299,57.495,1.88347219921809));
#37578=CARTESIAN_POINT('Ctrl Pts',(6.14006878432982,57.495,1.91060895733317));
#37579=CARTESIAN_POINT('Ctrl Pts',(6.17417680788945,57.495,1.93898880419737));
#37580=CARTESIAN_POINT('Ctrl Pts',(6.20853885514981,57.495,1.96860861168851));
#37581=CARTESIAN_POINT('Ctrl Pts',(6.24311798195985,57.495,1.99945211810837));
#37582=CARTESIAN_POINT('Ctrl Pts',(6.27785854554194,57.495,2.03149622201769));
#37583=CARTESIAN_POINT('Ctrl Pts',(6.31269482043467,57.495,2.06471490843563));
#37584=CARTESIAN_POINT('Ctrl Pts',(6.34756091533115,57.495,2.09908352929888));
#37585=CARTESIAN_POINT('Ctrl Pts',(6.38240181135703,57.495,2.13458349574329));
#37586=CARTESIAN_POINT('Ctrl Pts',(6.41717671306138,57.495,2.17120312938042));
#37587=CARTESIAN_POINT('Ctrl Pts',(6.45185553518375,57.495,2.20893514043555));
#37588=CARTESIAN_POINT('Ctrl Pts',(6.48641743997175,57.495,2.24777479550457));
#37589=CARTESIAN_POINT('Ctrl Pts',(6.52084865967127,57.495,2.2877177827968));
#37590=CARTESIAN_POINT('Ctrl Pts',(6.55514062276556,57.495,2.32875748935421));
#37591=CARTESIAN_POINT('Ctrl Pts',(6.58928830924802,57.495,2.37088387159981));
#37592=CARTESIAN_POINT('Ctrl Pts',(6.6232894242584,57.495,2.41408612451229));
#37593=CARTESIAN_POINT('Ctrl Pts',(6.65037263123018,57.495,2.4495007016118));
#37594=CARTESIAN_POINT('Ctrl Pts',(6.67061900235304,57.495,2.47653809829358));
#37595=CARTESIAN_POINT('Ctrl Pts',(6.68408728750664,57.495,2.49477440711619));
#37596=CARTESIAN_POINT('Ctrl Pts',(6.69081410619341,57.495,2.50394540602692));
#37597=CARTESIAN_POINT('',(5.1463899549833,57.495,1.4909173120086));
#37598=CARTESIAN_POINT('',(5.00231408838243,57.495,1.4491783055134));
#37599=CARTESIAN_POINT('',(5.32519370006274,57.495,0.592010183030742));
#37600=CARTESIAN_POINT('Origin',(0.,57.495,0.));
#37601=CARTESIAN_POINT('',(5.93051272372135,57.495,0.659304453656786));
#37602=CARTESIAN_POINT('',(5.93051272372135,57.495,0.659304453656786));
#37603=CARTESIAN_POINT('',(7.13972463098307,57.495,0.247119796320915));
#37604=CARTESIAN_POINT('Ctrl Pts',(5.93051272372135,57.495,0.659304453656786));
#37605=CARTESIAN_POINT('Ctrl Pts',(5.93440822125369,57.495,0.659649967278209));
#37606=CARTESIAN_POINT('Ctrl Pts',(5.94245897164689,57.495,0.66024299963913));
#37607=CARTESIAN_POINT('Ctrl Pts',(5.95531437453421,57.495,0.660838563360811));
#37608=CARTESIAN_POINT('Ctrl Pts',(5.97401619058905,57.495,0.661043615595394));
#37609=CARTESIAN_POINT('Ctrl Pts',(5.99999062205821,57.495,0.660311421925918));
#37610=CARTESIAN_POINT('Ctrl Pts',(6.02851672315009,57.495,0.658581184594064));
#37611=CARTESIAN_POINT('Ctrl Pts',(6.05948455921138,57.495,0.655842009648653));
#37612=CARTESIAN_POINT('Ctrl Pts',(6.092682497423,57.495,0.652083489461662));
#37613=CARTESIAN_POINT('Ctrl Pts',(6.12780215712609,57.495,0.647296629738963));
#37614=CARTESIAN_POINT('Ctrl Pts',(6.16449561918681,57.495,0.641473544543642));
#37615=CARTESIAN_POINT('Ctrl Pts',(6.2024209037432,57.495,0.634607707876569));
#37616=CARTESIAN_POINT('Ctrl Pts',(6.24128706412512,57.495,0.626694128202827));
#37617=CARTESIAN_POINT('Ctrl Pts',(6.28091120375433,57.495,0.617730009530282));
#37618=CARTESIAN_POINT('Ctrl Pts',(6.32121490697708,57.495,0.607714431517377));
#37619=CARTESIAN_POINT('Ctrl Pts',(6.36218460951721,57.495,0.596647533682194));
#37620=CARTESIAN_POINT('Ctrl Pts',(6.40384227175349,57.495,0.584530087032232));
#37621=CARTESIAN_POINT('Ctrl Pts',(6.4462144738227,57.495,0.571363102905584));
#37622=CARTESIAN_POINT('Ctrl Pts',(6.48929587557851,57.495,0.557147755196286));
#37623=CARTESIAN_POINT('Ctrl Pts',(6.53304612199338,57.495,0.541884929839957));
#37624=CARTESIAN_POINT('Ctrl Pts',(6.57740496530586,57.495,0.525574676214359));
#37625=CARTESIAN_POINT('Ctrl Pts',(6.62230172760518,57.495,0.508215876982666));
#37626=CARTESIAN_POINT('Ctrl Pts',(6.66766610085612,57.495,0.489806088474619));
#37627=CARTESIAN_POINT('Ctrl Pts',(6.71344014059646,57.495,0.470341429749655));
#37628=CARTESIAN_POINT('Ctrl Pts',(6.75958168761835,57.495,0.449817078488633));
#37629=CARTESIAN_POINT('Ctrl Pts',(6.80606015708944,57.495,0.42822825643448));
#37630=CARTESIAN_POINT('Ctrl Pts',(6.85285448604147,57.495,0.405571362419761));
#37631=CARTESIAN_POINT('Ctrl Pts',(6.89995030467732,57.495,0.38184511132823));
#37632=CARTESIAN_POINT('Ctrl Pts',(6.94733716327859,57.495,0.357052332559016));
#37633=CARTESIAN_POINT('Ctrl Pts',(6.99500658045334,57.495,0.331200384093974));
#37634=CARTESIAN_POINT('Ctrl Pts',(7.04295230112448,57.495,0.304298370266161));
#37635=CARTESIAN_POINT('Ctrl Pts',(7.0815264936406,57.495,0.281943861934802));
#37636=CARTESIAN_POINT('Ctrl Pts',(7.1105784652929,57.495,0.264712515322363));
#37637=CARTESIAN_POINT('Ctrl Pts',(7.13000027153814,57.495,0.253018452443265));
#37638=CARTESIAN_POINT('Ctrl Pts',(7.13972463098307,57.495,0.247119796320915));
#37639=CARTESIAN_POINT('',(7.13972463098307,57.495,-0.247119796320921));
#37640=CARTESIAN_POINT('Origin',(1.6286971771251E-12,57.495,-4.16333634234733E-16));
#37641=CARTESIAN_POINT('',(5.93051272372135,57.495,-0.659304453656789));
#37642=CARTESIAN_POINT('Ctrl Pts',(5.93051272372135,57.495,-0.659304453656789));
#37643=CARTESIAN_POINT('Ctrl Pts',(5.9344082212537,57.495,-0.659649967278237));
#37644=CARTESIAN_POINT('Ctrl Pts',(5.94245897164691,57.495,-0.660242999639202));
#37645=CARTESIAN_POINT('Ctrl Pts',(5.95531437453424,57.495,-0.660838563360922));
#37646=CARTESIAN_POINT('Ctrl Pts',(5.97401619058907,57.495,-0.661043615595513));
#37647=CARTESIAN_POINT('Ctrl Pts',(5.99999062205823,57.495,-0.660311421925998));
#37648=CARTESIAN_POINT('Ctrl Pts',(6.0285167231501,57.495,-0.658581184594089));
#37649=CARTESIAN_POINT('Ctrl Pts',(6.05948455921138,57.495,-0.655842009648634));
#37650=CARTESIAN_POINT('Ctrl Pts',(6.09268249742298,57.495,-0.652083489461621));
#37651=CARTESIAN_POINT('Ctrl Pts',(6.12780215712604,57.495,-0.647296629738921));
#37652=CARTESIAN_POINT('Ctrl Pts',(6.16449561918676,57.495,-0.641473544543615));
#37653=CARTESIAN_POINT('Ctrl Pts',(6.20242090374318,57.495,-0.634607707876565));
#37654=CARTESIAN_POINT('Ctrl Pts',(6.24128706412515,57.495,-0.626694128202843));
#37655=CARTESIAN_POINT('Ctrl Pts',(6.2809112037544,57.495,-0.617730009530308));
#37656=CARTESIAN_POINT('Ctrl Pts',(6.32121490697716,57.495,-0.607714431517403));
#37657=CARTESIAN_POINT('Ctrl Pts',(6.36218460951727,57.495,-0.596647533682212));
#37658=CARTESIAN_POINT('Ctrl Pts',(6.40384227175352,57.495,-0.584530087032239));
#37659=CARTESIAN_POINT('Ctrl Pts',(6.44621447382266,57.495,-0.57136310290558));
#37660=CARTESIAN_POINT('Ctrl Pts',(6.4892958755784,57.495,-0.557147755196278));
#37661=CARTESIAN_POINT('Ctrl Pts',(6.53304612199323,57.495,-0.541884929839951));
#37662=CARTESIAN_POINT('Ctrl Pts',(6.57740496530571,57.495,-0.525574676214357));
#37663=CARTESIAN_POINT('Ctrl Pts',(6.62230172760513,57.495,-0.508215876982669));
#37664=CARTESIAN_POINT('Ctrl Pts',(6.66766610085618,57.495,-0.489806088474624));
#37665=CARTESIAN_POINT('Ctrl Pts',(6.71344014059664,57.495,-0.470341429749656));
#37666=CARTESIAN_POINT('Ctrl Pts',(6.75958168761858,57.495,-0.44981707848863));
#37667=CARTESIAN_POINT('Ctrl Pts',(6.80606015708966,57.495,-0.428228256434474));
#37668=CARTESIAN_POINT('Ctrl Pts',(6.85285448604159,57.495,-0.405571362419757));
#37669=CARTESIAN_POINT('Ctrl Pts',(6.89995030467727,57.495,-0.381845111328236));
#37670=CARTESIAN_POINT('Ctrl Pts',(6.94733716327837,57.495,-0.357052332559036));
#37671=CARTESIAN_POINT('Ctrl Pts',(6.99500658045299,57.495,-0.33120038409401));
#37672=CARTESIAN_POINT('Ctrl Pts',(7.0429523011241,57.495,-0.304298370266206));
#37673=CARTESIAN_POINT('Ctrl Pts',(7.0815264936403,57.495,-0.281943861934841));
#37674=CARTESIAN_POINT('Ctrl Pts',(7.11057846529273,57.495,-0.264712515322388));
#37675=CARTESIAN_POINT('Ctrl Pts',(7.13000027153808,57.495,-0.253018452443277));
#37676=CARTESIAN_POINT('Ctrl Pts',(7.13972463098307,57.495,-0.247119796320918));
#37677=CARTESIAN_POINT('',(5.32519370006274,57.495,-0.592010183030745));
#37678=CARTESIAN_POINT('',(5.17611212951227,57.495,-0.575436549687219));
#37679=CARTESIAN_POINT('',(5.1463899549833,57.495,-1.4909173120086));
#37680=CARTESIAN_POINT('Origin',(0.,57.495,0.));
#37681=CARTESIAN_POINT('',(5.73138421404289,57.495,-1.66039107437149));
#37682=CARTESIAN_POINT('',(5.73138421404289,57.495,-1.66039107437149));
#37683=CARTESIAN_POINT('',(6.6908141061934,57.495,-2.50394540602693));
#37684=CARTESIAN_POINT('Ctrl Pts',(5.73138421404289,57.495,-1.66039107437149));
#37685=CARTESIAN_POINT('Ctrl Pts',(5.73511540682054,57.495,-1.66156260377489));
#37686=CARTESIAN_POINT('Ctrl Pts',(5.74278027398956,57.495,-1.66409560210811));
#37687=CARTESIAN_POINT('Ctrl Pts',(5.75488502996854,57.495,-1.6684649226767));
#37688=CARTESIAN_POINT('Ctrl Pts',(5.77224172513534,57.495,-1.67543235427339));
#37689=CARTESIAN_POINT('Ctrl Pts',(5.79595877235173,57.495,-1.68604879760681));
#37690=CARTESIAN_POINT('Ctrl Pts',(5.8216513201319,57.495,-1.69856379474193));
#37691=CARTESIAN_POINT('Ctrl Pts',(5.84921363316514,57.495,-1.71294534020682));
#37692=CARTESIAN_POINT('Ctrl Pts',(5.87844620539466,57.495,-1.72912206102238));
#37693=CARTESIAN_POINT('Ctrl Pts',(5.90906068827417,57.495,-1.74698425466385));
#37694=CARTESIAN_POINT('Ctrl Pts',(5.94073262861954,57.495,-1.76640606389863));
#37695=CARTESIAN_POINT('Ctrl Pts',(5.97314358084405,57.495,-1.78726264793637));
#37696=CARTESIAN_POINT('Ctrl Pts',(6.00602283509636,57.495,-1.80944727788364));
#37697=CARTESIAN_POINT('Ctrl Pts',(6.03920034699142,57.495,-1.83289254541003));
#37698=CARTESIAN_POINT('Ctrl Pts',(6.07260331771223,57.495,-1.85756929242873));
#37699=CARTESIAN_POINT('Ctrl Pts',(6.10621926889293,57.495,-1.88347219921808));
#37700=CARTESIAN_POINT('Ctrl Pts',(6.14006878432979,57.495,-1.91060895733316));
#37701=CARTESIAN_POINT('Ctrl Pts',(6.17417680788948,57.495,-1.93898880419739));
#37702=CARTESIAN_POINT('Ctrl Pts',(6.20853885514991,57.495,-1.96860861168855));
#37703=CARTESIAN_POINT('Ctrl Pts',(6.24311798195999,57.495,-1.99945211810842));
#37704=CARTESIAN_POINT('Ctrl Pts',(6.27785854554207,57.495,-2.03149622201774));
#37705=CARTESIAN_POINT('Ctrl Pts',(6.31269482043472,57.495,-2.06471490843566));
#37706=CARTESIAN_POINT('Ctrl Pts',(6.34756091533109,57.495,-2.09908352929886));
#37707=CARTESIAN_POINT('Ctrl Pts',(6.38240181135686,57.495,-2.13458349574322));
#37708=CARTESIAN_POINT('Ctrl Pts',(6.41717671306116,57.495,-2.17120312938033));
#37709=CARTESIAN_POINT('Ctrl Pts',(6.45185553518355,57.495,-2.20893514043546));
#37710=CARTESIAN_POINT('Ctrl Pts',(6.48641743997165,57.495,-2.24777479550452));
#37711=CARTESIAN_POINT('Ctrl Pts',(6.52084865967131,57.495,-2.28771778279682));
#37712=CARTESIAN_POINT('Ctrl Pts',(6.55514062276576,57.495,-2.32875748935431));
#37713=CARTESIAN_POINT('Ctrl Pts',(6.58928830924832,57.495,-2.37088387159998));
#37714=CARTESIAN_POINT('Ctrl Pts',(6.62328942425873,57.495,-2.41408612451248));
#37715=CARTESIAN_POINT('Ctrl Pts',(6.65037263123044,57.495,-2.44950070161195));
#37716=CARTESIAN_POINT('Ctrl Pts',(6.67061900235319,57.495,-2.47653809829367));
#37717=CARTESIAN_POINT('Ctrl Pts',(6.6840872875067,57.495,-2.49477440711623));
#37718=CARTESIAN_POINT('Ctrl Pts',(6.6908141061934,57.495,-2.50394540602693));
#37719=CARTESIAN_POINT('',(6.5016768024705,57.495,-2.96056324982543));
#37720=CARTESIAN_POINT('Origin',(1.50456066262064E-12,57.495,-6.23660068148934E-13));
#37721=CARTESIAN_POINT('',(5.22677443144495,57.495,-2.87862685522557));
#37722=CARTESIAN_POINT('Ctrl Pts',(5.22677443144495,57.495,-2.87862685522557));
#37723=CARTESIAN_POINT('Ctrl Pts',(5.23024117954544,57.495,-2.88043681055508));
#37724=CARTESIAN_POINT('Ctrl Pts',(5.2374521593957,57.495,-2.88406558980908));
#37725=CARTESIAN_POINT('Ctrl Pts',(5.24910109063627,57.495,-2.88953536864324));
#37726=CARTESIAN_POINT('Ctrl Pts',(5.26630084561717,57.495,-2.8968816873652));
#37727=CARTESIAN_POINT('Ctrl Pts',(5.29057828960674,57.495,-2.90614521320845));
#37728=CARTESIAN_POINT('Ctrl Pts',(5.31759510370885,57.495,-2.91546314862894));
#37729=CARTESIAN_POINT('Ctrl Pts',(5.34725389048201,57.495,-2.92478335875772));
#37730=CARTESIAN_POINT('Ctrl Pts',(5.37936310952306,57.495,-2.93401523982667));
#37731=CARTESIAN_POINT('Ctrl Pts',(5.41364129622042,57.495,-2.94303247002252));
#37732=CARTESIAN_POINT('Ctrl Pts',(5.44977003302479,57.495,-2.95169462080126));
#37733=CARTESIAN_POINT('Ctrl Pts',(5.48743586913294,57.495,-2.95986479289849));
#37734=CARTESIAN_POINT('Ctrl Pts',(5.52637191504897,57.495,-2.96742703426686));
#37735=CARTESIAN_POINT('Ctrl Pts',(5.56641026634754,57.495,-2.97430877025614));
#37736=CARTESIAN_POINT('Ctrl Pts',(5.60747882861056,57.495,-2.98047914221006));
#37737=CARTESIAN_POINT('Ctrl Pts',(5.64956501668965,57.495,-2.98593308820275));
#37738=CARTESIAN_POINT('Ctrl Pts',(5.6926888242775,57.495,-2.99067972442542));
#37739=CARTESIAN_POINT('Ctrl Pts',(5.73687442119609,57.495,-2.99473015701059));
#37740=CARTESIAN_POINT('Ctrl Pts',(5.78211642456377,57.495,-2.99808342690941));
#37741=CARTESIAN_POINT('Ctrl Pts',(5.82837721216371,57.495,-3.00072490941926));
#37742=CARTESIAN_POINT('Ctrl Pts',(5.87560110342618,57.495,-3.00263159433907));
#37743=CARTESIAN_POINT('Ctrl Pts',(5.92372322806235,57.495,-3.00377540211876));
#37744=CARTESIAN_POINT('Ctrl Pts',(5.97267956506957,57.495,-3.00412716938112));
#37745=CARTESIAN_POINT('Ctrl Pts',(6.02241806591682,57.495,-3.0036611362189));
#37746=CARTESIAN_POINT('Ctrl Pts',(6.07290162599645,57.495,-3.00235671375976));
#37747=CARTESIAN_POINT('Ctrl Pts',(6.12410381716763,57.495,-3.00019778316116));
#37748=CARTESIAN_POINT('Ctrl Pts',(6.17600655789219,57.495,-2.99717295692923));
#37749=CARTESIAN_POINT('Ctrl Pts',(6.22859706400143,57.495,-2.9932755486881));
#37750=CARTESIAN_POINT('Ctrl Pts',(6.28186459845025,57.495,-2.98850417352762));
#37751=CARTESIAN_POINT('Ctrl Pts',(6.33579850967655,57.495,-2.98286238364848));
#37752=CARTESIAN_POINT('Ctrl Pts',(6.39038953466525,57.495,-2.97635619664327));
#37753=CARTESIAN_POINT('Ctrl Pts',(6.43458214159119,57.495,-2.97046502832938));
#37754=CARTESIAN_POINT('Ctrl Pts',(6.4680168144459,57.495,-2.96566304810545));
#37755=CARTESIAN_POINT('Ctrl Pts',(6.49043534784125,57.495,-2.96229154623624));
#37756=CARTESIAN_POINT('Ctrl Pts',(6.5016768024705,57.495,-2.96056324982543));
#37757=CARTESIAN_POINT('',(4.69328497730872,57.495,-2.58480949428933));
#37758=CARTESIAN_POINT('',(4.56189402049717,57.495,-2.51244640654327));
#37759=CARTESIAN_POINT('',(4.18409499139877,57.495,-3.34686616149372));
#37760=CARTESIAN_POINT('Origin',(0.,57.495,0.));
#37761=CARTESIAN_POINT('',(4.65970441290367,57.495,-3.72730711280926));
#37762=CARTESIAN_POINT('',(4.65970441290367,57.495,-3.72730711280926));
#37763=CARTESIAN_POINT('',(5.22328778611671,57.495,-4.87380761862879));
#37764=CARTESIAN_POINT('Ctrl Pts',(4.65970441290367,57.495,-3.72730711280926));
#37765=CARTESIAN_POINT('Ctrl Pts',(4.66270326064959,57.495,-3.72981733050578));
#37766=CARTESIAN_POINT('Ctrl Pts',(4.66881533805013,57.495,-3.73509073349858));
#37767=CARTESIAN_POINT('Ctrl Pts',(4.67832660775287,57.495,-3.74375974890886));
#37768=CARTESIAN_POINT('Ctrl Pts',(4.69169578253132,57.495,-3.75683893603616));
#37769=CARTESIAN_POINT('Ctrl Pts',(4.7095447400518,57.495,-3.77572337177431));
#37770=CARTESIAN_POINT('Ctrl Pts',(4.72849227702427,57.495,-3.7971178338476));
#37771=CARTESIAN_POINT('Ctrl Pts',(4.74845295472312,57.495,-3.82095228990397));
#37772=CARTESIAN_POINT('Ctrl Pts',(4.76926976684252,57.495,-3.84708445224627));
#37773=CARTESIAN_POINT('Ctrl Pts',(4.79071829540103,57.495,-3.8753026227458));
#37774=CARTESIAN_POINT('Ctrl Pts',(4.81254694822034,57.495,-3.90536636162318));
#37775=CARTESIAN_POINT('Ctrl Pts',(4.83450929444279,57.495,-3.93703846717724));
#37776=CARTESIAN_POINT('Ctrl Pts',(4.85639607415676,57.495,-3.97011673859274));
#37777=CARTESIAN_POINT('Ctrl Pts',(4.87807598288654,57.495,-4.00447382552396));
#37778=CARTESIAN_POINT('Ctrl Pts',(4.89949292161185,57.495,-4.04005493051012));
#37779=CARTESIAN_POINT('Ctrl Pts',(4.92063739759521,57.495,-4.07685036350539));
#37780=CARTESIAN_POINT('Ctrl Pts',(4.94152548435402,57.495,-4.11487510765791));
#37781=CARTESIAN_POINT('Ctrl Pts',(4.96217669200723,57.495,-4.15414724283858));
#37782=CARTESIAN_POINT('Ctrl Pts',(4.98258807456962,57.495,-4.1946621629253));
#37783=CARTESIAN_POINT('Ctrl Pts',(5.00273172317863,57.495,-4.23639070615337));
#37784=CARTESIAN_POINT('Ctrl Pts',(5.02256507114894,57.495,-4.27929023600674));
#37785=CARTESIAN_POINT('Ctrl Pts',(5.04203735157413,57.495,-4.3233115657319));
#37786=CARTESIAN_POINT('Ctrl Pts',(5.06109712122989,57.495,-4.36840670797617));
#37787=CARTESIAN_POINT('Ctrl Pts',(5.07970066295468,57.495,-4.41453743405677));
#37788=CARTESIAN_POINT('Ctrl Pts',(5.09781475579217,57.495,-4.46167734280651));
#37789=CARTESIAN_POINT('Ctrl Pts',(5.11541439426204,57.495,-4.50980818622101));
#37790=CARTESIAN_POINT('Ctrl Pts',(5.13248213818666,57.495,-4.5589176169425));
#37791=CARTESIAN_POINT('Ctrl Pts',(5.14900691787064,57.495,-4.60899638270439));
#37792=CARTESIAN_POINT('Ctrl Pts',(5.16498334493456,57.495,-4.66003509375265));
#37793=CARTESIAN_POINT('Ctrl Pts',(5.18041062500752,57.495,-4.71202254995864));
#37794=CARTESIAN_POINT('Ctrl Pts',(5.19529077281773,57.495,-4.7649478905793));
#37795=CARTESIAN_POINT('Ctrl Pts',(5.20675982149348,57.495,-4.80803098811744));
#37796=CARTESIAN_POINT('Ctrl Pts',(5.21511826561704,57.495,-4.84075823631826));
#37797=CARTESIAN_POINT('Ctrl Pts',(5.2205826053545,57.495,-4.86276047837859));
#37798=CARTESIAN_POINT('Ctrl Pts',(5.22328778611671,57.495,-4.87380761862879));
#37799=CARTESIAN_POINT('',(4.87380761862879,57.495,-5.22328778611671));
#37800=CARTESIAN_POINT('Origin',(1.15136842610855E-12,57.495,-1.15195721078055E-12));
#37801=CARTESIAN_POINT('',(3.72730711280926,57.495,-4.65970441290368));
#37802=CARTESIAN_POINT('Ctrl Pts',(3.72730711280926,57.495,-4.65970441290368));
#37803=CARTESIAN_POINT('Ctrl Pts',(3.72981733050576,57.495,-4.66270326064961));
#37804=CARTESIAN_POINT('Ctrl Pts',(3.73509073349854,57.495,-4.6688153380502));
#37805=CARTESIAN_POINT('Ctrl Pts',(3.7437597489088,57.495,-4.67832660775297));
#37806=CARTESIAN_POINT('Ctrl Pts',(3.7568389360361,57.495,-4.69169578253142));
#37807=CARTESIAN_POINT('Ctrl Pts',(3.77572337177426,57.495,-4.70954474005187));
#37808=CARTESIAN_POINT('Ctrl Pts',(3.79711783384759,57.495,-4.72849227702429));
#37809=CARTESIAN_POINT('Ctrl Pts',(3.82095228990398,57.495,-4.74845295472311));
#37810=CARTESIAN_POINT('Ctrl Pts',(3.84708445224628,57.495,-4.76926976684248));
#37811=CARTESIAN_POINT('Ctrl Pts',(3.87530262274579,57.495,-4.79071829540097));
#37812=CARTESIAN_POINT('Ctrl Pts',(3.90536636162316,57.495,-4.81254694822028));
#37813=CARTESIAN_POINT('Ctrl Pts',(3.93703846717723,57.495,-4.83450929444277));
#37814=CARTESIAN_POINT('Ctrl Pts',(3.97011673859275,57.495,-4.85639607415679));
#37815=CARTESIAN_POINT('Ctrl Pts',(4.00447382552398,57.495,-4.87807598288661));
#37816=CARTESIAN_POINT('Ctrl Pts',(4.04005493051016,57.495,-4.89949292161193));
#37817=CARTESIAN_POINT('Ctrl Pts',(4.07685036350543,57.495,-4.92063739759527));
#37818=CARTESIAN_POINT('Ctrl Pts',(4.11487510765792,57.495,-4.94152548435404));
#37819=CARTESIAN_POINT('Ctrl Pts',(4.15414724283855,57.495,-4.9621766920072));
#37820=CARTESIAN_POINT('Ctrl Pts',(4.19466216292523,57.495,-4.98258807456953));
#37821=CARTESIAN_POINT('Ctrl Pts',(4.23639070615327,57.495,-5.00273172317852));
#37822=CARTESIAN_POINT('Ctrl Pts',(4.27929023600664,57.495,-5.02256507114883));
#37823=CARTESIAN_POINT('Ctrl Pts',(4.32331156573186,57.495,-5.04203735157409));
#37824=CARTESIAN_POINT('Ctrl Pts',(4.36840670797621,57.495,-5.06109712122993));
#37825=CARTESIAN_POINT('Ctrl Pts',(4.41453743405689,57.495,-5.07970066295481));
#37826=CARTESIAN_POINT('Ctrl Pts',(4.46167734280668,57.495,-5.09781475579234));
#37827=CARTESIAN_POINT('Ctrl Pts',(4.50980818622117,57.495,-5.11541439426219));
#37828=CARTESIAN_POINT('Ctrl Pts',(4.55891761694258,57.495,-5.13248213818673));
#37829=CARTESIAN_POINT('Ctrl Pts',(4.60899638270436,57.495,-5.14900691787061));
#37830=CARTESIAN_POINT('Ctrl Pts',(4.66003509375248,57.495,-5.16498334493441));
#37831=CARTESIAN_POINT('Ctrl Pts',(4.71202254995837,57.495,-5.1804106250073));
#37832=CARTESIAN_POINT('Ctrl Pts',(4.764947890579,57.495,-5.1952907728175));
#37833=CARTESIAN_POINT('Ctrl Pts',(4.8080309881172,57.495,-5.2067598214933));
#37834=CARTESIAN_POINT('Ctrl Pts',(4.84075823631811,57.495,-5.21511826561693));
#37835=CARTESIAN_POINT('Ctrl Pts',(4.86276047837853,57.495,-5.22058260535447));
#37836=CARTESIAN_POINT('Ctrl Pts',(4.87380761862879,57.495,-5.22328778611671));
#37837=CARTESIAN_POINT('',(3.34686616149372,57.495,-4.18409499139877));
#37838=CARTESIAN_POINT('',(3.25316890053365,57.495,-4.06695907338649));
#37839=CARTESIAN_POINT('',(2.58480949428932,57.495,-4.69328497730873));
#37840=CARTESIAN_POINT('Origin',(0.,57.495,0.));
#37841=CARTESIAN_POINT('',(2.87862685522556,57.495,-5.22677443144495));
#37842=CARTESIAN_POINT('',(2.87862685522556,57.495,-5.22677443144495));
#37843=CARTESIAN_POINT('',(2.96056324982543,57.495,-6.50167680247051));
#37844=CARTESIAN_POINT('Ctrl Pts',(2.87862685522556,57.495,-5.22677443144495));
#37845=CARTESIAN_POINT('Ctrl Pts',(2.88043681055505,57.495,-5.23024117954545));
#37846=CARTESIAN_POINT('Ctrl Pts',(2.884065589809,57.495,-5.23745215939571));
#37847=CARTESIAN_POINT('Ctrl Pts',(2.88953536864313,57.495,-5.24910109063628));
#37848=CARTESIAN_POINT('Ctrl Pts',(2.89688168736508,57.495,-5.26630084561719));
#37849=CARTESIAN_POINT('Ctrl Pts',(2.90614521320837,57.495,-5.29057828960676));
#37850=CARTESIAN_POINT('Ctrl Pts',(2.91546314862891,57.495,-5.31759510370886));
#37851=CARTESIAN_POINT('Ctrl Pts',(2.92478335875774,57.495,-5.34725389048201));
#37852=CARTESIAN_POINT('Ctrl Pts',(2.93401523982671,57.495,-5.37936310952307));
#37853=CARTESIAN_POINT('Ctrl Pts',(2.94303247002258,57.495,-5.41364129622045));
#37854=CARTESIAN_POINT('Ctrl Pts',(2.95169462080131,57.495,-5.44977003302482));
#37855=CARTESIAN_POINT('Ctrl Pts',(2.95986479289849,57.495,-5.48743586913296));
#37856=CARTESIAN_POINT('Ctrl Pts',(2.96742703426683,57.495,-5.52637191504895));
#37857=CARTESIAN_POINT('Ctrl Pts',(2.97430877025608,57.495,-5.56641026634749));
#37858=CARTESIAN_POINT('Ctrl Pts',(2.98047914221,57.495,-5.6074788286105));
#37859=CARTESIAN_POINT('Ctrl Pts',(2.98593308820271,57.495,-5.64956501668959));
#37860=CARTESIAN_POINT('Ctrl Pts',(2.9906797244254,57.495,-5.69268882427748));
#37861=CARTESIAN_POINT('Ctrl Pts',(2.9947301570106,57.495,-5.73687442119613));
#37862=CARTESIAN_POINT('Ctrl Pts',(2.99808342690946,57.495,-5.78211642456387));
#37863=CARTESIAN_POINT('Ctrl Pts',(3.00072490941932,57.495,-5.82837721216385));
#37864=CARTESIAN_POINT('Ctrl Pts',(3.00263159433912,57.495,-5.87560110342631));
#37865=CARTESIAN_POINT('Ctrl Pts',(3.00377540211877,57.495,-5.9237232280624));
#37866=CARTESIAN_POINT('Ctrl Pts',(3.00412716938109,57.495,-5.97267956506952));
#37867=CARTESIAN_POINT('Ctrl Pts',(3.00366113621882,57.495,-6.02241806591666));
#37868=CARTESIAN_POINT('Ctrl Pts',(3.00235671375967,57.495,-6.07290162599622));
#37869=CARTESIAN_POINT('Ctrl Pts',(3.00019778316108,57.495,-6.12410381716742));
#37870=CARTESIAN_POINT('Ctrl Pts',(2.99717295692919,57.495,-6.17600655789209));
#37871=CARTESIAN_POINT('Ctrl Pts',(2.99327554868811,57.495,-6.22859706400148));
#37872=CARTESIAN_POINT('Ctrl Pts',(2.98850417352769,57.495,-6.28186459845047));
#37873=CARTESIAN_POINT('Ctrl Pts',(2.98286238364857,57.495,-6.33579850967689));
#37874=CARTESIAN_POINT('Ctrl Pts',(2.97635619664337,57.495,-6.39038953466561));
#37875=CARTESIAN_POINT('Ctrl Pts',(2.97046502832945,57.495,-6.43458214159149));
#37876=CARTESIAN_POINT('Ctrl Pts',(2.96566304810549,57.495,-6.46801681444607));
#37877=CARTESIAN_POINT('Ctrl Pts',(2.96229154623625,57.495,-6.49043534784131));
#37878=CARTESIAN_POINT('Ctrl Pts',(2.96056324982543,57.495,-6.50167680247051));
#37879=CARTESIAN_POINT('',(2.50394540602692,57.495,-6.69081410619341));
#37880=CARTESIAN_POINT('Origin',(6.22890783902202E-13,57.495,-1.50487931058895E-12));
#37881=CARTESIAN_POINT('',(1.66039107437148,57.495,-5.73138421404289));
#37882=CARTESIAN_POINT('Ctrl Pts',(1.66039107437148,57.495,-5.73138421404289));
#37883=CARTESIAN_POINT('Ctrl Pts',(1.66156260377487,57.495,-5.73511540682056));
#37884=CARTESIAN_POINT('Ctrl Pts',(1.66409560210805,57.495,-5.7427802739896));
#37885=CARTESIAN_POINT('Ctrl Pts',(1.6684649226766,57.495,-5.75488502996861));
#37886=CARTESIAN_POINT('Ctrl Pts',(1.67543235427329,57.495,-5.77224172513541));
#37887=CARTESIAN_POINT('Ctrl Pts',(1.68604879760674,57.495,-5.79595877235177));
#37888=CARTESIAN_POINT('Ctrl Pts',(1.69856379474191,57.495,-5.82165132013192));
#37889=CARTESIAN_POINT('Ctrl Pts',(1.71294534020683,57.495,-5.84921363316513));
#37890=CARTESIAN_POINT('Ctrl Pts',(1.7291220610224,57.495,-5.87844620539462));
#37891=CARTESIAN_POINT('Ctrl Pts',(1.74698425466387,57.495,-5.90906068827411));
#37892=CARTESIAN_POINT('Ctrl Pts',(1.76640606389864,57.495,-5.94073262861949));
#37893=CARTESIAN_POINT('Ctrl Pts',(1.78726264793636,57.495,-5.97314358084403));
#37894=CARTESIAN_POINT('Ctrl Pts',(1.80944727788364,57.495,-6.00602283509639));
#37895=CARTESIAN_POINT('Ctrl Pts',(1.83289254541003,57.495,-6.03920034699149));
#37896=CARTESIAN_POINT('Ctrl Pts',(1.85756929242873,57.495,-6.07260331771232));
#37897=CARTESIAN_POINT('Ctrl Pts',(1.88347219921808,57.495,-6.106219268893));
#37898=CARTESIAN_POINT('Ctrl Pts',(1.91060895733316,57.495,-6.14006878432982));
#37899=CARTESIAN_POINT('Ctrl Pts',(1.93898880419737,57.495,-6.17417680788945));
#37900=CARTESIAN_POINT('Ctrl Pts',(1.96860861168851,57.495,-6.20853885514981));
#37901=CARTESIAN_POINT('Ctrl Pts',(1.99945211810836,57.495,-6.24311798195985));
#37902=CARTESIAN_POINT('Ctrl Pts',(2.03149622201768,57.495,-6.27785854554194));
#37903=CARTESIAN_POINT('Ctrl Pts',(2.06471490843563,57.495,-6.31269482043467));
#37904=CARTESIAN_POINT('Ctrl Pts',(2.09908352929888,57.495,-6.34756091533115));
#37905=CARTESIAN_POINT('Ctrl Pts',(2.13458349574329,57.495,-6.38240181135703));
#37906=CARTESIAN_POINT('Ctrl Pts',(2.17120312938042,57.495,-6.41717671306138));
#37907=CARTESIAN_POINT('Ctrl Pts',(2.20893514043555,57.495,-6.45185553518375));
#37908=CARTESIAN_POINT('Ctrl Pts',(2.24777479550457,57.495,-6.48641743997175));
#37909=CARTESIAN_POINT('Ctrl Pts',(2.2877177827968,57.495,-6.52084865967127));
#37910=CARTESIAN_POINT('Ctrl Pts',(2.3287574893542,57.495,-6.55514062276556));
#37911=CARTESIAN_POINT('Ctrl Pts',(2.37088387159981,57.495,-6.58928830924802));
#37912=CARTESIAN_POINT('Ctrl Pts',(2.41408612451229,57.495,-6.6232894242584));
#37913=CARTESIAN_POINT('Ctrl Pts',(2.4495007016118,57.495,-6.65037263123018));
#37914=CARTESIAN_POINT('Ctrl Pts',(2.47653809829358,57.495,-6.67061900235304));
#37915=CARTESIAN_POINT('Ctrl Pts',(2.49477440711619,57.495,-6.68408728750665));
#37916=CARTESIAN_POINT('Ctrl Pts',(2.50394540602692,57.495,-6.69081410619341));
#37917=CARTESIAN_POINT('',(1.4909173120086,57.495,-5.1463899549833));
#37918=CARTESIAN_POINT('',(1.44917830551339,57.495,-5.00231408838243));
#37919=CARTESIAN_POINT('',(0.592010183030743,57.495,-5.32519370006274));
#37920=CARTESIAN_POINT('Origin',(0.,57.495,0.));
#37921=CARTESIAN_POINT('',(0.659304453656786,57.495,-5.93051272372135));
#37922=CARTESIAN_POINT('',(0.659304453656786,57.495,-5.93051272372135));
#37923=CARTESIAN_POINT('',(0.247119796320915,57.495,-7.13972463098307));
#37924=CARTESIAN_POINT('Ctrl Pts',(0.659304453656786,57.495,-5.93051272372135));
#37925=CARTESIAN_POINT('Ctrl Pts',(0.659649967278209,57.495,-5.93440822125369));
#37926=CARTESIAN_POINT('Ctrl Pts',(0.660242999639131,57.495,-5.94245897164689));
#37927=CARTESIAN_POINT('Ctrl Pts',(0.660838563360811,57.495,-5.95531437453421));
#37928=CARTESIAN_POINT('Ctrl Pts',(0.661043615595394,57.495,-5.97401619058905));
#37929=CARTESIAN_POINT('Ctrl Pts',(0.660311421925919,57.495,-5.99999062205821));
#37930=CARTESIAN_POINT('Ctrl Pts',(0.658581184594064,57.495,-6.02851672315009));
#37931=CARTESIAN_POINT('Ctrl Pts',(0.655842009648654,57.495,-6.05948455921138));
#37932=CARTESIAN_POINT('Ctrl Pts',(0.652083489461663,57.495,-6.092682497423));
#37933=CARTESIAN_POINT('Ctrl Pts',(0.647296629738964,57.495,-6.12780215712609));
#37934=CARTESIAN_POINT('Ctrl Pts',(0.641473544543642,57.495,-6.16449561918681));
#37935=CARTESIAN_POINT('Ctrl Pts',(0.63460770787657,57.495,-6.2024209037432));
#37936=CARTESIAN_POINT('Ctrl Pts',(0.626694128202827,57.495,-6.24128706412512));
#37937=CARTESIAN_POINT('Ctrl Pts',(0.617730009530282,57.495,-6.28091120375433));
#37938=CARTESIAN_POINT('Ctrl Pts',(0.607714431517377,57.495,-6.32121490697708));
#37939=CARTESIAN_POINT('Ctrl Pts',(0.596647533682195,57.495,-6.36218460951721));
#37940=CARTESIAN_POINT('Ctrl Pts',(0.584530087032233,57.495,-6.40384227175349));
#37941=CARTESIAN_POINT('Ctrl Pts',(0.571363102905584,57.495,-6.4462144738227));
#37942=CARTESIAN_POINT('Ctrl Pts',(0.557147755196286,57.495,-6.48929587557851));
#37943=CARTESIAN_POINT('Ctrl Pts',(0.541884929839957,57.495,-6.53304612199338));
#37944=CARTESIAN_POINT('Ctrl Pts',(0.525574676214359,57.495,-6.57740496530586));
#37945=CARTESIAN_POINT('Ctrl Pts',(0.508215876982667,57.495,-6.62230172760518));
#37946=CARTESIAN_POINT('Ctrl Pts',(0.489806088474619,57.495,-6.66766610085612));
#37947=CARTESIAN_POINT('Ctrl Pts',(0.470341429749655,57.495,-6.71344014059646));
#37948=CARTESIAN_POINT('Ctrl Pts',(0.449817078488634,57.495,-6.75958168761835));
#37949=CARTESIAN_POINT('Ctrl Pts',(0.428228256434481,57.495,-6.80606015708944));
#37950=CARTESIAN_POINT('Ctrl Pts',(0.405571362419761,57.495,-6.85285448604147));
#37951=CARTESIAN_POINT('Ctrl Pts',(0.38184511132823,57.495,-6.89995030467732));
#37952=CARTESIAN_POINT('Ctrl Pts',(0.357052332559016,57.495,-6.94733716327859));
#37953=CARTESIAN_POINT('Ctrl Pts',(0.331200384093974,57.495,-6.99500658045334));
#37954=CARTESIAN_POINT('Ctrl Pts',(0.304298370266162,57.495,-7.04295230112448));
#37955=CARTESIAN_POINT('Ctrl Pts',(0.281943861934803,57.495,-7.0815264936406));
#37956=CARTESIAN_POINT('Ctrl Pts',(0.264712515322363,57.495,-7.1105784652929));
#37957=CARTESIAN_POINT('Ctrl Pts',(0.253018452443265,57.495,-7.13000027153814));
#37958=CARTESIAN_POINT('Ctrl Pts',(0.247119796320915,57.495,-7.13972463098307));
#37959=CARTESIAN_POINT('',(-0.247119796320921,57.495,-7.13972463098307));
#37960=CARTESIAN_POINT('Origin',(-4.16333634234633E-16,57.495,-1.6286971771251E-12));
#37961=CARTESIAN_POINT('',(-0.659304453656788,57.495,-5.93051272372135));
#37962=CARTESIAN_POINT('Ctrl Pts',(-0.659304453656788,57.495,-5.93051272372135));
#37963=CARTESIAN_POINT('Ctrl Pts',(-0.659649967278237,57.495,-5.9344082212537));
#37964=CARTESIAN_POINT('Ctrl Pts',(-0.660242999639202,57.495,-5.94245897164691));
#37965=CARTESIAN_POINT('Ctrl Pts',(-0.660838563360922,57.495,-5.95531437453424));
#37966=CARTESIAN_POINT('Ctrl Pts',(-0.661043615595512,57.495,-5.97401619058907));
#37967=CARTESIAN_POINT('Ctrl Pts',(-0.660311421925998,57.495,-5.99999062205823));
#37968=CARTESIAN_POINT('Ctrl Pts',(-0.658581184594089,57.495,-6.0285167231501));
#37969=CARTESIAN_POINT('Ctrl Pts',(-0.655842009648634,57.495,-6.05948455921138));
#37970=CARTESIAN_POINT('Ctrl Pts',(-0.65208348946162,57.495,-6.09268249742298));
#37971=CARTESIAN_POINT('Ctrl Pts',(-0.647296629738921,57.495,-6.12780215712604));
#37972=CARTESIAN_POINT('Ctrl Pts',(-0.641473544543615,57.495,-6.16449561918676));
#37973=CARTESIAN_POINT('Ctrl Pts',(-0.634607707876565,57.495,-6.20242090374318));
#37974=CARTESIAN_POINT('Ctrl Pts',(-0.626694128202842,57.495,-6.24128706412515));
#37975=CARTESIAN_POINT('Ctrl Pts',(-0.617730009530307,57.495,-6.2809112037544));
#37976=CARTESIAN_POINT('Ctrl Pts',(-0.607714431517402,57.495,-6.32121490697716));
#37977=CARTESIAN_POINT('Ctrl Pts',(-0.596647533682212,57.495,-6.36218460951727));
#37978=CARTESIAN_POINT('Ctrl Pts',(-0.584530087032238,57.495,-6.40384227175352));
#37979=CARTESIAN_POINT('Ctrl Pts',(-0.57136310290558,57.495,-6.44621447382266));
#37980=CARTESIAN_POINT('Ctrl Pts',(-0.557147755196278,57.495,-6.4892958755784));
#37981=CARTESIAN_POINT('Ctrl Pts',(-0.54188492983995,57.495,-6.53304612199323));
#37982=CARTESIAN_POINT('Ctrl Pts',(-0.525574676214357,57.495,-6.57740496530571));
#37983=CARTESIAN_POINT('Ctrl Pts',(-0.508215876982669,57.495,-6.62230172760513));
#37984=CARTESIAN_POINT('Ctrl Pts',(-0.489806088474623,57.495,-6.66766610085618));
#37985=CARTESIAN_POINT('Ctrl Pts',(-0.470341429749656,57.495,-6.71344014059664));
#37986=CARTESIAN_POINT('Ctrl Pts',(-0.44981707848863,57.495,-6.75958168761858));
#37987=CARTESIAN_POINT('Ctrl Pts',(-0.428228256434474,57.495,-6.80606015708966));
#37988=CARTESIAN_POINT('Ctrl Pts',(-0.405571362419757,57.495,-6.85285448604159));
#37989=CARTESIAN_POINT('Ctrl Pts',(-0.381845111328235,57.495,-6.89995030467727));
#37990=CARTESIAN_POINT('Ctrl Pts',(-0.357052332559036,57.495,-6.94733716327837));
#37991=CARTESIAN_POINT('Ctrl Pts',(-0.331200384094009,57.495,-6.99500658045299));
#37992=CARTESIAN_POINT('Ctrl Pts',(-0.304298370266205,57.495,-7.0429523011241));
#37993=CARTESIAN_POINT('Ctrl Pts',(-0.281943861934841,57.495,-7.0815264936403));
#37994=CARTESIAN_POINT('Ctrl Pts',(-0.264712515322388,57.495,-7.11057846529273));
#37995=CARTESIAN_POINT('Ctrl Pts',(-0.253018452443276,57.495,-7.13000027153808));
#37996=CARTESIAN_POINT('Ctrl Pts',(-0.247119796320918,57.495,-7.13972463098307));
#37997=CARTESIAN_POINT('',(-0.592010183030745,57.495,-5.32519370006274));
#37998=CARTESIAN_POINT('',(-0.575436549687219,57.495,-5.17611212951227));
#37999=CARTESIAN_POINT('',(-1.4909173120086,57.495,-5.1463899549833));
#38000=CARTESIAN_POINT('Origin',(0.,57.495,0.));
#38001=CARTESIAN_POINT('',(-1.66039107437148,57.495,-5.73138421404289));
#38002=CARTESIAN_POINT('',(-1.66039107437148,57.495,-5.73138421404289));
#38003=CARTESIAN_POINT('',(-2.50394540602692,57.495,-6.69081410619341));
#38004=CARTESIAN_POINT('Ctrl Pts',(-1.66039107437148,57.495,-5.73138421404289));
#38005=CARTESIAN_POINT('Ctrl Pts',(-1.66156260377489,57.495,-5.73511540682054));
#38006=CARTESIAN_POINT('Ctrl Pts',(-1.66409560210811,57.495,-5.74278027398956));
#38007=CARTESIAN_POINT('Ctrl Pts',(-1.66846492267669,57.495,-5.75488502996854));
#38008=CARTESIAN_POINT('Ctrl Pts',(-1.67543235427339,57.495,-5.77224172513534));
#38009=CARTESIAN_POINT('Ctrl Pts',(-1.68604879760681,57.495,-5.79595877235173));
#38010=CARTESIAN_POINT('Ctrl Pts',(-1.69856379474193,57.495,-5.8216513201319));
#38011=CARTESIAN_POINT('Ctrl Pts',(-1.71294534020681,57.495,-5.84921363316514));
#38012=CARTESIAN_POINT('Ctrl Pts',(-1.72912206102237,57.495,-5.87844620539466));
#38013=CARTESIAN_POINT('Ctrl Pts',(-1.74698425466385,57.495,-5.90906068827417));
#38014=CARTESIAN_POINT('Ctrl Pts',(-1.76640606389863,57.495,-5.94073262861954));
#38015=CARTESIAN_POINT('Ctrl Pts',(-1.78726264793637,57.495,-5.97314358084405));
#38016=CARTESIAN_POINT('Ctrl Pts',(-1.80944727788364,57.495,-6.00602283509636));
#38017=CARTESIAN_POINT('Ctrl Pts',(-1.83289254541003,57.495,-6.03920034699142));
#38018=CARTESIAN_POINT('Ctrl Pts',(-1.85756929242873,57.495,-6.07260331771224));
#38019=CARTESIAN_POINT('Ctrl Pts',(-1.88347219921807,57.495,-6.10621926889293));
#38020=CARTESIAN_POINT('Ctrl Pts',(-1.91060895733316,57.495,-6.14006878432979));
#38021=CARTESIAN_POINT('Ctrl Pts',(-1.93898880419738,57.495,-6.17417680788948));
#38022=CARTESIAN_POINT('Ctrl Pts',(-1.96860861168855,57.495,-6.20853885514991));
#38023=CARTESIAN_POINT('Ctrl Pts',(-1.99945211810842,57.495,-6.24311798195999));
#38024=CARTESIAN_POINT('Ctrl Pts',(-2.03149622201774,57.495,-6.27785854554207));
#38025=CARTESIAN_POINT('Ctrl Pts',(-2.06471490843566,57.495,-6.31269482043472));
#38026=CARTESIAN_POINT('Ctrl Pts',(-2.09908352929886,57.495,-6.34756091533109));
#38027=CARTESIAN_POINT('Ctrl Pts',(-2.13458349574322,57.495,-6.38240181135686));
#38028=CARTESIAN_POINT('Ctrl Pts',(-2.17120312938032,57.495,-6.41717671306116));
#38029=CARTESIAN_POINT('Ctrl Pts',(-2.20893514043546,57.495,-6.45185553518355));
#38030=CARTESIAN_POINT('Ctrl Pts',(-2.24777479550452,57.495,-6.48641743997165));
#38031=CARTESIAN_POINT('Ctrl Pts',(-2.28771778279682,57.495,-6.52084865967131));
#38032=CARTESIAN_POINT('Ctrl Pts',(-2.32875748935431,57.495,-6.55514062276576));
#38033=CARTESIAN_POINT('Ctrl Pts',(-2.37088387159997,57.495,-6.58928830924833));
#38034=CARTESIAN_POINT('Ctrl Pts',(-2.41408612451247,57.495,-6.62328942425873));
#38035=CARTESIAN_POINT('Ctrl Pts',(-2.44950070161195,57.495,-6.65037263123044));
#38036=CARTESIAN_POINT('Ctrl Pts',(-2.47653809829367,57.495,-6.67061900235319));
#38037=CARTESIAN_POINT('Ctrl Pts',(-2.49477440711622,57.495,-6.6840872875067));
#38038=CARTESIAN_POINT('Ctrl Pts',(-2.50394540602692,57.495,-6.69081410619341));
#38039=CARTESIAN_POINT('',(-2.96056324982543,57.495,-6.5016768024705));
#38040=CARTESIAN_POINT('Origin',(-6.23660068148933E-13,57.495,-1.50456066262064E-12));
#38041=CARTESIAN_POINT('',(-2.87862685522557,57.495,-5.22677443144495));
#38042=CARTESIAN_POINT('Ctrl Pts',(-2.87862685522557,57.495,-5.22677443144495));
#38043=CARTESIAN_POINT('Ctrl Pts',(-2.88043681055508,57.495,-5.23024117954545));
#38044=CARTESIAN_POINT('Ctrl Pts',(-2.88406558980908,57.495,-5.2374521593957));
#38045=CARTESIAN_POINT('Ctrl Pts',(-2.88953536864324,57.495,-5.24910109063627));
#38046=CARTESIAN_POINT('Ctrl Pts',(-2.8968816873652,57.495,-5.26630084561717));
#38047=CARTESIAN_POINT('Ctrl Pts',(-2.90614521320845,57.495,-5.29057828960674));
#38048=CARTESIAN_POINT('Ctrl Pts',(-2.91546314862894,57.495,-5.31759510370885));
#38049=CARTESIAN_POINT('Ctrl Pts',(-2.92478335875772,57.495,-5.34725389048201));
#38050=CARTESIAN_POINT('Ctrl Pts',(-2.93401523982666,57.495,-5.37936310952307));
#38051=CARTESIAN_POINT('Ctrl Pts',(-2.94303247002252,57.495,-5.41364129622042));
#38052=CARTESIAN_POINT('Ctrl Pts',(-2.95169462080126,57.495,-5.44977003302479));
#38053=CARTESIAN_POINT('Ctrl Pts',(-2.95986479289848,57.495,-5.48743586913294));
#38054=CARTESIAN_POINT('Ctrl Pts',(-2.96742703426686,57.495,-5.52637191504897));
#38055=CARTESIAN_POINT('Ctrl Pts',(-2.97430877025613,57.495,-5.56641026634754));
#38056=CARTESIAN_POINT('Ctrl Pts',(-2.98047914221005,57.495,-5.60747882861056));
#38057=CARTESIAN_POINT('Ctrl Pts',(-2.98593308820275,57.495,-5.64956501668965));
#38058=CARTESIAN_POINT('Ctrl Pts',(-2.99067972442542,57.495,-5.6926888242775));
#38059=CARTESIAN_POINT('Ctrl Pts',(-2.99473015701058,57.495,-5.7368744211961));
#38060=CARTESIAN_POINT('Ctrl Pts',(-2.99808342690941,57.495,-5.78211642456377));
#38061=CARTESIAN_POINT('Ctrl Pts',(-3.00072490941925,57.495,-5.82837721216372));
#38062=CARTESIAN_POINT('Ctrl Pts',(-3.00263159433907,57.495,-5.87560110342618));
#38063=CARTESIAN_POINT('Ctrl Pts',(-3.00377540211876,57.495,-5.92372322806235));
#38064=CARTESIAN_POINT('Ctrl Pts',(-3.00412716938111,57.495,-5.97267956506957));
#38065=CARTESIAN_POINT('Ctrl Pts',(-3.00366113621889,57.495,-6.02241806591683));
#38066=CARTESIAN_POINT('Ctrl Pts',(-3.00235671375975,57.495,-6.07290162599645));
#38067=CARTESIAN_POINT('Ctrl Pts',(-3.00019778316116,57.495,-6.12410381716763));
#38068=CARTESIAN_POINT('Ctrl Pts',(-2.99717295692923,57.495,-6.1760065578922));
#38069=CARTESIAN_POINT('Ctrl Pts',(-2.9932755486881,57.495,-6.22859706400143));
#38070=CARTESIAN_POINT('Ctrl Pts',(-2.98850417352762,57.495,-6.28186459845025));
#38071=CARTESIAN_POINT('Ctrl Pts',(-2.98286238364847,57.495,-6.33579850967655));
#38072=CARTESIAN_POINT('Ctrl Pts',(-2.97635619664327,57.495,-6.39038953466525));
#38073=CARTESIAN_POINT('Ctrl Pts',(-2.97046502832937,57.495,-6.43458214159119));
#38074=CARTESIAN_POINT('Ctrl Pts',(-2.96566304810545,57.495,-6.4680168144459));
#38075=CARTESIAN_POINT('Ctrl Pts',(-2.96229154623624,57.495,-6.49043534784125));
#38076=CARTESIAN_POINT('Ctrl Pts',(-2.96056324982543,57.495,-6.5016768024705));
#38077=CARTESIAN_POINT('',(-2.58480949428933,57.495,-4.69328497730872));
#38078=CARTESIAN_POINT('',(-2.51244640654327,57.495,-4.56189402049717));
#38079=CARTESIAN_POINT('',(-3.34686616149372,57.495,-4.18409499139877));
#38080=CARTESIAN_POINT('Origin',(0.,57.495,0.));
#38081=CARTESIAN_POINT('',(-3.72730711280926,57.495,-4.65970441290367));
#38082=CARTESIAN_POINT('',(-3.72730711280926,57.495,-4.65970441290367));
#38083=CARTESIAN_POINT('',(-4.87380761862879,57.495,-5.22328778611671));
#38084=CARTESIAN_POINT('Ctrl Pts',(-3.72730711280926,57.495,-4.65970441290367));
#38085=CARTESIAN_POINT('Ctrl Pts',(-3.72981733050578,57.495,-4.66270326064959));
#38086=CARTESIAN_POINT('Ctrl Pts',(-3.73509073349858,57.495,-4.66881533805013));
#38087=CARTESIAN_POINT('Ctrl Pts',(-3.74375974890886,57.495,-4.67832660775287));
#38088=CARTESIAN_POINT('Ctrl Pts',(-3.75683893603616,57.495,-4.69169578253132));
#38089=CARTESIAN_POINT('Ctrl Pts',(-3.77572337177431,57.495,-4.7095447400518));
#38090=CARTESIAN_POINT('Ctrl Pts',(-3.7971178338476,57.495,-4.72849227702427));
#38091=CARTESIAN_POINT('Ctrl Pts',(-3.82095228990397,57.495,-4.74845295472312));
#38092=CARTESIAN_POINT('Ctrl Pts',(-3.84708445224627,57.495,-4.76926976684252));
#38093=CARTESIAN_POINT('Ctrl Pts',(-3.8753026227458,57.495,-4.79071829540103));
#38094=CARTESIAN_POINT('Ctrl Pts',(-3.90536636162318,57.495,-4.81254694822034));
#38095=CARTESIAN_POINT('Ctrl Pts',(-3.93703846717724,57.495,-4.83450929444279));
#38096=CARTESIAN_POINT('Ctrl Pts',(-3.97011673859274,57.495,-4.85639607415676));
#38097=CARTESIAN_POINT('Ctrl Pts',(-4.00447382552396,57.495,-4.87807598288654));
#38098=CARTESIAN_POINT('Ctrl Pts',(-4.04005493051012,57.495,-4.89949292161185));
#38099=CARTESIAN_POINT('Ctrl Pts',(-4.07685036350539,57.495,-4.92063739759521));
#38100=CARTESIAN_POINT('Ctrl Pts',(-4.11487510765791,57.495,-4.94152548435402));
#38101=CARTESIAN_POINT('Ctrl Pts',(-4.15414724283858,57.495,-4.96217669200723));
#38102=CARTESIAN_POINT('Ctrl Pts',(-4.1946621629253,57.495,-4.98258807456961));
#38103=CARTESIAN_POINT('Ctrl Pts',(-4.23639070615337,57.495,-5.00273172317863));
#38104=CARTESIAN_POINT('Ctrl Pts',(-4.27929023600674,57.495,-5.02256507114894));
#38105=CARTESIAN_POINT('Ctrl Pts',(-4.3233115657319,57.495,-5.04203735157413));
#38106=CARTESIAN_POINT('Ctrl Pts',(-4.36840670797617,57.495,-5.06109712122989));
#38107=CARTESIAN_POINT('Ctrl Pts',(-4.41453743405677,57.495,-5.07970066295468));
#38108=CARTESIAN_POINT('Ctrl Pts',(-4.4616773428065,57.495,-5.09781475579217));
#38109=CARTESIAN_POINT('Ctrl Pts',(-4.50980818622101,57.495,-5.11541439426204));
#38110=CARTESIAN_POINT('Ctrl Pts',(-4.5589176169425,57.495,-5.13248213818666));
#38111=CARTESIAN_POINT('Ctrl Pts',(-4.60899638270439,57.495,-5.14900691787064));
#38112=CARTESIAN_POINT('Ctrl Pts',(-4.66003509375265,57.495,-5.16498334493456));
#38113=CARTESIAN_POINT('Ctrl Pts',(-4.71202254995864,57.495,-5.18041062500752));
#38114=CARTESIAN_POINT('Ctrl Pts',(-4.7649478905793,57.495,-5.19529077281773));
#38115=CARTESIAN_POINT('Ctrl Pts',(-4.80803098811744,57.495,-5.20675982149348));
#38116=CARTESIAN_POINT('Ctrl Pts',(-4.84075823631825,57.495,-5.21511826561704));
#38117=CARTESIAN_POINT('Ctrl Pts',(-4.86276047837859,57.495,-5.2205826053545));
#38118=CARTESIAN_POINT('Ctrl Pts',(-4.87380761862879,57.495,-5.22328778611671));
#38119=CARTESIAN_POINT('',(-5.22328778611671,57.495,-4.87380761862879));
#38120=CARTESIAN_POINT('Origin',(-1.15195721078055E-12,57.495,-1.15136842610855E-12));
#38121=CARTESIAN_POINT('',(-4.65970441290367,57.495,-3.72730711280926));
#38122=CARTESIAN_POINT('Ctrl Pts',(-4.65970441290367,57.495,-3.72730711280926));
#38123=CARTESIAN_POINT('Ctrl Pts',(-4.66270326064961,57.495,-3.72981733050576));
#38124=CARTESIAN_POINT('Ctrl Pts',(-4.6688153380502,57.495,-3.73509073349854));
#38125=CARTESIAN_POINT('Ctrl Pts',(-4.67832660775297,57.495,-3.7437597489088));
#38126=CARTESIAN_POINT('Ctrl Pts',(-4.69169578253142,57.495,-3.7568389360361));
#38127=CARTESIAN_POINT('Ctrl Pts',(-4.70954474005187,57.495,-3.77572337177426));
#38128=CARTESIAN_POINT('Ctrl Pts',(-4.72849227702429,57.495,-3.79711783384759));
#38129=CARTESIAN_POINT('Ctrl Pts',(-4.74845295472311,57.495,-3.82095228990398));
#38130=CARTESIAN_POINT('Ctrl Pts',(-4.76926976684248,57.495,-3.84708445224628));
#38131=CARTESIAN_POINT('Ctrl Pts',(-4.79071829540097,57.495,-3.87530262274579));
#38132=CARTESIAN_POINT('Ctrl Pts',(-4.81254694822028,57.495,-3.90536636162316));
#38133=CARTESIAN_POINT('Ctrl Pts',(-4.83450929444277,57.495,-3.93703846717723));
#38134=CARTESIAN_POINT('Ctrl Pts',(-4.85639607415679,57.495,-3.97011673859275));
#38135=CARTESIAN_POINT('Ctrl Pts',(-4.8780759828866,57.495,-4.00447382552398));
#38136=CARTESIAN_POINT('Ctrl Pts',(-4.89949292161193,57.495,-4.04005493051016));
#38137=CARTESIAN_POINT('Ctrl Pts',(-4.92063739759527,57.495,-4.07685036350543));
#38138=CARTESIAN_POINT('Ctrl Pts',(-4.94152548435404,57.495,-4.11487510765792));
#38139=CARTESIAN_POINT('Ctrl Pts',(-4.9621766920072,57.495,-4.15414724283855));
#38140=CARTESIAN_POINT('Ctrl Pts',(-4.98258807456953,57.495,-4.19466216292523));
#38141=CARTESIAN_POINT('Ctrl Pts',(-5.00273172317852,57.495,-4.23639070615327));
#38142=CARTESIAN_POINT('Ctrl Pts',(-5.02256507114883,57.495,-4.27929023600664));
#38143=CARTESIAN_POINT('Ctrl Pts',(-5.04203735157409,57.495,-4.32331156573186));
#38144=CARTESIAN_POINT('Ctrl Pts',(-5.06109712122993,57.495,-4.36840670797621));
#38145=CARTESIAN_POINT('Ctrl Pts',(-5.07970066295481,57.495,-4.41453743405689));
#38146=CARTESIAN_POINT('Ctrl Pts',(-5.09781475579234,57.495,-4.46167734280668));
#38147=CARTESIAN_POINT('Ctrl Pts',(-5.11541439426219,57.495,-4.50980818622117));
#38148=CARTESIAN_POINT('Ctrl Pts',(-5.13248213818673,57.495,-4.55891761694258));
#38149=CARTESIAN_POINT('Ctrl Pts',(-5.14900691787061,57.495,-4.60899638270436));
#38150=CARTESIAN_POINT('Ctrl Pts',(-5.16498334493441,57.495,-4.66003509375248));
#38151=CARTESIAN_POINT('Ctrl Pts',(-5.1804106250073,57.495,-4.71202254995837));
#38152=CARTESIAN_POINT('Ctrl Pts',(-5.1952907728175,57.495,-4.764947890579));
#38153=CARTESIAN_POINT('Ctrl Pts',(-5.2067598214933,57.495,-4.8080309881172));
#38154=CARTESIAN_POINT('Ctrl Pts',(-5.21511826561693,57.495,-4.84075823631811));
#38155=CARTESIAN_POINT('Ctrl Pts',(-5.22058260535447,57.495,-4.86276047837853));
#38156=CARTESIAN_POINT('Ctrl Pts',(-5.22328778611671,57.495,-4.87380761862879));
#38157=CARTESIAN_POINT('',(-4.18409499139877,57.495,-3.34686616149372));
#38158=CARTESIAN_POINT('',(-4.06695907338649,57.495,-3.25316890053365));
#38159=CARTESIAN_POINT('',(-4.69328497730872,57.495,-2.58480949428933));
#38160=CARTESIAN_POINT('Origin',(0.,57.495,0.));
#38161=CARTESIAN_POINT('',(-5.22677443144495,57.495,-2.87862685522556));
#38162=CARTESIAN_POINT('',(-5.22677443144495,57.495,-2.87862685522556));
#38163=CARTESIAN_POINT('',(-6.50167680247051,57.495,-2.96056324982543));
#38164=CARTESIAN_POINT('Ctrl Pts',(-5.22677443144495,57.495,-2.87862685522556));
#38165=CARTESIAN_POINT('Ctrl Pts',(-5.23024117954545,57.495,-2.88043681055505));
#38166=CARTESIAN_POINT('Ctrl Pts',(-5.23745215939571,57.495,-2.884065589809));
#38167=CARTESIAN_POINT('Ctrl Pts',(-5.24910109063628,57.495,-2.88953536864313));
#38168=CARTESIAN_POINT('Ctrl Pts',(-5.26630084561719,57.495,-2.89688168736508));
#38169=CARTESIAN_POINT('Ctrl Pts',(-5.29057828960676,57.495,-2.90614521320837));
#38170=CARTESIAN_POINT('Ctrl Pts',(-5.31759510370885,57.495,-2.91546314862891));
#38171=CARTESIAN_POINT('Ctrl Pts',(-5.34725389048201,57.495,-2.92478335875774));
#38172=CARTESIAN_POINT('Ctrl Pts',(-5.37936310952307,57.495,-2.93401523982671));
#38173=CARTESIAN_POINT('Ctrl Pts',(-5.41364129622045,57.495,-2.94303247002258));
#38174=CARTESIAN_POINT('Ctrl Pts',(-5.44977003302482,57.495,-2.95169462080131));
#38175=CARTESIAN_POINT('Ctrl Pts',(-5.48743586913296,57.495,-2.9598647928985));
#38176=CARTESIAN_POINT('Ctrl Pts',(-5.52637191504895,57.495,-2.96742703426683));
#38177=CARTESIAN_POINT('Ctrl Pts',(-5.56641026634749,57.495,-2.97430877025609));
#38178=CARTESIAN_POINT('Ctrl Pts',(-5.6074788286105,57.495,-2.98047914221));
#38179=CARTESIAN_POINT('Ctrl Pts',(-5.64956501668959,57.495,-2.98593308820271));
#38180=CARTESIAN_POINT('Ctrl Pts',(-5.69268882427748,57.495,-2.9906797244254));
#38181=CARTESIAN_POINT('Ctrl Pts',(-5.73687442119613,57.495,-2.9947301570106));
#38182=CARTESIAN_POINT('Ctrl Pts',(-5.78211642456387,57.495,-2.99808342690946));
#38183=CARTESIAN_POINT('Ctrl Pts',(-5.82837721216385,57.495,-3.00072490941932));
#38184=CARTESIAN_POINT('Ctrl Pts',(-5.87560110342631,57.495,-3.00263159433912));
#38185=CARTESIAN_POINT('Ctrl Pts',(-5.9237232280624,57.495,-3.00377540211877));
#38186=CARTESIAN_POINT('Ctrl Pts',(-5.97267956506952,57.495,-3.00412716938109));
#38187=CARTESIAN_POINT('Ctrl Pts',(-6.02241806591666,57.495,-3.00366113621883));
#38188=CARTESIAN_POINT('Ctrl Pts',(-6.07290162599622,57.495,-3.00235671375967));
#38189=CARTESIAN_POINT('Ctrl Pts',(-6.12410381716742,57.495,-3.00019778316108));
#38190=CARTESIAN_POINT('Ctrl Pts',(-6.17600655789209,57.495,-2.99717295692919));
#38191=CARTESIAN_POINT('Ctrl Pts',(-6.22859706400147,57.495,-2.99327554868811));
#38192=CARTESIAN_POINT('Ctrl Pts',(-6.28186459845047,57.495,-2.98850417352769));
#38193=CARTESIAN_POINT('Ctrl Pts',(-6.33579850967689,57.495,-2.98286238364857));
#38194=CARTESIAN_POINT('Ctrl Pts',(-6.39038953466561,57.495,-2.97635619664337));
#38195=CARTESIAN_POINT('Ctrl Pts',(-6.43458214159149,57.495,-2.97046502832945));
#38196=CARTESIAN_POINT('Ctrl Pts',(-6.46801681444607,57.495,-2.96566304810549));
#38197=CARTESIAN_POINT('Ctrl Pts',(-6.49043534784131,57.495,-2.96229154623625));
#38198=CARTESIAN_POINT('Ctrl Pts',(-6.50167680247051,57.495,-2.96056324982543));
#38199=CARTESIAN_POINT('',(-6.69081410619341,57.495,-2.50394540602692));
#38200=CARTESIAN_POINT('Origin',(-1.50487931058895E-12,57.495,-6.22890783902202E-13));
#38201=CARTESIAN_POINT('',(-5.73138421404289,57.495,-1.66039107437148));
#38202=CARTESIAN_POINT('Ctrl Pts',(-5.73138421404289,57.495,-1.66039107437148));
#38203=CARTESIAN_POINT('Ctrl Pts',(-5.73511540682056,57.495,-1.66156260377487));
#38204=CARTESIAN_POINT('Ctrl Pts',(-5.7427802739896,57.495,-1.66409560210805));
#38205=CARTESIAN_POINT('Ctrl Pts',(-5.75488502996861,57.495,-1.6684649226766));
#38206=CARTESIAN_POINT('Ctrl Pts',(-5.77224172513541,57.495,-1.67543235427329));
#38207=CARTESIAN_POINT('Ctrl Pts',(-5.79595877235177,57.495,-1.68604879760674));
#38208=CARTESIAN_POINT('Ctrl Pts',(-5.82165132013192,57.495,-1.69856379474191));
#38209=CARTESIAN_POINT('Ctrl Pts',(-5.84921363316513,57.495,-1.71294534020683));
#38210=CARTESIAN_POINT('Ctrl Pts',(-5.87844620539462,57.495,-1.7291220610224));
#38211=CARTESIAN_POINT('Ctrl Pts',(-5.90906068827411,57.495,-1.74698425466387));
#38212=CARTESIAN_POINT('Ctrl Pts',(-5.94073262861949,57.495,-1.76640606389864));
#38213=CARTESIAN_POINT('Ctrl Pts',(-5.97314358084403,57.495,-1.78726264793636));
#38214=CARTESIAN_POINT('Ctrl Pts',(-6.00602283509639,57.495,-1.80944727788364));
#38215=CARTESIAN_POINT('Ctrl Pts',(-6.03920034699149,57.495,-1.83289254541003));
#38216=CARTESIAN_POINT('Ctrl Pts',(-6.07260331771232,57.495,-1.85756929242873));
#38217=CARTESIAN_POINT('Ctrl Pts',(-6.10621926889299,57.495,-1.88347219921808));
#38218=CARTESIAN_POINT('Ctrl Pts',(-6.14006878432982,57.495,-1.91060895733317));
#38219=CARTESIAN_POINT('Ctrl Pts',(-6.17417680788945,57.495,-1.93898880419737));
#38220=CARTESIAN_POINT('Ctrl Pts',(-6.20853885514981,57.495,-1.96860861168851));
#38221=CARTESIAN_POINT('Ctrl Pts',(-6.24311798195985,57.495,-1.99945211810837));
#38222=CARTESIAN_POINT('Ctrl Pts',(-6.27785854554194,57.495,-2.03149622201768));
#38223=CARTESIAN_POINT('Ctrl Pts',(-6.31269482043467,57.495,-2.06471490843563));
#38224=CARTESIAN_POINT('Ctrl Pts',(-6.34756091533115,57.495,-2.09908352929888));
#38225=CARTESIAN_POINT('Ctrl Pts',(-6.38240181135703,57.495,-2.13458349574329));
#38226=CARTESIAN_POINT('Ctrl Pts',(-6.41717671306138,57.495,-2.17120312938042));
#38227=CARTESIAN_POINT('Ctrl Pts',(-6.45185553518375,57.495,-2.20893514043555));
#38228=CARTESIAN_POINT('Ctrl Pts',(-6.48641743997175,57.495,-2.24777479550457));
#38229=CARTESIAN_POINT('Ctrl Pts',(-6.52084865967127,57.495,-2.2877177827968));
#38230=CARTESIAN_POINT('Ctrl Pts',(-6.55514062276556,57.495,-2.32875748935421));
#38231=CARTESIAN_POINT('Ctrl Pts',(-6.58928830924802,57.495,-2.37088387159981));
#38232=CARTESIAN_POINT('Ctrl Pts',(-6.6232894242584,57.495,-2.41408612451229));
#38233=CARTESIAN_POINT('Ctrl Pts',(-6.65037263123018,57.495,-2.4495007016118));
#38234=CARTESIAN_POINT('Ctrl Pts',(-6.67061900235304,57.495,-2.47653809829358));
#38235=CARTESIAN_POINT('Ctrl Pts',(-6.68408728750664,57.495,-2.49477440711619));
#38236=CARTESIAN_POINT('Ctrl Pts',(-6.69081410619341,57.495,-2.50394540602692));
#38237=CARTESIAN_POINT('',(-5.1463899549833,57.495,-1.4909173120086));
#38238=CARTESIAN_POINT('',(-5.00231408838243,57.495,-1.44917830551339));
#38239=CARTESIAN_POINT('',(-5.32519370006274,57.495,-0.592010183030743));
#38240=CARTESIAN_POINT('Origin',(0.,57.495,0.));
#38241=CARTESIAN_POINT('',(-5.93051272372135,57.495,-0.659304453656786));
#38242=CARTESIAN_POINT('',(-5.93051272372135,57.495,-0.659304453656786));
#38243=CARTESIAN_POINT('',(-7.13972463098307,57.495,-0.247119796320916));
#38244=CARTESIAN_POINT('Ctrl Pts',(-5.93051272372135,57.495,-0.659304453656786));
#38245=CARTESIAN_POINT('Ctrl Pts',(-5.93440822125369,57.495,-0.659649967278209));
#38246=CARTESIAN_POINT('Ctrl Pts',(-5.94245897164689,57.495,-0.660242999639131));
#38247=CARTESIAN_POINT('Ctrl Pts',(-5.95531437453421,57.495,-0.660838563360812));
#38248=CARTESIAN_POINT('Ctrl Pts',(-5.97401619058905,57.495,-0.661043615595395));
#38249=CARTESIAN_POINT('Ctrl Pts',(-5.99999062205821,57.495,-0.660311421925919));
#38250=CARTESIAN_POINT('Ctrl Pts',(-6.02851672315009,57.495,-0.658581184594065));
#38251=CARTESIAN_POINT('Ctrl Pts',(-6.05948455921138,57.495,-0.655842009648654));
#38252=CARTESIAN_POINT('Ctrl Pts',(-6.092682497423,57.495,-0.652083489461663));
#38253=CARTESIAN_POINT('Ctrl Pts',(-6.12780215712609,57.495,-0.647296629738964));
#38254=CARTESIAN_POINT('Ctrl Pts',(-6.16449561918681,57.495,-0.641473544543642));
#38255=CARTESIAN_POINT('Ctrl Pts',(-6.2024209037432,57.495,-0.63460770787657));
#38256=CARTESIAN_POINT('Ctrl Pts',(-6.24128706412512,57.495,-0.626694128202827));
#38257=CARTESIAN_POINT('Ctrl Pts',(-6.28091120375433,57.495,-0.617730009530283));
#38258=CARTESIAN_POINT('Ctrl Pts',(-6.32121490697708,57.495,-0.607714431517378));
#38259=CARTESIAN_POINT('Ctrl Pts',(-6.36218460951721,57.495,-0.596647533682195));
#38260=CARTESIAN_POINT('Ctrl Pts',(-6.40384227175349,57.495,-0.584530087032233));
#38261=CARTESIAN_POINT('Ctrl Pts',(-6.4462144738227,57.495,-0.571363102905585));
#38262=CARTESIAN_POINT('Ctrl Pts',(-6.48929587557851,57.495,-0.557147755196287));
#38263=CARTESIAN_POINT('Ctrl Pts',(-6.53304612199338,57.495,-0.541884929839958));
#38264=CARTESIAN_POINT('Ctrl Pts',(-6.57740496530586,57.495,-0.52557467621436));
#38265=CARTESIAN_POINT('Ctrl Pts',(-6.62230172760518,57.495,-0.508215876982667));
#38266=CARTESIAN_POINT('Ctrl Pts',(-6.66766610085612,57.495,-0.48980608847462));
#38267=CARTESIAN_POINT('Ctrl Pts',(-6.71344014059646,57.495,-0.470341429749656));
#38268=CARTESIAN_POINT('Ctrl Pts',(-6.75958168761835,57.495,-0.449817078488634));
#38269=CARTESIAN_POINT('Ctrl Pts',(-6.80606015708944,57.495,-0.428228256434481));
#38270=CARTESIAN_POINT('Ctrl Pts',(-6.85285448604147,57.495,-0.405571362419762));
#38271=CARTESIAN_POINT('Ctrl Pts',(-6.89995030467732,57.495,-0.381845111328231));
#38272=CARTESIAN_POINT('Ctrl Pts',(-6.94733716327859,57.495,-0.357052332559016));
#38273=CARTESIAN_POINT('Ctrl Pts',(-6.99500658045334,57.495,-0.331200384093975));
#38274=CARTESIAN_POINT('Ctrl Pts',(-7.04295230112448,57.495,-0.304298370266162));
#38275=CARTESIAN_POINT('Ctrl Pts',(-7.0815264936406,57.495,-0.281943861934803));
#38276=CARTESIAN_POINT('Ctrl Pts',(-7.1105784652929,57.495,-0.264712515322364));
#38277=CARTESIAN_POINT('Ctrl Pts',(-7.13000027153814,57.495,-0.253018452443266));
#38278=CARTESIAN_POINT('Ctrl Pts',(-7.13972463098307,57.495,-0.247119796320916));
#38279=CARTESIAN_POINT('',(-7.13972463098307,57.495,0.24711979632092));
#38280=CARTESIAN_POINT('Origin',(-1.6286971771251E-12,57.495,4.16333634234533E-16));
#38281=CARTESIAN_POINT('',(-5.93051272372135,57.495,0.659304453656788));
#38282=CARTESIAN_POINT('Ctrl Pts',(-5.93051272372135,57.495,0.659304453656788));
#38283=CARTESIAN_POINT('Ctrl Pts',(-5.9344082212537,57.495,0.659649967278237));
#38284=CARTESIAN_POINT('Ctrl Pts',(-5.94245897164691,57.495,0.660242999639201));
#38285=CARTESIAN_POINT('Ctrl Pts',(-5.95531437453424,57.495,0.660838563360922));
#38286=CARTESIAN_POINT('Ctrl Pts',(-5.97401619058907,57.495,0.661043615595512));
#38287=CARTESIAN_POINT('Ctrl Pts',(-5.99999062205823,57.495,0.660311421925997));
#38288=CARTESIAN_POINT('Ctrl Pts',(-6.0285167231501,57.495,0.658581184594089));
#38289=CARTESIAN_POINT('Ctrl Pts',(-6.05948455921138,57.495,0.655842009648634));
#38290=CARTESIAN_POINT('Ctrl Pts',(-6.09268249742298,57.495,0.65208348946162));
#38291=CARTESIAN_POINT('Ctrl Pts',(-6.12780215712604,57.495,0.64729662973892));
#38292=CARTESIAN_POINT('Ctrl Pts',(-6.16449561918676,57.495,0.641473544543615));
#38293=CARTESIAN_POINT('Ctrl Pts',(-6.20242090374318,57.495,0.634607707876565));
#38294=CARTESIAN_POINT('Ctrl Pts',(-6.24128706412515,57.495,0.626694128202842));
#38295=CARTESIAN_POINT('Ctrl Pts',(-6.2809112037544,57.495,0.617730009530307));
#38296=CARTESIAN_POINT('Ctrl Pts',(-6.32121490697716,57.495,0.607714431517402));
#38297=CARTESIAN_POINT('Ctrl Pts',(-6.36218460951727,57.495,0.596647533682211));
#38298=CARTESIAN_POINT('Ctrl Pts',(-6.40384227175352,57.495,0.584530087032238));
#38299=CARTESIAN_POINT('Ctrl Pts',(-6.44621447382266,57.495,0.57136310290558));
#38300=CARTESIAN_POINT('Ctrl Pts',(-6.4892958755784,57.495,0.557147755196277));
#38301=CARTESIAN_POINT('Ctrl Pts',(-6.53304612199323,57.495,0.54188492983995));
#38302=CARTESIAN_POINT('Ctrl Pts',(-6.57740496530571,57.495,0.525574676214356));
#38303=CARTESIAN_POINT('Ctrl Pts',(-6.62230172760513,57.495,0.508215876982669));
#38304=CARTESIAN_POINT('Ctrl Pts',(-6.66766610085618,57.495,0.489806088474623));
#38305=CARTESIAN_POINT('Ctrl Pts',(-6.71344014059664,57.495,0.470341429749656));
#38306=CARTESIAN_POINT('Ctrl Pts',(-6.75958168761858,57.495,0.449817078488629));
#38307=CARTESIAN_POINT('Ctrl Pts',(-6.80606015708966,57.495,0.428228256434473));
#38308=CARTESIAN_POINT('Ctrl Pts',(-6.85285448604159,57.495,0.405571362419756));
#38309=CARTESIAN_POINT('Ctrl Pts',(-6.89995030467727,57.495,0.381845111328235));
#38310=CARTESIAN_POINT('Ctrl Pts',(-6.94733716327837,57.495,0.357052332559036));
#38311=CARTESIAN_POINT('Ctrl Pts',(-6.99500658045299,57.495,0.331200384094009));
#38312=CARTESIAN_POINT('Ctrl Pts',(-7.0429523011241,57.495,0.304298370266205));
#38313=CARTESIAN_POINT('Ctrl Pts',(-7.0815264936403,57.495,0.28194386193484));
#38314=CARTESIAN_POINT('Ctrl Pts',(-7.11057846529273,57.495,0.264712515322387));
#38315=CARTESIAN_POINT('Ctrl Pts',(-7.13000027153808,57.495,0.253018452443276));
#38316=CARTESIAN_POINT('Ctrl Pts',(-7.13972463098307,57.495,0.247119796320917));
#38317=CARTESIAN_POINT('',(-5.32519370006274,57.495,0.592010183030744));
#38318=CARTESIAN_POINT('',(-5.17611212951227,57.495,0.575436549687218));
#38319=CARTESIAN_POINT('',(-5.1463899549833,57.495,1.4909173120086));
#38320=CARTESIAN_POINT('Origin',(0.,57.495,0.));
#38321=CARTESIAN_POINT('',(-5.73138421404289,57.495,1.66039107437148));
#38322=CARTESIAN_POINT('',(-5.73138421404289,57.495,1.66039107437148));
#38323=CARTESIAN_POINT('',(-6.69081410619341,57.495,2.50394540602692));
#38324=CARTESIAN_POINT('Ctrl Pts',(-5.73138421404289,57.495,1.66039107437148));
#38325=CARTESIAN_POINT('Ctrl Pts',(-5.73511540682054,57.495,1.66156260377489));
#38326=CARTESIAN_POINT('Ctrl Pts',(-5.74278027398956,57.495,1.6640956021081));
#38327=CARTESIAN_POINT('Ctrl Pts',(-5.75488502996854,57.495,1.66846492267669));
#38328=CARTESIAN_POINT('Ctrl Pts',(-5.77224172513534,57.495,1.67543235427339));
#38329=CARTESIAN_POINT('Ctrl Pts',(-5.79595877235173,57.495,1.68604879760681));
#38330=CARTESIAN_POINT('Ctrl Pts',(-5.8216513201319,57.495,1.69856379474193));
#38331=CARTESIAN_POINT('Ctrl Pts',(-5.84921363316514,57.495,1.71294534020681));
#38332=CARTESIAN_POINT('Ctrl Pts',(-5.87844620539466,57.495,1.72912206102237));
#38333=CARTESIAN_POINT('Ctrl Pts',(-5.90906068827417,57.495,1.74698425466385));
#38334=CARTESIAN_POINT('Ctrl Pts',(-5.94073262861954,57.495,1.76640606389863));
#38335=CARTESIAN_POINT('Ctrl Pts',(-5.97314358084405,57.495,1.78726264793637));
#38336=CARTESIAN_POINT('Ctrl Pts',(-6.00602283509636,57.495,1.80944727788364));
#38337=CARTESIAN_POINT('Ctrl Pts',(-6.03920034699142,57.495,1.83289254541003));
#38338=CARTESIAN_POINT('Ctrl Pts',(-6.07260331771224,57.495,1.85756929242873));
#38339=CARTESIAN_POINT('Ctrl Pts',(-6.10621926889293,57.495,1.88347219921807));
#38340=CARTESIAN_POINT('Ctrl Pts',(-6.14006878432979,57.495,1.91060895733316));
#38341=CARTESIAN_POINT('Ctrl Pts',(-6.17417680788948,57.495,1.93898880419738));
#38342=CARTESIAN_POINT('Ctrl Pts',(-6.20853885514991,57.495,1.96860861168855));
#38343=CARTESIAN_POINT('Ctrl Pts',(-6.24311798195999,57.495,1.99945211810842));
#38344=CARTESIAN_POINT('Ctrl Pts',(-6.27785854554207,57.495,2.03149622201774));
#38345=CARTESIAN_POINT('Ctrl Pts',(-6.31269482043472,57.495,2.06471490843565));
#38346=CARTESIAN_POINT('Ctrl Pts',(-6.34756091533109,57.495,2.09908352929886));
#38347=CARTESIAN_POINT('Ctrl Pts',(-6.38240181135686,57.495,2.13458349574322));
#38348=CARTESIAN_POINT('Ctrl Pts',(-6.41717671306116,57.495,2.17120312938032));
#38349=CARTESIAN_POINT('Ctrl Pts',(-6.45185553518355,57.495,2.20893514043546));
#38350=CARTESIAN_POINT('Ctrl Pts',(-6.48641743997165,57.495,2.24777479550452));
#38351=CARTESIAN_POINT('Ctrl Pts',(-6.52084865967131,57.495,2.28771778279682));
#38352=CARTESIAN_POINT('Ctrl Pts',(-6.55514062276576,57.495,2.32875748935431));
#38353=CARTESIAN_POINT('Ctrl Pts',(-6.58928830924833,57.495,2.37088387159997));
#38354=CARTESIAN_POINT('Ctrl Pts',(-6.62328942425873,57.495,2.41408612451247));
#38355=CARTESIAN_POINT('Ctrl Pts',(-6.65037263123044,57.495,2.44950070161195));
#38356=CARTESIAN_POINT('Ctrl Pts',(-6.67061900235319,57.495,2.47653809829367));
#38357=CARTESIAN_POINT('Ctrl Pts',(-6.6840872875067,57.495,2.49477440711622));
#38358=CARTESIAN_POINT('Ctrl Pts',(-6.69081410619341,57.495,2.50394540602692));
#38359=CARTESIAN_POINT('',(-6.5016768024705,57.495,2.96056324982543));
#38360=CARTESIAN_POINT('Origin',(-1.50456066262064E-12,57.495,6.23660068148933E-13));
#38361=CARTESIAN_POINT('',(-5.22677443144495,57.495,2.87862685522557));
#38362=CARTESIAN_POINT('Ctrl Pts',(-5.22677443144495,57.495,2.87862685522557));
#38363=CARTESIAN_POINT('Ctrl Pts',(-5.23024117954545,57.495,2.88043681055507));
#38364=CARTESIAN_POINT('Ctrl Pts',(-5.2374521593957,57.495,2.88406558980908));
#38365=CARTESIAN_POINT('Ctrl Pts',(-5.24910109063627,57.495,2.88953536864324));
#38366=CARTESIAN_POINT('Ctrl Pts',(-5.26630084561717,57.495,2.8968816873652));
#38367=CARTESIAN_POINT('Ctrl Pts',(-5.29057828960674,57.495,2.90614521320845));
#38368=CARTESIAN_POINT('Ctrl Pts',(-5.31759510370885,57.495,2.91546314862894));
#38369=CARTESIAN_POINT('Ctrl Pts',(-5.34725389048201,57.495,2.92478335875772));
#38370=CARTESIAN_POINT('Ctrl Pts',(-5.37936310952307,57.495,2.93401523982666));
#38371=CARTESIAN_POINT('Ctrl Pts',(-5.41364129622042,57.495,2.94303247002252));
#38372=CARTESIAN_POINT('Ctrl Pts',(-5.44977003302479,57.495,2.95169462080126));
#38373=CARTESIAN_POINT('Ctrl Pts',(-5.48743586913294,57.495,2.95986479289848));
#38374=CARTESIAN_POINT('Ctrl Pts',(-5.52637191504897,57.495,2.96742703426686));
#38375=CARTESIAN_POINT('Ctrl Pts',(-5.56641026634754,57.495,2.97430877025613));
#38376=CARTESIAN_POINT('Ctrl Pts',(-5.60747882861056,57.495,2.98047914221005));
#38377=CARTESIAN_POINT('Ctrl Pts',(-5.64956501668965,57.495,2.98593308820275));
#38378=CARTESIAN_POINT('Ctrl Pts',(-5.6926888242775,57.495,2.99067972442542));
#38379=CARTESIAN_POINT('Ctrl Pts',(-5.7368744211961,57.495,2.99473015701058));
#38380=CARTESIAN_POINT('Ctrl Pts',(-5.78211642456377,57.495,2.99808342690941));
#38381=CARTESIAN_POINT('Ctrl Pts',(-5.82837721216372,57.495,3.00072490941925));
#38382=CARTESIAN_POINT('Ctrl Pts',(-5.87560110342618,57.495,3.00263159433907));
#38383=CARTESIAN_POINT('Ctrl Pts',(-5.92372322806235,57.495,3.00377540211876));
#38384=CARTESIAN_POINT('Ctrl Pts',(-5.97267956506957,57.495,3.00412716938111));
#38385=CARTESIAN_POINT('Ctrl Pts',(-6.02241806591683,57.495,3.00366113621889));
#38386=CARTESIAN_POINT('Ctrl Pts',(-6.07290162599645,57.495,3.00235671375975));
#38387=CARTESIAN_POINT('Ctrl Pts',(-6.12410381716763,57.495,3.00019778316116));
#38388=CARTESIAN_POINT('Ctrl Pts',(-6.1760065578922,57.495,2.99717295692923));
#38389=CARTESIAN_POINT('Ctrl Pts',(-6.22859706400143,57.495,2.9932755486881));
#38390=CARTESIAN_POINT('Ctrl Pts',(-6.28186459845025,57.495,2.98850417352762));
#38391=CARTESIAN_POINT('Ctrl Pts',(-6.33579850967655,57.495,2.98286238364847));
#38392=CARTESIAN_POINT('Ctrl Pts',(-6.39038953466525,57.495,2.97635619664327));
#38393=CARTESIAN_POINT('Ctrl Pts',(-6.43458214159119,57.495,2.97046502832937));
#38394=CARTESIAN_POINT('Ctrl Pts',(-6.4680168144459,57.495,2.96566304810545));
#38395=CARTESIAN_POINT('Ctrl Pts',(-6.49043534784125,57.495,2.96229154623624));
#38396=CARTESIAN_POINT('Ctrl Pts',(-6.5016768024705,57.495,2.96056324982543));
#38397=CARTESIAN_POINT('',(-4.69328497730872,57.495,2.58480949428933));
#38398=CARTESIAN_POINT('',(-4.56189402049717,57.495,2.51244640654327));
#38399=CARTESIAN_POINT('',(-4.18409499139877,57.495,3.34686616149372));
#38400=CARTESIAN_POINT('Origin',(0.,57.495,0.));
#38401=CARTESIAN_POINT('',(-4.65970441290367,57.495,3.72730711280926));
#38402=CARTESIAN_POINT('',(-4.65970441290367,57.495,3.72730711280926));
#38403=CARTESIAN_POINT('',(-5.22328778611671,57.495,4.87380761862879));
#38404=CARTESIAN_POINT('Ctrl Pts',(-4.65970441290367,57.495,3.72730711280926));
#38405=CARTESIAN_POINT('Ctrl Pts',(-4.66270326064959,57.495,3.72981733050578));
#38406=CARTESIAN_POINT('Ctrl Pts',(-4.66881533805013,57.495,3.73509073349858));
#38407=CARTESIAN_POINT('Ctrl Pts',(-4.67832660775287,57.495,3.74375974890886));
#38408=CARTESIAN_POINT('Ctrl Pts',(-4.69169578253132,57.495,3.75683893603616));
#38409=CARTESIAN_POINT('Ctrl Pts',(-4.7095447400518,57.495,3.77572337177431));
#38410=CARTESIAN_POINT('Ctrl Pts',(-4.72849227702427,57.495,3.7971178338476));
#38411=CARTESIAN_POINT('Ctrl Pts',(-4.74845295472312,57.495,3.82095228990397));
#38412=CARTESIAN_POINT('Ctrl Pts',(-4.76926976684252,57.495,3.84708445224627));
#38413=CARTESIAN_POINT('Ctrl Pts',(-4.79071829540103,57.495,3.8753026227458));
#38414=CARTESIAN_POINT('Ctrl Pts',(-4.81254694822034,57.495,3.90536636162318));
#38415=CARTESIAN_POINT('Ctrl Pts',(-4.83450929444279,57.495,3.93703846717724));
#38416=CARTESIAN_POINT('Ctrl Pts',(-4.85639607415676,57.495,3.97011673859274));
#38417=CARTESIAN_POINT('Ctrl Pts',(-4.87807598288654,57.495,4.00447382552396));
#38418=CARTESIAN_POINT('Ctrl Pts',(-4.89949292161185,57.495,4.04005493051012));
#38419=CARTESIAN_POINT('Ctrl Pts',(-4.92063739759521,57.495,4.07685036350539));
#38420=CARTESIAN_POINT('Ctrl Pts',(-4.94152548435402,57.495,4.11487510765791));
#38421=CARTESIAN_POINT('Ctrl Pts',(-4.96217669200723,57.495,4.15414724283858));
#38422=CARTESIAN_POINT('Ctrl Pts',(-4.98258807456962,57.495,4.1946621629253));
#38423=CARTESIAN_POINT('Ctrl Pts',(-5.00273172317863,57.495,4.23639070615337));
#38424=CARTESIAN_POINT('Ctrl Pts',(-5.02256507114894,57.495,4.27929023600674));
#38425=CARTESIAN_POINT('Ctrl Pts',(-5.04203735157413,57.495,4.3233115657319));
#38426=CARTESIAN_POINT('Ctrl Pts',(-5.06109712122989,57.495,4.36840670797617));
#38427=CARTESIAN_POINT('Ctrl Pts',(-5.07970066295468,57.495,4.41453743405677));
#38428=CARTESIAN_POINT('Ctrl Pts',(-5.09781475579217,57.495,4.4616773428065));
#38429=CARTESIAN_POINT('Ctrl Pts',(-5.11541439426204,57.495,4.50980818622101));
#38430=CARTESIAN_POINT('Ctrl Pts',(-5.13248213818666,57.495,4.5589176169425));
#38431=CARTESIAN_POINT('Ctrl Pts',(-5.14900691787064,57.495,4.60899638270439));
#38432=CARTESIAN_POINT('Ctrl Pts',(-5.16498334493456,57.495,4.66003509375265));
#38433=CARTESIAN_POINT('Ctrl Pts',(-5.18041062500752,57.495,4.71202254995864));
#38434=CARTESIAN_POINT('Ctrl Pts',(-5.19529077281773,57.495,4.7649478905793));
#38435=CARTESIAN_POINT('Ctrl Pts',(-5.20675982149348,57.495,4.80803098811744));
#38436=CARTESIAN_POINT('Ctrl Pts',(-5.21511826561704,57.495,4.84075823631825));
#38437=CARTESIAN_POINT('Ctrl Pts',(-5.22058260535451,57.495,4.86276047837859));
#38438=CARTESIAN_POINT('Ctrl Pts',(-5.22328778611671,57.495,4.87380761862879));
#38439=CARTESIAN_POINT('',(-4.87380761862879,57.495,5.22328778611671));
#38440=CARTESIAN_POINT('Origin',(-1.15136842610855E-12,57.495,1.15195721078055E-12));
#38441=CARTESIAN_POINT('',(-3.72730711280926,57.495,4.65970441290367));
#38442=CARTESIAN_POINT('Ctrl Pts',(-3.72730711280926,57.495,4.65970441290367));
#38443=CARTESIAN_POINT('Ctrl Pts',(-3.72981733050576,57.495,4.66270326064961));
#38444=CARTESIAN_POINT('Ctrl Pts',(-3.73509073349854,57.495,4.6688153380502));
#38445=CARTESIAN_POINT('Ctrl Pts',(-3.7437597489088,57.495,4.67832660775297));
#38446=CARTESIAN_POINT('Ctrl Pts',(-3.7568389360361,57.495,4.69169578253142));
#38447=CARTESIAN_POINT('Ctrl Pts',(-3.77572337177426,57.495,4.70954474005187));
#38448=CARTESIAN_POINT('Ctrl Pts',(-3.79711783384759,57.495,4.72849227702429));
#38449=CARTESIAN_POINT('Ctrl Pts',(-3.82095228990398,57.495,4.74845295472311));
#38450=CARTESIAN_POINT('Ctrl Pts',(-3.84708445224628,57.495,4.76926976684248));
#38451=CARTESIAN_POINT('Ctrl Pts',(-3.87530262274579,57.495,4.79071829540097));
#38452=CARTESIAN_POINT('Ctrl Pts',(-3.90536636162316,57.495,4.81254694822028));
#38453=CARTESIAN_POINT('Ctrl Pts',(-3.93703846717723,57.495,4.83450929444277));
#38454=CARTESIAN_POINT('Ctrl Pts',(-3.97011673859275,57.495,4.85639607415679));
#38455=CARTESIAN_POINT('Ctrl Pts',(-4.00447382552398,57.495,4.8780759828866));
#38456=CARTESIAN_POINT('Ctrl Pts',(-4.04005493051016,57.495,4.89949292161193));
#38457=CARTESIAN_POINT('Ctrl Pts',(-4.07685036350543,57.495,4.92063739759527));
#38458=CARTESIAN_POINT('Ctrl Pts',(-4.11487510765792,57.495,4.94152548435404));
#38459=CARTESIAN_POINT('Ctrl Pts',(-4.15414724283855,57.495,4.9621766920072));
#38460=CARTESIAN_POINT('Ctrl Pts',(-4.19466216292523,57.495,4.98258807456953));
#38461=CARTESIAN_POINT('Ctrl Pts',(-4.23639070615327,57.495,5.00273172317852));
#38462=CARTESIAN_POINT('Ctrl Pts',(-4.27929023600664,57.495,5.02256507114883));
#38463=CARTESIAN_POINT('Ctrl Pts',(-4.32331156573186,57.495,5.04203735157409));
#38464=CARTESIAN_POINT('Ctrl Pts',(-4.36840670797621,57.495,5.06109712122993));
#38465=CARTESIAN_POINT('Ctrl Pts',(-4.41453743405689,57.495,5.07970066295481));
#38466=CARTESIAN_POINT('Ctrl Pts',(-4.46167734280668,57.495,5.09781475579234));
#38467=CARTESIAN_POINT('Ctrl Pts',(-4.50980818622117,57.495,5.11541439426219));
#38468=CARTESIAN_POINT('Ctrl Pts',(-4.55891761694258,57.495,5.13248213818673));
#38469=CARTESIAN_POINT('Ctrl Pts',(-4.60899638270436,57.495,5.14900691787061));
#38470=CARTESIAN_POINT('Ctrl Pts',(-4.66003509375248,57.495,5.16498334493441));
#38471=CARTESIAN_POINT('Ctrl Pts',(-4.71202254995837,57.495,5.1804106250073));
#38472=CARTESIAN_POINT('Ctrl Pts',(-4.764947890579,57.495,5.1952907728175));
#38473=CARTESIAN_POINT('Ctrl Pts',(-4.8080309881172,57.495,5.2067598214933));
#38474=CARTESIAN_POINT('Ctrl Pts',(-4.84075823631812,57.495,5.21511826561693));
#38475=CARTESIAN_POINT('Ctrl Pts',(-4.86276047837854,57.495,5.22058260535447));
#38476=CARTESIAN_POINT('Ctrl Pts',(-4.87380761862879,57.495,5.22328778611671));
#38477=CARTESIAN_POINT('',(-3.34686616149372,57.495,4.18409499139877));
#38478=CARTESIAN_POINT('',(-3.25316890053365,57.495,4.06695907338649));
#38479=CARTESIAN_POINT('',(-2.58480949428933,57.495,4.69328497730872));
#38480=CARTESIAN_POINT('Origin',(0.,57.495,0.));
#38481=CARTESIAN_POINT('',(-2.87862685522557,57.495,5.22677443144495));
#38482=CARTESIAN_POINT('',(-2.87862685522557,57.495,5.22677443144495));
#38483=CARTESIAN_POINT('',(-2.96056324982543,57.495,6.50167680247051));
#38484=CARTESIAN_POINT('Ctrl Pts',(-2.87862685522557,57.495,5.22677443144495));
#38485=CARTESIAN_POINT('Ctrl Pts',(-2.88043681055505,57.495,5.23024117954545));
#38486=CARTESIAN_POINT('Ctrl Pts',(-2.884065589809,57.495,5.23745215939571));
#38487=CARTESIAN_POINT('Ctrl Pts',(-2.88953536864313,57.495,5.24910109063628));
#38488=CARTESIAN_POINT('Ctrl Pts',(-2.89688168736508,57.495,5.26630084561719));
#38489=CARTESIAN_POINT('Ctrl Pts',(-2.90614521320837,57.495,5.29057828960676));
#38490=CARTESIAN_POINT('Ctrl Pts',(-2.91546314862891,57.495,5.31759510370885));
#38491=CARTESIAN_POINT('Ctrl Pts',(-2.92478335875774,57.495,5.34725389048201));
#38492=CARTESIAN_POINT('Ctrl Pts',(-2.93401523982671,57.495,5.37936310952307));
#38493=CARTESIAN_POINT('Ctrl Pts',(-2.94303247002258,57.495,5.41364129622045));
#38494=CARTESIAN_POINT('Ctrl Pts',(-2.95169462080131,57.495,5.44977003302482));
#38495=CARTESIAN_POINT('Ctrl Pts',(-2.9598647928985,57.495,5.48743586913296));
#38496=CARTESIAN_POINT('Ctrl Pts',(-2.96742703426683,57.495,5.52637191504895));
#38497=CARTESIAN_POINT('Ctrl Pts',(-2.97430877025609,57.495,5.56641026634749));
#38498=CARTESIAN_POINT('Ctrl Pts',(-2.98047914221,57.495,5.6074788286105));
#38499=CARTESIAN_POINT('Ctrl Pts',(-2.98593308820271,57.495,5.64956501668959));
#38500=CARTESIAN_POINT('Ctrl Pts',(-2.9906797244254,57.495,5.69268882427748));
#38501=CARTESIAN_POINT('Ctrl Pts',(-2.9947301570106,57.495,5.73687442119613));
#38502=CARTESIAN_POINT('Ctrl Pts',(-2.99808342690946,57.495,5.78211642456387));
#38503=CARTESIAN_POINT('Ctrl Pts',(-3.00072490941932,57.495,5.82837721216385));
#38504=CARTESIAN_POINT('Ctrl Pts',(-3.00263159433912,57.495,5.87560110342631));
#38505=CARTESIAN_POINT('Ctrl Pts',(-3.00377540211877,57.495,5.9237232280624));
#38506=CARTESIAN_POINT('Ctrl Pts',(-3.00412716938109,57.495,5.97267956506952));
#38507=CARTESIAN_POINT('Ctrl Pts',(-3.00366113621883,57.495,6.02241806591666));
#38508=CARTESIAN_POINT('Ctrl Pts',(-3.00235671375967,57.495,6.07290162599622));
#38509=CARTESIAN_POINT('Ctrl Pts',(-3.00019778316108,57.495,6.12410381716742));
#38510=CARTESIAN_POINT('Ctrl Pts',(-2.99717295692919,57.495,6.17600655789209));
#38511=CARTESIAN_POINT('Ctrl Pts',(-2.99327554868811,57.495,6.22859706400147));
#38512=CARTESIAN_POINT('Ctrl Pts',(-2.98850417352769,57.495,6.28186459845047));
#38513=CARTESIAN_POINT('Ctrl Pts',(-2.98286238364857,57.495,6.33579850967689));
#38514=CARTESIAN_POINT('Ctrl Pts',(-2.97635619664337,57.495,6.39038953466561));
#38515=CARTESIAN_POINT('Ctrl Pts',(-2.97046502832945,57.495,6.43458214159149));
#38516=CARTESIAN_POINT('Ctrl Pts',(-2.96566304810549,57.495,6.46801681444607));
#38517=CARTESIAN_POINT('Ctrl Pts',(-2.96229154623625,57.495,6.49043534784131));
#38518=CARTESIAN_POINT('Ctrl Pts',(-2.96056324982543,57.495,6.50167680247051));
#38519=CARTESIAN_POINT('',(-2.50394540602692,57.495,6.69081410619341));
#38520=CARTESIAN_POINT('Origin',(-6.22890783902202E-13,57.495,1.50487931058895E-12));
#38521=CARTESIAN_POINT('',(-1.66039107437148,57.495,5.73138421404289));
#38522=CARTESIAN_POINT('Ctrl Pts',(-1.66039107437148,57.495,5.73138421404289));
#38523=CARTESIAN_POINT('Ctrl Pts',(-1.66156260377487,57.495,5.73511540682056));
#38524=CARTESIAN_POINT('Ctrl Pts',(-1.66409560210805,57.495,5.7427802739896));
#38525=CARTESIAN_POINT('Ctrl Pts',(-1.6684649226766,57.495,5.75488502996861));
#38526=CARTESIAN_POINT('Ctrl Pts',(-1.67543235427329,57.495,5.77224172513541));
#38527=CARTESIAN_POINT('Ctrl Pts',(-1.68604879760674,57.495,5.79595877235177));
#38528=CARTESIAN_POINT('Ctrl Pts',(-1.69856379474191,57.495,5.82165132013192));
#38529=CARTESIAN_POINT('Ctrl Pts',(-1.71294534020683,57.495,5.84921363316513));
#38530=CARTESIAN_POINT('Ctrl Pts',(-1.7291220610224,57.495,5.87844620539462));
#38531=CARTESIAN_POINT('Ctrl Pts',(-1.74698425466387,57.495,5.90906068827411));
#38532=CARTESIAN_POINT('Ctrl Pts',(-1.76640606389864,57.495,5.94073262861949));
#38533=CARTESIAN_POINT('Ctrl Pts',(-1.78726264793636,57.495,5.97314358084403));
#38534=CARTESIAN_POINT('Ctrl Pts',(-1.80944727788364,57.495,6.0060228350964));
#38535=CARTESIAN_POINT('Ctrl Pts',(-1.83289254541003,57.495,6.03920034699149));
#38536=CARTESIAN_POINT('Ctrl Pts',(-1.85756929242873,57.495,6.07260331771232));
#38537=CARTESIAN_POINT('Ctrl Pts',(-1.88347219921808,57.495,6.10621926889299));
#38538=CARTESIAN_POINT('Ctrl Pts',(-1.91060895733317,57.495,6.14006878432982));
#38539=CARTESIAN_POINT('Ctrl Pts',(-1.93898880419737,57.495,6.17417680788945));
#38540=CARTESIAN_POINT('Ctrl Pts',(-1.96860861168851,57.495,6.20853885514981));
#38541=CARTESIAN_POINT('Ctrl Pts',(-1.99945211810837,57.495,6.24311798195985));
#38542=CARTESIAN_POINT('Ctrl Pts',(-2.03149622201768,57.495,6.27785854554194));
#38543=CARTESIAN_POINT('Ctrl Pts',(-2.06471490843563,57.495,6.31269482043467));
#38544=CARTESIAN_POINT('Ctrl Pts',(-2.09908352929888,57.495,6.34756091533115));
#38545=CARTESIAN_POINT('Ctrl Pts',(-2.13458349574329,57.495,6.38240181135703));
#38546=CARTESIAN_POINT('Ctrl Pts',(-2.17120312938042,57.495,6.41717671306138));
#38547=CARTESIAN_POINT('Ctrl Pts',(-2.20893514043555,57.495,6.45185553518375));
#38548=CARTESIAN_POINT('Ctrl Pts',(-2.24777479550457,57.495,6.48641743997175));
#38549=CARTESIAN_POINT('Ctrl Pts',(-2.2877177827968,57.495,6.52084865967127));
#38550=CARTESIAN_POINT('Ctrl Pts',(-2.32875748935421,57.495,6.55514062276556));
#38551=CARTESIAN_POINT('Ctrl Pts',(-2.37088387159981,57.495,6.58928830924802));
#38552=CARTESIAN_POINT('Ctrl Pts',(-2.41408612451229,57.495,6.6232894242584));
#38553=CARTESIAN_POINT('Ctrl Pts',(-2.4495007016118,57.495,6.65037263123018));
#38554=CARTESIAN_POINT('Ctrl Pts',(-2.47653809829358,57.495,6.67061900235304));
#38555=CARTESIAN_POINT('Ctrl Pts',(-2.49477440711619,57.495,6.68408728750664));
#38556=CARTESIAN_POINT('Ctrl Pts',(-2.50394540602692,57.495,6.69081410619341));
#38557=CARTESIAN_POINT('',(-1.4909173120086,57.495,5.1463899549833));
#38558=CARTESIAN_POINT('',(-1.4491783055134,57.495,5.00231408838243));
#38559=CARTESIAN_POINT('',(-0.592010183030743,57.495,5.32519370006274));
#38560=CARTESIAN_POINT('Origin',(0.,57.495,0.));
#38561=CARTESIAN_POINT('',(-0.659304453656787,57.495,5.93051272372135));
#38562=CARTESIAN_POINT('',(-0.659304453656787,57.495,5.93051272372135));
#38563=CARTESIAN_POINT('',(-0.247119796320916,57.495,7.13972463098307));
#38564=CARTESIAN_POINT('Ctrl Pts',(-0.659304453656787,57.495,5.93051272372135));
#38565=CARTESIAN_POINT('Ctrl Pts',(-0.65964996727821,57.495,5.93440822125369));
#38566=CARTESIAN_POINT('Ctrl Pts',(-0.660242999639131,57.495,5.94245897164689));
#38567=CARTESIAN_POINT('Ctrl Pts',(-0.660838563360812,57.495,5.95531437453421));
#38568=CARTESIAN_POINT('Ctrl Pts',(-0.661043615595395,57.495,5.97401619058905));
#38569=CARTESIAN_POINT('Ctrl Pts',(-0.660311421925919,57.495,5.99999062205821));
#38570=CARTESIAN_POINT('Ctrl Pts',(-0.658581184594065,57.495,6.02851672315009));
#38571=CARTESIAN_POINT('Ctrl Pts',(-0.655842009648655,57.495,6.05948455921138));
#38572=CARTESIAN_POINT('Ctrl Pts',(-0.652083489461663,57.495,6.092682497423));
#38573=CARTESIAN_POINT('Ctrl Pts',(-0.647296629738964,57.495,6.12780215712609));
#38574=CARTESIAN_POINT('Ctrl Pts',(-0.641473544543643,57.495,6.16449561918681));
#38575=CARTESIAN_POINT('Ctrl Pts',(-0.63460770787657,57.495,6.2024209037432));
#38576=CARTESIAN_POINT('Ctrl Pts',(-0.626694128202828,57.495,6.24128706412512));
#38577=CARTESIAN_POINT('Ctrl Pts',(-0.617730009530283,57.495,6.28091120375433));
#38578=CARTESIAN_POINT('Ctrl Pts',(-0.607714431517378,57.495,6.32121490697708));
#38579=CARTESIAN_POINT('Ctrl Pts',(-0.596647533682196,57.495,6.36218460951721));
#38580=CARTESIAN_POINT('Ctrl Pts',(-0.584530087032233,57.495,6.40384227175349));
#38581=CARTESIAN_POINT('Ctrl Pts',(-0.571363102905585,57.495,6.4462144738227));
#38582=CARTESIAN_POINT('Ctrl Pts',(-0.557147755196287,57.495,6.48929587557851));
#38583=CARTESIAN_POINT('Ctrl Pts',(-0.541884929839958,57.495,6.53304612199338));
#38584=CARTESIAN_POINT('Ctrl Pts',(-0.52557467621436,57.495,6.57740496530586));
#38585=CARTESIAN_POINT('Ctrl Pts',(-0.508215876982667,57.495,6.62230172760518));
#38586=CARTESIAN_POINT('Ctrl Pts',(-0.48980608847462,57.495,6.66766610085612));
#38587=CARTESIAN_POINT('Ctrl Pts',(-0.470341429749656,57.495,6.71344014059646));
#38588=CARTESIAN_POINT('Ctrl Pts',(-0.449817078488635,57.495,6.75958168761835));
#38589=CARTESIAN_POINT('Ctrl Pts',(-0.428228256434482,57.495,6.80606015708944));
#38590=CARTESIAN_POINT('Ctrl Pts',(-0.405571362419762,57.495,6.85285448604147));
#38591=CARTESIAN_POINT('Ctrl Pts',(-0.381845111328231,57.495,6.89995030467732));
#38592=CARTESIAN_POINT('Ctrl Pts',(-0.357052332559017,57.495,6.94733716327859));
#38593=CARTESIAN_POINT('Ctrl Pts',(-0.331200384093975,57.495,6.99500658045334));
#38594=CARTESIAN_POINT('Ctrl Pts',(-0.304298370266163,57.495,7.04295230112448));
#38595=CARTESIAN_POINT('Ctrl Pts',(-0.281943861934804,57.495,7.0815264936406));
#38596=CARTESIAN_POINT('Ctrl Pts',(-0.264712515322364,57.495,7.1105784652929));
#38597=CARTESIAN_POINT('Ctrl Pts',(-0.253018452443266,57.495,7.13000027153814));
#38598=CARTESIAN_POINT('Ctrl Pts',(-0.247119796320916,57.495,7.13972463098307));
#38599=CARTESIAN_POINT('',(0.24711979632092,57.495,7.13972463098307));
#38600=CARTESIAN_POINT('Origin',(4.16333634234434E-16,57.495,1.6286971771251E-12));
#38601=CARTESIAN_POINT('',(0.659304453656788,57.495,5.93051272372135));
#38602=CARTESIAN_POINT('Ctrl Pts',(0.659304453656788,57.495,5.93051272372135));
#38603=CARTESIAN_POINT('Ctrl Pts',(0.659649967278236,57.495,5.9344082212537));
#38604=CARTESIAN_POINT('Ctrl Pts',(0.660242999639201,57.495,5.94245897164691));
#38605=CARTESIAN_POINT('Ctrl Pts',(0.660838563360921,57.495,5.95531437453424));
#38606=CARTESIAN_POINT('Ctrl Pts',(0.661043615595512,57.495,5.97401619058907));
#38607=CARTESIAN_POINT('Ctrl Pts',(0.660311421925997,57.495,5.99999062205823));
#38608=CARTESIAN_POINT('Ctrl Pts',(0.658581184594088,57.495,6.0285167231501));
#38609=CARTESIAN_POINT('Ctrl Pts',(0.655842009648633,57.495,6.05948455921138));
#38610=CARTESIAN_POINT('Ctrl Pts',(0.652083489461619,57.495,6.09268249742298));
#38611=CARTESIAN_POINT('Ctrl Pts',(0.64729662973892,57.495,6.12780215712604));
#38612=CARTESIAN_POINT('Ctrl Pts',(0.641473544543614,57.495,6.16449561918676));
#38613=CARTESIAN_POINT('Ctrl Pts',(0.634607707876564,57.495,6.20242090374318));
#38614=CARTESIAN_POINT('Ctrl Pts',(0.626694128202842,57.495,6.24128706412515));
#38615=CARTESIAN_POINT('Ctrl Pts',(0.617730009530307,57.495,6.2809112037544));
#38616=CARTESIAN_POINT('Ctrl Pts',(0.607714431517401,57.495,6.32121490697716));
#38617=CARTESIAN_POINT('Ctrl Pts',(0.596647533682211,57.495,6.36218460951727));
#38618=CARTESIAN_POINT('Ctrl Pts',(0.584530087032237,57.495,6.40384227175352));
#38619=CARTESIAN_POINT('Ctrl Pts',(0.571363102905579,57.495,6.44621447382266));
#38620=CARTESIAN_POINT('Ctrl Pts',(0.557147755196277,57.495,6.4892958755784));
#38621=CARTESIAN_POINT('Ctrl Pts',(0.541884929839949,57.495,6.53304612199323));
#38622=CARTESIAN_POINT('Ctrl Pts',(0.525574676214356,57.495,6.57740496530571));
#38623=CARTESIAN_POINT('Ctrl Pts',(0.508215876982668,57.495,6.62230172760513));
#38624=CARTESIAN_POINT('Ctrl Pts',(0.489806088474622,57.495,6.66766610085618));
#38625=CARTESIAN_POINT('Ctrl Pts',(0.470341429749655,57.495,6.71344014059664));
#38626=CARTESIAN_POINT('Ctrl Pts',(0.449817078488629,57.495,6.75958168761858));
#38627=CARTESIAN_POINT('Ctrl Pts',(0.428228256434473,57.495,6.80606015708966));
#38628=CARTESIAN_POINT('Ctrl Pts',(0.405571362419756,57.495,6.85285448604159));
#38629=CARTESIAN_POINT('Ctrl Pts',(0.381845111328234,57.495,6.89995030467727));
#38630=CARTESIAN_POINT('Ctrl Pts',(0.357052332559035,57.495,6.94733716327837));
#38631=CARTESIAN_POINT('Ctrl Pts',(0.331200384094009,57.495,6.99500658045299));
#38632=CARTESIAN_POINT('Ctrl Pts',(0.304298370266204,57.495,7.0429523011241));
#38633=CARTESIAN_POINT('Ctrl Pts',(0.28194386193484,57.495,7.0815264936403));
#38634=CARTESIAN_POINT('Ctrl Pts',(0.264712515322387,57.495,7.11057846529273));
#38635=CARTESIAN_POINT('Ctrl Pts',(0.253018452443275,57.495,7.13000027153808));
#38636=CARTESIAN_POINT('Ctrl Pts',(0.247119796320917,57.495,7.13972463098307));
#38637=CARTESIAN_POINT('',(0.592010183030744,57.495,5.32519370006274));
#38638=CARTESIAN_POINT('',(0.575436549687218,57.495,5.17611212951227));
#38639=CARTESIAN_POINT('Origin',(0.,57.495,0.));
#38640=CARTESIAN_POINT('',(-4.477,57.495,-5.4827437197827E-16));
#38641=CARTESIAN_POINT('Origin',(0.,57.495,0.));
#38642=CARTESIAN_POINT('Origin',(0.,54.32,0.));
#38643=CARTESIAN_POINT('',(3.34686616149372,51.145,4.18409499139877));
#38644=CARTESIAN_POINT('Origin',(0.,51.145,0.));
#38645=CARTESIAN_POINT('',(3.34686616149372,54.32,4.18409499139877));
#38646=CARTESIAN_POINT('Origin',(3.72730711280926,57.495,4.65970441290367));
#38647=CARTESIAN_POINT('',(3.72730711280926,51.145,4.65970441290367));
#38648=CARTESIAN_POINT('',(3.72730711280926,51.145,4.65970441290367));
#38649=CARTESIAN_POINT('',(3.72730711280926,57.495,4.65970441290367));
#38650=CARTESIAN_POINT('Origin',(1.15195721078055E-12,57.495,1.15136842610855E-12));
#38651=CARTESIAN_POINT('',(4.87380761862879,51.145,5.22328778611671));
#38652=CARTESIAN_POINT('',(4.87380761862879,57.495,5.22328778611671));
#38653=CARTESIAN_POINT('',(5.22328778611671,51.145,4.87380761862879));
#38654=CARTESIAN_POINT('Origin',(1.15195721078055E-12,51.145,1.15136842610855E-12));
#38655=CARTESIAN_POINT('',(5.22328778611671,57.495,4.87380761862879));
#38656=CARTESIAN_POINT('Ctrl Pts',(4.65970441290368,57.495,3.72730711280926));
#38657=CARTESIAN_POINT('Ctrl Pts',(4.65970441290368,49.875,3.72730711280926));
#38658=CARTESIAN_POINT('Ctrl Pts',(4.66270326064961,57.495,3.72981733050576));
#38659=CARTESIAN_POINT('Ctrl Pts',(4.66270326064961,49.875,3.72981733050576));
#38660=CARTESIAN_POINT('Ctrl Pts',(4.6688153380502,57.495,3.73509073349854));
#38661=CARTESIAN_POINT('Ctrl Pts',(4.6688153380502,49.875,3.73509073349854));
#38662=CARTESIAN_POINT('Ctrl Pts',(4.67832660775297,57.495,3.7437597489088));
#38663=CARTESIAN_POINT('Ctrl Pts',(4.67832660775297,49.875,3.7437597489088));
#38664=CARTESIAN_POINT('Ctrl Pts',(4.69169578253142,57.495,3.7568389360361));
#38665=CARTESIAN_POINT('Ctrl Pts',(4.69169578253142,49.875,3.7568389360361));
#38666=CARTESIAN_POINT('Ctrl Pts',(4.70954474005187,57.495,3.77572337177426));
#38667=CARTESIAN_POINT('Ctrl Pts',(4.70954474005187,49.875,3.77572337177426));
#38668=CARTESIAN_POINT('Ctrl Pts',(4.72849227702429,57.495,3.79711783384759));
#38669=CARTESIAN_POINT('Ctrl Pts',(4.72849227702429,49.875,3.79711783384759));
#38670=CARTESIAN_POINT('Ctrl Pts',(4.74845295472311,57.495,3.82095228990398));
#38671=CARTESIAN_POINT('Ctrl Pts',(4.74845295472311,49.875,3.82095228990398));
#38672=CARTESIAN_POINT('Ctrl Pts',(4.76926976684248,57.495,3.84708445224628));
#38673=CARTESIAN_POINT('Ctrl Pts',(4.76926976684248,49.875,3.84708445224628));
#38674=CARTESIAN_POINT('Ctrl Pts',(4.79071829540097,57.495,3.87530262274579));
#38675=CARTESIAN_POINT('Ctrl Pts',(4.79071829540097,49.875,3.87530262274579));
#38676=CARTESIAN_POINT('Ctrl Pts',(4.81254694822028,57.495,3.90536636162316));
#38677=CARTESIAN_POINT('Ctrl Pts',(4.81254694822028,49.875,3.90536636162316));
#38678=CARTESIAN_POINT('Ctrl Pts',(4.83450929444277,57.495,3.93703846717723));
#38679=CARTESIAN_POINT('Ctrl Pts',(4.83450929444277,49.875,3.93703846717723));
#38680=CARTESIAN_POINT('Ctrl Pts',(4.85639607415679,57.495,3.97011673859275));
#38681=CARTESIAN_POINT('Ctrl Pts',(4.85639607415679,49.875,3.97011673859275));
#38682=CARTESIAN_POINT('Ctrl Pts',(4.87807598288661,57.495,4.00447382552398));
#38683=CARTESIAN_POINT('Ctrl Pts',(4.87807598288661,49.875,4.00447382552398));
#38684=CARTESIAN_POINT('Ctrl Pts',(4.89949292161193,57.495,4.04005493051016));
#38685=CARTESIAN_POINT('Ctrl Pts',(4.89949292161193,49.875,4.04005493051016));
#38686=CARTESIAN_POINT('Ctrl Pts',(4.92063739759527,57.495,4.07685036350543));
#38687=CARTESIAN_POINT('Ctrl Pts',(4.92063739759527,49.875,4.07685036350543));
#38688=CARTESIAN_POINT('Ctrl Pts',(4.94152548435404,57.495,4.11487510765792));
#38689=CARTESIAN_POINT('Ctrl Pts',(4.94152548435404,49.875,4.11487510765792));
#38690=CARTESIAN_POINT('Ctrl Pts',(4.9621766920072,57.495,4.15414724283855));
#38691=CARTESIAN_POINT('Ctrl Pts',(4.9621766920072,49.875,4.15414724283855));
#38692=CARTESIAN_POINT('Ctrl Pts',(4.98258807456953,57.495,4.19466216292523));
#38693=CARTESIAN_POINT('Ctrl Pts',(4.98258807456953,49.875,4.19466216292523));
#38694=CARTESIAN_POINT('Ctrl Pts',(5.00273172317852,57.495,4.23639070615327));
#38695=CARTESIAN_POINT('Ctrl Pts',(5.00273172317852,49.875,4.23639070615327));
#38696=CARTESIAN_POINT('Ctrl Pts',(5.02256507114883,57.495,4.27929023600664));
#38697=CARTESIAN_POINT('Ctrl Pts',(5.02256507114883,49.875,4.27929023600664));
#38698=CARTESIAN_POINT('Ctrl Pts',(5.04203735157409,57.495,4.32331156573186));
#38699=CARTESIAN_POINT('Ctrl Pts',(5.04203735157409,49.875,4.32331156573186));
#38700=CARTESIAN_POINT('Ctrl Pts',(5.06109712122993,57.495,4.36840670797621));
#38701=CARTESIAN_POINT('Ctrl Pts',(5.06109712122993,49.875,4.36840670797621));
#38702=CARTESIAN_POINT('Ctrl Pts',(5.07970066295481,57.495,4.41453743405689));
#38703=CARTESIAN_POINT('Ctrl Pts',(5.07970066295481,49.875,4.41453743405689));
#38704=CARTESIAN_POINT('Ctrl Pts',(5.09781475579234,57.495,4.46167734280668));
#38705=CARTESIAN_POINT('Ctrl Pts',(5.09781475579234,49.875,4.46167734280668));
#38706=CARTESIAN_POINT('Ctrl Pts',(5.11541439426219,57.495,4.50980818622117));
#38707=CARTESIAN_POINT('Ctrl Pts',(5.11541439426219,49.875,4.50980818622117));
#38708=CARTESIAN_POINT('Ctrl Pts',(5.13248213818673,57.495,4.55891761694258));
#38709=CARTESIAN_POINT('Ctrl Pts',(5.13248213818673,49.875,4.55891761694258));
#38710=CARTESIAN_POINT('Ctrl Pts',(5.14900691787061,57.495,4.60899638270436));
#38711=CARTESIAN_POINT('Ctrl Pts',(5.14900691787061,49.875,4.60899638270436));
#38712=CARTESIAN_POINT('Ctrl Pts',(5.16498334493441,57.495,4.66003509375248));
#38713=CARTESIAN_POINT('Ctrl Pts',(5.16498334493441,49.875,4.66003509375248));
#38714=CARTESIAN_POINT('Ctrl Pts',(5.1804106250073,57.495,4.71202254995837));
#38715=CARTESIAN_POINT('Ctrl Pts',(5.1804106250073,49.875,4.71202254995837));
#38716=CARTESIAN_POINT('Ctrl Pts',(5.1952907728175,57.495,4.764947890579));
#38717=CARTESIAN_POINT('Ctrl Pts',(5.1952907728175,49.875,4.764947890579));
#38718=CARTESIAN_POINT('Ctrl Pts',(5.2067598214933,57.495,4.8080309881172));
#38719=CARTESIAN_POINT('Ctrl Pts',(5.2067598214933,49.875,4.8080309881172));
#38720=CARTESIAN_POINT('Ctrl Pts',(5.21511826561693,57.495,4.84075823631811));
#38721=CARTESIAN_POINT('Ctrl Pts',(5.21511826561693,49.875,4.84075823631811));
#38722=CARTESIAN_POINT('Ctrl Pts',(5.22058260535447,57.495,4.86276047837853));
#38723=CARTESIAN_POINT('Ctrl Pts',(5.22058260535447,49.875,4.86276047837853));
#38724=CARTESIAN_POINT('Ctrl Pts',(5.22328778611671,57.495,4.87380761862879));
#38725=CARTESIAN_POINT('Ctrl Pts',(5.22328778611671,49.875,4.87380761862879));
#38726=CARTESIAN_POINT('',(4.65970441290368,51.145,3.72730711280926));
#38727=CARTESIAN_POINT('Ctrl Pts',(4.65970441290368,51.145,3.72730711280926));
#38728=CARTESIAN_POINT('Ctrl Pts',(4.66270326064961,51.145,3.72981733050576));
#38729=CARTESIAN_POINT('Ctrl Pts',(4.6688153380502,51.145,3.73509073349854));
#38730=CARTESIAN_POINT('Ctrl Pts',(4.67832660775297,51.145,3.7437597489088));
#38731=CARTESIAN_POINT('Ctrl Pts',(4.69169578253142,51.145,3.7568389360361));
#38732=CARTESIAN_POINT('Ctrl Pts',(4.70954474005187,51.145,3.77572337177426));
#38733=CARTESIAN_POINT('Ctrl Pts',(4.72849227702429,51.145,3.79711783384759));
#38734=CARTESIAN_POINT('Ctrl Pts',(4.74845295472311,51.145,3.82095228990398));
#38735=CARTESIAN_POINT('Ctrl Pts',(4.76926976684248,51.145,3.84708445224628));
#38736=CARTESIAN_POINT('Ctrl Pts',(4.79071829540097,51.145,3.87530262274579));
#38737=CARTESIAN_POINT('Ctrl Pts',(4.81254694822028,51.145,3.90536636162316));
#38738=CARTESIAN_POINT('Ctrl Pts',(4.83450929444277,51.145,3.93703846717723));
#38739=CARTESIAN_POINT('Ctrl Pts',(4.85639607415679,51.145,3.97011673859275));
#38740=CARTESIAN_POINT('Ctrl Pts',(4.87807598288661,51.145,4.00447382552398));
#38741=CARTESIAN_POINT('Ctrl Pts',(4.89949292161193,51.145,4.04005493051016));
#38742=CARTESIAN_POINT('Ctrl Pts',(4.92063739759527,51.145,4.07685036350543));
#38743=CARTESIAN_POINT('Ctrl Pts',(4.94152548435404,51.145,4.11487510765792));
#38744=CARTESIAN_POINT('Ctrl Pts',(4.9621766920072,51.145,4.15414724283855));
#38745=CARTESIAN_POINT('Ctrl Pts',(4.98258807456953,51.145,4.19466216292523));
#38746=CARTESIAN_POINT('Ctrl Pts',(5.00273172317852,51.145,4.23639070615327));
#38747=CARTESIAN_POINT('Ctrl Pts',(5.02256507114883,51.145,4.27929023600664));
#38748=CARTESIAN_POINT('Ctrl Pts',(5.04203735157409,51.145,4.32331156573186));
#38749=CARTESIAN_POINT('Ctrl Pts',(5.06109712122993,51.145,4.36840670797621));
#38750=CARTESIAN_POINT('Ctrl Pts',(5.07970066295481,51.145,4.41453743405689));
#38751=CARTESIAN_POINT('Ctrl Pts',(5.09781475579234,51.145,4.46167734280668));
#38752=CARTESIAN_POINT('Ctrl Pts',(5.11541439426219,51.145,4.50980818622117));
#38753=CARTESIAN_POINT('Ctrl Pts',(5.13248213818673,51.145,4.55891761694258));
#38754=CARTESIAN_POINT('Ctrl Pts',(5.14900691787061,51.145,4.60899638270436));
#38755=CARTESIAN_POINT('Ctrl Pts',(5.16498334493441,51.145,4.66003509375248));
#38756=CARTESIAN_POINT('Ctrl Pts',(5.1804106250073,51.145,4.71202254995837));
#38757=CARTESIAN_POINT('Ctrl Pts',(5.1952907728175,51.145,4.764947890579));
#38758=CARTESIAN_POINT('Ctrl Pts',(5.2067598214933,51.145,4.8080309881172));
#38759=CARTESIAN_POINT('Ctrl Pts',(5.21511826561693,51.145,4.84075823631811));
#38760=CARTESIAN_POINT('Ctrl Pts',(5.22058260535447,51.145,4.86276047837853));
#38761=CARTESIAN_POINT('Ctrl Pts',(5.22328778611671,51.145,4.87380761862879));
#38762=CARTESIAN_POINT('',(4.65970441290368,57.495,3.72730711280926));
#38763=CARTESIAN_POINT('Origin',(4.06695907338649,57.495,3.25316890053365));
#38764=CARTESIAN_POINT('',(4.18409499139877,51.145,3.34686616149372));
#38765=CARTESIAN_POINT('',(4.18409499139877,54.32,3.34686616149372));
#38766=CARTESIAN_POINT('',(4.06695907338649,51.145,3.25316890053365));
#38767=CARTESIAN_POINT('Ctrl Pts',(4.87380761862879,57.495,5.22328778611671));
#38768=CARTESIAN_POINT('Ctrl Pts',(4.87380761862879,49.875,5.22328778611671));
#38769=CARTESIAN_POINT('Ctrl Pts',(4.86276047837859,57.495,5.2205826053545));
#38770=CARTESIAN_POINT('Ctrl Pts',(4.86276047837859,49.875,5.2205826053545));
#38771=CARTESIAN_POINT('Ctrl Pts',(4.84075823631826,57.495,5.21511826561704));
#38772=CARTESIAN_POINT('Ctrl Pts',(4.84075823631826,49.875,5.21511826561704));
#38773=CARTESIAN_POINT('Ctrl Pts',(4.80803098811744,57.495,5.20675982149348));
#38774=CARTESIAN_POINT('Ctrl Pts',(4.80803098811744,49.875,5.20675982149348));
#38775=CARTESIAN_POINT('Ctrl Pts',(4.7649478905793,57.495,5.19529077281773));
#38776=CARTESIAN_POINT('Ctrl Pts',(4.7649478905793,49.875,5.19529077281773));
#38777=CARTESIAN_POINT('Ctrl Pts',(4.71202254995864,57.495,5.18041062500752));
#38778=CARTESIAN_POINT('Ctrl Pts',(4.71202254995864,49.875,5.18041062500752));
#38779=CARTESIAN_POINT('Ctrl Pts',(4.66003509375265,57.495,5.16498334493456));
#38780=CARTESIAN_POINT('Ctrl Pts',(4.66003509375265,49.875,5.16498334493456));
#38781=CARTESIAN_POINT('Ctrl Pts',(4.60899638270439,57.495,5.14900691787064));
#38782=CARTESIAN_POINT('Ctrl Pts',(4.60899638270439,49.875,5.14900691787064));
#38783=CARTESIAN_POINT('Ctrl Pts',(4.5589176169425,57.495,5.13248213818666));
#38784=CARTESIAN_POINT('Ctrl Pts',(4.5589176169425,49.875,5.13248213818666));
#38785=CARTESIAN_POINT('Ctrl Pts',(4.50980818622101,57.495,5.11541439426204));
#38786=CARTESIAN_POINT('Ctrl Pts',(4.50980818622101,49.875,5.11541439426204));
#38787=CARTESIAN_POINT('Ctrl Pts',(4.46167734280651,57.495,5.09781475579217));
#38788=CARTESIAN_POINT('Ctrl Pts',(4.46167734280651,49.875,5.09781475579217));
#38789=CARTESIAN_POINT('Ctrl Pts',(4.41453743405677,57.495,5.07970066295468));
#38790=CARTESIAN_POINT('Ctrl Pts',(4.41453743405677,49.875,5.07970066295468));
#38791=CARTESIAN_POINT('Ctrl Pts',(4.36840670797617,57.495,5.06109712122989));
#38792=CARTESIAN_POINT('Ctrl Pts',(4.36840670797617,49.875,5.06109712122989));
#38793=CARTESIAN_POINT('Ctrl Pts',(4.3233115657319,57.495,5.04203735157412));
#38794=CARTESIAN_POINT('Ctrl Pts',(4.3233115657319,49.875,5.04203735157412));
#38795=CARTESIAN_POINT('Ctrl Pts',(4.27929023600674,57.495,5.02256507114894));
#38796=CARTESIAN_POINT('Ctrl Pts',(4.27929023600674,49.875,5.02256507114894));
#38797=CARTESIAN_POINT('Ctrl Pts',(4.23639070615337,57.495,5.00273172317863));
#38798=CARTESIAN_POINT('Ctrl Pts',(4.23639070615337,49.875,5.00273172317863));
#38799=CARTESIAN_POINT('Ctrl Pts',(4.1946621629253,57.495,4.98258807456961));
#38800=CARTESIAN_POINT('Ctrl Pts',(4.1946621629253,49.875,4.98258807456961));
#38801=CARTESIAN_POINT('Ctrl Pts',(4.15414724283858,57.495,4.96217669200723));
#38802=CARTESIAN_POINT('Ctrl Pts',(4.15414724283858,49.875,4.96217669200723));
#38803=CARTESIAN_POINT('Ctrl Pts',(4.11487510765791,57.495,4.94152548435402));
#38804=CARTESIAN_POINT('Ctrl Pts',(4.11487510765791,49.875,4.94152548435402));
#38805=CARTESIAN_POINT('Ctrl Pts',(4.07685036350539,57.495,4.92063739759521));
#38806=CARTESIAN_POINT('Ctrl Pts',(4.07685036350539,49.875,4.92063739759521));
#38807=CARTESIAN_POINT('Ctrl Pts',(4.04005493051012,57.495,4.89949292161185));
#38808=CARTESIAN_POINT('Ctrl Pts',(4.04005493051012,49.875,4.89949292161185));
#38809=CARTESIAN_POINT('Ctrl Pts',(4.00447382552396,57.495,4.87807598288654));
#38810=CARTESIAN_POINT('Ctrl Pts',(4.00447382552396,49.875,4.87807598288654));
#38811=CARTESIAN_POINT('Ctrl Pts',(3.97011673859274,57.495,4.85639607415676));
#38812=CARTESIAN_POINT('Ctrl Pts',(3.97011673859274,49.875,4.85639607415676));
#38813=CARTESIAN_POINT('Ctrl Pts',(3.93703846717724,57.495,4.83450929444279));
#38814=CARTESIAN_POINT('Ctrl Pts',(3.93703846717724,49.875,4.83450929444279));
#38815=CARTESIAN_POINT('Ctrl Pts',(3.90536636162318,57.495,4.81254694822034));
#38816=CARTESIAN_POINT('Ctrl Pts',(3.90536636162318,49.875,4.81254694822034));
#38817=CARTESIAN_POINT('Ctrl Pts',(3.8753026227458,57.495,4.79071829540103));
#38818=CARTESIAN_POINT('Ctrl Pts',(3.8753026227458,49.875,4.79071829540103));
#38819=CARTESIAN_POINT('Ctrl Pts',(3.84708445224627,57.495,4.76926976684252));
#38820=CARTESIAN_POINT('Ctrl Pts',(3.84708445224627,49.875,4.76926976684252));
#38821=CARTESIAN_POINT('Ctrl Pts',(3.82095228990397,57.495,4.74845295472312));
#38822=CARTESIAN_POINT('Ctrl Pts',(3.82095228990397,49.875,4.74845295472312));
#38823=CARTESIAN_POINT('Ctrl Pts',(3.7971178338476,57.495,4.72849227702426));
#38824=CARTESIAN_POINT('Ctrl Pts',(3.7971178338476,49.875,4.72849227702426));
#38825=CARTESIAN_POINT('Ctrl Pts',(3.77572337177431,57.495,4.7095447400518));
#38826=CARTESIAN_POINT('Ctrl Pts',(3.77572337177431,49.875,4.7095447400518));
#38827=CARTESIAN_POINT('Ctrl Pts',(3.75683893603616,57.495,4.69169578253132));
#38828=CARTESIAN_POINT('Ctrl Pts',(3.75683893603616,49.875,4.69169578253132));
#38829=CARTESIAN_POINT('Ctrl Pts',(3.74375974890886,57.495,4.67832660775287));
#38830=CARTESIAN_POINT('Ctrl Pts',(3.74375974890886,49.875,4.67832660775287));
#38831=CARTESIAN_POINT('Ctrl Pts',(3.73509073349858,57.495,4.66881533805013));
#38832=CARTESIAN_POINT('Ctrl Pts',(3.73509073349858,49.875,4.66881533805013));
#38833=CARTESIAN_POINT('Ctrl Pts',(3.72981733050578,57.495,4.66270326064959));
#38834=CARTESIAN_POINT('Ctrl Pts',(3.72981733050578,49.875,4.66270326064959));
#38835=CARTESIAN_POINT('Ctrl Pts',(3.72730711280926,57.495,4.65970441290367));
#38836=CARTESIAN_POINT('Ctrl Pts',(3.72730711280926,49.875,4.65970441290367));
#38837=CARTESIAN_POINT('Ctrl Pts',(4.87380761862879,51.145,5.22328778611671));
#38838=CARTESIAN_POINT('Ctrl Pts',(4.86276047837859,51.145,5.2205826053545));
#38839=CARTESIAN_POINT('Ctrl Pts',(4.84075823631826,51.145,5.21511826561704));
#38840=CARTESIAN_POINT('Ctrl Pts',(4.80803098811744,51.145,5.20675982149348));
#38841=CARTESIAN_POINT('Ctrl Pts',(4.7649478905793,51.145,5.19529077281773));
#38842=CARTESIAN_POINT('Ctrl Pts',(4.71202254995864,51.145,5.18041062500752));
#38843=CARTESIAN_POINT('Ctrl Pts',(4.66003509375265,51.145,5.16498334493456));
#38844=CARTESIAN_POINT('Ctrl Pts',(4.60899638270439,51.145,5.14900691787064));
#38845=CARTESIAN_POINT('Ctrl Pts',(4.5589176169425,51.145,5.13248213818666));
#38846=CARTESIAN_POINT('Ctrl Pts',(4.50980818622101,51.145,5.11541439426204));
#38847=CARTESIAN_POINT('Ctrl Pts',(4.46167734280651,51.145,5.09781475579217));
#38848=CARTESIAN_POINT('Ctrl Pts',(4.41453743405677,51.145,5.07970066295468));
#38849=CARTESIAN_POINT('Ctrl Pts',(4.36840670797617,51.145,5.06109712122989));
#38850=CARTESIAN_POINT('Ctrl Pts',(4.3233115657319,51.145,5.04203735157412));
#38851=CARTESIAN_POINT('Ctrl Pts',(4.27929023600674,51.145,5.02256507114894));
#38852=CARTESIAN_POINT('Ctrl Pts',(4.23639070615337,51.145,5.00273172317863));
#38853=CARTESIAN_POINT('Ctrl Pts',(4.1946621629253,51.145,4.98258807456961));
#38854=CARTESIAN_POINT('Ctrl Pts',(4.15414724283858,51.145,4.96217669200723));
#38855=CARTESIAN_POINT('Ctrl Pts',(4.11487510765791,51.145,4.94152548435402));
#38856=CARTESIAN_POINT('Ctrl Pts',(4.07685036350539,51.145,4.92063739759521));
#38857=CARTESIAN_POINT('Ctrl Pts',(4.04005493051012,51.145,4.89949292161185));
#38858=CARTESIAN_POINT('Ctrl Pts',(4.00447382552396,51.145,4.87807598288654));
#38859=CARTESIAN_POINT('Ctrl Pts',(3.97011673859274,51.145,4.85639607415676));
#38860=CARTESIAN_POINT('Ctrl Pts',(3.93703846717724,51.145,4.83450929444279));
#38861=CARTESIAN_POINT('Ctrl Pts',(3.90536636162318,51.145,4.81254694822034));
#38862=CARTESIAN_POINT('Ctrl Pts',(3.8753026227458,51.145,4.79071829540103));
#38863=CARTESIAN_POINT('Ctrl Pts',(3.84708445224627,51.145,4.76926976684252));
#38864=CARTESIAN_POINT('Ctrl Pts',(3.82095228990397,51.145,4.74845295472312));
#38865=CARTESIAN_POINT('Ctrl Pts',(3.7971178338476,51.145,4.72849227702426));
#38866=CARTESIAN_POINT('Ctrl Pts',(3.77572337177431,51.145,4.7095447400518));
#38867=CARTESIAN_POINT('Ctrl Pts',(3.75683893603616,51.145,4.69169578253132));
#38868=CARTESIAN_POINT('Ctrl Pts',(3.74375974890886,51.145,4.67832660775287));
#38869=CARTESIAN_POINT('Ctrl Pts',(3.73509073349858,51.145,4.66881533805013));
#38870=CARTESIAN_POINT('Ctrl Pts',(3.72981733050578,51.145,4.66270326064959));
#38871=CARTESIAN_POINT('Ctrl Pts',(3.72730711280926,51.145,4.65970441290367));
#38872=CARTESIAN_POINT('Origin',(0.,54.32,0.));
#38873=CARTESIAN_POINT('',(4.69328497730872,51.145,2.58480949428933));
#38874=CARTESIAN_POINT('Origin',(0.,51.145,0.));
#38875=CARTESIAN_POINT('',(4.69328497730872,54.32,2.58480949428933));
#38876=CARTESIAN_POINT('Origin',(5.22677443144495,57.495,2.87862685522557));
#38877=CARTESIAN_POINT('',(5.22677443144495,51.145,2.87862685522557));
#38878=CARTESIAN_POINT('',(5.22677443144495,51.145,2.87862685522557));
#38879=CARTESIAN_POINT('',(5.22677443144495,57.495,2.87862685522557));
#38880=CARTESIAN_POINT('Origin',(1.50487931058895E-12,57.495,6.22890783902203E-13));
#38881=CARTESIAN_POINT('',(6.50167680247051,51.145,2.96056324982543));
#38882=CARTESIAN_POINT('',(6.50167680247051,57.495,2.96056324982543));
#38883=CARTESIAN_POINT('',(6.69081410619341,51.145,2.50394540602692));
#38884=CARTESIAN_POINT('Origin',(1.50487931058895E-12,51.145,6.22890783902203E-13));
#38885=CARTESIAN_POINT('',(6.69081410619341,57.495,2.50394540602692));
#38886=CARTESIAN_POINT('Ctrl Pts',(5.73138421404289,57.495,1.66039107437148));
#38887=CARTESIAN_POINT('Ctrl Pts',(5.73138421404289,49.875,1.66039107437148));
#38888=CARTESIAN_POINT('Ctrl Pts',(5.73511540682056,57.495,1.66156260377487));
#38889=CARTESIAN_POINT('Ctrl Pts',(5.73511540682056,49.875,1.66156260377487));
#38890=CARTESIAN_POINT('Ctrl Pts',(5.7427802739896,57.495,1.66409560210805));
#38891=CARTESIAN_POINT('Ctrl Pts',(5.7427802739896,49.875,1.66409560210805));
#38892=CARTESIAN_POINT('Ctrl Pts',(5.75488502996861,57.495,1.6684649226766));
#38893=CARTESIAN_POINT('Ctrl Pts',(5.75488502996861,49.875,1.6684649226766));
#38894=CARTESIAN_POINT('Ctrl Pts',(5.77224172513541,57.495,1.67543235427329));
#38895=CARTESIAN_POINT('Ctrl Pts',(5.77224172513541,49.875,1.67543235427329));
#38896=CARTESIAN_POINT('Ctrl Pts',(5.79595877235177,57.495,1.68604879760674));
#38897=CARTESIAN_POINT('Ctrl Pts',(5.79595877235177,49.875,1.68604879760674));
#38898=CARTESIAN_POINT('Ctrl Pts',(5.82165132013192,57.495,1.69856379474191));
#38899=CARTESIAN_POINT('Ctrl Pts',(5.82165132013192,49.875,1.69856379474191));
#38900=CARTESIAN_POINT('Ctrl Pts',(5.84921363316513,57.495,1.71294534020683));
#38901=CARTESIAN_POINT('Ctrl Pts',(5.84921363316513,49.875,1.71294534020683));
#38902=CARTESIAN_POINT('Ctrl Pts',(5.87844620539462,57.495,1.72912206102241));
#38903=CARTESIAN_POINT('Ctrl Pts',(5.87844620539462,49.875,1.72912206102241));
#38904=CARTESIAN_POINT('Ctrl Pts',(5.90906068827411,57.495,1.74698425466387));
#38905=CARTESIAN_POINT('Ctrl Pts',(5.90906068827411,49.875,1.74698425466387));
#38906=CARTESIAN_POINT('Ctrl Pts',(5.94073262861949,57.495,1.76640606389864));
#38907=CARTESIAN_POINT('Ctrl Pts',(5.94073262861949,49.875,1.76640606389864));
#38908=CARTESIAN_POINT('Ctrl Pts',(5.97314358084403,57.495,1.78726264793637));
#38909=CARTESIAN_POINT('Ctrl Pts',(5.97314358084403,49.875,1.78726264793637));
#38910=CARTESIAN_POINT('Ctrl Pts',(6.0060228350964,57.495,1.80944727788364));
#38911=CARTESIAN_POINT('Ctrl Pts',(6.0060228350964,49.875,1.80944727788364));
#38912=CARTESIAN_POINT('Ctrl Pts',(6.03920034699149,57.495,1.83289254541003));
#38913=CARTESIAN_POINT('Ctrl Pts',(6.03920034699149,49.875,1.83289254541003));
#38914=CARTESIAN_POINT('Ctrl Pts',(6.07260331771232,57.495,1.85756929242874));
#38915=CARTESIAN_POINT('Ctrl Pts',(6.07260331771232,49.875,1.85756929242874));
#38916=CARTESIAN_POINT('Ctrl Pts',(6.10621926889299,57.495,1.88347219921809));
#38917=CARTESIAN_POINT('Ctrl Pts',(6.10621926889299,49.875,1.88347219921809));
#38918=CARTESIAN_POINT('Ctrl Pts',(6.14006878432982,57.495,1.91060895733317));
#38919=CARTESIAN_POINT('Ctrl Pts',(6.14006878432982,49.875,1.91060895733317));
#38920=CARTESIAN_POINT('Ctrl Pts',(6.17417680788945,57.495,1.93898880419737));
#38921=CARTESIAN_POINT('Ctrl Pts',(6.17417680788945,49.875,1.93898880419737));
#38922=CARTESIAN_POINT('Ctrl Pts',(6.20853885514981,57.495,1.96860861168851));
#38923=CARTESIAN_POINT('Ctrl Pts',(6.20853885514981,49.875,1.96860861168851));
#38924=CARTESIAN_POINT('Ctrl Pts',(6.24311798195985,57.495,1.99945211810837));
#38925=CARTESIAN_POINT('Ctrl Pts',(6.24311798195985,49.875,1.99945211810837));
#38926=CARTESIAN_POINT('Ctrl Pts',(6.27785854554194,57.495,2.03149622201769));
#38927=CARTESIAN_POINT('Ctrl Pts',(6.27785854554194,49.875,2.03149622201769));
#38928=CARTESIAN_POINT('Ctrl Pts',(6.31269482043467,57.495,2.06471490843563));
#38929=CARTESIAN_POINT('Ctrl Pts',(6.31269482043467,49.875,2.06471490843563));
#38930=CARTESIAN_POINT('Ctrl Pts',(6.34756091533115,57.495,2.09908352929888));
#38931=CARTESIAN_POINT('Ctrl Pts',(6.34756091533115,49.875,2.09908352929888));
#38932=CARTESIAN_POINT('Ctrl Pts',(6.38240181135703,57.495,2.13458349574329));
#38933=CARTESIAN_POINT('Ctrl Pts',(6.38240181135703,49.875,2.13458349574329));
#38934=CARTESIAN_POINT('Ctrl Pts',(6.41717671306138,57.495,2.17120312938042));
#38935=CARTESIAN_POINT('Ctrl Pts',(6.41717671306138,49.875,2.17120312938042));
#38936=CARTESIAN_POINT('Ctrl Pts',(6.45185553518375,57.495,2.20893514043555));
#38937=CARTESIAN_POINT('Ctrl Pts',(6.45185553518375,49.875,2.20893514043555));
#38938=CARTESIAN_POINT('Ctrl Pts',(6.48641743997175,57.495,2.24777479550457));
#38939=CARTESIAN_POINT('Ctrl Pts',(6.48641743997175,49.875,2.24777479550457));
#38940=CARTESIAN_POINT('Ctrl Pts',(6.52084865967127,57.495,2.2877177827968));
#38941=CARTESIAN_POINT('Ctrl Pts',(6.52084865967127,49.875,2.2877177827968));
#38942=CARTESIAN_POINT('Ctrl Pts',(6.55514062276556,57.495,2.32875748935421));
#38943=CARTESIAN_POINT('Ctrl Pts',(6.55514062276556,49.875,2.32875748935421));
#38944=CARTESIAN_POINT('Ctrl Pts',(6.58928830924802,57.495,2.37088387159981));
#38945=CARTESIAN_POINT('Ctrl Pts',(6.58928830924802,49.875,2.37088387159981));
#38946=CARTESIAN_POINT('Ctrl Pts',(6.6232894242584,57.495,2.41408612451229));
#38947=CARTESIAN_POINT('Ctrl Pts',(6.6232894242584,49.875,2.41408612451229));
#38948=CARTESIAN_POINT('Ctrl Pts',(6.65037263123018,57.495,2.4495007016118));
#38949=CARTESIAN_POINT('Ctrl Pts',(6.65037263123018,49.875,2.4495007016118));
#38950=CARTESIAN_POINT('Ctrl Pts',(6.67061900235304,57.495,2.47653809829358));
#38951=CARTESIAN_POINT('Ctrl Pts',(6.67061900235304,49.875,2.47653809829358));
#38952=CARTESIAN_POINT('Ctrl Pts',(6.68408728750664,57.495,2.49477440711619));
#38953=CARTESIAN_POINT('Ctrl Pts',(6.68408728750664,49.875,2.49477440711619));
#38954=CARTESIAN_POINT('Ctrl Pts',(6.69081410619341,57.495,2.50394540602692));
#38955=CARTESIAN_POINT('Ctrl Pts',(6.69081410619341,49.875,2.50394540602692));
#38956=CARTESIAN_POINT('',(5.73138421404289,51.145,1.66039107437148));
#38957=CARTESIAN_POINT('Ctrl Pts',(5.73138421404289,51.145,1.66039107437148));
#38958=CARTESIAN_POINT('Ctrl Pts',(5.73511540682056,51.145,1.66156260377487));
#38959=CARTESIAN_POINT('Ctrl Pts',(5.7427802739896,51.145,1.66409560210805));
#38960=CARTESIAN_POINT('Ctrl Pts',(5.75488502996861,51.145,1.6684649226766));
#38961=CARTESIAN_POINT('Ctrl Pts',(5.77224172513541,51.145,1.67543235427329));
#38962=CARTESIAN_POINT('Ctrl Pts',(5.79595877235177,51.145,1.68604879760674));
#38963=CARTESIAN_POINT('Ctrl Pts',(5.82165132013192,51.145,1.69856379474191));
#38964=CARTESIAN_POINT('Ctrl Pts',(5.84921363316513,51.145,1.71294534020683));
#38965=CARTESIAN_POINT('Ctrl Pts',(5.87844620539462,51.145,1.72912206102241));
#38966=CARTESIAN_POINT('Ctrl Pts',(5.90906068827411,51.145,1.74698425466387));
#38967=CARTESIAN_POINT('Ctrl Pts',(5.94073262861949,51.145,1.76640606389864));
#38968=CARTESIAN_POINT('Ctrl Pts',(5.97314358084403,51.145,1.78726264793637));
#38969=CARTESIAN_POINT('Ctrl Pts',(6.0060228350964,51.145,1.80944727788364));
#38970=CARTESIAN_POINT('Ctrl Pts',(6.03920034699149,51.145,1.83289254541003));
#38971=CARTESIAN_POINT('Ctrl Pts',(6.07260331771232,51.145,1.85756929242874));
#38972=CARTESIAN_POINT('Ctrl Pts',(6.10621926889299,51.145,1.88347219921809));
#38973=CARTESIAN_POINT('Ctrl Pts',(6.14006878432982,51.145,1.91060895733317));
#38974=CARTESIAN_POINT('Ctrl Pts',(6.17417680788945,51.145,1.93898880419737));
#38975=CARTESIAN_POINT('Ctrl Pts',(6.20853885514981,51.145,1.96860861168851));
#38976=CARTESIAN_POINT('Ctrl Pts',(6.24311798195985,51.145,1.99945211810837));
#38977=CARTESIAN_POINT('Ctrl Pts',(6.27785854554194,51.145,2.03149622201769));
#38978=CARTESIAN_POINT('Ctrl Pts',(6.31269482043467,51.145,2.06471490843563));
#38979=CARTESIAN_POINT('Ctrl Pts',(6.34756091533115,51.145,2.09908352929888));
#38980=CARTESIAN_POINT('Ctrl Pts',(6.38240181135703,51.145,2.13458349574329));
#38981=CARTESIAN_POINT('Ctrl Pts',(6.41717671306138,51.145,2.17120312938042));
#38982=CARTESIAN_POINT('Ctrl Pts',(6.45185553518375,51.145,2.20893514043555));
#38983=CARTESIAN_POINT('Ctrl Pts',(6.48641743997175,51.145,2.24777479550457));
#38984=CARTESIAN_POINT('Ctrl Pts',(6.52084865967127,51.145,2.2877177827968));
#38985=CARTESIAN_POINT('Ctrl Pts',(6.55514062276556,51.145,2.32875748935421));
#38986=CARTESIAN_POINT('Ctrl Pts',(6.58928830924802,51.145,2.37088387159981));
#38987=CARTESIAN_POINT('Ctrl Pts',(6.6232894242584,51.145,2.41408612451229));
#38988=CARTESIAN_POINT('Ctrl Pts',(6.65037263123018,51.145,2.4495007016118));
#38989=CARTESIAN_POINT('Ctrl Pts',(6.67061900235304,51.145,2.47653809829358));
#38990=CARTESIAN_POINT('Ctrl Pts',(6.68408728750664,51.145,2.49477440711619));
#38991=CARTESIAN_POINT('Ctrl Pts',(6.69081410619341,51.145,2.50394540602692));
#38992=CARTESIAN_POINT('',(5.73138421404289,57.495,1.66039107437148));
#38993=CARTESIAN_POINT('Origin',(5.00231408838243,57.495,1.4491783055134));
#38994=CARTESIAN_POINT('',(5.1463899549833,51.145,1.4909173120086));
#38995=CARTESIAN_POINT('',(5.1463899549833,54.32,1.4909173120086));
#38996=CARTESIAN_POINT('',(5.00231408838243,51.145,1.4491783055134));
#38997=CARTESIAN_POINT('Ctrl Pts',(6.50167680247051,57.495,2.96056324982543));
#38998=CARTESIAN_POINT('Ctrl Pts',(6.50167680247051,49.875,2.96056324982543));
#38999=CARTESIAN_POINT('Ctrl Pts',(6.49043534784131,57.495,2.96229154623625));
#39000=CARTESIAN_POINT('Ctrl Pts',(6.49043534784131,49.875,2.96229154623625));
#39001=CARTESIAN_POINT('Ctrl Pts',(6.46801681444607,57.495,2.9656630481055));
#39002=CARTESIAN_POINT('Ctrl Pts',(6.46801681444607,49.875,2.9656630481055));
#39003=CARTESIAN_POINT('Ctrl Pts',(6.43458214159149,57.495,2.97046502832946));
#39004=CARTESIAN_POINT('Ctrl Pts',(6.43458214159149,49.875,2.97046502832946));
#39005=CARTESIAN_POINT('Ctrl Pts',(6.39038953466561,57.495,2.97635619664337));
#39006=CARTESIAN_POINT('Ctrl Pts',(6.39038953466561,49.875,2.97635619664337));
#39007=CARTESIAN_POINT('Ctrl Pts',(6.33579850967689,57.495,2.98286238364858));
#39008=CARTESIAN_POINT('Ctrl Pts',(6.33579850967689,49.875,2.98286238364858));
#39009=CARTESIAN_POINT('Ctrl Pts',(6.28186459845047,57.495,2.98850417352769));
#39010=CARTESIAN_POINT('Ctrl Pts',(6.28186459845047,49.875,2.98850417352769));
#39011=CARTESIAN_POINT('Ctrl Pts',(6.22859706400147,57.495,2.99327554868811));
#39012=CARTESIAN_POINT('Ctrl Pts',(6.22859706400147,49.875,2.99327554868811));
#39013=CARTESIAN_POINT('Ctrl Pts',(6.17600655789209,57.495,2.99717295692919));
#39014=CARTESIAN_POINT('Ctrl Pts',(6.17600655789209,49.875,2.99717295692919));
#39015=CARTESIAN_POINT('Ctrl Pts',(6.12410381716742,57.495,3.00019778316108));
#39016=CARTESIAN_POINT('Ctrl Pts',(6.12410381716742,49.875,3.00019778316108));
#39017=CARTESIAN_POINT('Ctrl Pts',(6.07290162599622,57.495,3.00235671375967));
#39018=CARTESIAN_POINT('Ctrl Pts',(6.07290162599622,49.875,3.00235671375967));
#39019=CARTESIAN_POINT('Ctrl Pts',(6.02241806591666,57.495,3.00366113621883));
#39020=CARTESIAN_POINT('Ctrl Pts',(6.02241806591666,49.875,3.00366113621883));
#39021=CARTESIAN_POINT('Ctrl Pts',(5.97267956506952,57.495,3.00412716938109));
#39022=CARTESIAN_POINT('Ctrl Pts',(5.97267956506952,49.875,3.00412716938109));
#39023=CARTESIAN_POINT('Ctrl Pts',(5.9237232280624,57.495,3.00377540211878));
#39024=CARTESIAN_POINT('Ctrl Pts',(5.9237232280624,49.875,3.00377540211878));
#39025=CARTESIAN_POINT('Ctrl Pts',(5.87560110342631,57.495,3.00263159433912));
#39026=CARTESIAN_POINT('Ctrl Pts',(5.87560110342631,49.875,3.00263159433912));
#39027=CARTESIAN_POINT('Ctrl Pts',(5.82837721216385,57.495,3.00072490941932));
#39028=CARTESIAN_POINT('Ctrl Pts',(5.82837721216385,49.875,3.00072490941932));
#39029=CARTESIAN_POINT('Ctrl Pts',(5.78211642456387,57.495,2.99808342690946));
#39030=CARTESIAN_POINT('Ctrl Pts',(5.78211642456387,49.875,2.99808342690946));
#39031=CARTESIAN_POINT('Ctrl Pts',(5.73687442119613,57.495,2.9947301570106));
#39032=CARTESIAN_POINT('Ctrl Pts',(5.73687442119613,49.875,2.9947301570106));
#39033=CARTESIAN_POINT('Ctrl Pts',(5.69268882427748,57.495,2.9906797244254));
#39034=CARTESIAN_POINT('Ctrl Pts',(5.69268882427748,49.875,2.9906797244254));
#39035=CARTESIAN_POINT('Ctrl Pts',(5.64956501668959,57.495,2.98593308820271));
#39036=CARTESIAN_POINT('Ctrl Pts',(5.64956501668959,49.875,2.98593308820271));
#39037=CARTESIAN_POINT('Ctrl Pts',(5.60747882861049,57.495,2.98047914221));
#39038=CARTESIAN_POINT('Ctrl Pts',(5.60747882861049,49.875,2.98047914221));
#39039=CARTESIAN_POINT('Ctrl Pts',(5.56641026634749,57.495,2.97430877025609));
#39040=CARTESIAN_POINT('Ctrl Pts',(5.56641026634749,49.875,2.97430877025609));
#39041=CARTESIAN_POINT('Ctrl Pts',(5.52637191504895,57.495,2.96742703426683));
#39042=CARTESIAN_POINT('Ctrl Pts',(5.52637191504895,49.875,2.96742703426683));
#39043=CARTESIAN_POINT('Ctrl Pts',(5.48743586913296,57.495,2.9598647928985));
#39044=CARTESIAN_POINT('Ctrl Pts',(5.48743586913296,49.875,2.9598647928985));
#39045=CARTESIAN_POINT('Ctrl Pts',(5.44977003302482,57.495,2.95169462080131));
#39046=CARTESIAN_POINT('Ctrl Pts',(5.44977003302482,49.875,2.95169462080131));
#39047=CARTESIAN_POINT('Ctrl Pts',(5.41364129622045,57.495,2.94303247002258));
#39048=CARTESIAN_POINT('Ctrl Pts',(5.41364129622045,49.875,2.94303247002258));
#39049=CARTESIAN_POINT('Ctrl Pts',(5.37936310952307,57.495,2.93401523982671));
#39050=CARTESIAN_POINT('Ctrl Pts',(5.37936310952307,49.875,2.93401523982671));
#39051=CARTESIAN_POINT('Ctrl Pts',(5.34725389048201,57.495,2.92478335875774));
#39052=CARTESIAN_POINT('Ctrl Pts',(5.34725389048201,49.875,2.92478335875774));
#39053=CARTESIAN_POINT('Ctrl Pts',(5.31759510370885,57.495,2.91546314862892));
#39054=CARTESIAN_POINT('Ctrl Pts',(5.31759510370885,49.875,2.91546314862892));
#39055=CARTESIAN_POINT('Ctrl Pts',(5.29057828960676,57.495,2.90614521320837));
#39056=CARTESIAN_POINT('Ctrl Pts',(5.29057828960676,49.875,2.90614521320837));
#39057=CARTESIAN_POINT('Ctrl Pts',(5.26630084561719,57.495,2.89688168736508));
#39058=CARTESIAN_POINT('Ctrl Pts',(5.26630084561719,49.875,2.89688168736508));
#39059=CARTESIAN_POINT('Ctrl Pts',(5.24910109063628,57.495,2.88953536864313));
#39060=CARTESIAN_POINT('Ctrl Pts',(5.24910109063628,49.875,2.88953536864313));
#39061=CARTESIAN_POINT('Ctrl Pts',(5.23745215939571,57.495,2.88406558980901));
#39062=CARTESIAN_POINT('Ctrl Pts',(5.23745215939571,49.875,2.88406558980901));
#39063=CARTESIAN_POINT('Ctrl Pts',(5.23024117954545,57.495,2.88043681055505));
#39064=CARTESIAN_POINT('Ctrl Pts',(5.23024117954545,49.875,2.88043681055505));
#39065=CARTESIAN_POINT('Ctrl Pts',(5.22677443144495,57.495,2.87862685522557));
#39066=CARTESIAN_POINT('Ctrl Pts',(5.22677443144495,49.875,2.87862685522557));
#39067=CARTESIAN_POINT('Ctrl Pts',(6.50167680247051,51.145,2.96056324982543));
#39068=CARTESIAN_POINT('Ctrl Pts',(6.49043534784131,51.145,2.96229154623625));
#39069=CARTESIAN_POINT('Ctrl Pts',(6.46801681444607,51.145,2.9656630481055));
#39070=CARTESIAN_POINT('Ctrl Pts',(6.43458214159149,51.145,2.97046502832946));
#39071=CARTESIAN_POINT('Ctrl Pts',(6.39038953466561,51.145,2.97635619664337));
#39072=CARTESIAN_POINT('Ctrl Pts',(6.33579850967689,51.145,2.98286238364858));
#39073=CARTESIAN_POINT('Ctrl Pts',(6.28186459845047,51.145,2.98850417352769));
#39074=CARTESIAN_POINT('Ctrl Pts',(6.22859706400147,51.145,2.99327554868811));
#39075=CARTESIAN_POINT('Ctrl Pts',(6.17600655789209,51.145,2.99717295692919));
#39076=CARTESIAN_POINT('Ctrl Pts',(6.12410381716742,51.145,3.00019778316108));
#39077=CARTESIAN_POINT('Ctrl Pts',(6.07290162599622,51.145,3.00235671375967));
#39078=CARTESIAN_POINT('Ctrl Pts',(6.02241806591666,51.145,3.00366113621883));
#39079=CARTESIAN_POINT('Ctrl Pts',(5.97267956506952,51.145,3.00412716938109));
#39080=CARTESIAN_POINT('Ctrl Pts',(5.9237232280624,51.145,3.00377540211878));
#39081=CARTESIAN_POINT('Ctrl Pts',(5.87560110342631,51.145,3.00263159433912));
#39082=CARTESIAN_POINT('Ctrl Pts',(5.82837721216385,51.145,3.00072490941932));
#39083=CARTESIAN_POINT('Ctrl Pts',(5.78211642456387,51.145,2.99808342690946));
#39084=CARTESIAN_POINT('Ctrl Pts',(5.73687442119613,51.145,2.9947301570106));
#39085=CARTESIAN_POINT('Ctrl Pts',(5.69268882427748,51.145,2.9906797244254));
#39086=CARTESIAN_POINT('Ctrl Pts',(5.64956501668959,51.145,2.98593308820271));
#39087=CARTESIAN_POINT('Ctrl Pts',(5.60747882861049,51.145,2.98047914221));
#39088=CARTESIAN_POINT('Ctrl Pts',(5.56641026634749,51.145,2.97430877025609));
#39089=CARTESIAN_POINT('Ctrl Pts',(5.52637191504895,51.145,2.96742703426683));
#39090=CARTESIAN_POINT('Ctrl Pts',(5.48743586913296,51.145,2.9598647928985));
#39091=CARTESIAN_POINT('Ctrl Pts',(5.44977003302482,51.145,2.95169462080131));
#39092=CARTESIAN_POINT('Ctrl Pts',(5.41364129622045,51.145,2.94303247002258));
#39093=CARTESIAN_POINT('Ctrl Pts',(5.37936310952307,51.145,2.93401523982671));
#39094=CARTESIAN_POINT('Ctrl Pts',(5.34725389048201,51.145,2.92478335875774));
#39095=CARTESIAN_POINT('Ctrl Pts',(5.31759510370885,51.145,2.91546314862892));
#39096=CARTESIAN_POINT('Ctrl Pts',(5.29057828960676,51.145,2.90614521320837));
#39097=CARTESIAN_POINT('Ctrl Pts',(5.26630084561719,51.145,2.89688168736508));
#39098=CARTESIAN_POINT('Ctrl Pts',(5.24910109063628,51.145,2.88953536864313));
#39099=CARTESIAN_POINT('Ctrl Pts',(5.23745215939571,51.145,2.88406558980901));
#39100=CARTESIAN_POINT('Ctrl Pts',(5.23024117954545,51.145,2.88043681055505));
#39101=CARTESIAN_POINT('Ctrl Pts',(5.22677443144495,51.145,2.87862685522557));
#39102=CARTESIAN_POINT('Origin',(0.,54.32,0.));
#39103=CARTESIAN_POINT('',(5.32519370006274,51.145,0.592010183030742));
#39104=CARTESIAN_POINT('Origin',(0.,51.145,0.));
#39105=CARTESIAN_POINT('',(5.32519370006274,54.32,0.592010183030742));
#39106=CARTESIAN_POINT('Origin',(5.93051272372135,57.495,0.659304453656786));
#39107=CARTESIAN_POINT('',(5.93051272372135,51.145,0.659304453656786));
#39108=CARTESIAN_POINT('',(5.93051272372135,51.145,0.659304453656786));
#39109=CARTESIAN_POINT('',(5.93051272372135,57.495,0.659304453656786));
#39110=CARTESIAN_POINT('Origin',(1.6286971771251E-12,57.495,-4.16333634234733E-16));
#39111=CARTESIAN_POINT('',(7.13972463098307,51.145,0.247119796320915));
#39112=CARTESIAN_POINT('',(7.13972463098307,57.495,0.247119796320915));
#39113=CARTESIAN_POINT('',(7.13972463098307,51.145,-0.247119796320921));
#39114=CARTESIAN_POINT('Origin',(1.6286971771251E-12,51.145,-4.16333634234733E-16));
#39115=CARTESIAN_POINT('',(7.13972463098307,57.495,-0.247119796320921));
#39116=CARTESIAN_POINT('Ctrl Pts',(5.93051272372135,57.495,-0.659304453656789));
#39117=CARTESIAN_POINT('Ctrl Pts',(5.93051272372135,49.875,-0.659304453656789));
#39118=CARTESIAN_POINT('Ctrl Pts',(5.9344082212537,57.495,-0.659649967278237));
#39119=CARTESIAN_POINT('Ctrl Pts',(5.9344082212537,49.875,-0.659649967278237));
#39120=CARTESIAN_POINT('Ctrl Pts',(5.94245897164691,57.495,-0.660242999639202));
#39121=CARTESIAN_POINT('Ctrl Pts',(5.94245897164691,49.875,-0.660242999639202));
#39122=CARTESIAN_POINT('Ctrl Pts',(5.95531437453424,57.495,-0.660838563360922));
#39123=CARTESIAN_POINT('Ctrl Pts',(5.95531437453424,49.875,-0.660838563360922));
#39124=CARTESIAN_POINT('Ctrl Pts',(5.97401619058907,57.495,-0.661043615595513));
#39125=CARTESIAN_POINT('Ctrl Pts',(5.97401619058907,49.875,-0.661043615595513));
#39126=CARTESIAN_POINT('Ctrl Pts',(5.99999062205823,57.495,-0.660311421925998));
#39127=CARTESIAN_POINT('Ctrl Pts',(5.99999062205823,49.875,-0.660311421925998));
#39128=CARTESIAN_POINT('Ctrl Pts',(6.0285167231501,57.495,-0.658581184594089));
#39129=CARTESIAN_POINT('Ctrl Pts',(6.0285167231501,49.875,-0.658581184594089));
#39130=CARTESIAN_POINT('Ctrl Pts',(6.05948455921138,57.495,-0.655842009648634));
#39131=CARTESIAN_POINT('Ctrl Pts',(6.05948455921138,49.875,-0.655842009648634));
#39132=CARTESIAN_POINT('Ctrl Pts',(6.09268249742298,57.495,-0.652083489461621));
#39133=CARTESIAN_POINT('Ctrl Pts',(6.09268249742298,49.875,-0.652083489461621));
#39134=CARTESIAN_POINT('Ctrl Pts',(6.12780215712604,57.495,-0.647296629738921));
#39135=CARTESIAN_POINT('Ctrl Pts',(6.12780215712604,49.875,-0.647296629738921));
#39136=CARTESIAN_POINT('Ctrl Pts',(6.16449561918676,57.495,-0.641473544543615));
#39137=CARTESIAN_POINT('Ctrl Pts',(6.16449561918676,49.875,-0.641473544543615));
#39138=CARTESIAN_POINT('Ctrl Pts',(6.20242090374318,57.495,-0.634607707876565));
#39139=CARTESIAN_POINT('Ctrl Pts',(6.20242090374318,49.875,-0.634607707876565));
#39140=CARTESIAN_POINT('Ctrl Pts',(6.24128706412515,57.495,-0.626694128202843));
#39141=CARTESIAN_POINT('Ctrl Pts',(6.24128706412515,49.875,-0.626694128202843));
#39142=CARTESIAN_POINT('Ctrl Pts',(6.2809112037544,57.495,-0.617730009530308));
#39143=CARTESIAN_POINT('Ctrl Pts',(6.2809112037544,49.875,-0.617730009530308));
#39144=CARTESIAN_POINT('Ctrl Pts',(6.32121490697716,57.495,-0.607714431517403));
#39145=CARTESIAN_POINT('Ctrl Pts',(6.32121490697716,49.875,-0.607714431517403));
#39146=CARTESIAN_POINT('Ctrl Pts',(6.36218460951727,57.495,-0.596647533682212));
#39147=CARTESIAN_POINT('Ctrl Pts',(6.36218460951727,49.875,-0.596647533682212));
#39148=CARTESIAN_POINT('Ctrl Pts',(6.40384227175352,57.495,-0.584530087032239));
#39149=CARTESIAN_POINT('Ctrl Pts',(6.40384227175352,49.875,-0.584530087032239));
#39150=CARTESIAN_POINT('Ctrl Pts',(6.44621447382266,57.495,-0.57136310290558));
#39151=CARTESIAN_POINT('Ctrl Pts',(6.44621447382266,49.875,-0.57136310290558));
#39152=CARTESIAN_POINT('Ctrl Pts',(6.4892958755784,57.495,-0.557147755196278));
#39153=CARTESIAN_POINT('Ctrl Pts',(6.4892958755784,49.875,-0.557147755196278));
#39154=CARTESIAN_POINT('Ctrl Pts',(6.53304612199323,57.495,-0.541884929839951));
#39155=CARTESIAN_POINT('Ctrl Pts',(6.53304612199323,49.875,-0.541884929839951));
#39156=CARTESIAN_POINT('Ctrl Pts',(6.57740496530571,57.495,-0.525574676214357));
#39157=CARTESIAN_POINT('Ctrl Pts',(6.57740496530571,49.875,-0.525574676214357));
#39158=CARTESIAN_POINT('Ctrl Pts',(6.62230172760513,57.495,-0.508215876982669));
#39159=CARTESIAN_POINT('Ctrl Pts',(6.62230172760513,49.875,-0.508215876982669));
#39160=CARTESIAN_POINT('Ctrl Pts',(6.66766610085618,57.495,-0.489806088474624));
#39161=CARTESIAN_POINT('Ctrl Pts',(6.66766610085618,49.875,-0.489806088474624));
#39162=CARTESIAN_POINT('Ctrl Pts',(6.71344014059664,57.495,-0.470341429749656));
#39163=CARTESIAN_POINT('Ctrl Pts',(6.71344014059664,49.875,-0.470341429749656));
#39164=CARTESIAN_POINT('Ctrl Pts',(6.75958168761858,57.495,-0.44981707848863));
#39165=CARTESIAN_POINT('Ctrl Pts',(6.75958168761858,49.875,-0.44981707848863));
#39166=CARTESIAN_POINT('Ctrl Pts',(6.80606015708966,57.495,-0.428228256434474));
#39167=CARTESIAN_POINT('Ctrl Pts',(6.80606015708966,49.875,-0.428228256434474));
#39168=CARTESIAN_POINT('Ctrl Pts',(6.85285448604159,57.495,-0.405571362419757));
#39169=CARTESIAN_POINT('Ctrl Pts',(6.85285448604159,49.875,-0.405571362419757));
#39170=CARTESIAN_POINT('Ctrl Pts',(6.89995030467727,57.495,-0.381845111328236));
#39171=CARTESIAN_POINT('Ctrl Pts',(6.89995030467727,49.875,-0.381845111328236));
#39172=CARTESIAN_POINT('Ctrl Pts',(6.94733716327837,57.495,-0.357052332559036));
#39173=CARTESIAN_POINT('Ctrl Pts',(6.94733716327837,49.875,-0.357052332559036));
#39174=CARTESIAN_POINT('Ctrl Pts',(6.99500658045299,57.495,-0.33120038409401));
#39175=CARTESIAN_POINT('Ctrl Pts',(6.99500658045299,49.875,-0.33120038409401));
#39176=CARTESIAN_POINT('Ctrl Pts',(7.0429523011241,57.495,-0.304298370266206));
#39177=CARTESIAN_POINT('Ctrl Pts',(7.0429523011241,49.875,-0.304298370266206));
#39178=CARTESIAN_POINT('Ctrl Pts',(7.0815264936403,57.495,-0.281943861934841));
#39179=CARTESIAN_POINT('Ctrl Pts',(7.0815264936403,49.875,-0.281943861934841));
#39180=CARTESIAN_POINT('Ctrl Pts',(7.11057846529273,57.495,-0.264712515322388));
#39181=CARTESIAN_POINT('Ctrl Pts',(7.11057846529273,49.875,-0.264712515322388));
#39182=CARTESIAN_POINT('Ctrl Pts',(7.13000027153808,57.495,-0.253018452443277));
#39183=CARTESIAN_POINT('Ctrl Pts',(7.13000027153808,49.875,-0.253018452443277));
#39184=CARTESIAN_POINT('Ctrl Pts',(7.13972463098307,57.495,-0.247119796320918));
#39185=CARTESIAN_POINT('Ctrl Pts',(7.13972463098307,49.875,-0.247119796320918));
#39186=CARTESIAN_POINT('',(5.93051272372135,51.145,-0.659304453656789));
#39187=CARTESIAN_POINT('Ctrl Pts',(5.93051272372135,51.145,-0.659304453656789));
#39188=CARTESIAN_POINT('Ctrl Pts',(5.9344082212537,51.145,-0.659649967278237));
#39189=CARTESIAN_POINT('Ctrl Pts',(5.94245897164691,51.145,-0.660242999639202));
#39190=CARTESIAN_POINT('Ctrl Pts',(5.95531437453424,51.145,-0.660838563360922));
#39191=CARTESIAN_POINT('Ctrl Pts',(5.97401619058907,51.145,-0.661043615595513));
#39192=CARTESIAN_POINT('Ctrl Pts',(5.99999062205823,51.145,-0.660311421925998));
#39193=CARTESIAN_POINT('Ctrl Pts',(6.0285167231501,51.145,-0.658581184594089));
#39194=CARTESIAN_POINT('Ctrl Pts',(6.05948455921138,51.145,-0.655842009648634));
#39195=CARTESIAN_POINT('Ctrl Pts',(6.09268249742298,51.145,-0.652083489461621));
#39196=CARTESIAN_POINT('Ctrl Pts',(6.12780215712604,51.145,-0.647296629738921));
#39197=CARTESIAN_POINT('Ctrl Pts',(6.16449561918676,51.145,-0.641473544543615));
#39198=CARTESIAN_POINT('Ctrl Pts',(6.20242090374318,51.145,-0.634607707876565));
#39199=CARTESIAN_POINT('Ctrl Pts',(6.24128706412515,51.145,-0.626694128202843));
#39200=CARTESIAN_POINT('Ctrl Pts',(6.2809112037544,51.145,-0.617730009530308));
#39201=CARTESIAN_POINT('Ctrl Pts',(6.32121490697716,51.145,-0.607714431517403));
#39202=CARTESIAN_POINT('Ctrl Pts',(6.36218460951727,51.145,-0.596647533682212));
#39203=CARTESIAN_POINT('Ctrl Pts',(6.40384227175352,51.145,-0.584530087032239));
#39204=CARTESIAN_POINT('Ctrl Pts',(6.44621447382266,51.145,-0.57136310290558));
#39205=CARTESIAN_POINT('Ctrl Pts',(6.4892958755784,51.145,-0.557147755196278));
#39206=CARTESIAN_POINT('Ctrl Pts',(6.53304612199323,51.145,-0.541884929839951));
#39207=CARTESIAN_POINT('Ctrl Pts',(6.57740496530571,51.145,-0.525574676214357));
#39208=CARTESIAN_POINT('Ctrl Pts',(6.62230172760513,51.145,-0.508215876982669));
#39209=CARTESIAN_POINT('Ctrl Pts',(6.66766610085618,51.145,-0.489806088474624));
#39210=CARTESIAN_POINT('Ctrl Pts',(6.71344014059664,51.145,-0.470341429749656));
#39211=CARTESIAN_POINT('Ctrl Pts',(6.75958168761858,51.145,-0.44981707848863));
#39212=CARTESIAN_POINT('Ctrl Pts',(6.80606015708966,51.145,-0.428228256434474));
#39213=CARTESIAN_POINT('Ctrl Pts',(6.85285448604159,51.145,-0.405571362419757));
#39214=CARTESIAN_POINT('Ctrl Pts',(6.89995030467727,51.145,-0.381845111328236));
#39215=CARTESIAN_POINT('Ctrl Pts',(6.94733716327837,51.145,-0.357052332559036));
#39216=CARTESIAN_POINT('Ctrl Pts',(6.99500658045299,51.145,-0.33120038409401));
#39217=CARTESIAN_POINT('Ctrl Pts',(7.0429523011241,51.145,-0.304298370266206));
#39218=CARTESIAN_POINT('Ctrl Pts',(7.0815264936403,51.145,-0.281943861934841));
#39219=CARTESIAN_POINT('Ctrl Pts',(7.11057846529273,51.145,-0.264712515322388));
#39220=CARTESIAN_POINT('Ctrl Pts',(7.13000027153808,51.145,-0.253018452443277));
#39221=CARTESIAN_POINT('Ctrl Pts',(7.13972463098307,51.145,-0.247119796320918));
#39222=CARTESIAN_POINT('',(5.93051272372135,57.495,-0.659304453656789));
#39223=CARTESIAN_POINT('Origin',(5.17611212951227,57.495,-0.575436549687219));
#39224=CARTESIAN_POINT('',(5.32519370006274,51.145,-0.592010183030745));
#39225=CARTESIAN_POINT('',(5.32519370006274,54.32,-0.592010183030745));
#39226=CARTESIAN_POINT('',(5.17611212951227,51.145,-0.575436549687219));
#39227=CARTESIAN_POINT('Ctrl Pts',(7.13972463098307,57.495,0.247119796320915));
#39228=CARTESIAN_POINT('Ctrl Pts',(7.13972463098307,49.875,0.247119796320915));
#39229=CARTESIAN_POINT('Ctrl Pts',(7.13000027153814,57.495,0.253018452443265));
#39230=CARTESIAN_POINT('Ctrl Pts',(7.13000027153814,49.875,0.253018452443265));
#39231=CARTESIAN_POINT('Ctrl Pts',(7.1105784652929,57.495,0.264712515322363));
#39232=CARTESIAN_POINT('Ctrl Pts',(7.1105784652929,49.875,0.264712515322363));
#39233=CARTESIAN_POINT('Ctrl Pts',(7.0815264936406,57.495,0.281943861934802));
#39234=CARTESIAN_POINT('Ctrl Pts',(7.0815264936406,49.875,0.281943861934802));
#39235=CARTESIAN_POINT('Ctrl Pts',(7.04295230112448,57.495,0.304298370266161));
#39236=CARTESIAN_POINT('Ctrl Pts',(7.04295230112448,49.875,0.304298370266161));
#39237=CARTESIAN_POINT('Ctrl Pts',(6.99500658045334,57.495,0.331200384093974));
#39238=CARTESIAN_POINT('Ctrl Pts',(6.99500658045334,49.875,0.331200384093974));
#39239=CARTESIAN_POINT('Ctrl Pts',(6.94733716327859,57.495,0.357052332559016));
#39240=CARTESIAN_POINT('Ctrl Pts',(6.94733716327859,49.875,0.357052332559016));
#39241=CARTESIAN_POINT('Ctrl Pts',(6.89995030467732,57.495,0.38184511132823));
#39242=CARTESIAN_POINT('Ctrl Pts',(6.89995030467732,49.875,0.38184511132823));
#39243=CARTESIAN_POINT('Ctrl Pts',(6.85285448604147,57.495,0.405571362419761));
#39244=CARTESIAN_POINT('Ctrl Pts',(6.85285448604147,49.875,0.405571362419761));
#39245=CARTESIAN_POINT('Ctrl Pts',(6.80606015708944,57.495,0.42822825643448));
#39246=CARTESIAN_POINT('Ctrl Pts',(6.80606015708944,49.875,0.42822825643448));
#39247=CARTESIAN_POINT('Ctrl Pts',(6.75958168761835,57.495,0.449817078488633));
#39248=CARTESIAN_POINT('Ctrl Pts',(6.75958168761835,49.875,0.449817078488633));
#39249=CARTESIAN_POINT('Ctrl Pts',(6.71344014059646,57.495,0.470341429749655));
#39250=CARTESIAN_POINT('Ctrl Pts',(6.71344014059646,49.875,0.470341429749655));
#39251=CARTESIAN_POINT('Ctrl Pts',(6.66766610085612,57.495,0.489806088474619));
#39252=CARTESIAN_POINT('Ctrl Pts',(6.66766610085612,49.875,0.489806088474619));
#39253=CARTESIAN_POINT('Ctrl Pts',(6.62230172760518,57.495,0.508215876982666));
#39254=CARTESIAN_POINT('Ctrl Pts',(6.62230172760518,49.875,0.508215876982666));
#39255=CARTESIAN_POINT('Ctrl Pts',(6.57740496530586,57.495,0.525574676214359));
#39256=CARTESIAN_POINT('Ctrl Pts',(6.57740496530586,49.875,0.525574676214359));
#39257=CARTESIAN_POINT('Ctrl Pts',(6.53304612199338,57.495,0.541884929839957));
#39258=CARTESIAN_POINT('Ctrl Pts',(6.53304612199338,49.875,0.541884929839957));
#39259=CARTESIAN_POINT('Ctrl Pts',(6.48929587557851,57.495,0.557147755196286));
#39260=CARTESIAN_POINT('Ctrl Pts',(6.48929587557851,49.875,0.557147755196286));
#39261=CARTESIAN_POINT('Ctrl Pts',(6.4462144738227,57.495,0.571363102905584));
#39262=CARTESIAN_POINT('Ctrl Pts',(6.4462144738227,49.875,0.571363102905584));
#39263=CARTESIAN_POINT('Ctrl Pts',(6.40384227175349,57.495,0.584530087032232));
#39264=CARTESIAN_POINT('Ctrl Pts',(6.40384227175349,49.875,0.584530087032232));
#39265=CARTESIAN_POINT('Ctrl Pts',(6.36218460951721,57.495,0.596647533682194));
#39266=CARTESIAN_POINT('Ctrl Pts',(6.36218460951721,49.875,0.596647533682194));
#39267=CARTESIAN_POINT('Ctrl Pts',(6.32121490697708,57.495,0.607714431517377));
#39268=CARTESIAN_POINT('Ctrl Pts',(6.32121490697708,49.875,0.607714431517377));
#39269=CARTESIAN_POINT('Ctrl Pts',(6.28091120375433,57.495,0.617730009530282));
#39270=CARTESIAN_POINT('Ctrl Pts',(6.28091120375433,49.875,0.617730009530282));
#39271=CARTESIAN_POINT('Ctrl Pts',(6.24128706412512,57.495,0.626694128202827));
#39272=CARTESIAN_POINT('Ctrl Pts',(6.24128706412512,49.875,0.626694128202827));
#39273=CARTESIAN_POINT('Ctrl Pts',(6.2024209037432,57.495,0.634607707876569));
#39274=CARTESIAN_POINT('Ctrl Pts',(6.2024209037432,49.875,0.634607707876569));
#39275=CARTESIAN_POINT('Ctrl Pts',(6.16449561918681,57.495,0.641473544543642));
#39276=CARTESIAN_POINT('Ctrl Pts',(6.16449561918681,49.875,0.641473544543642));
#39277=CARTESIAN_POINT('Ctrl Pts',(6.12780215712609,57.495,0.647296629738963));
#39278=CARTESIAN_POINT('Ctrl Pts',(6.12780215712609,49.875,0.647296629738963));
#39279=CARTESIAN_POINT('Ctrl Pts',(6.092682497423,57.495,0.652083489461662));
#39280=CARTESIAN_POINT('Ctrl Pts',(6.092682497423,49.875,0.652083489461662));
#39281=CARTESIAN_POINT('Ctrl Pts',(6.05948455921138,57.495,0.655842009648653));
#39282=CARTESIAN_POINT('Ctrl Pts',(6.05948455921138,49.875,0.655842009648653));
#39283=CARTESIAN_POINT('Ctrl Pts',(6.02851672315009,57.495,0.658581184594064));
#39284=CARTESIAN_POINT('Ctrl Pts',(6.02851672315009,49.875,0.658581184594064));
#39285=CARTESIAN_POINT('Ctrl Pts',(5.99999062205821,57.495,0.660311421925918));
#39286=CARTESIAN_POINT('Ctrl Pts',(5.99999062205821,49.875,0.660311421925918));
#39287=CARTESIAN_POINT('Ctrl Pts',(5.97401619058905,57.495,0.661043615595394));
#39288=CARTESIAN_POINT('Ctrl Pts',(5.97401619058905,49.875,0.661043615595394));
#39289=CARTESIAN_POINT('Ctrl Pts',(5.95531437453421,57.495,0.660838563360811));
#39290=CARTESIAN_POINT('Ctrl Pts',(5.95531437453421,49.875,0.660838563360811));
#39291=CARTESIAN_POINT('Ctrl Pts',(5.94245897164689,57.495,0.66024299963913));
#39292=CARTESIAN_POINT('Ctrl Pts',(5.94245897164689,49.875,0.66024299963913));
#39293=CARTESIAN_POINT('Ctrl Pts',(5.93440822125369,57.495,0.659649967278209));
#39294=CARTESIAN_POINT('Ctrl Pts',(5.93440822125369,49.875,0.659649967278209));
#39295=CARTESIAN_POINT('Ctrl Pts',(5.93051272372135,57.495,0.659304453656786));
#39296=CARTESIAN_POINT('Ctrl Pts',(5.93051272372135,49.875,0.659304453656786));
#39297=CARTESIAN_POINT('Ctrl Pts',(7.13972463098307,51.145,0.247119796320915));
#39298=CARTESIAN_POINT('Ctrl Pts',(7.13000027153814,51.145,0.253018452443265));
#39299=CARTESIAN_POINT('Ctrl Pts',(7.1105784652929,51.145,0.264712515322363));
#39300=CARTESIAN_POINT('Ctrl Pts',(7.0815264936406,51.145,0.281943861934802));
#39301=CARTESIAN_POINT('Ctrl Pts',(7.04295230112448,51.145,0.304298370266161));
#39302=CARTESIAN_POINT('Ctrl Pts',(6.99500658045334,51.145,0.331200384093974));
#39303=CARTESIAN_POINT('Ctrl Pts',(6.94733716327859,51.145,0.357052332559016));
#39304=CARTESIAN_POINT('Ctrl Pts',(6.89995030467732,51.145,0.38184511132823));
#39305=CARTESIAN_POINT('Ctrl Pts',(6.85285448604147,51.145,0.405571362419761));
#39306=CARTESIAN_POINT('Ctrl Pts',(6.80606015708944,51.145,0.42822825643448));
#39307=CARTESIAN_POINT('Ctrl Pts',(6.75958168761835,51.145,0.449817078488633));
#39308=CARTESIAN_POINT('Ctrl Pts',(6.71344014059646,51.145,0.470341429749655));
#39309=CARTESIAN_POINT('Ctrl Pts',(6.66766610085612,51.145,0.489806088474619));
#39310=CARTESIAN_POINT('Ctrl Pts',(6.62230172760518,51.145,0.508215876982666));
#39311=CARTESIAN_POINT('Ctrl Pts',(6.57740496530586,51.145,0.525574676214359));
#39312=CARTESIAN_POINT('Ctrl Pts',(6.53304612199338,51.145,0.541884929839957));
#39313=CARTESIAN_POINT('Ctrl Pts',(6.48929587557851,51.145,0.557147755196286));
#39314=CARTESIAN_POINT('Ctrl Pts',(6.4462144738227,51.145,0.571363102905584));
#39315=CARTESIAN_POINT('Ctrl Pts',(6.40384227175349,51.145,0.584530087032232));
#39316=CARTESIAN_POINT('Ctrl Pts',(6.36218460951721,51.145,0.596647533682194));
#39317=CARTESIAN_POINT('Ctrl Pts',(6.32121490697708,51.145,0.607714431517377));
#39318=CARTESIAN_POINT('Ctrl Pts',(6.28091120375433,51.145,0.617730009530282));
#39319=CARTESIAN_POINT('Ctrl Pts',(6.24128706412512,51.145,0.626694128202827));
#39320=CARTESIAN_POINT('Ctrl Pts',(6.2024209037432,51.145,0.634607707876569));
#39321=CARTESIAN_POINT('Ctrl Pts',(6.16449561918681,51.145,0.641473544543642));
#39322=CARTESIAN_POINT('Ctrl Pts',(6.12780215712609,51.145,0.647296629738963));
#39323=CARTESIAN_POINT('Ctrl Pts',(6.092682497423,51.145,0.652083489461662));
#39324=CARTESIAN_POINT('Ctrl Pts',(6.05948455921138,51.145,0.655842009648653));
#39325=CARTESIAN_POINT('Ctrl Pts',(6.02851672315009,51.145,0.658581184594064));
#39326=CARTESIAN_POINT('Ctrl Pts',(5.99999062205821,51.145,0.660311421925918));
#39327=CARTESIAN_POINT('Ctrl Pts',(5.97401619058905,51.145,0.661043615595394));
#39328=CARTESIAN_POINT('Ctrl Pts',(5.95531437453421,51.145,0.660838563360811));
#39329=CARTESIAN_POINT('Ctrl Pts',(5.94245897164689,51.145,0.66024299963913));
#39330=CARTESIAN_POINT('Ctrl Pts',(5.93440822125369,51.145,0.659649967278209));
#39331=CARTESIAN_POINT('Ctrl Pts',(5.93051272372135,51.145,0.659304453656786));
#39332=CARTESIAN_POINT('Origin',(0.,54.32,0.));
#39333=CARTESIAN_POINT('',(5.1463899549833,51.145,-1.4909173120086));
#39334=CARTESIAN_POINT('Origin',(0.,51.145,0.));
#39335=CARTESIAN_POINT('',(5.1463899549833,54.32,-1.4909173120086));
#39336=CARTESIAN_POINT('Origin',(5.73138421404289,57.495,-1.66039107437149));
#39337=CARTESIAN_POINT('',(5.73138421404289,51.145,-1.66039107437149));
#39338=CARTESIAN_POINT('',(5.73138421404289,51.145,-1.66039107437149));
#39339=CARTESIAN_POINT('',(5.73138421404289,57.495,-1.66039107437149));
#39340=CARTESIAN_POINT('Origin',(1.50456066262064E-12,57.495,-6.23660068148934E-13));
#39341=CARTESIAN_POINT('',(6.6908141061934,51.145,-2.50394540602693));
#39342=CARTESIAN_POINT('',(6.6908141061934,57.495,-2.50394540602693));
#39343=CARTESIAN_POINT('',(6.5016768024705,51.145,-2.96056324982543));
#39344=CARTESIAN_POINT('Origin',(1.50456066262064E-12,51.145,-6.23660068148934E-13));
#39345=CARTESIAN_POINT('',(6.5016768024705,57.495,-2.96056324982543));
#39346=CARTESIAN_POINT('Ctrl Pts',(5.22677443144495,57.495,-2.87862685522557));
#39347=CARTESIAN_POINT('Ctrl Pts',(5.22677443144495,49.875,-2.87862685522557));
#39348=CARTESIAN_POINT('Ctrl Pts',(5.23024117954544,57.495,-2.88043681055508));
#39349=CARTESIAN_POINT('Ctrl Pts',(5.23024117954544,49.875,-2.88043681055508));
#39350=CARTESIAN_POINT('Ctrl Pts',(5.2374521593957,57.495,-2.88406558980908));
#39351=CARTESIAN_POINT('Ctrl Pts',(5.2374521593957,49.875,-2.88406558980908));
#39352=CARTESIAN_POINT('Ctrl Pts',(5.24910109063627,57.495,-2.88953536864324));
#39353=CARTESIAN_POINT('Ctrl Pts',(5.24910109063627,49.875,-2.88953536864324));
#39354=CARTESIAN_POINT('Ctrl Pts',(5.26630084561717,57.495,-2.8968816873652));
#39355=CARTESIAN_POINT('Ctrl Pts',(5.26630084561717,49.875,-2.8968816873652));
#39356=CARTESIAN_POINT('Ctrl Pts',(5.29057828960674,57.495,-2.90614521320845));
#39357=CARTESIAN_POINT('Ctrl Pts',(5.29057828960674,49.875,-2.90614521320845));
#39358=CARTESIAN_POINT('Ctrl Pts',(5.31759510370885,57.495,-2.91546314862894));
#39359=CARTESIAN_POINT('Ctrl Pts',(5.31759510370885,49.875,-2.91546314862894));
#39360=CARTESIAN_POINT('Ctrl Pts',(5.34725389048201,57.495,-2.92478335875772));
#39361=CARTESIAN_POINT('Ctrl Pts',(5.34725389048201,49.875,-2.92478335875772));
#39362=CARTESIAN_POINT('Ctrl Pts',(5.37936310952306,57.495,-2.93401523982667));
#39363=CARTESIAN_POINT('Ctrl Pts',(5.37936310952306,49.875,-2.93401523982667));
#39364=CARTESIAN_POINT('Ctrl Pts',(5.41364129622042,57.495,-2.94303247002252));
#39365=CARTESIAN_POINT('Ctrl Pts',(5.41364129622042,49.875,-2.94303247002252));
#39366=CARTESIAN_POINT('Ctrl Pts',(5.44977003302479,57.495,-2.95169462080126));
#39367=CARTESIAN_POINT('Ctrl Pts',(5.44977003302479,49.875,-2.95169462080126));
#39368=CARTESIAN_POINT('Ctrl Pts',(5.48743586913294,57.495,-2.95986479289849));
#39369=CARTESIAN_POINT('Ctrl Pts',(5.48743586913294,49.875,-2.95986479289849));
#39370=CARTESIAN_POINT('Ctrl Pts',(5.52637191504897,57.495,-2.96742703426686));
#39371=CARTESIAN_POINT('Ctrl Pts',(5.52637191504897,49.875,-2.96742703426686));
#39372=CARTESIAN_POINT('Ctrl Pts',(5.56641026634754,57.495,-2.97430877025614));
#39373=CARTESIAN_POINT('Ctrl Pts',(5.56641026634754,49.875,-2.97430877025614));
#39374=CARTESIAN_POINT('Ctrl Pts',(5.60747882861056,57.495,-2.98047914221006));
#39375=CARTESIAN_POINT('Ctrl Pts',(5.60747882861056,49.875,-2.98047914221006));
#39376=CARTESIAN_POINT('Ctrl Pts',(5.64956501668965,57.495,-2.98593308820275));
#39377=CARTESIAN_POINT('Ctrl Pts',(5.64956501668965,49.875,-2.98593308820275));
#39378=CARTESIAN_POINT('Ctrl Pts',(5.6926888242775,57.495,-2.99067972442542));
#39379=CARTESIAN_POINT('Ctrl Pts',(5.6926888242775,49.875,-2.99067972442542));
#39380=CARTESIAN_POINT('Ctrl Pts',(5.73687442119609,57.495,-2.99473015701059));
#39381=CARTESIAN_POINT('Ctrl Pts',(5.73687442119609,49.875,-2.99473015701059));
#39382=CARTESIAN_POINT('Ctrl Pts',(5.78211642456377,57.495,-2.99808342690941));
#39383=CARTESIAN_POINT('Ctrl Pts',(5.78211642456377,49.875,-2.99808342690941));
#39384=CARTESIAN_POINT('Ctrl Pts',(5.82837721216371,57.495,-3.00072490941926));
#39385=CARTESIAN_POINT('Ctrl Pts',(5.82837721216371,49.875,-3.00072490941926));
#39386=CARTESIAN_POINT('Ctrl Pts',(5.87560110342618,57.495,-3.00263159433907));
#39387=CARTESIAN_POINT('Ctrl Pts',(5.87560110342618,49.875,-3.00263159433907));
#39388=CARTESIAN_POINT('Ctrl Pts',(5.92372322806235,57.495,-3.00377540211876));
#39389=CARTESIAN_POINT('Ctrl Pts',(5.92372322806235,49.875,-3.00377540211876));
#39390=CARTESIAN_POINT('Ctrl Pts',(5.97267956506957,57.495,-3.00412716938112));
#39391=CARTESIAN_POINT('Ctrl Pts',(5.97267956506957,49.875,-3.00412716938112));
#39392=CARTESIAN_POINT('Ctrl Pts',(6.02241806591682,57.495,-3.0036611362189));
#39393=CARTESIAN_POINT('Ctrl Pts',(6.02241806591682,49.875,-3.0036611362189));
#39394=CARTESIAN_POINT('Ctrl Pts',(6.07290162599645,57.495,-3.00235671375976));
#39395=CARTESIAN_POINT('Ctrl Pts',(6.07290162599645,49.875,-3.00235671375976));
#39396=CARTESIAN_POINT('Ctrl Pts',(6.12410381716763,57.495,-3.00019778316116));
#39397=CARTESIAN_POINT('Ctrl Pts',(6.12410381716763,49.875,-3.00019778316116));
#39398=CARTESIAN_POINT('Ctrl Pts',(6.17600655789219,57.495,-2.99717295692923));
#39399=CARTESIAN_POINT('Ctrl Pts',(6.17600655789219,49.875,-2.99717295692923));
#39400=CARTESIAN_POINT('Ctrl Pts',(6.22859706400143,57.495,-2.9932755486881));
#39401=CARTESIAN_POINT('Ctrl Pts',(6.22859706400143,49.875,-2.9932755486881));
#39402=CARTESIAN_POINT('Ctrl Pts',(6.28186459845025,57.495,-2.98850417352762));
#39403=CARTESIAN_POINT('Ctrl Pts',(6.28186459845025,49.875,-2.98850417352762));
#39404=CARTESIAN_POINT('Ctrl Pts',(6.33579850967655,57.495,-2.98286238364848));
#39405=CARTESIAN_POINT('Ctrl Pts',(6.33579850967655,49.875,-2.98286238364848));
#39406=CARTESIAN_POINT('Ctrl Pts',(6.39038953466525,57.495,-2.97635619664327));
#39407=CARTESIAN_POINT('Ctrl Pts',(6.39038953466525,49.875,-2.97635619664327));
#39408=CARTESIAN_POINT('Ctrl Pts',(6.43458214159119,57.495,-2.97046502832938));
#39409=CARTESIAN_POINT('Ctrl Pts',(6.43458214159119,49.875,-2.97046502832938));
#39410=CARTESIAN_POINT('Ctrl Pts',(6.4680168144459,57.495,-2.96566304810545));
#39411=CARTESIAN_POINT('Ctrl Pts',(6.4680168144459,49.875,-2.96566304810545));
#39412=CARTESIAN_POINT('Ctrl Pts',(6.49043534784125,57.495,-2.96229154623624));
#39413=CARTESIAN_POINT('Ctrl Pts',(6.49043534784125,49.875,-2.96229154623624));
#39414=CARTESIAN_POINT('Ctrl Pts',(6.5016768024705,57.495,-2.96056324982543));
#39415=CARTESIAN_POINT('Ctrl Pts',(6.5016768024705,49.875,-2.96056324982543));
#39416=CARTESIAN_POINT('',(5.22677443144495,51.145,-2.87862685522557));
#39417=CARTESIAN_POINT('Ctrl Pts',(5.22677443144495,51.145,-2.87862685522557));
#39418=CARTESIAN_POINT('Ctrl Pts',(5.23024117954544,51.145,-2.88043681055508));
#39419=CARTESIAN_POINT('Ctrl Pts',(5.2374521593957,51.145,-2.88406558980908));
#39420=CARTESIAN_POINT('Ctrl Pts',(5.24910109063627,51.145,-2.88953536864324));
#39421=CARTESIAN_POINT('Ctrl Pts',(5.26630084561717,51.145,-2.8968816873652));
#39422=CARTESIAN_POINT('Ctrl Pts',(5.29057828960674,51.145,-2.90614521320845));
#39423=CARTESIAN_POINT('Ctrl Pts',(5.31759510370885,51.145,-2.91546314862894));
#39424=CARTESIAN_POINT('Ctrl Pts',(5.34725389048201,51.145,-2.92478335875772));
#39425=CARTESIAN_POINT('Ctrl Pts',(5.37936310952306,51.145,-2.93401523982667));
#39426=CARTESIAN_POINT('Ctrl Pts',(5.41364129622042,51.145,-2.94303247002252));
#39427=CARTESIAN_POINT('Ctrl Pts',(5.44977003302479,51.145,-2.95169462080126));
#39428=CARTESIAN_POINT('Ctrl Pts',(5.48743586913294,51.145,-2.95986479289849));
#39429=CARTESIAN_POINT('Ctrl Pts',(5.52637191504897,51.145,-2.96742703426686));
#39430=CARTESIAN_POINT('Ctrl Pts',(5.56641026634754,51.145,-2.97430877025614));
#39431=CARTESIAN_POINT('Ctrl Pts',(5.60747882861056,51.145,-2.98047914221006));
#39432=CARTESIAN_POINT('Ctrl Pts',(5.64956501668965,51.145,-2.98593308820275));
#39433=CARTESIAN_POINT('Ctrl Pts',(5.6926888242775,51.145,-2.99067972442542));
#39434=CARTESIAN_POINT('Ctrl Pts',(5.73687442119609,51.145,-2.99473015701059));
#39435=CARTESIAN_POINT('Ctrl Pts',(5.78211642456377,51.145,-2.99808342690941));
#39436=CARTESIAN_POINT('Ctrl Pts',(5.82837721216371,51.145,-3.00072490941926));
#39437=CARTESIAN_POINT('Ctrl Pts',(5.87560110342618,51.145,-3.00263159433907));
#39438=CARTESIAN_POINT('Ctrl Pts',(5.92372322806235,51.145,-3.00377540211876));
#39439=CARTESIAN_POINT('Ctrl Pts',(5.97267956506957,51.145,-3.00412716938112));
#39440=CARTESIAN_POINT('Ctrl Pts',(6.02241806591682,51.145,-3.0036611362189));
#39441=CARTESIAN_POINT('Ctrl Pts',(6.07290162599645,51.145,-3.00235671375976));
#39442=CARTESIAN_POINT('Ctrl Pts',(6.12410381716763,51.145,-3.00019778316116));
#39443=CARTESIAN_POINT('Ctrl Pts',(6.17600655789219,51.145,-2.99717295692923));
#39444=CARTESIAN_POINT('Ctrl Pts',(6.22859706400143,51.145,-2.9932755486881));
#39445=CARTESIAN_POINT('Ctrl Pts',(6.28186459845025,51.145,-2.98850417352762));
#39446=CARTESIAN_POINT('Ctrl Pts',(6.33579850967655,51.145,-2.98286238364848));
#39447=CARTESIAN_POINT('Ctrl Pts',(6.39038953466525,51.145,-2.97635619664327));
#39448=CARTESIAN_POINT('Ctrl Pts',(6.43458214159119,51.145,-2.97046502832938));
#39449=CARTESIAN_POINT('Ctrl Pts',(6.4680168144459,51.145,-2.96566304810545));
#39450=CARTESIAN_POINT('Ctrl Pts',(6.49043534784125,51.145,-2.96229154623624));
#39451=CARTESIAN_POINT('Ctrl Pts',(6.5016768024705,51.145,-2.96056324982543));
#39452=CARTESIAN_POINT('',(5.22677443144495,57.495,-2.87862685522557));
#39453=CARTESIAN_POINT('Origin',(4.56189402049717,57.495,-2.51244640654327));
#39454=CARTESIAN_POINT('',(4.69328497730872,51.145,-2.58480949428933));
#39455=CARTESIAN_POINT('',(4.69328497730872,54.32,-2.58480949428933));
#39456=CARTESIAN_POINT('',(4.56189402049717,51.145,-2.51244640654327));
#39457=CARTESIAN_POINT('Ctrl Pts',(6.6908141061934,57.495,-2.50394540602693));
#39458=CARTESIAN_POINT('Ctrl Pts',(6.6908141061934,49.875,-2.50394540602693));
#39459=CARTESIAN_POINT('Ctrl Pts',(6.6840872875067,57.495,-2.49477440711623));
#39460=CARTESIAN_POINT('Ctrl Pts',(6.6840872875067,49.875,-2.49477440711623));
#39461=CARTESIAN_POINT('Ctrl Pts',(6.67061900235319,57.495,-2.47653809829367));
#39462=CARTESIAN_POINT('Ctrl Pts',(6.67061900235319,49.875,-2.47653809829367));
#39463=CARTESIAN_POINT('Ctrl Pts',(6.65037263123044,57.495,-2.44950070161195));
#39464=CARTESIAN_POINT('Ctrl Pts',(6.65037263123044,49.875,-2.44950070161195));
#39465=CARTESIAN_POINT('Ctrl Pts',(6.62328942425873,57.495,-2.41408612451248));
#39466=CARTESIAN_POINT('Ctrl Pts',(6.62328942425873,49.875,-2.41408612451248));
#39467=CARTESIAN_POINT('Ctrl Pts',(6.58928830924832,57.495,-2.37088387159998));
#39468=CARTESIAN_POINT('Ctrl Pts',(6.58928830924832,49.875,-2.37088387159998));
#39469=CARTESIAN_POINT('Ctrl Pts',(6.55514062276576,57.495,-2.32875748935431));
#39470=CARTESIAN_POINT('Ctrl Pts',(6.55514062276576,49.875,-2.32875748935431));
#39471=CARTESIAN_POINT('Ctrl Pts',(6.52084865967131,57.495,-2.28771778279682));
#39472=CARTESIAN_POINT('Ctrl Pts',(6.52084865967131,49.875,-2.28771778279682));
#39473=CARTESIAN_POINT('Ctrl Pts',(6.48641743997165,57.495,-2.24777479550452));
#39474=CARTESIAN_POINT('Ctrl Pts',(6.48641743997165,49.875,-2.24777479550452));
#39475=CARTESIAN_POINT('Ctrl Pts',(6.45185553518355,57.495,-2.20893514043546));
#39476=CARTESIAN_POINT('Ctrl Pts',(6.45185553518355,49.875,-2.20893514043546));
#39477=CARTESIAN_POINT('Ctrl Pts',(6.41717671306116,57.495,-2.17120312938033));
#39478=CARTESIAN_POINT('Ctrl Pts',(6.41717671306116,49.875,-2.17120312938033));
#39479=CARTESIAN_POINT('Ctrl Pts',(6.38240181135686,57.495,-2.13458349574322));
#39480=CARTESIAN_POINT('Ctrl Pts',(6.38240181135686,49.875,-2.13458349574322));
#39481=CARTESIAN_POINT('Ctrl Pts',(6.34756091533109,57.495,-2.09908352929886));
#39482=CARTESIAN_POINT('Ctrl Pts',(6.34756091533109,49.875,-2.09908352929886));
#39483=CARTESIAN_POINT('Ctrl Pts',(6.31269482043472,57.495,-2.06471490843566));
#39484=CARTESIAN_POINT('Ctrl Pts',(6.31269482043472,49.875,-2.06471490843566));
#39485=CARTESIAN_POINT('Ctrl Pts',(6.27785854554207,57.495,-2.03149622201774));
#39486=CARTESIAN_POINT('Ctrl Pts',(6.27785854554207,49.875,-2.03149622201774));
#39487=CARTESIAN_POINT('Ctrl Pts',(6.24311798195999,57.495,-1.99945211810842));
#39488=CARTESIAN_POINT('Ctrl Pts',(6.24311798195999,49.875,-1.99945211810842));
#39489=CARTESIAN_POINT('Ctrl Pts',(6.20853885514991,57.495,-1.96860861168855));
#39490=CARTESIAN_POINT('Ctrl Pts',(6.20853885514991,49.875,-1.96860861168855));
#39491=CARTESIAN_POINT('Ctrl Pts',(6.17417680788948,57.495,-1.93898880419739));
#39492=CARTESIAN_POINT('Ctrl Pts',(6.17417680788948,49.875,-1.93898880419739));
#39493=CARTESIAN_POINT('Ctrl Pts',(6.14006878432979,57.495,-1.91060895733316));
#39494=CARTESIAN_POINT('Ctrl Pts',(6.14006878432979,49.875,-1.91060895733316));
#39495=CARTESIAN_POINT('Ctrl Pts',(6.10621926889293,57.495,-1.88347219921808));
#39496=CARTESIAN_POINT('Ctrl Pts',(6.10621926889293,49.875,-1.88347219921808));
#39497=CARTESIAN_POINT('Ctrl Pts',(6.07260331771223,57.495,-1.85756929242873));
#39498=CARTESIAN_POINT('Ctrl Pts',(6.07260331771223,49.875,-1.85756929242873));
#39499=CARTESIAN_POINT('Ctrl Pts',(6.03920034699142,57.495,-1.83289254541003));
#39500=CARTESIAN_POINT('Ctrl Pts',(6.03920034699142,49.875,-1.83289254541003));
#39501=CARTESIAN_POINT('Ctrl Pts',(6.00602283509636,57.495,-1.80944727788364));
#39502=CARTESIAN_POINT('Ctrl Pts',(6.00602283509636,49.875,-1.80944727788364));
#39503=CARTESIAN_POINT('Ctrl Pts',(5.97314358084405,57.495,-1.78726264793637));
#39504=CARTESIAN_POINT('Ctrl Pts',(5.97314358084405,49.875,-1.78726264793637));
#39505=CARTESIAN_POINT('Ctrl Pts',(5.94073262861954,57.495,-1.76640606389863));
#39506=CARTESIAN_POINT('Ctrl Pts',(5.94073262861954,49.875,-1.76640606389863));
#39507=CARTESIAN_POINT('Ctrl Pts',(5.90906068827417,57.495,-1.74698425466385));
#39508=CARTESIAN_POINT('Ctrl Pts',(5.90906068827417,49.875,-1.74698425466385));
#39509=CARTESIAN_POINT('Ctrl Pts',(5.87844620539466,57.495,-1.72912206102238));
#39510=CARTESIAN_POINT('Ctrl Pts',(5.87844620539466,49.875,-1.72912206102238));
#39511=CARTESIAN_POINT('Ctrl Pts',(5.84921363316514,57.495,-1.71294534020682));
#39512=CARTESIAN_POINT('Ctrl Pts',(5.84921363316514,49.875,-1.71294534020682));
#39513=CARTESIAN_POINT('Ctrl Pts',(5.8216513201319,57.495,-1.69856379474193));
#39514=CARTESIAN_POINT('Ctrl Pts',(5.8216513201319,49.875,-1.69856379474193));
#39515=CARTESIAN_POINT('Ctrl Pts',(5.79595877235173,57.495,-1.68604879760681));
#39516=CARTESIAN_POINT('Ctrl Pts',(5.79595877235173,49.875,-1.68604879760681));
#39517=CARTESIAN_POINT('Ctrl Pts',(5.77224172513534,57.495,-1.67543235427339));
#39518=CARTESIAN_POINT('Ctrl Pts',(5.77224172513534,49.875,-1.67543235427339));
#39519=CARTESIAN_POINT('Ctrl Pts',(5.75488502996854,57.495,-1.6684649226767));
#39520=CARTESIAN_POINT('Ctrl Pts',(5.75488502996854,49.875,-1.6684649226767));
#39521=CARTESIAN_POINT('Ctrl Pts',(5.74278027398956,57.495,-1.66409560210811));
#39522=CARTESIAN_POINT('Ctrl Pts',(5.74278027398956,49.875,-1.66409560210811));
#39523=CARTESIAN_POINT('Ctrl Pts',(5.73511540682054,57.495,-1.66156260377489));
#39524=CARTESIAN_POINT('Ctrl Pts',(5.73511540682054,49.875,-1.66156260377489));
#39525=CARTESIAN_POINT('Ctrl Pts',(5.73138421404289,57.495,-1.66039107437149));
#39526=CARTESIAN_POINT('Ctrl Pts',(5.73138421404289,49.875,-1.66039107437149));
#39527=CARTESIAN_POINT('Ctrl Pts',(6.6908141061934,51.145,-2.50394540602693));
#39528=CARTESIAN_POINT('Ctrl Pts',(6.6840872875067,51.145,-2.49477440711623));
#39529=CARTESIAN_POINT('Ctrl Pts',(6.67061900235319,51.145,-2.47653809829367));
#39530=CARTESIAN_POINT('Ctrl Pts',(6.65037263123044,51.145,-2.44950070161195));
#39531=CARTESIAN_POINT('Ctrl Pts',(6.62328942425873,51.145,-2.41408612451248));
#39532=CARTESIAN_POINT('Ctrl Pts',(6.58928830924832,51.145,-2.37088387159998));
#39533=CARTESIAN_POINT('Ctrl Pts',(6.55514062276576,51.145,-2.32875748935431));
#39534=CARTESIAN_POINT('Ctrl Pts',(6.52084865967131,51.145,-2.28771778279682));
#39535=CARTESIAN_POINT('Ctrl Pts',(6.48641743997165,51.145,-2.24777479550452));
#39536=CARTESIAN_POINT('Ctrl Pts',(6.45185553518355,51.145,-2.20893514043546));
#39537=CARTESIAN_POINT('Ctrl Pts',(6.41717671306116,51.145,-2.17120312938033));
#39538=CARTESIAN_POINT('Ctrl Pts',(6.38240181135686,51.145,-2.13458349574322));
#39539=CARTESIAN_POINT('Ctrl Pts',(6.34756091533109,51.145,-2.09908352929886));
#39540=CARTESIAN_POINT('Ctrl Pts',(6.31269482043472,51.145,-2.06471490843566));
#39541=CARTESIAN_POINT('Ctrl Pts',(6.27785854554207,51.145,-2.03149622201774));
#39542=CARTESIAN_POINT('Ctrl Pts',(6.24311798195999,51.145,-1.99945211810842));
#39543=CARTESIAN_POINT('Ctrl Pts',(6.20853885514991,51.145,-1.96860861168855));
#39544=CARTESIAN_POINT('Ctrl Pts',(6.17417680788948,51.145,-1.93898880419739));
#39545=CARTESIAN_POINT('Ctrl Pts',(6.14006878432979,51.145,-1.91060895733316));
#39546=CARTESIAN_POINT('Ctrl Pts',(6.10621926889293,51.145,-1.88347219921808));
#39547=CARTESIAN_POINT('Ctrl Pts',(6.07260331771223,51.145,-1.85756929242873));
#39548=CARTESIAN_POINT('Ctrl Pts',(6.03920034699142,51.145,-1.83289254541003));
#39549=CARTESIAN_POINT('Ctrl Pts',(6.00602283509636,51.145,-1.80944727788364));
#39550=CARTESIAN_POINT('Ctrl Pts',(5.97314358084405,51.145,-1.78726264793637));
#39551=CARTESIAN_POINT('Ctrl Pts',(5.94073262861954,51.145,-1.76640606389863));
#39552=CARTESIAN_POINT('Ctrl Pts',(5.90906068827417,51.145,-1.74698425466385));
#39553=CARTESIAN_POINT('Ctrl Pts',(5.87844620539466,51.145,-1.72912206102238));
#39554=CARTESIAN_POINT('Ctrl Pts',(5.84921363316514,51.145,-1.71294534020682));
#39555=CARTESIAN_POINT('Ctrl Pts',(5.8216513201319,51.145,-1.69856379474193));
#39556=CARTESIAN_POINT('Ctrl Pts',(5.79595877235173,51.145,-1.68604879760681));
#39557=CARTESIAN_POINT('Ctrl Pts',(5.77224172513534,51.145,-1.67543235427339));
#39558=CARTESIAN_POINT('Ctrl Pts',(5.75488502996854,51.145,-1.6684649226767));
#39559=CARTESIAN_POINT('Ctrl Pts',(5.74278027398956,51.145,-1.66409560210811));
#39560=CARTESIAN_POINT('Ctrl Pts',(5.73511540682054,51.145,-1.66156260377489));
#39561=CARTESIAN_POINT('Ctrl Pts',(5.73138421404289,51.145,-1.66039107437149));
#39562=CARTESIAN_POINT('Origin',(0.,54.32,0.));
#39563=CARTESIAN_POINT('',(4.18409499139877,51.145,-3.34686616149372));
#39564=CARTESIAN_POINT('Origin',(0.,51.145,0.));
#39565=CARTESIAN_POINT('',(4.18409499139877,54.32,-3.34686616149372));
#39566=CARTESIAN_POINT('Origin',(4.65970441290367,57.495,-3.72730711280926));
#39567=CARTESIAN_POINT('',(4.65970441290367,51.145,-3.72730711280926));
#39568=CARTESIAN_POINT('',(4.65970441290367,51.145,-3.72730711280926));
#39569=CARTESIAN_POINT('',(4.65970441290367,57.495,-3.72730711280926));
#39570=CARTESIAN_POINT('Origin',(1.15136842610855E-12,57.495,-1.15195721078055E-12));
#39571=CARTESIAN_POINT('',(5.22328778611671,51.145,-4.87380761862879));
#39572=CARTESIAN_POINT('',(5.22328778611671,57.495,-4.87380761862879));
#39573=CARTESIAN_POINT('',(4.87380761862879,51.145,-5.22328778611671));
#39574=CARTESIAN_POINT('Origin',(1.15136842610855E-12,51.145,-1.15195721078055E-12));
#39575=CARTESIAN_POINT('',(4.87380761862879,57.495,-5.22328778611671));
#39576=CARTESIAN_POINT('Ctrl Pts',(3.72730711280926,57.495,-4.65970441290368));
#39577=CARTESIAN_POINT('Ctrl Pts',(3.72730711280926,49.875,-4.65970441290368));
#39578=CARTESIAN_POINT('Ctrl Pts',(3.72981733050576,57.495,-4.66270326064961));
#39579=CARTESIAN_POINT('Ctrl Pts',(3.72981733050576,49.875,-4.66270326064961));
#39580=CARTESIAN_POINT('Ctrl Pts',(3.73509073349854,57.495,-4.6688153380502));
#39581=CARTESIAN_POINT('Ctrl Pts',(3.73509073349854,49.875,-4.6688153380502));
#39582=CARTESIAN_POINT('Ctrl Pts',(3.7437597489088,57.495,-4.67832660775297));
#39583=CARTESIAN_POINT('Ctrl Pts',(3.7437597489088,49.875,-4.67832660775297));
#39584=CARTESIAN_POINT('Ctrl Pts',(3.7568389360361,57.495,-4.69169578253142));
#39585=CARTESIAN_POINT('Ctrl Pts',(3.7568389360361,49.875,-4.69169578253142));
#39586=CARTESIAN_POINT('Ctrl Pts',(3.77572337177426,57.495,-4.70954474005187));
#39587=CARTESIAN_POINT('Ctrl Pts',(3.77572337177426,49.875,-4.70954474005187));
#39588=CARTESIAN_POINT('Ctrl Pts',(3.79711783384759,57.495,-4.72849227702429));
#39589=CARTESIAN_POINT('Ctrl Pts',(3.79711783384759,49.875,-4.72849227702429));
#39590=CARTESIAN_POINT('Ctrl Pts',(3.82095228990398,57.495,-4.74845295472311));
#39591=CARTESIAN_POINT('Ctrl Pts',(3.82095228990398,49.875,-4.74845295472311));
#39592=CARTESIAN_POINT('Ctrl Pts',(3.84708445224628,57.495,-4.76926976684248));
#39593=CARTESIAN_POINT('Ctrl Pts',(3.84708445224628,49.875,-4.76926976684248));
#39594=CARTESIAN_POINT('Ctrl Pts',(3.87530262274579,57.495,-4.79071829540097));
#39595=CARTESIAN_POINT('Ctrl Pts',(3.87530262274579,49.875,-4.79071829540097));
#39596=CARTESIAN_POINT('Ctrl Pts',(3.90536636162316,57.495,-4.81254694822028));
#39597=CARTESIAN_POINT('Ctrl Pts',(3.90536636162316,49.875,-4.81254694822028));
#39598=CARTESIAN_POINT('Ctrl Pts',(3.93703846717723,57.495,-4.83450929444277));
#39599=CARTESIAN_POINT('Ctrl Pts',(3.93703846717723,49.875,-4.83450929444277));
#39600=CARTESIAN_POINT('Ctrl Pts',(3.97011673859275,57.495,-4.85639607415679));
#39601=CARTESIAN_POINT('Ctrl Pts',(3.97011673859275,49.875,-4.85639607415679));
#39602=CARTESIAN_POINT('Ctrl Pts',(4.00447382552398,57.495,-4.87807598288661));
#39603=CARTESIAN_POINT('Ctrl Pts',(4.00447382552398,49.875,-4.87807598288661));
#39604=CARTESIAN_POINT('Ctrl Pts',(4.04005493051016,57.495,-4.89949292161193));
#39605=CARTESIAN_POINT('Ctrl Pts',(4.04005493051016,49.875,-4.89949292161193));
#39606=CARTESIAN_POINT('Ctrl Pts',(4.07685036350543,57.495,-4.92063739759527));
#39607=CARTESIAN_POINT('Ctrl Pts',(4.07685036350543,49.875,-4.92063739759527));
#39608=CARTESIAN_POINT('Ctrl Pts',(4.11487510765792,57.495,-4.94152548435404));
#39609=CARTESIAN_POINT('Ctrl Pts',(4.11487510765792,49.875,-4.94152548435404));
#39610=CARTESIAN_POINT('Ctrl Pts',(4.15414724283855,57.495,-4.9621766920072));
#39611=CARTESIAN_POINT('Ctrl Pts',(4.15414724283855,49.875,-4.9621766920072));
#39612=CARTESIAN_POINT('Ctrl Pts',(4.19466216292523,57.495,-4.98258807456953));
#39613=CARTESIAN_POINT('Ctrl Pts',(4.19466216292523,49.875,-4.98258807456953));
#39614=CARTESIAN_POINT('Ctrl Pts',(4.23639070615327,57.495,-5.00273172317852));
#39615=CARTESIAN_POINT('Ctrl Pts',(4.23639070615327,49.875,-5.00273172317852));
#39616=CARTESIAN_POINT('Ctrl Pts',(4.27929023600664,57.495,-5.02256507114883));
#39617=CARTESIAN_POINT('Ctrl Pts',(4.27929023600664,49.875,-5.02256507114883));
#39618=CARTESIAN_POINT('Ctrl Pts',(4.32331156573186,57.495,-5.04203735157409));
#39619=CARTESIAN_POINT('Ctrl Pts',(4.32331156573186,49.875,-5.04203735157409));
#39620=CARTESIAN_POINT('Ctrl Pts',(4.36840670797621,57.495,-5.06109712122993));
#39621=CARTESIAN_POINT('Ctrl Pts',(4.36840670797621,49.875,-5.06109712122993));
#39622=CARTESIAN_POINT('Ctrl Pts',(4.41453743405689,57.495,-5.07970066295481));
#39623=CARTESIAN_POINT('Ctrl Pts',(4.41453743405689,49.875,-5.07970066295481));
#39624=CARTESIAN_POINT('Ctrl Pts',(4.46167734280668,57.495,-5.09781475579234));
#39625=CARTESIAN_POINT('Ctrl Pts',(4.46167734280668,49.875,-5.09781475579234));
#39626=CARTESIAN_POINT('Ctrl Pts',(4.50980818622117,57.495,-5.11541439426219));
#39627=CARTESIAN_POINT('Ctrl Pts',(4.50980818622117,49.875,-5.11541439426219));
#39628=CARTESIAN_POINT('Ctrl Pts',(4.55891761694258,57.495,-5.13248213818673));
#39629=CARTESIAN_POINT('Ctrl Pts',(4.55891761694258,49.875,-5.13248213818673));
#39630=CARTESIAN_POINT('Ctrl Pts',(4.60899638270436,57.495,-5.14900691787061));
#39631=CARTESIAN_POINT('Ctrl Pts',(4.60899638270436,49.875,-5.14900691787061));
#39632=CARTESIAN_POINT('Ctrl Pts',(4.66003509375248,57.495,-5.16498334493441));
#39633=CARTESIAN_POINT('Ctrl Pts',(4.66003509375248,49.875,-5.16498334493441));
#39634=CARTESIAN_POINT('Ctrl Pts',(4.71202254995837,57.495,-5.1804106250073));
#39635=CARTESIAN_POINT('Ctrl Pts',(4.71202254995837,49.875,-5.1804106250073));
#39636=CARTESIAN_POINT('Ctrl Pts',(4.764947890579,57.495,-5.1952907728175));
#39637=CARTESIAN_POINT('Ctrl Pts',(4.764947890579,49.875,-5.1952907728175));
#39638=CARTESIAN_POINT('Ctrl Pts',(4.8080309881172,57.495,-5.2067598214933));
#39639=CARTESIAN_POINT('Ctrl Pts',(4.8080309881172,49.875,-5.2067598214933));
#39640=CARTESIAN_POINT('Ctrl Pts',(4.84075823631811,57.495,-5.21511826561693));
#39641=CARTESIAN_POINT('Ctrl Pts',(4.84075823631811,49.875,-5.21511826561693));
#39642=CARTESIAN_POINT('Ctrl Pts',(4.86276047837853,57.495,-5.22058260535447));
#39643=CARTESIAN_POINT('Ctrl Pts',(4.86276047837853,49.875,-5.22058260535447));
#39644=CARTESIAN_POINT('Ctrl Pts',(4.87380761862879,57.495,-5.22328778611671));
#39645=CARTESIAN_POINT('Ctrl Pts',(4.87380761862879,49.875,-5.22328778611671));
#39646=CARTESIAN_POINT('',(3.72730711280926,51.145,-4.65970441290368));
#39647=CARTESIAN_POINT('Ctrl Pts',(3.72730711280926,51.145,-4.65970441290368));
#39648=CARTESIAN_POINT('Ctrl Pts',(3.72981733050576,51.145,-4.66270326064961));
#39649=CARTESIAN_POINT('Ctrl Pts',(3.73509073349854,51.145,-4.6688153380502));
#39650=CARTESIAN_POINT('Ctrl Pts',(3.7437597489088,51.145,-4.67832660775297));
#39651=CARTESIAN_POINT('Ctrl Pts',(3.7568389360361,51.145,-4.69169578253142));
#39652=CARTESIAN_POINT('Ctrl Pts',(3.77572337177426,51.145,-4.70954474005187));
#39653=CARTESIAN_POINT('Ctrl Pts',(3.79711783384759,51.145,-4.72849227702429));
#39654=CARTESIAN_POINT('Ctrl Pts',(3.82095228990398,51.145,-4.74845295472311));
#39655=CARTESIAN_POINT('Ctrl Pts',(3.84708445224628,51.145,-4.76926976684248));
#39656=CARTESIAN_POINT('Ctrl Pts',(3.87530262274579,51.145,-4.79071829540097));
#39657=CARTESIAN_POINT('Ctrl Pts',(3.90536636162316,51.145,-4.81254694822028));
#39658=CARTESIAN_POINT('Ctrl Pts',(3.93703846717723,51.145,-4.83450929444277));
#39659=CARTESIAN_POINT('Ctrl Pts',(3.97011673859275,51.145,-4.85639607415679));
#39660=CARTESIAN_POINT('Ctrl Pts',(4.00447382552398,51.145,-4.87807598288661));
#39661=CARTESIAN_POINT('Ctrl Pts',(4.04005493051016,51.145,-4.89949292161193));
#39662=CARTESIAN_POINT('Ctrl Pts',(4.07685036350543,51.145,-4.92063739759527));
#39663=CARTESIAN_POINT('Ctrl Pts',(4.11487510765792,51.145,-4.94152548435404));
#39664=CARTESIAN_POINT('Ctrl Pts',(4.15414724283855,51.145,-4.9621766920072));
#39665=CARTESIAN_POINT('Ctrl Pts',(4.19466216292523,51.145,-4.98258807456953));
#39666=CARTESIAN_POINT('Ctrl Pts',(4.23639070615327,51.145,-5.00273172317852));
#39667=CARTESIAN_POINT('Ctrl Pts',(4.27929023600664,51.145,-5.02256507114883));
#39668=CARTESIAN_POINT('Ctrl Pts',(4.32331156573186,51.145,-5.04203735157409));
#39669=CARTESIAN_POINT('Ctrl Pts',(4.36840670797621,51.145,-5.06109712122993));
#39670=CARTESIAN_POINT('Ctrl Pts',(4.41453743405689,51.145,-5.07970066295481));
#39671=CARTESIAN_POINT('Ctrl Pts',(4.46167734280668,51.145,-5.09781475579234));
#39672=CARTESIAN_POINT('Ctrl Pts',(4.50980818622117,51.145,-5.11541439426219));
#39673=CARTESIAN_POINT('Ctrl Pts',(4.55891761694258,51.145,-5.13248213818673));
#39674=CARTESIAN_POINT('Ctrl Pts',(4.60899638270436,51.145,-5.14900691787061));
#39675=CARTESIAN_POINT('Ctrl Pts',(4.66003509375248,51.145,-5.16498334493441));
#39676=CARTESIAN_POINT('Ctrl Pts',(4.71202254995837,51.145,-5.1804106250073));
#39677=CARTESIAN_POINT('Ctrl Pts',(4.764947890579,51.145,-5.1952907728175));
#39678=CARTESIAN_POINT('Ctrl Pts',(4.8080309881172,51.145,-5.2067598214933));
#39679=CARTESIAN_POINT('Ctrl Pts',(4.84075823631811,51.145,-5.21511826561693));
#39680=CARTESIAN_POINT('Ctrl Pts',(4.86276047837853,51.145,-5.22058260535447));
#39681=CARTESIAN_POINT('Ctrl Pts',(4.87380761862879,51.145,-5.22328778611671));
#39682=CARTESIAN_POINT('',(3.72730711280926,57.495,-4.65970441290368));
#39683=CARTESIAN_POINT('Origin',(3.25316890053365,57.495,-4.06695907338649));
#39684=CARTESIAN_POINT('',(3.34686616149372,51.145,-4.18409499139877));
#39685=CARTESIAN_POINT('',(3.34686616149372,54.32,-4.18409499139877));
#39686=CARTESIAN_POINT('',(3.25316890053365,51.145,-4.06695907338649));
#39687=CARTESIAN_POINT('Ctrl Pts',(5.22328778611671,57.495,-4.87380761862879));
#39688=CARTESIAN_POINT('Ctrl Pts',(5.22328778611671,49.875,-4.87380761862879));
#39689=CARTESIAN_POINT('Ctrl Pts',(5.2205826053545,57.495,-4.86276047837859));
#39690=CARTESIAN_POINT('Ctrl Pts',(5.2205826053545,49.875,-4.86276047837859));
#39691=CARTESIAN_POINT('Ctrl Pts',(5.21511826561704,57.495,-4.84075823631826));
#39692=CARTESIAN_POINT('Ctrl Pts',(5.21511826561704,49.875,-4.84075823631826));
#39693=CARTESIAN_POINT('Ctrl Pts',(5.20675982149348,57.495,-4.80803098811744));
#39694=CARTESIAN_POINT('Ctrl Pts',(5.20675982149348,49.875,-4.80803098811744));
#39695=CARTESIAN_POINT('Ctrl Pts',(5.19529077281773,57.495,-4.7649478905793));
#39696=CARTESIAN_POINT('Ctrl Pts',(5.19529077281773,49.875,-4.7649478905793));
#39697=CARTESIAN_POINT('Ctrl Pts',(5.18041062500752,57.495,-4.71202254995864));
#39698=CARTESIAN_POINT('Ctrl Pts',(5.18041062500752,49.875,-4.71202254995864));
#39699=CARTESIAN_POINT('Ctrl Pts',(5.16498334493456,57.495,-4.66003509375265));
#39700=CARTESIAN_POINT('Ctrl Pts',(5.16498334493456,49.875,-4.66003509375265));
#39701=CARTESIAN_POINT('Ctrl Pts',(5.14900691787064,57.495,-4.60899638270439));
#39702=CARTESIAN_POINT('Ctrl Pts',(5.14900691787064,49.875,-4.60899638270439));
#39703=CARTESIAN_POINT('Ctrl Pts',(5.13248213818666,57.495,-4.5589176169425));
#39704=CARTESIAN_POINT('Ctrl Pts',(5.13248213818666,49.875,-4.5589176169425));
#39705=CARTESIAN_POINT('Ctrl Pts',(5.11541439426204,57.495,-4.50980818622101));
#39706=CARTESIAN_POINT('Ctrl Pts',(5.11541439426204,49.875,-4.50980818622101));
#39707=CARTESIAN_POINT('Ctrl Pts',(5.09781475579217,57.495,-4.46167734280651));
#39708=CARTESIAN_POINT('Ctrl Pts',(5.09781475579217,49.875,-4.46167734280651));
#39709=CARTESIAN_POINT('Ctrl Pts',(5.07970066295468,57.495,-4.41453743405677));
#39710=CARTESIAN_POINT('Ctrl Pts',(5.07970066295468,49.875,-4.41453743405677));
#39711=CARTESIAN_POINT('Ctrl Pts',(5.06109712122989,57.495,-4.36840670797617));
#39712=CARTESIAN_POINT('Ctrl Pts',(5.06109712122989,49.875,-4.36840670797617));
#39713=CARTESIAN_POINT('Ctrl Pts',(5.04203735157413,57.495,-4.3233115657319));
#39714=CARTESIAN_POINT('Ctrl Pts',(5.04203735157413,49.875,-4.3233115657319));
#39715=CARTESIAN_POINT('Ctrl Pts',(5.02256507114894,57.495,-4.27929023600674));
#39716=CARTESIAN_POINT('Ctrl Pts',(5.02256507114894,49.875,-4.27929023600674));
#39717=CARTESIAN_POINT('Ctrl Pts',(5.00273172317863,57.495,-4.23639070615337));
#39718=CARTESIAN_POINT('Ctrl Pts',(5.00273172317863,49.875,-4.23639070615337));
#39719=CARTESIAN_POINT('Ctrl Pts',(4.98258807456962,57.495,-4.1946621629253));
#39720=CARTESIAN_POINT('Ctrl Pts',(4.98258807456962,49.875,-4.1946621629253));
#39721=CARTESIAN_POINT('Ctrl Pts',(4.96217669200723,57.495,-4.15414724283858));
#39722=CARTESIAN_POINT('Ctrl Pts',(4.96217669200723,49.875,-4.15414724283858));
#39723=CARTESIAN_POINT('Ctrl Pts',(4.94152548435402,57.495,-4.11487510765791));
#39724=CARTESIAN_POINT('Ctrl Pts',(4.94152548435402,49.875,-4.11487510765791));
#39725=CARTESIAN_POINT('Ctrl Pts',(4.92063739759521,57.495,-4.07685036350539));
#39726=CARTESIAN_POINT('Ctrl Pts',(4.92063739759521,49.875,-4.07685036350539));
#39727=CARTESIAN_POINT('Ctrl Pts',(4.89949292161185,57.495,-4.04005493051012));
#39728=CARTESIAN_POINT('Ctrl Pts',(4.89949292161185,49.875,-4.04005493051012));
#39729=CARTESIAN_POINT('Ctrl Pts',(4.87807598288654,57.495,-4.00447382552396));
#39730=CARTESIAN_POINT('Ctrl Pts',(4.87807598288654,49.875,-4.00447382552396));
#39731=CARTESIAN_POINT('Ctrl Pts',(4.85639607415676,57.495,-3.97011673859274));
#39732=CARTESIAN_POINT('Ctrl Pts',(4.85639607415676,49.875,-3.97011673859274));
#39733=CARTESIAN_POINT('Ctrl Pts',(4.83450929444279,57.495,-3.93703846717724));
#39734=CARTESIAN_POINT('Ctrl Pts',(4.83450929444279,49.875,-3.93703846717724));
#39735=CARTESIAN_POINT('Ctrl Pts',(4.81254694822034,57.495,-3.90536636162318));
#39736=CARTESIAN_POINT('Ctrl Pts',(4.81254694822034,49.875,-3.90536636162318));
#39737=CARTESIAN_POINT('Ctrl Pts',(4.79071829540103,57.495,-3.8753026227458));
#39738=CARTESIAN_POINT('Ctrl Pts',(4.79071829540103,49.875,-3.8753026227458));
#39739=CARTESIAN_POINT('Ctrl Pts',(4.76926976684252,57.495,-3.84708445224627));
#39740=CARTESIAN_POINT('Ctrl Pts',(4.76926976684252,49.875,-3.84708445224627));
#39741=CARTESIAN_POINT('Ctrl Pts',(4.74845295472312,57.495,-3.82095228990397));
#39742=CARTESIAN_POINT('Ctrl Pts',(4.74845295472312,49.875,-3.82095228990397));
#39743=CARTESIAN_POINT('Ctrl Pts',(4.72849227702427,57.495,-3.7971178338476));
#39744=CARTESIAN_POINT('Ctrl Pts',(4.72849227702427,49.875,-3.7971178338476));
#39745=CARTESIAN_POINT('Ctrl Pts',(4.7095447400518,57.495,-3.77572337177431));
#39746=CARTESIAN_POINT('Ctrl Pts',(4.7095447400518,49.875,-3.77572337177431));
#39747=CARTESIAN_POINT('Ctrl Pts',(4.69169578253132,57.495,-3.75683893603616));
#39748=CARTESIAN_POINT('Ctrl Pts',(4.69169578253132,49.875,-3.75683893603616));
#39749=CARTESIAN_POINT('Ctrl Pts',(4.67832660775287,57.495,-3.74375974890886));
#39750=CARTESIAN_POINT('Ctrl Pts',(4.67832660775287,49.875,-3.74375974890886));
#39751=CARTESIAN_POINT('Ctrl Pts',(4.66881533805013,57.495,-3.73509073349858));
#39752=CARTESIAN_POINT('Ctrl Pts',(4.66881533805013,49.875,-3.73509073349858));
#39753=CARTESIAN_POINT('Ctrl Pts',(4.66270326064959,57.495,-3.72981733050578));
#39754=CARTESIAN_POINT('Ctrl Pts',(4.66270326064959,49.875,-3.72981733050578));
#39755=CARTESIAN_POINT('Ctrl Pts',(4.65970441290367,57.495,-3.72730711280926));
#39756=CARTESIAN_POINT('Ctrl Pts',(4.65970441290367,49.875,-3.72730711280926));
#39757=CARTESIAN_POINT('Ctrl Pts',(5.22328778611671,51.145,-4.87380761862879));
#39758=CARTESIAN_POINT('Ctrl Pts',(5.2205826053545,51.145,-4.86276047837859));
#39759=CARTESIAN_POINT('Ctrl Pts',(5.21511826561704,51.145,-4.84075823631826));
#39760=CARTESIAN_POINT('Ctrl Pts',(5.20675982149348,51.145,-4.80803098811744));
#39761=CARTESIAN_POINT('Ctrl Pts',(5.19529077281773,51.145,-4.7649478905793));
#39762=CARTESIAN_POINT('Ctrl Pts',(5.18041062500752,51.145,-4.71202254995864));
#39763=CARTESIAN_POINT('Ctrl Pts',(5.16498334493456,51.145,-4.66003509375265));
#39764=CARTESIAN_POINT('Ctrl Pts',(5.14900691787064,51.145,-4.60899638270439));
#39765=CARTESIAN_POINT('Ctrl Pts',(5.13248213818666,51.145,-4.5589176169425));
#39766=CARTESIAN_POINT('Ctrl Pts',(5.11541439426204,51.145,-4.50980818622101));
#39767=CARTESIAN_POINT('Ctrl Pts',(5.09781475579217,51.145,-4.46167734280651));
#39768=CARTESIAN_POINT('Ctrl Pts',(5.07970066295468,51.145,-4.41453743405677));
#39769=CARTESIAN_POINT('Ctrl Pts',(5.06109712122989,51.145,-4.36840670797617));
#39770=CARTESIAN_POINT('Ctrl Pts',(5.04203735157413,51.145,-4.3233115657319));
#39771=CARTESIAN_POINT('Ctrl Pts',(5.02256507114894,51.145,-4.27929023600674));
#39772=CARTESIAN_POINT('Ctrl Pts',(5.00273172317863,51.145,-4.23639070615337));
#39773=CARTESIAN_POINT('Ctrl Pts',(4.98258807456962,51.145,-4.1946621629253));
#39774=CARTESIAN_POINT('Ctrl Pts',(4.96217669200723,51.145,-4.15414724283858));
#39775=CARTESIAN_POINT('Ctrl Pts',(4.94152548435402,51.145,-4.11487510765791));
#39776=CARTESIAN_POINT('Ctrl Pts',(4.92063739759521,51.145,-4.07685036350539));
#39777=CARTESIAN_POINT('Ctrl Pts',(4.89949292161185,51.145,-4.04005493051012));
#39778=CARTESIAN_POINT('Ctrl Pts',(4.87807598288654,51.145,-4.00447382552396));
#39779=CARTESIAN_POINT('Ctrl Pts',(4.85639607415676,51.145,-3.97011673859274));
#39780=CARTESIAN_POINT('Ctrl Pts',(4.83450929444279,51.145,-3.93703846717724));
#39781=CARTESIAN_POINT('Ctrl Pts',(4.81254694822034,51.145,-3.90536636162318));
#39782=CARTESIAN_POINT('Ctrl Pts',(4.79071829540103,51.145,-3.8753026227458));
#39783=CARTESIAN_POINT('Ctrl Pts',(4.76926976684252,51.145,-3.84708445224627));
#39784=CARTESIAN_POINT('Ctrl Pts',(4.74845295472312,51.145,-3.82095228990397));
#39785=CARTESIAN_POINT('Ctrl Pts',(4.72849227702427,51.145,-3.7971178338476));
#39786=CARTESIAN_POINT('Ctrl Pts',(4.7095447400518,51.145,-3.77572337177431));
#39787=CARTESIAN_POINT('Ctrl Pts',(4.69169578253132,51.145,-3.75683893603616));
#39788=CARTESIAN_POINT('Ctrl Pts',(4.67832660775287,51.145,-3.74375974890886));
#39789=CARTESIAN_POINT('Ctrl Pts',(4.66881533805013,51.145,-3.73509073349858));
#39790=CARTESIAN_POINT('Ctrl Pts',(4.66270326064959,51.145,-3.72981733050578));
#39791=CARTESIAN_POINT('Ctrl Pts',(4.65970441290367,51.145,-3.72730711280926));
#39792=CARTESIAN_POINT('Origin',(0.,54.32,0.));
#39793=CARTESIAN_POINT('',(2.58480949428932,51.145,-4.69328497730873));
#39794=CARTESIAN_POINT('Origin',(0.,51.145,0.));
#39795=CARTESIAN_POINT('',(2.58480949428932,54.32,-4.69328497730873));
#39796=CARTESIAN_POINT('Origin',(2.87862685522556,57.495,-5.22677443144495));
#39797=CARTESIAN_POINT('',(2.87862685522556,51.145,-5.22677443144495));
#39798=CARTESIAN_POINT('',(2.87862685522556,51.145,-5.22677443144495));
#39799=CARTESIAN_POINT('',(2.87862685522556,57.495,-5.22677443144495));
#39800=CARTESIAN_POINT('Origin',(6.22890783902202E-13,57.495,-1.50487931058895E-12));
#39801=CARTESIAN_POINT('',(2.96056324982543,51.145,-6.50167680247051));
#39802=CARTESIAN_POINT('',(2.96056324982543,57.495,-6.50167680247051));
#39803=CARTESIAN_POINT('',(2.50394540602692,51.145,-6.69081410619341));
#39804=CARTESIAN_POINT('Origin',(6.22890783902202E-13,51.145,-1.50487931058895E-12));
#39805=CARTESIAN_POINT('',(2.50394540602692,57.495,-6.69081410619341));
#39806=CARTESIAN_POINT('Ctrl Pts',(1.66039107437148,57.495,-5.73138421404289));
#39807=CARTESIAN_POINT('Ctrl Pts',(1.66039107437148,49.875,-5.73138421404289));
#39808=CARTESIAN_POINT('Ctrl Pts',(1.66156260377487,57.495,-5.73511540682056));
#39809=CARTESIAN_POINT('Ctrl Pts',(1.66156260377487,49.875,-5.73511540682056));
#39810=CARTESIAN_POINT('Ctrl Pts',(1.66409560210805,57.495,-5.7427802739896));
#39811=CARTESIAN_POINT('Ctrl Pts',(1.66409560210805,49.875,-5.7427802739896));
#39812=CARTESIAN_POINT('Ctrl Pts',(1.6684649226766,57.495,-5.75488502996861));
#39813=CARTESIAN_POINT('Ctrl Pts',(1.6684649226766,49.875,-5.75488502996861));
#39814=CARTESIAN_POINT('Ctrl Pts',(1.67543235427329,57.495,-5.77224172513541));
#39815=CARTESIAN_POINT('Ctrl Pts',(1.67543235427329,49.875,-5.77224172513541));
#39816=CARTESIAN_POINT('Ctrl Pts',(1.68604879760674,57.495,-5.79595877235177));
#39817=CARTESIAN_POINT('Ctrl Pts',(1.68604879760674,49.875,-5.79595877235177));
#39818=CARTESIAN_POINT('Ctrl Pts',(1.69856379474191,57.495,-5.82165132013192));
#39819=CARTESIAN_POINT('Ctrl Pts',(1.69856379474191,49.875,-5.82165132013192));
#39820=CARTESIAN_POINT('Ctrl Pts',(1.71294534020683,57.495,-5.84921363316513));
#39821=CARTESIAN_POINT('Ctrl Pts',(1.71294534020683,49.875,-5.84921363316513));
#39822=CARTESIAN_POINT('Ctrl Pts',(1.7291220610224,57.495,-5.87844620539462));
#39823=CARTESIAN_POINT('Ctrl Pts',(1.7291220610224,49.875,-5.87844620539462));
#39824=CARTESIAN_POINT('Ctrl Pts',(1.74698425466387,57.495,-5.90906068827411));
#39825=CARTESIAN_POINT('Ctrl Pts',(1.74698425466387,49.875,-5.90906068827411));
#39826=CARTESIAN_POINT('Ctrl Pts',(1.76640606389864,57.495,-5.94073262861949));
#39827=CARTESIAN_POINT('Ctrl Pts',(1.76640606389864,49.875,-5.94073262861949));
#39828=CARTESIAN_POINT('Ctrl Pts',(1.78726264793636,57.495,-5.97314358084403));
#39829=CARTESIAN_POINT('Ctrl Pts',(1.78726264793636,49.875,-5.97314358084403));
#39830=CARTESIAN_POINT('Ctrl Pts',(1.80944727788364,57.495,-6.00602283509639));
#39831=CARTESIAN_POINT('Ctrl Pts',(1.80944727788364,49.875,-6.00602283509639));
#39832=CARTESIAN_POINT('Ctrl Pts',(1.83289254541003,57.495,-6.03920034699149));
#39833=CARTESIAN_POINT('Ctrl Pts',(1.83289254541003,49.875,-6.03920034699149));
#39834=CARTESIAN_POINT('Ctrl Pts',(1.85756929242873,57.495,-6.07260331771232));
#39835=CARTESIAN_POINT('Ctrl Pts',(1.85756929242873,49.875,-6.07260331771232));
#39836=CARTESIAN_POINT('Ctrl Pts',(1.88347219921808,57.495,-6.106219268893));
#39837=CARTESIAN_POINT('Ctrl Pts',(1.88347219921808,49.875,-6.106219268893));
#39838=CARTESIAN_POINT('Ctrl Pts',(1.91060895733316,57.495,-6.14006878432982));
#39839=CARTESIAN_POINT('Ctrl Pts',(1.91060895733316,49.875,-6.14006878432982));
#39840=CARTESIAN_POINT('Ctrl Pts',(1.93898880419737,57.495,-6.17417680788945));
#39841=CARTESIAN_POINT('Ctrl Pts',(1.93898880419737,49.875,-6.17417680788945));
#39842=CARTESIAN_POINT('Ctrl Pts',(1.96860861168851,57.495,-6.20853885514981));
#39843=CARTESIAN_POINT('Ctrl Pts',(1.96860861168851,49.875,-6.20853885514981));
#39844=CARTESIAN_POINT('Ctrl Pts',(1.99945211810836,57.495,-6.24311798195985));
#39845=CARTESIAN_POINT('Ctrl Pts',(1.99945211810836,49.875,-6.24311798195985));
#39846=CARTESIAN_POINT('Ctrl Pts',(2.03149622201768,57.495,-6.27785854554194));
#39847=CARTESIAN_POINT('Ctrl Pts',(2.03149622201768,49.875,-6.27785854554194));
#39848=CARTESIAN_POINT('Ctrl Pts',(2.06471490843563,57.495,-6.31269482043467));
#39849=CARTESIAN_POINT('Ctrl Pts',(2.06471490843563,49.875,-6.31269482043467));
#39850=CARTESIAN_POINT('Ctrl Pts',(2.09908352929888,57.495,-6.34756091533115));
#39851=CARTESIAN_POINT('Ctrl Pts',(2.09908352929888,49.875,-6.34756091533115));
#39852=CARTESIAN_POINT('Ctrl Pts',(2.13458349574329,57.495,-6.38240181135703));
#39853=CARTESIAN_POINT('Ctrl Pts',(2.13458349574329,49.875,-6.38240181135703));
#39854=CARTESIAN_POINT('Ctrl Pts',(2.17120312938042,57.495,-6.41717671306138));
#39855=CARTESIAN_POINT('Ctrl Pts',(2.17120312938042,49.875,-6.41717671306138));
#39856=CARTESIAN_POINT('Ctrl Pts',(2.20893514043555,57.495,-6.45185553518375));
#39857=CARTESIAN_POINT('Ctrl Pts',(2.20893514043555,49.875,-6.45185553518375));
#39858=CARTESIAN_POINT('Ctrl Pts',(2.24777479550457,57.495,-6.48641743997175));
#39859=CARTESIAN_POINT('Ctrl Pts',(2.24777479550457,49.875,-6.48641743997175));
#39860=CARTESIAN_POINT('Ctrl Pts',(2.2877177827968,57.495,-6.52084865967127));
#39861=CARTESIAN_POINT('Ctrl Pts',(2.2877177827968,49.875,-6.52084865967127));
#39862=CARTESIAN_POINT('Ctrl Pts',(2.3287574893542,57.495,-6.55514062276556));
#39863=CARTESIAN_POINT('Ctrl Pts',(2.3287574893542,49.875,-6.55514062276556));
#39864=CARTESIAN_POINT('Ctrl Pts',(2.37088387159981,57.495,-6.58928830924802));
#39865=CARTESIAN_POINT('Ctrl Pts',(2.37088387159981,49.875,-6.58928830924802));
#39866=CARTESIAN_POINT('Ctrl Pts',(2.41408612451229,57.495,-6.6232894242584));
#39867=CARTESIAN_POINT('Ctrl Pts',(2.41408612451229,49.875,-6.6232894242584));
#39868=CARTESIAN_POINT('Ctrl Pts',(2.4495007016118,57.495,-6.65037263123018));
#39869=CARTESIAN_POINT('Ctrl Pts',(2.4495007016118,49.875,-6.65037263123018));
#39870=CARTESIAN_POINT('Ctrl Pts',(2.47653809829358,57.495,-6.67061900235304));
#39871=CARTESIAN_POINT('Ctrl Pts',(2.47653809829358,49.875,-6.67061900235304));
#39872=CARTESIAN_POINT('Ctrl Pts',(2.49477440711619,57.495,-6.68408728750665));
#39873=CARTESIAN_POINT('Ctrl Pts',(2.49477440711619,49.875,-6.68408728750665));
#39874=CARTESIAN_POINT('Ctrl Pts',(2.50394540602692,57.495,-6.69081410619341));
#39875=CARTESIAN_POINT('Ctrl Pts',(2.50394540602692,49.875,-6.69081410619341));
#39876=CARTESIAN_POINT('',(1.66039107437148,51.145,-5.73138421404289));
#39877=CARTESIAN_POINT('Ctrl Pts',(1.66039107437148,51.145,-5.73138421404289));
#39878=CARTESIAN_POINT('Ctrl Pts',(1.66156260377487,51.145,-5.73511540682056));
#39879=CARTESIAN_POINT('Ctrl Pts',(1.66409560210805,51.145,-5.7427802739896));
#39880=CARTESIAN_POINT('Ctrl Pts',(1.6684649226766,51.145,-5.75488502996861));
#39881=CARTESIAN_POINT('Ctrl Pts',(1.67543235427329,51.145,-5.77224172513541));
#39882=CARTESIAN_POINT('Ctrl Pts',(1.68604879760674,51.145,-5.79595877235177));
#39883=CARTESIAN_POINT('Ctrl Pts',(1.69856379474191,51.145,-5.82165132013192));
#39884=CARTESIAN_POINT('Ctrl Pts',(1.71294534020683,51.145,-5.84921363316513));
#39885=CARTESIAN_POINT('Ctrl Pts',(1.7291220610224,51.145,-5.87844620539462));
#39886=CARTESIAN_POINT('Ctrl Pts',(1.74698425466387,51.145,-5.90906068827411));
#39887=CARTESIAN_POINT('Ctrl Pts',(1.76640606389864,51.145,-5.94073262861949));
#39888=CARTESIAN_POINT('Ctrl Pts',(1.78726264793636,51.145,-5.97314358084403));
#39889=CARTESIAN_POINT('Ctrl Pts',(1.80944727788364,51.145,-6.00602283509639));
#39890=CARTESIAN_POINT('Ctrl Pts',(1.83289254541003,51.145,-6.03920034699149));
#39891=CARTESIAN_POINT('Ctrl Pts',(1.85756929242873,51.145,-6.07260331771232));
#39892=CARTESIAN_POINT('Ctrl Pts',(1.88347219921808,51.145,-6.106219268893));
#39893=CARTESIAN_POINT('Ctrl Pts',(1.91060895733316,51.145,-6.14006878432982));
#39894=CARTESIAN_POINT('Ctrl Pts',(1.93898880419737,51.145,-6.17417680788945));
#39895=CARTESIAN_POINT('Ctrl Pts',(1.96860861168851,51.145,-6.20853885514981));
#39896=CARTESIAN_POINT('Ctrl Pts',(1.99945211810836,51.145,-6.24311798195985));
#39897=CARTESIAN_POINT('Ctrl Pts',(2.03149622201768,51.145,-6.27785854554194));
#39898=CARTESIAN_POINT('Ctrl Pts',(2.06471490843563,51.145,-6.31269482043467));
#39899=CARTESIAN_POINT('Ctrl Pts',(2.09908352929888,51.145,-6.34756091533115));
#39900=CARTESIAN_POINT('Ctrl Pts',(2.13458349574329,51.145,-6.38240181135703));
#39901=CARTESIAN_POINT('Ctrl Pts',(2.17120312938042,51.145,-6.41717671306138));
#39902=CARTESIAN_POINT('Ctrl Pts',(2.20893514043555,51.145,-6.45185553518375));
#39903=CARTESIAN_POINT('Ctrl Pts',(2.24777479550457,51.145,-6.48641743997175));
#39904=CARTESIAN_POINT('Ctrl Pts',(2.2877177827968,51.145,-6.52084865967127));
#39905=CARTESIAN_POINT('Ctrl Pts',(2.3287574893542,51.145,-6.55514062276556));
#39906=CARTESIAN_POINT('Ctrl Pts',(2.37088387159981,51.145,-6.58928830924802));
#39907=CARTESIAN_POINT('Ctrl Pts',(2.41408612451229,51.145,-6.6232894242584));
#39908=CARTESIAN_POINT('Ctrl Pts',(2.4495007016118,51.145,-6.65037263123018));
#39909=CARTESIAN_POINT('Ctrl Pts',(2.47653809829358,51.145,-6.67061900235304));
#39910=CARTESIAN_POINT('Ctrl Pts',(2.49477440711619,51.145,-6.68408728750665));
#39911=CARTESIAN_POINT('Ctrl Pts',(2.50394540602692,51.145,-6.69081410619341));
#39912=CARTESIAN_POINT('',(1.66039107437148,57.495,-5.73138421404289));
#39913=CARTESIAN_POINT('Origin',(1.44917830551339,57.495,-5.00231408838243));
#39914=CARTESIAN_POINT('',(1.4909173120086,51.145,-5.1463899549833));
#39915=CARTESIAN_POINT('',(1.4909173120086,54.32,-5.1463899549833));
#39916=CARTESIAN_POINT('',(1.44917830551339,51.145,-5.00231408838243));
#39917=CARTESIAN_POINT('Ctrl Pts',(2.96056324982543,57.495,-6.50167680247051));
#39918=CARTESIAN_POINT('Ctrl Pts',(2.96056324982543,49.875,-6.50167680247051));
#39919=CARTESIAN_POINT('Ctrl Pts',(2.96229154623625,57.495,-6.49043534784131));
#39920=CARTESIAN_POINT('Ctrl Pts',(2.96229154623625,49.875,-6.49043534784131));
#39921=CARTESIAN_POINT('Ctrl Pts',(2.96566304810549,57.495,-6.46801681444607));
#39922=CARTESIAN_POINT('Ctrl Pts',(2.96566304810549,49.875,-6.46801681444607));
#39923=CARTESIAN_POINT('Ctrl Pts',(2.97046502832945,57.495,-6.43458214159149));
#39924=CARTESIAN_POINT('Ctrl Pts',(2.97046502832945,49.875,-6.43458214159149));
#39925=CARTESIAN_POINT('Ctrl Pts',(2.97635619664337,57.495,-6.39038953466561));
#39926=CARTESIAN_POINT('Ctrl Pts',(2.97635619664337,49.875,-6.39038953466561));
#39927=CARTESIAN_POINT('Ctrl Pts',(2.98286238364857,57.495,-6.33579850967689));
#39928=CARTESIAN_POINT('Ctrl Pts',(2.98286238364857,49.875,-6.33579850967689));
#39929=CARTESIAN_POINT('Ctrl Pts',(2.98850417352769,57.495,-6.28186459845047));
#39930=CARTESIAN_POINT('Ctrl Pts',(2.98850417352769,49.875,-6.28186459845047));
#39931=CARTESIAN_POINT('Ctrl Pts',(2.99327554868811,57.495,-6.22859706400148));
#39932=CARTESIAN_POINT('Ctrl Pts',(2.99327554868811,49.875,-6.22859706400148));
#39933=CARTESIAN_POINT('Ctrl Pts',(2.99717295692919,57.495,-6.17600655789209));
#39934=CARTESIAN_POINT('Ctrl Pts',(2.99717295692919,49.875,-6.17600655789209));
#39935=CARTESIAN_POINT('Ctrl Pts',(3.00019778316108,57.495,-6.12410381716742));
#39936=CARTESIAN_POINT('Ctrl Pts',(3.00019778316108,49.875,-6.12410381716742));
#39937=CARTESIAN_POINT('Ctrl Pts',(3.00235671375967,57.495,-6.07290162599622));
#39938=CARTESIAN_POINT('Ctrl Pts',(3.00235671375967,49.875,-6.07290162599622));
#39939=CARTESIAN_POINT('Ctrl Pts',(3.00366113621882,57.495,-6.02241806591666));
#39940=CARTESIAN_POINT('Ctrl Pts',(3.00366113621882,49.875,-6.02241806591666));
#39941=CARTESIAN_POINT('Ctrl Pts',(3.00412716938109,57.495,-5.97267956506952));
#39942=CARTESIAN_POINT('Ctrl Pts',(3.00412716938109,49.875,-5.97267956506952));
#39943=CARTESIAN_POINT('Ctrl Pts',(3.00377540211877,57.495,-5.9237232280624));
#39944=CARTESIAN_POINT('Ctrl Pts',(3.00377540211877,49.875,-5.9237232280624));
#39945=CARTESIAN_POINT('Ctrl Pts',(3.00263159433912,57.495,-5.87560110342631));
#39946=CARTESIAN_POINT('Ctrl Pts',(3.00263159433912,49.875,-5.87560110342631));
#39947=CARTESIAN_POINT('Ctrl Pts',(3.00072490941932,57.495,-5.82837721216385));
#39948=CARTESIAN_POINT('Ctrl Pts',(3.00072490941932,49.875,-5.82837721216385));
#39949=CARTESIAN_POINT('Ctrl Pts',(2.99808342690946,57.495,-5.78211642456387));
#39950=CARTESIAN_POINT('Ctrl Pts',(2.99808342690946,49.875,-5.78211642456387));
#39951=CARTESIAN_POINT('Ctrl Pts',(2.9947301570106,57.495,-5.73687442119613));
#39952=CARTESIAN_POINT('Ctrl Pts',(2.9947301570106,49.875,-5.73687442119613));
#39953=CARTESIAN_POINT('Ctrl Pts',(2.9906797244254,57.495,-5.69268882427748));
#39954=CARTESIAN_POINT('Ctrl Pts',(2.9906797244254,49.875,-5.69268882427748));
#39955=CARTESIAN_POINT('Ctrl Pts',(2.98593308820271,57.495,-5.64956501668959));
#39956=CARTESIAN_POINT('Ctrl Pts',(2.98593308820271,49.875,-5.64956501668959));
#39957=CARTESIAN_POINT('Ctrl Pts',(2.98047914221,57.495,-5.6074788286105));
#39958=CARTESIAN_POINT('Ctrl Pts',(2.98047914221,49.875,-5.6074788286105));
#39959=CARTESIAN_POINT('Ctrl Pts',(2.97430877025608,57.495,-5.56641026634749));
#39960=CARTESIAN_POINT('Ctrl Pts',(2.97430877025608,49.875,-5.56641026634749));
#39961=CARTESIAN_POINT('Ctrl Pts',(2.96742703426683,57.495,-5.52637191504895));
#39962=CARTESIAN_POINT('Ctrl Pts',(2.96742703426683,49.875,-5.52637191504895));
#39963=CARTESIAN_POINT('Ctrl Pts',(2.95986479289849,57.495,-5.48743586913296));
#39964=CARTESIAN_POINT('Ctrl Pts',(2.95986479289849,49.875,-5.48743586913296));
#39965=CARTESIAN_POINT('Ctrl Pts',(2.95169462080131,57.495,-5.44977003302482));
#39966=CARTESIAN_POINT('Ctrl Pts',(2.95169462080131,49.875,-5.44977003302482));
#39967=CARTESIAN_POINT('Ctrl Pts',(2.94303247002258,57.495,-5.41364129622045));
#39968=CARTESIAN_POINT('Ctrl Pts',(2.94303247002258,49.875,-5.41364129622045));
#39969=CARTESIAN_POINT('Ctrl Pts',(2.93401523982671,57.495,-5.37936310952307));
#39970=CARTESIAN_POINT('Ctrl Pts',(2.93401523982671,49.875,-5.37936310952307));
#39971=CARTESIAN_POINT('Ctrl Pts',(2.92478335875774,57.495,-5.34725389048201));
#39972=CARTESIAN_POINT('Ctrl Pts',(2.92478335875774,49.875,-5.34725389048201));
#39973=CARTESIAN_POINT('Ctrl Pts',(2.91546314862891,57.495,-5.31759510370886));
#39974=CARTESIAN_POINT('Ctrl Pts',(2.91546314862891,49.875,-5.31759510370886));
#39975=CARTESIAN_POINT('Ctrl Pts',(2.90614521320837,57.495,-5.29057828960676));
#39976=CARTESIAN_POINT('Ctrl Pts',(2.90614521320837,49.875,-5.29057828960676));
#39977=CARTESIAN_POINT('Ctrl Pts',(2.89688168736508,57.495,-5.26630084561719));
#39978=CARTESIAN_POINT('Ctrl Pts',(2.89688168736508,49.875,-5.26630084561719));
#39979=CARTESIAN_POINT('Ctrl Pts',(2.88953536864313,57.495,-5.24910109063628));
#39980=CARTESIAN_POINT('Ctrl Pts',(2.88953536864313,49.875,-5.24910109063628));
#39981=CARTESIAN_POINT('Ctrl Pts',(2.884065589809,57.495,-5.23745215939571));
#39982=CARTESIAN_POINT('Ctrl Pts',(2.884065589809,49.875,-5.23745215939571));
#39983=CARTESIAN_POINT('Ctrl Pts',(2.88043681055505,57.495,-5.23024117954545));
#39984=CARTESIAN_POINT('Ctrl Pts',(2.88043681055505,49.875,-5.23024117954545));
#39985=CARTESIAN_POINT('Ctrl Pts',(2.87862685522556,57.495,-5.22677443144495));
#39986=CARTESIAN_POINT('Ctrl Pts',(2.87862685522556,49.875,-5.22677443144495));
#39987=CARTESIAN_POINT('Ctrl Pts',(2.96056324982543,51.145,-6.50167680247051));
#39988=CARTESIAN_POINT('Ctrl Pts',(2.96229154623625,51.145,-6.49043534784131));
#39989=CARTESIAN_POINT('Ctrl Pts',(2.96566304810549,51.145,-6.46801681444607));
#39990=CARTESIAN_POINT('Ctrl Pts',(2.97046502832945,51.145,-6.43458214159149));
#39991=CARTESIAN_POINT('Ctrl Pts',(2.97635619664337,51.145,-6.39038953466561));
#39992=CARTESIAN_POINT('Ctrl Pts',(2.98286238364857,51.145,-6.33579850967689));
#39993=CARTESIAN_POINT('Ctrl Pts',(2.98850417352769,51.145,-6.28186459845047));
#39994=CARTESIAN_POINT('Ctrl Pts',(2.99327554868811,51.145,-6.22859706400148));
#39995=CARTESIAN_POINT('Ctrl Pts',(2.99717295692919,51.145,-6.17600655789209));
#39996=CARTESIAN_POINT('Ctrl Pts',(3.00019778316108,51.145,-6.12410381716742));
#39997=CARTESIAN_POINT('Ctrl Pts',(3.00235671375967,51.145,-6.07290162599622));
#39998=CARTESIAN_POINT('Ctrl Pts',(3.00366113621882,51.145,-6.02241806591666));
#39999=CARTESIAN_POINT('Ctrl Pts',(3.00412716938109,51.145,-5.97267956506952));
#40000=CARTESIAN_POINT('Ctrl Pts',(3.00377540211877,51.145,-5.9237232280624));
#40001=CARTESIAN_POINT('Ctrl Pts',(3.00263159433912,51.145,-5.87560110342631));
#40002=CARTESIAN_POINT('Ctrl Pts',(3.00072490941932,51.145,-5.82837721216385));
#40003=CARTESIAN_POINT('Ctrl Pts',(2.99808342690946,51.145,-5.78211642456387));
#40004=CARTESIAN_POINT('Ctrl Pts',(2.9947301570106,51.145,-5.73687442119613));
#40005=CARTESIAN_POINT('Ctrl Pts',(2.9906797244254,51.145,-5.69268882427748));
#40006=CARTESIAN_POINT('Ctrl Pts',(2.98593308820271,51.145,-5.64956501668959));
#40007=CARTESIAN_POINT('Ctrl Pts',(2.98047914221,51.145,-5.6074788286105));
#40008=CARTESIAN_POINT('Ctrl Pts',(2.97430877025608,51.145,-5.56641026634749));
#40009=CARTESIAN_POINT('Ctrl Pts',(2.96742703426683,51.145,-5.52637191504895));
#40010=CARTESIAN_POINT('Ctrl Pts',(2.95986479289849,51.145,-5.48743586913296));
#40011=CARTESIAN_POINT('Ctrl Pts',(2.95169462080131,51.145,-5.44977003302482));
#40012=CARTESIAN_POINT('Ctrl Pts',(2.94303247002258,51.145,-5.41364129622045));
#40013=CARTESIAN_POINT('Ctrl Pts',(2.93401523982671,51.145,-5.37936310952307));
#40014=CARTESIAN_POINT('Ctrl Pts',(2.92478335875774,51.145,-5.34725389048201));
#40015=CARTESIAN_POINT('Ctrl Pts',(2.91546314862891,51.145,-5.31759510370886));
#40016=CARTESIAN_POINT('Ctrl Pts',(2.90614521320837,51.145,-5.29057828960676));
#40017=CARTESIAN_POINT('Ctrl Pts',(2.89688168736508,51.145,-5.26630084561719));
#40018=CARTESIAN_POINT('Ctrl Pts',(2.88953536864313,51.145,-5.24910109063628));
#40019=CARTESIAN_POINT('Ctrl Pts',(2.884065589809,51.145,-5.23745215939571));
#40020=CARTESIAN_POINT('Ctrl Pts',(2.88043681055505,51.145,-5.23024117954545));
#40021=CARTESIAN_POINT('Ctrl Pts',(2.87862685522556,51.145,-5.22677443144495));
#40022=CARTESIAN_POINT('Origin',(0.,54.32,0.));
#40023=CARTESIAN_POINT('',(0.592010183030743,51.145,-5.32519370006274));
#40024=CARTESIAN_POINT('Origin',(0.,51.145,0.));
#40025=CARTESIAN_POINT('',(0.592010183030743,54.32,-5.32519370006274));
#40026=CARTESIAN_POINT('Origin',(0.659304453656786,57.495,-5.93051272372135));
#40027=CARTESIAN_POINT('',(0.659304453656786,51.145,-5.93051272372135));
#40028=CARTESIAN_POINT('',(0.659304453656786,51.145,-5.93051272372135));
#40029=CARTESIAN_POINT('',(0.659304453656786,57.495,-5.93051272372135));
#40030=CARTESIAN_POINT('Origin',(-4.16333634234633E-16,57.495,-1.6286971771251E-12));
#40031=CARTESIAN_POINT('',(0.247119796320915,51.145,-7.13972463098307));
#40032=CARTESIAN_POINT('',(0.247119796320915,57.495,-7.13972463098307));
#40033=CARTESIAN_POINT('',(-0.247119796320921,51.145,-7.13972463098307));
#40034=CARTESIAN_POINT('Origin',(-4.16333634234633E-16,51.145,-1.6286971771251E-12));
#40035=CARTESIAN_POINT('',(-0.247119796320921,57.495,-7.13972463098307));
#40036=CARTESIAN_POINT('Ctrl Pts',(-0.659304453656788,57.495,-5.93051272372135));
#40037=CARTESIAN_POINT('Ctrl Pts',(-0.659304453656788,49.875,-5.93051272372135));
#40038=CARTESIAN_POINT('Ctrl Pts',(-0.659649967278237,57.495,-5.9344082212537));
#40039=CARTESIAN_POINT('Ctrl Pts',(-0.659649967278237,49.875,-5.9344082212537));
#40040=CARTESIAN_POINT('Ctrl Pts',(-0.660242999639202,57.495,-5.94245897164691));
#40041=CARTESIAN_POINT('Ctrl Pts',(-0.660242999639202,49.875,-5.94245897164691));
#40042=CARTESIAN_POINT('Ctrl Pts',(-0.660838563360922,57.495,-5.95531437453424));
#40043=CARTESIAN_POINT('Ctrl Pts',(-0.660838563360922,49.875,-5.95531437453424));
#40044=CARTESIAN_POINT('Ctrl Pts',(-0.661043615595512,57.495,-5.97401619058907));
#40045=CARTESIAN_POINT('Ctrl Pts',(-0.661043615595512,49.875,-5.97401619058907));
#40046=CARTESIAN_POINT('Ctrl Pts',(-0.660311421925998,57.495,-5.99999062205823));
#40047=CARTESIAN_POINT('Ctrl Pts',(-0.660311421925998,49.875,-5.99999062205823));
#40048=CARTESIAN_POINT('Ctrl Pts',(-0.658581184594089,57.495,-6.0285167231501));
#40049=CARTESIAN_POINT('Ctrl Pts',(-0.658581184594089,49.875,-6.0285167231501));
#40050=CARTESIAN_POINT('Ctrl Pts',(-0.655842009648634,57.495,-6.05948455921138));
#40051=CARTESIAN_POINT('Ctrl Pts',(-0.655842009648634,49.875,-6.05948455921138));
#40052=CARTESIAN_POINT('Ctrl Pts',(-0.65208348946162,57.495,-6.09268249742298));
#40053=CARTESIAN_POINT('Ctrl Pts',(-0.65208348946162,49.875,-6.09268249742298));
#40054=CARTESIAN_POINT('Ctrl Pts',(-0.647296629738921,57.495,-6.12780215712604));
#40055=CARTESIAN_POINT('Ctrl Pts',(-0.647296629738921,49.875,-6.12780215712604));
#40056=CARTESIAN_POINT('Ctrl Pts',(-0.641473544543615,57.495,-6.16449561918676));
#40057=CARTESIAN_POINT('Ctrl Pts',(-0.641473544543615,49.875,-6.16449561918676));
#40058=CARTESIAN_POINT('Ctrl Pts',(-0.634607707876565,57.495,-6.20242090374318));
#40059=CARTESIAN_POINT('Ctrl Pts',(-0.634607707876565,49.875,-6.20242090374318));
#40060=CARTESIAN_POINT('Ctrl Pts',(-0.626694128202842,57.495,-6.24128706412515));
#40061=CARTESIAN_POINT('Ctrl Pts',(-0.626694128202842,49.875,-6.24128706412515));
#40062=CARTESIAN_POINT('Ctrl Pts',(-0.617730009530307,57.495,-6.2809112037544));
#40063=CARTESIAN_POINT('Ctrl Pts',(-0.617730009530307,49.875,-6.2809112037544));
#40064=CARTESIAN_POINT('Ctrl Pts',(-0.607714431517402,57.495,-6.32121490697716));
#40065=CARTESIAN_POINT('Ctrl Pts',(-0.607714431517402,49.875,-6.32121490697716));
#40066=CARTESIAN_POINT('Ctrl Pts',(-0.596647533682212,57.495,-6.36218460951727));
#40067=CARTESIAN_POINT('Ctrl Pts',(-0.596647533682212,49.875,-6.36218460951727));
#40068=CARTESIAN_POINT('Ctrl Pts',(-0.584530087032238,57.495,-6.40384227175352));
#40069=CARTESIAN_POINT('Ctrl Pts',(-0.584530087032238,49.875,-6.40384227175352));
#40070=CARTESIAN_POINT('Ctrl Pts',(-0.57136310290558,57.495,-6.44621447382266));
#40071=CARTESIAN_POINT('Ctrl Pts',(-0.57136310290558,49.875,-6.44621447382266));
#40072=CARTESIAN_POINT('Ctrl Pts',(-0.557147755196278,57.495,-6.4892958755784));
#40073=CARTESIAN_POINT('Ctrl Pts',(-0.557147755196278,49.875,-6.4892958755784));
#40074=CARTESIAN_POINT('Ctrl Pts',(-0.54188492983995,57.495,-6.53304612199323));
#40075=CARTESIAN_POINT('Ctrl Pts',(-0.54188492983995,49.875,-6.53304612199323));
#40076=CARTESIAN_POINT('Ctrl Pts',(-0.525574676214357,57.495,-6.57740496530571));
#40077=CARTESIAN_POINT('Ctrl Pts',(-0.525574676214357,49.875,-6.57740496530571));
#40078=CARTESIAN_POINT('Ctrl Pts',(-0.508215876982669,57.495,-6.62230172760513));
#40079=CARTESIAN_POINT('Ctrl Pts',(-0.508215876982669,49.875,-6.62230172760513));
#40080=CARTESIAN_POINT('Ctrl Pts',(-0.489806088474623,57.495,-6.66766610085618));
#40081=CARTESIAN_POINT('Ctrl Pts',(-0.489806088474623,49.875,-6.66766610085618));
#40082=CARTESIAN_POINT('Ctrl Pts',(-0.470341429749656,57.495,-6.71344014059664));
#40083=CARTESIAN_POINT('Ctrl Pts',(-0.470341429749656,49.875,-6.71344014059664));
#40084=CARTESIAN_POINT('Ctrl Pts',(-0.44981707848863,57.495,-6.75958168761858));
#40085=CARTESIAN_POINT('Ctrl Pts',(-0.44981707848863,49.875,-6.75958168761858));
#40086=CARTESIAN_POINT('Ctrl Pts',(-0.428228256434474,57.495,-6.80606015708966));
#40087=CARTESIAN_POINT('Ctrl Pts',(-0.428228256434474,49.875,-6.80606015708966));
#40088=CARTESIAN_POINT('Ctrl Pts',(-0.405571362419757,57.495,-6.85285448604159));
#40089=CARTESIAN_POINT('Ctrl Pts',(-0.405571362419757,49.875,-6.85285448604159));
#40090=CARTESIAN_POINT('Ctrl Pts',(-0.381845111328235,57.495,-6.89995030467727));
#40091=CARTESIAN_POINT('Ctrl Pts',(-0.381845111328235,49.875,-6.89995030467727));
#40092=CARTESIAN_POINT('Ctrl Pts',(-0.357052332559036,57.495,-6.94733716327837));
#40093=CARTESIAN_POINT('Ctrl Pts',(-0.357052332559036,49.875,-6.94733716327837));
#40094=CARTESIAN_POINT('Ctrl Pts',(-0.331200384094009,57.495,-6.99500658045299));
#40095=CARTESIAN_POINT('Ctrl Pts',(-0.331200384094009,49.875,-6.99500658045299));
#40096=CARTESIAN_POINT('Ctrl Pts',(-0.304298370266205,57.495,-7.0429523011241));
#40097=CARTESIAN_POINT('Ctrl Pts',(-0.304298370266205,49.875,-7.0429523011241));
#40098=CARTESIAN_POINT('Ctrl Pts',(-0.281943861934841,57.495,-7.0815264936403));
#40099=CARTESIAN_POINT('Ctrl Pts',(-0.281943861934841,49.875,-7.0815264936403));
#40100=CARTESIAN_POINT('Ctrl Pts',(-0.264712515322388,57.495,-7.11057846529273));
#40101=CARTESIAN_POINT('Ctrl Pts',(-0.264712515322388,49.875,-7.11057846529273));
#40102=CARTESIAN_POINT('Ctrl Pts',(-0.253018452443276,57.495,-7.13000027153808));
#40103=CARTESIAN_POINT('Ctrl Pts',(-0.253018452443276,49.875,-7.13000027153808));
#40104=CARTESIAN_POINT('Ctrl Pts',(-0.247119796320918,57.495,-7.13972463098307));
#40105=CARTESIAN_POINT('Ctrl Pts',(-0.247119796320918,49.875,-7.13972463098307));
#40106=CARTESIAN_POINT('',(-0.659304453656788,51.145,-5.93051272372135));
#40107=CARTESIAN_POINT('Ctrl Pts',(-0.659304453656788,51.145,-5.93051272372135));
#40108=CARTESIAN_POINT('Ctrl Pts',(-0.659649967278237,51.145,-5.9344082212537));
#40109=CARTESIAN_POINT('Ctrl Pts',(-0.660242999639202,51.145,-5.94245897164691));
#40110=CARTESIAN_POINT('Ctrl Pts',(-0.660838563360922,51.145,-5.95531437453424));
#40111=CARTESIAN_POINT('Ctrl Pts',(-0.661043615595512,51.145,-5.97401619058907));
#40112=CARTESIAN_POINT('Ctrl Pts',(-0.660311421925998,51.145,-5.99999062205823));
#40113=CARTESIAN_POINT('Ctrl Pts',(-0.658581184594089,51.145,-6.0285167231501));
#40114=CARTESIAN_POINT('Ctrl Pts',(-0.655842009648634,51.145,-6.05948455921138));
#40115=CARTESIAN_POINT('Ctrl Pts',(-0.65208348946162,51.145,-6.09268249742298));
#40116=CARTESIAN_POINT('Ctrl Pts',(-0.647296629738921,51.145,-6.12780215712604));
#40117=CARTESIAN_POINT('Ctrl Pts',(-0.641473544543615,51.145,-6.16449561918676));
#40118=CARTESIAN_POINT('Ctrl Pts',(-0.634607707876565,51.145,-6.20242090374318));
#40119=CARTESIAN_POINT('Ctrl Pts',(-0.626694128202842,51.145,-6.24128706412515));
#40120=CARTESIAN_POINT('Ctrl Pts',(-0.617730009530307,51.145,-6.2809112037544));
#40121=CARTESIAN_POINT('Ctrl Pts',(-0.607714431517402,51.145,-6.32121490697716));
#40122=CARTESIAN_POINT('Ctrl Pts',(-0.596647533682212,51.145,-6.36218460951727));
#40123=CARTESIAN_POINT('Ctrl Pts',(-0.584530087032238,51.145,-6.40384227175352));
#40124=CARTESIAN_POINT('Ctrl Pts',(-0.57136310290558,51.145,-6.44621447382266));
#40125=CARTESIAN_POINT('Ctrl Pts',(-0.557147755196278,51.145,-6.4892958755784));
#40126=CARTESIAN_POINT('Ctrl Pts',(-0.54188492983995,51.145,-6.53304612199323));
#40127=CARTESIAN_POINT('Ctrl Pts',(-0.525574676214357,51.145,-6.57740496530571));
#40128=CARTESIAN_POINT('Ctrl Pts',(-0.508215876982669,51.145,-6.62230172760513));
#40129=CARTESIAN_POINT('Ctrl Pts',(-0.489806088474623,51.145,-6.66766610085618));
#40130=CARTESIAN_POINT('Ctrl Pts',(-0.470341429749656,51.145,-6.71344014059664));
#40131=CARTESIAN_POINT('Ctrl Pts',(-0.44981707848863,51.145,-6.75958168761858));
#40132=CARTESIAN_POINT('Ctrl Pts',(-0.428228256434474,51.145,-6.80606015708966));
#40133=CARTESIAN_POINT('Ctrl Pts',(-0.405571362419757,51.145,-6.85285448604159));
#40134=CARTESIAN_POINT('Ctrl Pts',(-0.381845111328235,51.145,-6.89995030467727));
#40135=CARTESIAN_POINT('Ctrl Pts',(-0.357052332559036,51.145,-6.94733716327837));
#40136=CARTESIAN_POINT('Ctrl Pts',(-0.331200384094009,51.145,-6.99500658045299));
#40137=CARTESIAN_POINT('Ctrl Pts',(-0.304298370266205,51.145,-7.0429523011241));
#40138=CARTESIAN_POINT('Ctrl Pts',(-0.281943861934841,51.145,-7.0815264936403));
#40139=CARTESIAN_POINT('Ctrl Pts',(-0.264712515322388,51.145,-7.11057846529273));
#40140=CARTESIAN_POINT('Ctrl Pts',(-0.253018452443276,51.145,-7.13000027153808));
#40141=CARTESIAN_POINT('Ctrl Pts',(-0.247119796320918,51.145,-7.13972463098307));
#40142=CARTESIAN_POINT('',(-0.659304453656788,57.495,-5.93051272372135));
#40143=CARTESIAN_POINT('Origin',(-0.575436549687219,57.495,-5.17611212951227));
#40144=CARTESIAN_POINT('',(-0.592010183030745,51.145,-5.32519370006274));
#40145=CARTESIAN_POINT('',(-0.592010183030745,54.32,-5.32519370006274));
#40146=CARTESIAN_POINT('',(-0.575436549687219,51.145,-5.17611212951227));
#40147=CARTESIAN_POINT('Ctrl Pts',(0.247119796320915,57.495,-7.13972463098307));
#40148=CARTESIAN_POINT('Ctrl Pts',(0.247119796320915,49.875,-7.13972463098307));
#40149=CARTESIAN_POINT('Ctrl Pts',(0.253018452443265,57.495,-7.13000027153814));
#40150=CARTESIAN_POINT('Ctrl Pts',(0.253018452443265,49.875,-7.13000027153814));
#40151=CARTESIAN_POINT('Ctrl Pts',(0.264712515322363,57.495,-7.1105784652929));
#40152=CARTESIAN_POINT('Ctrl Pts',(0.264712515322363,49.875,-7.1105784652929));
#40153=CARTESIAN_POINT('Ctrl Pts',(0.281943861934803,57.495,-7.0815264936406));
#40154=CARTESIAN_POINT('Ctrl Pts',(0.281943861934803,49.875,-7.0815264936406));
#40155=CARTESIAN_POINT('Ctrl Pts',(0.304298370266162,57.495,-7.04295230112448));
#40156=CARTESIAN_POINT('Ctrl Pts',(0.304298370266162,49.875,-7.04295230112448));
#40157=CARTESIAN_POINT('Ctrl Pts',(0.331200384093974,57.495,-6.99500658045334));
#40158=CARTESIAN_POINT('Ctrl Pts',(0.331200384093974,49.875,-6.99500658045334));
#40159=CARTESIAN_POINT('Ctrl Pts',(0.357052332559016,57.495,-6.94733716327859));
#40160=CARTESIAN_POINT('Ctrl Pts',(0.357052332559016,49.875,-6.94733716327859));
#40161=CARTESIAN_POINT('Ctrl Pts',(0.38184511132823,57.495,-6.89995030467732));
#40162=CARTESIAN_POINT('Ctrl Pts',(0.38184511132823,49.875,-6.89995030467732));
#40163=CARTESIAN_POINT('Ctrl Pts',(0.405571362419761,57.495,-6.85285448604147));
#40164=CARTESIAN_POINT('Ctrl Pts',(0.405571362419761,49.875,-6.85285448604147));
#40165=CARTESIAN_POINT('Ctrl Pts',(0.428228256434481,57.495,-6.80606015708944));
#40166=CARTESIAN_POINT('Ctrl Pts',(0.428228256434481,49.875,-6.80606015708944));
#40167=CARTESIAN_POINT('Ctrl Pts',(0.449817078488634,57.495,-6.75958168761835));
#40168=CARTESIAN_POINT('Ctrl Pts',(0.449817078488634,49.875,-6.75958168761835));
#40169=CARTESIAN_POINT('Ctrl Pts',(0.470341429749655,57.495,-6.71344014059646));
#40170=CARTESIAN_POINT('Ctrl Pts',(0.470341429749655,49.875,-6.71344014059646));
#40171=CARTESIAN_POINT('Ctrl Pts',(0.489806088474619,57.495,-6.66766610085612));
#40172=CARTESIAN_POINT('Ctrl Pts',(0.489806088474619,49.875,-6.66766610085612));
#40173=CARTESIAN_POINT('Ctrl Pts',(0.508215876982667,57.495,-6.62230172760518));
#40174=CARTESIAN_POINT('Ctrl Pts',(0.508215876982667,49.875,-6.62230172760518));
#40175=CARTESIAN_POINT('Ctrl Pts',(0.525574676214359,57.495,-6.57740496530586));
#40176=CARTESIAN_POINT('Ctrl Pts',(0.525574676214359,49.875,-6.57740496530586));
#40177=CARTESIAN_POINT('Ctrl Pts',(0.541884929839957,57.495,-6.53304612199338));
#40178=CARTESIAN_POINT('Ctrl Pts',(0.541884929839957,49.875,-6.53304612199338));
#40179=CARTESIAN_POINT('Ctrl Pts',(0.557147755196286,57.495,-6.48929587557851));
#40180=CARTESIAN_POINT('Ctrl Pts',(0.557147755196286,49.875,-6.48929587557851));
#40181=CARTESIAN_POINT('Ctrl Pts',(0.571363102905584,57.495,-6.4462144738227));
#40182=CARTESIAN_POINT('Ctrl Pts',(0.571363102905584,49.875,-6.4462144738227));
#40183=CARTESIAN_POINT('Ctrl Pts',(0.584530087032233,57.495,-6.40384227175349));
#40184=CARTESIAN_POINT('Ctrl Pts',(0.584530087032233,49.875,-6.40384227175349));
#40185=CARTESIAN_POINT('Ctrl Pts',(0.596647533682195,57.495,-6.36218460951721));
#40186=CARTESIAN_POINT('Ctrl Pts',(0.596647533682195,49.875,-6.36218460951721));
#40187=CARTESIAN_POINT('Ctrl Pts',(0.607714431517377,57.495,-6.32121490697708));
#40188=CARTESIAN_POINT('Ctrl Pts',(0.607714431517377,49.875,-6.32121490697708));
#40189=CARTESIAN_POINT('Ctrl Pts',(0.617730009530282,57.495,-6.28091120375433));
#40190=CARTESIAN_POINT('Ctrl Pts',(0.617730009530282,49.875,-6.28091120375433));
#40191=CARTESIAN_POINT('Ctrl Pts',(0.626694128202827,57.495,-6.24128706412512));
#40192=CARTESIAN_POINT('Ctrl Pts',(0.626694128202827,49.875,-6.24128706412512));
#40193=CARTESIAN_POINT('Ctrl Pts',(0.63460770787657,57.495,-6.2024209037432));
#40194=CARTESIAN_POINT('Ctrl Pts',(0.63460770787657,49.875,-6.2024209037432));
#40195=CARTESIAN_POINT('Ctrl Pts',(0.641473544543642,57.495,-6.16449561918681));
#40196=CARTESIAN_POINT('Ctrl Pts',(0.641473544543642,49.875,-6.16449561918681));
#40197=CARTESIAN_POINT('Ctrl Pts',(0.647296629738964,57.495,-6.12780215712609));
#40198=CARTESIAN_POINT('Ctrl Pts',(0.647296629738964,49.875,-6.12780215712609));
#40199=CARTESIAN_POINT('Ctrl Pts',(0.652083489461663,57.495,-6.092682497423));
#40200=CARTESIAN_POINT('Ctrl Pts',(0.652083489461663,49.875,-6.092682497423));
#40201=CARTESIAN_POINT('Ctrl Pts',(0.655842009648654,57.495,-6.05948455921138));
#40202=CARTESIAN_POINT('Ctrl Pts',(0.655842009648654,49.875,-6.05948455921138));
#40203=CARTESIAN_POINT('Ctrl Pts',(0.658581184594064,57.495,-6.02851672315009));
#40204=CARTESIAN_POINT('Ctrl Pts',(0.658581184594064,49.875,-6.02851672315009));
#40205=CARTESIAN_POINT('Ctrl Pts',(0.660311421925919,57.495,-5.99999062205821));
#40206=CARTESIAN_POINT('Ctrl Pts',(0.660311421925919,49.875,-5.99999062205821));
#40207=CARTESIAN_POINT('Ctrl Pts',(0.661043615595394,57.495,-5.97401619058905));
#40208=CARTESIAN_POINT('Ctrl Pts',(0.661043615595394,49.875,-5.97401619058905));
#40209=CARTESIAN_POINT('Ctrl Pts',(0.660838563360811,57.495,-5.95531437453421));
#40210=CARTESIAN_POINT('Ctrl Pts',(0.660838563360811,49.875,-5.95531437453421));
#40211=CARTESIAN_POINT('Ctrl Pts',(0.660242999639131,57.495,-5.94245897164689));
#40212=CARTESIAN_POINT('Ctrl Pts',(0.660242999639131,49.875,-5.94245897164689));
#40213=CARTESIAN_POINT('Ctrl Pts',(0.659649967278209,57.495,-5.93440822125369));
#40214=CARTESIAN_POINT('Ctrl Pts',(0.659649967278209,49.875,-5.93440822125369));
#40215=CARTESIAN_POINT('Ctrl Pts',(0.659304453656786,57.495,-5.93051272372135));
#40216=CARTESIAN_POINT('Ctrl Pts',(0.659304453656786,49.875,-5.93051272372135));
#40217=CARTESIAN_POINT('Ctrl Pts',(0.247119796320915,51.145,-7.13972463098307));
#40218=CARTESIAN_POINT('Ctrl Pts',(0.253018452443265,51.145,-7.13000027153814));
#40219=CARTESIAN_POINT('Ctrl Pts',(0.264712515322363,51.145,-7.1105784652929));
#40220=CARTESIAN_POINT('Ctrl Pts',(0.281943861934803,51.145,-7.0815264936406));
#40221=CARTESIAN_POINT('Ctrl Pts',(0.304298370266162,51.145,-7.04295230112448));
#40222=CARTESIAN_POINT('Ctrl Pts',(0.331200384093974,51.145,-6.99500658045334));
#40223=CARTESIAN_POINT('Ctrl Pts',(0.357052332559016,51.145,-6.94733716327859));
#40224=CARTESIAN_POINT('Ctrl Pts',(0.38184511132823,51.145,-6.89995030467732));
#40225=CARTESIAN_POINT('Ctrl Pts',(0.405571362419761,51.145,-6.85285448604147));
#40226=CARTESIAN_POINT('Ctrl Pts',(0.428228256434481,51.145,-6.80606015708944));
#40227=CARTESIAN_POINT('Ctrl Pts',(0.449817078488634,51.145,-6.75958168761835));
#40228=CARTESIAN_POINT('Ctrl Pts',(0.470341429749655,51.145,-6.71344014059646));
#40229=CARTESIAN_POINT('Ctrl Pts',(0.489806088474619,51.145,-6.66766610085612));
#40230=CARTESIAN_POINT('Ctrl Pts',(0.508215876982667,51.145,-6.62230172760518));
#40231=CARTESIAN_POINT('Ctrl Pts',(0.525574676214359,51.145,-6.57740496530586));
#40232=CARTESIAN_POINT('Ctrl Pts',(0.541884929839957,51.145,-6.53304612199338));
#40233=CARTESIAN_POINT('Ctrl Pts',(0.557147755196286,51.145,-6.48929587557851));
#40234=CARTESIAN_POINT('Ctrl Pts',(0.571363102905584,51.145,-6.4462144738227));
#40235=CARTESIAN_POINT('Ctrl Pts',(0.584530087032233,51.145,-6.40384227175349));
#40236=CARTESIAN_POINT('Ctrl Pts',(0.596647533682195,51.145,-6.36218460951721));
#40237=CARTESIAN_POINT('Ctrl Pts',(0.607714431517377,51.145,-6.32121490697708));
#40238=CARTESIAN_POINT('Ctrl Pts',(0.617730009530282,51.145,-6.28091120375433));
#40239=CARTESIAN_POINT('Ctrl Pts',(0.626694128202827,51.145,-6.24128706412512));
#40240=CARTESIAN_POINT('Ctrl Pts',(0.63460770787657,51.145,-6.2024209037432));
#40241=CARTESIAN_POINT('Ctrl Pts',(0.641473544543642,51.145,-6.16449561918681));
#40242=CARTESIAN_POINT('Ctrl Pts',(0.647296629738964,51.145,-6.12780215712609));
#40243=CARTESIAN_POINT('Ctrl Pts',(0.652083489461663,51.145,-6.092682497423));
#40244=CARTESIAN_POINT('Ctrl Pts',(0.655842009648654,51.145,-6.05948455921138));
#40245=CARTESIAN_POINT('Ctrl Pts',(0.658581184594064,51.145,-6.02851672315009));
#40246=CARTESIAN_POINT('Ctrl Pts',(0.660311421925919,51.145,-5.99999062205821));
#40247=CARTESIAN_POINT('Ctrl Pts',(0.661043615595394,51.145,-5.97401619058905));
#40248=CARTESIAN_POINT('Ctrl Pts',(0.660838563360811,51.145,-5.95531437453421));
#40249=CARTESIAN_POINT('Ctrl Pts',(0.660242999639131,51.145,-5.94245897164689));
#40250=CARTESIAN_POINT('Ctrl Pts',(0.659649967278209,51.145,-5.93440822125369));
#40251=CARTESIAN_POINT('Ctrl Pts',(0.659304453656786,51.145,-5.93051272372135));
#40252=CARTESIAN_POINT('Origin',(0.,54.32,0.));
#40253=CARTESIAN_POINT('',(-1.4909173120086,51.145,-5.1463899549833));
#40254=CARTESIAN_POINT('Origin',(0.,51.145,0.));
#40255=CARTESIAN_POINT('',(-1.4909173120086,54.32,-5.1463899549833));
#40256=CARTESIAN_POINT('Origin',(-1.66039107437148,57.495,-5.73138421404289));
#40257=CARTESIAN_POINT('',(-1.66039107437148,51.145,-5.73138421404289));
#40258=CARTESIAN_POINT('',(-1.66039107437148,51.145,-5.73138421404289));
#40259=CARTESIAN_POINT('',(-1.66039107437148,57.495,-5.73138421404289));
#40260=CARTESIAN_POINT('Origin',(-6.23660068148933E-13,57.495,-1.50456066262064E-12));
#40261=CARTESIAN_POINT('',(-2.50394540602692,51.145,-6.69081410619341));
#40262=CARTESIAN_POINT('',(-2.50394540602692,57.495,-6.69081410619341));
#40263=CARTESIAN_POINT('',(-2.96056324982543,51.145,-6.5016768024705));
#40264=CARTESIAN_POINT('Origin',(-6.23660068148933E-13,51.145,-1.50456066262064E-12));
#40265=CARTESIAN_POINT('',(-2.96056324982543,57.495,-6.5016768024705));
#40266=CARTESIAN_POINT('Ctrl Pts',(-2.87862685522557,57.495,-5.22677443144495));
#40267=CARTESIAN_POINT('Ctrl Pts',(-2.87862685522557,49.875,-5.22677443144495));
#40268=CARTESIAN_POINT('Ctrl Pts',(-2.88043681055508,57.495,-5.23024117954545));
#40269=CARTESIAN_POINT('Ctrl Pts',(-2.88043681055508,49.875,-5.23024117954545));
#40270=CARTESIAN_POINT('Ctrl Pts',(-2.88406558980908,57.495,-5.2374521593957));
#40271=CARTESIAN_POINT('Ctrl Pts',(-2.88406558980908,49.875,-5.2374521593957));
#40272=CARTESIAN_POINT('Ctrl Pts',(-2.88953536864324,57.495,-5.24910109063627));
#40273=CARTESIAN_POINT('Ctrl Pts',(-2.88953536864324,49.875,-5.24910109063627));
#40274=CARTESIAN_POINT('Ctrl Pts',(-2.8968816873652,57.495,-5.26630084561717));
#40275=CARTESIAN_POINT('Ctrl Pts',(-2.8968816873652,49.875,-5.26630084561717));
#40276=CARTESIAN_POINT('Ctrl Pts',(-2.90614521320845,57.495,-5.29057828960674));
#40277=CARTESIAN_POINT('Ctrl Pts',(-2.90614521320845,49.875,-5.29057828960674));
#40278=CARTESIAN_POINT('Ctrl Pts',(-2.91546314862894,57.495,-5.31759510370885));
#40279=CARTESIAN_POINT('Ctrl Pts',(-2.91546314862894,49.875,-5.31759510370885));
#40280=CARTESIAN_POINT('Ctrl Pts',(-2.92478335875772,57.495,-5.34725389048201));
#40281=CARTESIAN_POINT('Ctrl Pts',(-2.92478335875772,49.875,-5.34725389048201));
#40282=CARTESIAN_POINT('Ctrl Pts',(-2.93401523982666,57.495,-5.37936310952307));
#40283=CARTESIAN_POINT('Ctrl Pts',(-2.93401523982666,49.875,-5.37936310952307));
#40284=CARTESIAN_POINT('Ctrl Pts',(-2.94303247002252,57.495,-5.41364129622042));
#40285=CARTESIAN_POINT('Ctrl Pts',(-2.94303247002252,49.875,-5.41364129622042));
#40286=CARTESIAN_POINT('Ctrl Pts',(-2.95169462080126,57.495,-5.44977003302479));
#40287=CARTESIAN_POINT('Ctrl Pts',(-2.95169462080126,49.875,-5.44977003302479));
#40288=CARTESIAN_POINT('Ctrl Pts',(-2.95986479289848,57.495,-5.48743586913294));
#40289=CARTESIAN_POINT('Ctrl Pts',(-2.95986479289848,49.875,-5.48743586913294));
#40290=CARTESIAN_POINT('Ctrl Pts',(-2.96742703426686,57.495,-5.52637191504897));
#40291=CARTESIAN_POINT('Ctrl Pts',(-2.96742703426686,49.875,-5.52637191504897));
#40292=CARTESIAN_POINT('Ctrl Pts',(-2.97430877025613,57.495,-5.56641026634754));
#40293=CARTESIAN_POINT('Ctrl Pts',(-2.97430877025613,49.875,-5.56641026634754));
#40294=CARTESIAN_POINT('Ctrl Pts',(-2.98047914221005,57.495,-5.60747882861056));
#40295=CARTESIAN_POINT('Ctrl Pts',(-2.98047914221005,49.875,-5.60747882861056));
#40296=CARTESIAN_POINT('Ctrl Pts',(-2.98593308820275,57.495,-5.64956501668965));
#40297=CARTESIAN_POINT('Ctrl Pts',(-2.98593308820275,49.875,-5.64956501668965));
#40298=CARTESIAN_POINT('Ctrl Pts',(-2.99067972442542,57.495,-5.6926888242775));
#40299=CARTESIAN_POINT('Ctrl Pts',(-2.99067972442542,49.875,-5.6926888242775));
#40300=CARTESIAN_POINT('Ctrl Pts',(-2.99473015701058,57.495,-5.7368744211961));
#40301=CARTESIAN_POINT('Ctrl Pts',(-2.99473015701058,49.875,-5.7368744211961));
#40302=CARTESIAN_POINT('Ctrl Pts',(-2.99808342690941,57.495,-5.78211642456377));
#40303=CARTESIAN_POINT('Ctrl Pts',(-2.99808342690941,49.875,-5.78211642456377));
#40304=CARTESIAN_POINT('Ctrl Pts',(-3.00072490941925,57.495,-5.82837721216372));
#40305=CARTESIAN_POINT('Ctrl Pts',(-3.00072490941925,49.875,-5.82837721216372));
#40306=CARTESIAN_POINT('Ctrl Pts',(-3.00263159433907,57.495,-5.87560110342618));
#40307=CARTESIAN_POINT('Ctrl Pts',(-3.00263159433907,49.875,-5.87560110342618));
#40308=CARTESIAN_POINT('Ctrl Pts',(-3.00377540211876,57.495,-5.92372322806235));
#40309=CARTESIAN_POINT('Ctrl Pts',(-3.00377540211876,49.875,-5.92372322806235));
#40310=CARTESIAN_POINT('Ctrl Pts',(-3.00412716938111,57.495,-5.97267956506957));
#40311=CARTESIAN_POINT('Ctrl Pts',(-3.00412716938111,49.875,-5.97267956506957));
#40312=CARTESIAN_POINT('Ctrl Pts',(-3.00366113621889,57.495,-6.02241806591683));
#40313=CARTESIAN_POINT('Ctrl Pts',(-3.00366113621889,49.875,-6.02241806591683));
#40314=CARTESIAN_POINT('Ctrl Pts',(-3.00235671375975,57.495,-6.07290162599645));
#40315=CARTESIAN_POINT('Ctrl Pts',(-3.00235671375975,49.875,-6.07290162599645));
#40316=CARTESIAN_POINT('Ctrl Pts',(-3.00019778316116,57.495,-6.12410381716763));
#40317=CARTESIAN_POINT('Ctrl Pts',(-3.00019778316116,49.875,-6.12410381716763));
#40318=CARTESIAN_POINT('Ctrl Pts',(-2.99717295692923,57.495,-6.1760065578922));
#40319=CARTESIAN_POINT('Ctrl Pts',(-2.99717295692923,49.875,-6.1760065578922));
#40320=CARTESIAN_POINT('Ctrl Pts',(-2.9932755486881,57.495,-6.22859706400143));
#40321=CARTESIAN_POINT('Ctrl Pts',(-2.9932755486881,49.875,-6.22859706400143));
#40322=CARTESIAN_POINT('Ctrl Pts',(-2.98850417352762,57.495,-6.28186459845025));
#40323=CARTESIAN_POINT('Ctrl Pts',(-2.98850417352762,49.875,-6.28186459845025));
#40324=CARTESIAN_POINT('Ctrl Pts',(-2.98286238364847,57.495,-6.33579850967655));
#40325=CARTESIAN_POINT('Ctrl Pts',(-2.98286238364847,49.875,-6.33579850967655));
#40326=CARTESIAN_POINT('Ctrl Pts',(-2.97635619664327,57.495,-6.39038953466525));
#40327=CARTESIAN_POINT('Ctrl Pts',(-2.97635619664327,49.875,-6.39038953466525));
#40328=CARTESIAN_POINT('Ctrl Pts',(-2.97046502832937,57.495,-6.43458214159119));
#40329=CARTESIAN_POINT('Ctrl Pts',(-2.97046502832937,49.875,-6.43458214159119));
#40330=CARTESIAN_POINT('Ctrl Pts',(-2.96566304810545,57.495,-6.4680168144459));
#40331=CARTESIAN_POINT('Ctrl Pts',(-2.96566304810545,49.875,-6.4680168144459));
#40332=CARTESIAN_POINT('Ctrl Pts',(-2.96229154623624,57.495,-6.49043534784125));
#40333=CARTESIAN_POINT('Ctrl Pts',(-2.96229154623624,49.875,-6.49043534784125));
#40334=CARTESIAN_POINT('Ctrl Pts',(-2.96056324982543,57.495,-6.5016768024705));
#40335=CARTESIAN_POINT('Ctrl Pts',(-2.96056324982543,49.875,-6.5016768024705));
#40336=CARTESIAN_POINT('',(-2.87862685522557,51.145,-5.22677443144495));
#40337=CARTESIAN_POINT('Ctrl Pts',(-2.87862685522557,51.145,-5.22677443144495));
#40338=CARTESIAN_POINT('Ctrl Pts',(-2.88043681055508,51.145,-5.23024117954545));
#40339=CARTESIAN_POINT('Ctrl Pts',(-2.88406558980908,51.145,-5.2374521593957));
#40340=CARTESIAN_POINT('Ctrl Pts',(-2.88953536864324,51.145,-5.24910109063627));
#40341=CARTESIAN_POINT('Ctrl Pts',(-2.8968816873652,51.145,-5.26630084561717));
#40342=CARTESIAN_POINT('Ctrl Pts',(-2.90614521320845,51.145,-5.29057828960674));
#40343=CARTESIAN_POINT('Ctrl Pts',(-2.91546314862894,51.145,-5.31759510370885));
#40344=CARTESIAN_POINT('Ctrl Pts',(-2.92478335875772,51.145,-5.34725389048201));
#40345=CARTESIAN_POINT('Ctrl Pts',(-2.93401523982666,51.145,-5.37936310952307));
#40346=CARTESIAN_POINT('Ctrl Pts',(-2.94303247002252,51.145,-5.41364129622042));
#40347=CARTESIAN_POINT('Ctrl Pts',(-2.95169462080126,51.145,-5.44977003302479));
#40348=CARTESIAN_POINT('Ctrl Pts',(-2.95986479289848,51.145,-5.48743586913294));
#40349=CARTESIAN_POINT('Ctrl Pts',(-2.96742703426686,51.145,-5.52637191504897));
#40350=CARTESIAN_POINT('Ctrl Pts',(-2.97430877025613,51.145,-5.56641026634754));
#40351=CARTESIAN_POINT('Ctrl Pts',(-2.98047914221005,51.145,-5.60747882861056));
#40352=CARTESIAN_POINT('Ctrl Pts',(-2.98593308820275,51.145,-5.64956501668965));
#40353=CARTESIAN_POINT('Ctrl Pts',(-2.99067972442542,51.145,-5.6926888242775));
#40354=CARTESIAN_POINT('Ctrl Pts',(-2.99473015701058,51.145,-5.7368744211961));
#40355=CARTESIAN_POINT('Ctrl Pts',(-2.99808342690941,51.145,-5.78211642456377));
#40356=CARTESIAN_POINT('Ctrl Pts',(-3.00072490941925,51.145,-5.82837721216372));
#40357=CARTESIAN_POINT('Ctrl Pts',(-3.00263159433907,51.145,-5.87560110342618));
#40358=CARTESIAN_POINT('Ctrl Pts',(-3.00377540211876,51.145,-5.92372322806235));
#40359=CARTESIAN_POINT('Ctrl Pts',(-3.00412716938111,51.145,-5.97267956506957));
#40360=CARTESIAN_POINT('Ctrl Pts',(-3.00366113621889,51.145,-6.02241806591683));
#40361=CARTESIAN_POINT('Ctrl Pts',(-3.00235671375975,51.145,-6.07290162599645));
#40362=CARTESIAN_POINT('Ctrl Pts',(-3.00019778316116,51.145,-6.12410381716763));
#40363=CARTESIAN_POINT('Ctrl Pts',(-2.99717295692923,51.145,-6.1760065578922));
#40364=CARTESIAN_POINT('Ctrl Pts',(-2.9932755486881,51.145,-6.22859706400143));
#40365=CARTESIAN_POINT('Ctrl Pts',(-2.98850417352762,51.145,-6.28186459845025));
#40366=CARTESIAN_POINT('Ctrl Pts',(-2.98286238364847,51.145,-6.33579850967655));
#40367=CARTESIAN_POINT('Ctrl Pts',(-2.97635619664327,51.145,-6.39038953466525));
#40368=CARTESIAN_POINT('Ctrl Pts',(-2.97046502832937,51.145,-6.43458214159119));
#40369=CARTESIAN_POINT('Ctrl Pts',(-2.96566304810545,51.145,-6.4680168144459));
#40370=CARTESIAN_POINT('Ctrl Pts',(-2.96229154623624,51.145,-6.49043534784125));
#40371=CARTESIAN_POINT('Ctrl Pts',(-2.96056324982543,51.145,-6.5016768024705));
#40372=CARTESIAN_POINT('',(-2.87862685522557,57.495,-5.22677443144495));
#40373=CARTESIAN_POINT('Origin',(-2.51244640654327,57.495,-4.56189402049717));
#40374=CARTESIAN_POINT('',(-2.58480949428933,51.145,-4.69328497730872));
#40375=CARTESIAN_POINT('',(-2.58480949428933,54.32,-4.69328497730872));
#40376=CARTESIAN_POINT('',(-2.51244640654327,51.145,-4.56189402049717));
#40377=CARTESIAN_POINT('Ctrl Pts',(-2.50394540602692,57.495,-6.69081410619341));
#40378=CARTESIAN_POINT('Ctrl Pts',(-2.50394540602692,49.875,-6.69081410619341));
#40379=CARTESIAN_POINT('Ctrl Pts',(-2.49477440711622,57.495,-6.6840872875067));
#40380=CARTESIAN_POINT('Ctrl Pts',(-2.49477440711622,49.875,-6.6840872875067));
#40381=CARTESIAN_POINT('Ctrl Pts',(-2.47653809829367,57.495,-6.67061900235319));
#40382=CARTESIAN_POINT('Ctrl Pts',(-2.47653809829367,49.875,-6.67061900235319));
#40383=CARTESIAN_POINT('Ctrl Pts',(-2.44950070161195,57.495,-6.65037263123044));
#40384=CARTESIAN_POINT('Ctrl Pts',(-2.44950070161195,49.875,-6.65037263123044));
#40385=CARTESIAN_POINT('Ctrl Pts',(-2.41408612451247,57.495,-6.62328942425873));
#40386=CARTESIAN_POINT('Ctrl Pts',(-2.41408612451247,49.875,-6.62328942425873));
#40387=CARTESIAN_POINT('Ctrl Pts',(-2.37088387159997,57.495,-6.58928830924833));
#40388=CARTESIAN_POINT('Ctrl Pts',(-2.37088387159997,49.875,-6.58928830924833));
#40389=CARTESIAN_POINT('Ctrl Pts',(-2.32875748935431,57.495,-6.55514062276576));
#40390=CARTESIAN_POINT('Ctrl Pts',(-2.32875748935431,49.875,-6.55514062276576));
#40391=CARTESIAN_POINT('Ctrl Pts',(-2.28771778279682,57.495,-6.52084865967131));
#40392=CARTESIAN_POINT('Ctrl Pts',(-2.28771778279682,49.875,-6.52084865967131));
#40393=CARTESIAN_POINT('Ctrl Pts',(-2.24777479550452,57.495,-6.48641743997165));
#40394=CARTESIAN_POINT('Ctrl Pts',(-2.24777479550452,49.875,-6.48641743997165));
#40395=CARTESIAN_POINT('Ctrl Pts',(-2.20893514043546,57.495,-6.45185553518355));
#40396=CARTESIAN_POINT('Ctrl Pts',(-2.20893514043546,49.875,-6.45185553518355));
#40397=CARTESIAN_POINT('Ctrl Pts',(-2.17120312938032,57.495,-6.41717671306116));
#40398=CARTESIAN_POINT('Ctrl Pts',(-2.17120312938032,49.875,-6.41717671306116));
#40399=CARTESIAN_POINT('Ctrl Pts',(-2.13458349574322,57.495,-6.38240181135686));
#40400=CARTESIAN_POINT('Ctrl Pts',(-2.13458349574322,49.875,-6.38240181135686));
#40401=CARTESIAN_POINT('Ctrl Pts',(-2.09908352929886,57.495,-6.34756091533109));
#40402=CARTESIAN_POINT('Ctrl Pts',(-2.09908352929886,49.875,-6.34756091533109));
#40403=CARTESIAN_POINT('Ctrl Pts',(-2.06471490843566,57.495,-6.31269482043472));
#40404=CARTESIAN_POINT('Ctrl Pts',(-2.06471490843566,49.875,-6.31269482043472));
#40405=CARTESIAN_POINT('Ctrl Pts',(-2.03149622201774,57.495,-6.27785854554207));
#40406=CARTESIAN_POINT('Ctrl Pts',(-2.03149622201774,49.875,-6.27785854554207));
#40407=CARTESIAN_POINT('Ctrl Pts',(-1.99945211810842,57.495,-6.24311798195999));
#40408=CARTESIAN_POINT('Ctrl Pts',(-1.99945211810842,49.875,-6.24311798195999));
#40409=CARTESIAN_POINT('Ctrl Pts',(-1.96860861168855,57.495,-6.20853885514991));
#40410=CARTESIAN_POINT('Ctrl Pts',(-1.96860861168855,49.875,-6.20853885514991));
#40411=CARTESIAN_POINT('Ctrl Pts',(-1.93898880419738,57.495,-6.17417680788948));
#40412=CARTESIAN_POINT('Ctrl Pts',(-1.93898880419738,49.875,-6.17417680788948));
#40413=CARTESIAN_POINT('Ctrl Pts',(-1.91060895733316,57.495,-6.14006878432979));
#40414=CARTESIAN_POINT('Ctrl Pts',(-1.91060895733316,49.875,-6.14006878432979));
#40415=CARTESIAN_POINT('Ctrl Pts',(-1.88347219921807,57.495,-6.10621926889293));
#40416=CARTESIAN_POINT('Ctrl Pts',(-1.88347219921807,49.875,-6.10621926889293));
#40417=CARTESIAN_POINT('Ctrl Pts',(-1.85756929242873,57.495,-6.07260331771224));
#40418=CARTESIAN_POINT('Ctrl Pts',(-1.85756929242873,49.875,-6.07260331771224));
#40419=CARTESIAN_POINT('Ctrl Pts',(-1.83289254541003,57.495,-6.03920034699142));
#40420=CARTESIAN_POINT('Ctrl Pts',(-1.83289254541003,49.875,-6.03920034699142));
#40421=CARTESIAN_POINT('Ctrl Pts',(-1.80944727788364,57.495,-6.00602283509636));
#40422=CARTESIAN_POINT('Ctrl Pts',(-1.80944727788364,49.875,-6.00602283509636));
#40423=CARTESIAN_POINT('Ctrl Pts',(-1.78726264793637,57.495,-5.97314358084405));
#40424=CARTESIAN_POINT('Ctrl Pts',(-1.78726264793637,49.875,-5.97314358084405));
#40425=CARTESIAN_POINT('Ctrl Pts',(-1.76640606389863,57.495,-5.94073262861954));
#40426=CARTESIAN_POINT('Ctrl Pts',(-1.76640606389863,49.875,-5.94073262861954));
#40427=CARTESIAN_POINT('Ctrl Pts',(-1.74698425466385,57.495,-5.90906068827417));
#40428=CARTESIAN_POINT('Ctrl Pts',(-1.74698425466385,49.875,-5.90906068827417));
#40429=CARTESIAN_POINT('Ctrl Pts',(-1.72912206102237,57.495,-5.87844620539466));
#40430=CARTESIAN_POINT('Ctrl Pts',(-1.72912206102237,49.875,-5.87844620539466));
#40431=CARTESIAN_POINT('Ctrl Pts',(-1.71294534020681,57.495,-5.84921363316514));
#40432=CARTESIAN_POINT('Ctrl Pts',(-1.71294534020681,49.875,-5.84921363316514));
#40433=CARTESIAN_POINT('Ctrl Pts',(-1.69856379474193,57.495,-5.8216513201319));
#40434=CARTESIAN_POINT('Ctrl Pts',(-1.69856379474193,49.875,-5.8216513201319));
#40435=CARTESIAN_POINT('Ctrl Pts',(-1.68604879760681,57.495,-5.79595877235173));
#40436=CARTESIAN_POINT('Ctrl Pts',(-1.68604879760681,49.875,-5.79595877235173));
#40437=CARTESIAN_POINT('Ctrl Pts',(-1.67543235427339,57.495,-5.77224172513534));
#40438=CARTESIAN_POINT('Ctrl Pts',(-1.67543235427339,49.875,-5.77224172513534));
#40439=CARTESIAN_POINT('Ctrl Pts',(-1.66846492267669,57.495,-5.75488502996854));
#40440=CARTESIAN_POINT('Ctrl Pts',(-1.66846492267669,49.875,-5.75488502996854));
#40441=CARTESIAN_POINT('Ctrl Pts',(-1.66409560210811,57.495,-5.74278027398956));
#40442=CARTESIAN_POINT('Ctrl Pts',(-1.66409560210811,49.875,-5.74278027398956));
#40443=CARTESIAN_POINT('Ctrl Pts',(-1.66156260377489,57.495,-5.73511540682054));
#40444=CARTESIAN_POINT('Ctrl Pts',(-1.66156260377489,49.875,-5.73511540682054));
#40445=CARTESIAN_POINT('Ctrl Pts',(-1.66039107437148,57.495,-5.73138421404289));
#40446=CARTESIAN_POINT('Ctrl Pts',(-1.66039107437148,49.875,-5.73138421404289));
#40447=CARTESIAN_POINT('Ctrl Pts',(-2.50394540602692,51.145,-6.69081410619341));
#40448=CARTESIAN_POINT('Ctrl Pts',(-2.49477440711622,51.145,-6.6840872875067));
#40449=CARTESIAN_POINT('Ctrl Pts',(-2.47653809829367,51.145,-6.67061900235319));
#40450=CARTESIAN_POINT('Ctrl Pts',(-2.44950070161195,51.145,-6.65037263123044));
#40451=CARTESIAN_POINT('Ctrl Pts',(-2.41408612451247,51.145,-6.62328942425873));
#40452=CARTESIAN_POINT('Ctrl Pts',(-2.37088387159997,51.145,-6.58928830924833));
#40453=CARTESIAN_POINT('Ctrl Pts',(-2.32875748935431,51.145,-6.55514062276576));
#40454=CARTESIAN_POINT('Ctrl Pts',(-2.28771778279682,51.145,-6.52084865967131));
#40455=CARTESIAN_POINT('Ctrl Pts',(-2.24777479550452,51.145,-6.48641743997165));
#40456=CARTESIAN_POINT('Ctrl Pts',(-2.20893514043546,51.145,-6.45185553518355));
#40457=CARTESIAN_POINT('Ctrl Pts',(-2.17120312938032,51.145,-6.41717671306116));
#40458=CARTESIAN_POINT('Ctrl Pts',(-2.13458349574322,51.145,-6.38240181135686));
#40459=CARTESIAN_POINT('Ctrl Pts',(-2.09908352929886,51.145,-6.34756091533109));
#40460=CARTESIAN_POINT('Ctrl Pts',(-2.06471490843566,51.145,-6.31269482043472));
#40461=CARTESIAN_POINT('Ctrl Pts',(-2.03149622201774,51.145,-6.27785854554207));
#40462=CARTESIAN_POINT('Ctrl Pts',(-1.99945211810842,51.145,-6.24311798195999));
#40463=CARTESIAN_POINT('Ctrl Pts',(-1.96860861168855,51.145,-6.20853885514991));
#40464=CARTESIAN_POINT('Ctrl Pts',(-1.93898880419738,51.145,-6.17417680788948));
#40465=CARTESIAN_POINT('Ctrl Pts',(-1.91060895733316,51.145,-6.14006878432979));
#40466=CARTESIAN_POINT('Ctrl Pts',(-1.88347219921807,51.145,-6.10621926889293));
#40467=CARTESIAN_POINT('Ctrl Pts',(-1.85756929242873,51.145,-6.07260331771224));
#40468=CARTESIAN_POINT('Ctrl Pts',(-1.83289254541003,51.145,-6.03920034699142));
#40469=CARTESIAN_POINT('Ctrl Pts',(-1.80944727788364,51.145,-6.00602283509636));
#40470=CARTESIAN_POINT('Ctrl Pts',(-1.78726264793637,51.145,-5.97314358084405));
#40471=CARTESIAN_POINT('Ctrl Pts',(-1.76640606389863,51.145,-5.94073262861954));
#40472=CARTESIAN_POINT('Ctrl Pts',(-1.74698425466385,51.145,-5.90906068827417));
#40473=CARTESIAN_POINT('Ctrl Pts',(-1.72912206102237,51.145,-5.87844620539466));
#40474=CARTESIAN_POINT('Ctrl Pts',(-1.71294534020681,51.145,-5.84921363316514));
#40475=CARTESIAN_POINT('Ctrl Pts',(-1.69856379474193,51.145,-5.8216513201319));
#40476=CARTESIAN_POINT('Ctrl Pts',(-1.68604879760681,51.145,-5.79595877235173));
#40477=CARTESIAN_POINT('Ctrl Pts',(-1.67543235427339,51.145,-5.77224172513534));
#40478=CARTESIAN_POINT('Ctrl Pts',(-1.66846492267669,51.145,-5.75488502996854));
#40479=CARTESIAN_POINT('Ctrl Pts',(-1.66409560210811,51.145,-5.74278027398956));
#40480=CARTESIAN_POINT('Ctrl Pts',(-1.66156260377489,51.145,-5.73511540682054));
#40481=CARTESIAN_POINT('Ctrl Pts',(-1.66039107437148,51.145,-5.73138421404289));
#40482=CARTESIAN_POINT('Origin',(0.,54.32,0.));
#40483=CARTESIAN_POINT('',(-3.34686616149372,51.145,-4.18409499139877));
#40484=CARTESIAN_POINT('Origin',(0.,51.145,0.));
#40485=CARTESIAN_POINT('',(-3.34686616149372,54.32,-4.18409499139877));
#40486=CARTESIAN_POINT('Origin',(-3.72730711280926,57.495,-4.65970441290367));
#40487=CARTESIAN_POINT('',(-3.72730711280926,51.145,-4.65970441290367));
#40488=CARTESIAN_POINT('',(-3.72730711280926,51.145,-4.65970441290367));
#40489=CARTESIAN_POINT('',(-3.72730711280926,57.495,-4.65970441290367));
#40490=CARTESIAN_POINT('Origin',(-1.15195721078055E-12,57.495,-1.15136842610855E-12));
#40491=CARTESIAN_POINT('',(-4.87380761862879,51.145,-5.22328778611671));
#40492=CARTESIAN_POINT('',(-4.87380761862879,57.495,-5.22328778611671));
#40493=CARTESIAN_POINT('',(-5.22328778611671,51.145,-4.87380761862879));
#40494=CARTESIAN_POINT('Origin',(-1.15195721078055E-12,51.145,-1.15136842610855E-12));
#40495=CARTESIAN_POINT('',(-5.22328778611671,57.495,-4.87380761862879));
#40496=CARTESIAN_POINT('Ctrl Pts',(-4.65970441290367,57.495,-3.72730711280926));
#40497=CARTESIAN_POINT('Ctrl Pts',(-4.65970441290367,49.875,-3.72730711280926));
#40498=CARTESIAN_POINT('Ctrl Pts',(-4.66270326064961,57.495,-3.72981733050576));
#40499=CARTESIAN_POINT('Ctrl Pts',(-4.66270326064961,49.875,-3.72981733050576));
#40500=CARTESIAN_POINT('Ctrl Pts',(-4.6688153380502,57.495,-3.73509073349854));
#40501=CARTESIAN_POINT('Ctrl Pts',(-4.6688153380502,49.875,-3.73509073349854));
#40502=CARTESIAN_POINT('Ctrl Pts',(-4.67832660775297,57.495,-3.7437597489088));
#40503=CARTESIAN_POINT('Ctrl Pts',(-4.67832660775297,49.875,-3.7437597489088));
#40504=CARTESIAN_POINT('Ctrl Pts',(-4.69169578253142,57.495,-3.7568389360361));
#40505=CARTESIAN_POINT('Ctrl Pts',(-4.69169578253142,49.875,-3.7568389360361));
#40506=CARTESIAN_POINT('Ctrl Pts',(-4.70954474005187,57.495,-3.77572337177426));
#40507=CARTESIAN_POINT('Ctrl Pts',(-4.70954474005187,49.875,-3.77572337177426));
#40508=CARTESIAN_POINT('Ctrl Pts',(-4.72849227702429,57.495,-3.79711783384759));
#40509=CARTESIAN_POINT('Ctrl Pts',(-4.72849227702429,49.875,-3.79711783384759));
#40510=CARTESIAN_POINT('Ctrl Pts',(-4.74845295472311,57.495,-3.82095228990398));
#40511=CARTESIAN_POINT('Ctrl Pts',(-4.74845295472311,49.875,-3.82095228990398));
#40512=CARTESIAN_POINT('Ctrl Pts',(-4.76926976684248,57.495,-3.84708445224628));
#40513=CARTESIAN_POINT('Ctrl Pts',(-4.76926976684248,49.875,-3.84708445224628));
#40514=CARTESIAN_POINT('Ctrl Pts',(-4.79071829540097,57.495,-3.87530262274579));
#40515=CARTESIAN_POINT('Ctrl Pts',(-4.79071829540097,49.875,-3.87530262274579));
#40516=CARTESIAN_POINT('Ctrl Pts',(-4.81254694822028,57.495,-3.90536636162316));
#40517=CARTESIAN_POINT('Ctrl Pts',(-4.81254694822028,49.875,-3.90536636162316));
#40518=CARTESIAN_POINT('Ctrl Pts',(-4.83450929444277,57.495,-3.93703846717723));
#40519=CARTESIAN_POINT('Ctrl Pts',(-4.83450929444277,49.875,-3.93703846717723));
#40520=CARTESIAN_POINT('Ctrl Pts',(-4.85639607415679,57.495,-3.97011673859275));
#40521=CARTESIAN_POINT('Ctrl Pts',(-4.85639607415679,49.875,-3.97011673859275));
#40522=CARTESIAN_POINT('Ctrl Pts',(-4.8780759828866,57.495,-4.00447382552398));
#40523=CARTESIAN_POINT('Ctrl Pts',(-4.8780759828866,49.875,-4.00447382552398));
#40524=CARTESIAN_POINT('Ctrl Pts',(-4.89949292161193,57.495,-4.04005493051016));
#40525=CARTESIAN_POINT('Ctrl Pts',(-4.89949292161193,49.875,-4.04005493051016));
#40526=CARTESIAN_POINT('Ctrl Pts',(-4.92063739759527,57.495,-4.07685036350543));
#40527=CARTESIAN_POINT('Ctrl Pts',(-4.92063739759527,49.875,-4.07685036350543));
#40528=CARTESIAN_POINT('Ctrl Pts',(-4.94152548435404,57.495,-4.11487510765792));
#40529=CARTESIAN_POINT('Ctrl Pts',(-4.94152548435404,49.875,-4.11487510765792));
#40530=CARTESIAN_POINT('Ctrl Pts',(-4.9621766920072,57.495,-4.15414724283855));
#40531=CARTESIAN_POINT('Ctrl Pts',(-4.9621766920072,49.875,-4.15414724283855));
#40532=CARTESIAN_POINT('Ctrl Pts',(-4.98258807456953,57.495,-4.19466216292523));
#40533=CARTESIAN_POINT('Ctrl Pts',(-4.98258807456953,49.875,-4.19466216292523));
#40534=CARTESIAN_POINT('Ctrl Pts',(-5.00273172317852,57.495,-4.23639070615327));
#40535=CARTESIAN_POINT('Ctrl Pts',(-5.00273172317852,49.875,-4.23639070615327));
#40536=CARTESIAN_POINT('Ctrl Pts',(-5.02256507114883,57.495,-4.27929023600664));
#40537=CARTESIAN_POINT('Ctrl Pts',(-5.02256507114883,49.875,-4.27929023600664));
#40538=CARTESIAN_POINT('Ctrl Pts',(-5.04203735157409,57.495,-4.32331156573186));
#40539=CARTESIAN_POINT('Ctrl Pts',(-5.04203735157409,49.875,-4.32331156573186));
#40540=CARTESIAN_POINT('Ctrl Pts',(-5.06109712122993,57.495,-4.36840670797621));
#40541=CARTESIAN_POINT('Ctrl Pts',(-5.06109712122993,49.875,-4.36840670797621));
#40542=CARTESIAN_POINT('Ctrl Pts',(-5.07970066295481,57.495,-4.41453743405689));
#40543=CARTESIAN_POINT('Ctrl Pts',(-5.07970066295481,49.875,-4.41453743405689));
#40544=CARTESIAN_POINT('Ctrl Pts',(-5.09781475579234,57.495,-4.46167734280668));
#40545=CARTESIAN_POINT('Ctrl Pts',(-5.09781475579234,49.875,-4.46167734280668));
#40546=CARTESIAN_POINT('Ctrl Pts',(-5.11541439426219,57.495,-4.50980818622117));
#40547=CARTESIAN_POINT('Ctrl Pts',(-5.11541439426219,49.875,-4.50980818622117));
#40548=CARTESIAN_POINT('Ctrl Pts',(-5.13248213818673,57.495,-4.55891761694258));
#40549=CARTESIAN_POINT('Ctrl Pts',(-5.13248213818673,49.875,-4.55891761694258));
#40550=CARTESIAN_POINT('Ctrl Pts',(-5.14900691787061,57.495,-4.60899638270436));
#40551=CARTESIAN_POINT('Ctrl Pts',(-5.14900691787061,49.875,-4.60899638270436));
#40552=CARTESIAN_POINT('Ctrl Pts',(-5.16498334493441,57.495,-4.66003509375248));
#40553=CARTESIAN_POINT('Ctrl Pts',(-5.16498334493441,49.875,-4.66003509375248));
#40554=CARTESIAN_POINT('Ctrl Pts',(-5.1804106250073,57.495,-4.71202254995837));
#40555=CARTESIAN_POINT('Ctrl Pts',(-5.1804106250073,49.875,-4.71202254995837));
#40556=CARTESIAN_POINT('Ctrl Pts',(-5.1952907728175,57.495,-4.764947890579));
#40557=CARTESIAN_POINT('Ctrl Pts',(-5.1952907728175,49.875,-4.764947890579));
#40558=CARTESIAN_POINT('Ctrl Pts',(-5.2067598214933,57.495,-4.8080309881172));
#40559=CARTESIAN_POINT('Ctrl Pts',(-5.2067598214933,49.875,-4.8080309881172));
#40560=CARTESIAN_POINT('Ctrl Pts',(-5.21511826561693,57.495,-4.84075823631811));
#40561=CARTESIAN_POINT('Ctrl Pts',(-5.21511826561693,49.875,-4.84075823631811));
#40562=CARTESIAN_POINT('Ctrl Pts',(-5.22058260535447,57.495,-4.86276047837853));
#40563=CARTESIAN_POINT('Ctrl Pts',(-5.22058260535447,49.875,-4.86276047837853));
#40564=CARTESIAN_POINT('Ctrl Pts',(-5.22328778611671,57.495,-4.87380761862879));
#40565=CARTESIAN_POINT('Ctrl Pts',(-5.22328778611671,49.875,-4.87380761862879));
#40566=CARTESIAN_POINT('',(-4.65970441290367,51.145,-3.72730711280926));
#40567=CARTESIAN_POINT('Ctrl Pts',(-4.65970441290367,51.145,-3.72730711280926));
#40568=CARTESIAN_POINT('Ctrl Pts',(-4.66270326064961,51.145,-3.72981733050576));
#40569=CARTESIAN_POINT('Ctrl Pts',(-4.6688153380502,51.145,-3.73509073349854));
#40570=CARTESIAN_POINT('Ctrl Pts',(-4.67832660775297,51.145,-3.7437597489088));
#40571=CARTESIAN_POINT('Ctrl Pts',(-4.69169578253142,51.145,-3.7568389360361));
#40572=CARTESIAN_POINT('Ctrl Pts',(-4.70954474005187,51.145,-3.77572337177426));
#40573=CARTESIAN_POINT('Ctrl Pts',(-4.72849227702429,51.145,-3.79711783384759));
#40574=CARTESIAN_POINT('Ctrl Pts',(-4.74845295472311,51.145,-3.82095228990398));
#40575=CARTESIAN_POINT('Ctrl Pts',(-4.76926976684248,51.145,-3.84708445224628));
#40576=CARTESIAN_POINT('Ctrl Pts',(-4.79071829540097,51.145,-3.87530262274579));
#40577=CARTESIAN_POINT('Ctrl Pts',(-4.81254694822028,51.145,-3.90536636162316));
#40578=CARTESIAN_POINT('Ctrl Pts',(-4.83450929444277,51.145,-3.93703846717723));
#40579=CARTESIAN_POINT('Ctrl Pts',(-4.85639607415679,51.145,-3.97011673859275));
#40580=CARTESIAN_POINT('Ctrl Pts',(-4.8780759828866,51.145,-4.00447382552398));
#40581=CARTESIAN_POINT('Ctrl Pts',(-4.89949292161193,51.145,-4.04005493051016));
#40582=CARTESIAN_POINT('Ctrl Pts',(-4.92063739759527,51.145,-4.07685036350543));
#40583=CARTESIAN_POINT('Ctrl Pts',(-4.94152548435404,51.145,-4.11487510765792));
#40584=CARTESIAN_POINT('Ctrl Pts',(-4.9621766920072,51.145,-4.15414724283855));
#40585=CARTESIAN_POINT('Ctrl Pts',(-4.98258807456953,51.145,-4.19466216292523));
#40586=CARTESIAN_POINT('Ctrl Pts',(-5.00273172317852,51.145,-4.23639070615327));
#40587=CARTESIAN_POINT('Ctrl Pts',(-5.02256507114883,51.145,-4.27929023600664));
#40588=CARTESIAN_POINT('Ctrl Pts',(-5.04203735157409,51.145,-4.32331156573186));
#40589=CARTESIAN_POINT('Ctrl Pts',(-5.06109712122993,51.145,-4.36840670797621));
#40590=CARTESIAN_POINT('Ctrl Pts',(-5.07970066295481,51.145,-4.41453743405689));
#40591=CARTESIAN_POINT('Ctrl Pts',(-5.09781475579234,51.145,-4.46167734280668));
#40592=CARTESIAN_POINT('Ctrl Pts',(-5.11541439426219,51.145,-4.50980818622117));
#40593=CARTESIAN_POINT('Ctrl Pts',(-5.13248213818673,51.145,-4.55891761694258));
#40594=CARTESIAN_POINT('Ctrl Pts',(-5.14900691787061,51.145,-4.60899638270436));
#40595=CARTESIAN_POINT('Ctrl Pts',(-5.16498334493441,51.145,-4.66003509375248));
#40596=CARTESIAN_POINT('Ctrl Pts',(-5.1804106250073,51.145,-4.71202254995837));
#40597=CARTESIAN_POINT('Ctrl Pts',(-5.1952907728175,51.145,-4.764947890579));
#40598=CARTESIAN_POINT('Ctrl Pts',(-5.2067598214933,51.145,-4.8080309881172));
#40599=CARTESIAN_POINT('Ctrl Pts',(-5.21511826561693,51.145,-4.84075823631811));
#40600=CARTESIAN_POINT('Ctrl Pts',(-5.22058260535447,51.145,-4.86276047837853));
#40601=CARTESIAN_POINT('Ctrl Pts',(-5.22328778611671,51.145,-4.87380761862879));
#40602=CARTESIAN_POINT('',(-4.65970441290367,57.495,-3.72730711280926));
#40603=CARTESIAN_POINT('Origin',(-4.06695907338649,57.495,-3.25316890053365));
#40604=CARTESIAN_POINT('',(-4.18409499139877,51.145,-3.34686616149372));
#40605=CARTESIAN_POINT('',(-4.18409499139877,54.32,-3.34686616149372));
#40606=CARTESIAN_POINT('',(-4.06695907338649,51.145,-3.25316890053365));
#40607=CARTESIAN_POINT('Ctrl Pts',(-4.87380761862879,57.495,-5.22328778611671));
#40608=CARTESIAN_POINT('Ctrl Pts',(-4.87380761862879,49.875,-5.22328778611671));
#40609=CARTESIAN_POINT('Ctrl Pts',(-4.86276047837859,57.495,-5.2205826053545));
#40610=CARTESIAN_POINT('Ctrl Pts',(-4.86276047837859,49.875,-5.2205826053545));
#40611=CARTESIAN_POINT('Ctrl Pts',(-4.84075823631825,57.495,-5.21511826561704));
#40612=CARTESIAN_POINT('Ctrl Pts',(-4.84075823631825,49.875,-5.21511826561704));
#40613=CARTESIAN_POINT('Ctrl Pts',(-4.80803098811744,57.495,-5.20675982149348));
#40614=CARTESIAN_POINT('Ctrl Pts',(-4.80803098811744,49.875,-5.20675982149348));
#40615=CARTESIAN_POINT('Ctrl Pts',(-4.7649478905793,57.495,-5.19529077281773));
#40616=CARTESIAN_POINT('Ctrl Pts',(-4.7649478905793,49.875,-5.19529077281773));
#40617=CARTESIAN_POINT('Ctrl Pts',(-4.71202254995864,57.495,-5.18041062500752));
#40618=CARTESIAN_POINT('Ctrl Pts',(-4.71202254995864,49.875,-5.18041062500752));
#40619=CARTESIAN_POINT('Ctrl Pts',(-4.66003509375265,57.495,-5.16498334493456));
#40620=CARTESIAN_POINT('Ctrl Pts',(-4.66003509375265,49.875,-5.16498334493456));
#40621=CARTESIAN_POINT('Ctrl Pts',(-4.60899638270439,57.495,-5.14900691787064));
#40622=CARTESIAN_POINT('Ctrl Pts',(-4.60899638270439,49.875,-5.14900691787064));
#40623=CARTESIAN_POINT('Ctrl Pts',(-4.5589176169425,57.495,-5.13248213818666));
#40624=CARTESIAN_POINT('Ctrl Pts',(-4.5589176169425,49.875,-5.13248213818666));
#40625=CARTESIAN_POINT('Ctrl Pts',(-4.50980818622101,57.495,-5.11541439426204));
#40626=CARTESIAN_POINT('Ctrl Pts',(-4.50980818622101,49.875,-5.11541439426204));
#40627=CARTESIAN_POINT('Ctrl Pts',(-4.4616773428065,57.495,-5.09781475579217));
#40628=CARTESIAN_POINT('Ctrl Pts',(-4.4616773428065,49.875,-5.09781475579217));
#40629=CARTESIAN_POINT('Ctrl Pts',(-4.41453743405677,57.495,-5.07970066295468));
#40630=CARTESIAN_POINT('Ctrl Pts',(-4.41453743405677,49.875,-5.07970066295468));
#40631=CARTESIAN_POINT('Ctrl Pts',(-4.36840670797617,57.495,-5.06109712122989));
#40632=CARTESIAN_POINT('Ctrl Pts',(-4.36840670797617,49.875,-5.06109712122989));
#40633=CARTESIAN_POINT('Ctrl Pts',(-4.3233115657319,57.495,-5.04203735157413));
#40634=CARTESIAN_POINT('Ctrl Pts',(-4.3233115657319,49.875,-5.04203735157413));
#40635=CARTESIAN_POINT('Ctrl Pts',(-4.27929023600674,57.495,-5.02256507114894));
#40636=CARTESIAN_POINT('Ctrl Pts',(-4.27929023600674,49.875,-5.02256507114894));
#40637=CARTESIAN_POINT('Ctrl Pts',(-4.23639070615337,57.495,-5.00273172317863));
#40638=CARTESIAN_POINT('Ctrl Pts',(-4.23639070615337,49.875,-5.00273172317863));
#40639=CARTESIAN_POINT('Ctrl Pts',(-4.1946621629253,57.495,-4.98258807456961));
#40640=CARTESIAN_POINT('Ctrl Pts',(-4.1946621629253,49.875,-4.98258807456961));
#40641=CARTESIAN_POINT('Ctrl Pts',(-4.15414724283858,57.495,-4.96217669200723));
#40642=CARTESIAN_POINT('Ctrl Pts',(-4.15414724283858,49.875,-4.96217669200723));
#40643=CARTESIAN_POINT('Ctrl Pts',(-4.11487510765791,57.495,-4.94152548435402));
#40644=CARTESIAN_POINT('Ctrl Pts',(-4.11487510765791,49.875,-4.94152548435402));
#40645=CARTESIAN_POINT('Ctrl Pts',(-4.07685036350539,57.495,-4.92063739759521));
#40646=CARTESIAN_POINT('Ctrl Pts',(-4.07685036350539,49.875,-4.92063739759521));
#40647=CARTESIAN_POINT('Ctrl Pts',(-4.04005493051012,57.495,-4.89949292161185));
#40648=CARTESIAN_POINT('Ctrl Pts',(-4.04005493051012,49.875,-4.89949292161185));
#40649=CARTESIAN_POINT('Ctrl Pts',(-4.00447382552396,57.495,-4.87807598288654));
#40650=CARTESIAN_POINT('Ctrl Pts',(-4.00447382552396,49.875,-4.87807598288654));
#40651=CARTESIAN_POINT('Ctrl Pts',(-3.97011673859274,57.495,-4.85639607415676));
#40652=CARTESIAN_POINT('Ctrl Pts',(-3.97011673859274,49.875,-4.85639607415676));
#40653=CARTESIAN_POINT('Ctrl Pts',(-3.93703846717724,57.495,-4.83450929444279));
#40654=CARTESIAN_POINT('Ctrl Pts',(-3.93703846717724,49.875,-4.83450929444279));
#40655=CARTESIAN_POINT('Ctrl Pts',(-3.90536636162318,57.495,-4.81254694822034));
#40656=CARTESIAN_POINT('Ctrl Pts',(-3.90536636162318,49.875,-4.81254694822034));
#40657=CARTESIAN_POINT('Ctrl Pts',(-3.8753026227458,57.495,-4.79071829540103));
#40658=CARTESIAN_POINT('Ctrl Pts',(-3.8753026227458,49.875,-4.79071829540103));
#40659=CARTESIAN_POINT('Ctrl Pts',(-3.84708445224627,57.495,-4.76926976684252));
#40660=CARTESIAN_POINT('Ctrl Pts',(-3.84708445224627,49.875,-4.76926976684252));
#40661=CARTESIAN_POINT('Ctrl Pts',(-3.82095228990397,57.495,-4.74845295472312));
#40662=CARTESIAN_POINT('Ctrl Pts',(-3.82095228990397,49.875,-4.74845295472312));
#40663=CARTESIAN_POINT('Ctrl Pts',(-3.7971178338476,57.495,-4.72849227702427));
#40664=CARTESIAN_POINT('Ctrl Pts',(-3.7971178338476,49.875,-4.72849227702427));
#40665=CARTESIAN_POINT('Ctrl Pts',(-3.77572337177431,57.495,-4.7095447400518));
#40666=CARTESIAN_POINT('Ctrl Pts',(-3.77572337177431,49.875,-4.7095447400518));
#40667=CARTESIAN_POINT('Ctrl Pts',(-3.75683893603616,57.495,-4.69169578253132));
#40668=CARTESIAN_POINT('Ctrl Pts',(-3.75683893603616,49.875,-4.69169578253132));
#40669=CARTESIAN_POINT('Ctrl Pts',(-3.74375974890886,57.495,-4.67832660775287));
#40670=CARTESIAN_POINT('Ctrl Pts',(-3.74375974890886,49.875,-4.67832660775287));
#40671=CARTESIAN_POINT('Ctrl Pts',(-3.73509073349858,57.495,-4.66881533805013));
#40672=CARTESIAN_POINT('Ctrl Pts',(-3.73509073349858,49.875,-4.66881533805013));
#40673=CARTESIAN_POINT('Ctrl Pts',(-3.72981733050578,57.495,-4.66270326064959));
#40674=CARTESIAN_POINT('Ctrl Pts',(-3.72981733050578,49.875,-4.66270326064959));
#40675=CARTESIAN_POINT('Ctrl Pts',(-3.72730711280926,57.495,-4.65970441290367));
#40676=CARTESIAN_POINT('Ctrl Pts',(-3.72730711280926,49.875,-4.65970441290367));
#40677=CARTESIAN_POINT('Ctrl Pts',(-4.87380761862879,51.145,-5.22328778611671));
#40678=CARTESIAN_POINT('Ctrl Pts',(-4.86276047837859,51.145,-5.2205826053545));
#40679=CARTESIAN_POINT('Ctrl Pts',(-4.84075823631825,51.145,-5.21511826561704));
#40680=CARTESIAN_POINT('Ctrl Pts',(-4.80803098811744,51.145,-5.20675982149348));
#40681=CARTESIAN_POINT('Ctrl Pts',(-4.7649478905793,51.145,-5.19529077281773));
#40682=CARTESIAN_POINT('Ctrl Pts',(-4.71202254995864,51.145,-5.18041062500752));
#40683=CARTESIAN_POINT('Ctrl Pts',(-4.66003509375265,51.145,-5.16498334493456));
#40684=CARTESIAN_POINT('Ctrl Pts',(-4.60899638270439,51.145,-5.14900691787064));
#40685=CARTESIAN_POINT('Ctrl Pts',(-4.5589176169425,51.145,-5.13248213818666));
#40686=CARTESIAN_POINT('Ctrl Pts',(-4.50980818622101,51.145,-5.11541439426204));
#40687=CARTESIAN_POINT('Ctrl Pts',(-4.4616773428065,51.145,-5.09781475579217));
#40688=CARTESIAN_POINT('Ctrl Pts',(-4.41453743405677,51.145,-5.07970066295468));
#40689=CARTESIAN_POINT('Ctrl Pts',(-4.36840670797617,51.145,-5.06109712122989));
#40690=CARTESIAN_POINT('Ctrl Pts',(-4.3233115657319,51.145,-5.04203735157413));
#40691=CARTESIAN_POINT('Ctrl Pts',(-4.27929023600674,51.145,-5.02256507114894));
#40692=CARTESIAN_POINT('Ctrl Pts',(-4.23639070615337,51.145,-5.00273172317863));
#40693=CARTESIAN_POINT('Ctrl Pts',(-4.1946621629253,51.145,-4.98258807456961));
#40694=CARTESIAN_POINT('Ctrl Pts',(-4.15414724283858,51.145,-4.96217669200723));
#40695=CARTESIAN_POINT('Ctrl Pts',(-4.11487510765791,51.145,-4.94152548435402));
#40696=CARTESIAN_POINT('Ctrl Pts',(-4.07685036350539,51.145,-4.92063739759521));
#40697=CARTESIAN_POINT('Ctrl Pts',(-4.04005493051012,51.145,-4.89949292161185));
#40698=CARTESIAN_POINT('Ctrl Pts',(-4.00447382552396,51.145,-4.87807598288654));
#40699=CARTESIAN_POINT('Ctrl Pts',(-3.97011673859274,51.145,-4.85639607415676));
#40700=CARTESIAN_POINT('Ctrl Pts',(-3.93703846717724,51.145,-4.83450929444279));
#40701=CARTESIAN_POINT('Ctrl Pts',(-3.90536636162318,51.145,-4.81254694822034));
#40702=CARTESIAN_POINT('Ctrl Pts',(-3.8753026227458,51.145,-4.79071829540103));
#40703=CARTESIAN_POINT('Ctrl Pts',(-3.84708445224627,51.145,-4.76926976684252));
#40704=CARTESIAN_POINT('Ctrl Pts',(-3.82095228990397,51.145,-4.74845295472312));
#40705=CARTESIAN_POINT('Ctrl Pts',(-3.7971178338476,51.145,-4.72849227702427));
#40706=CARTESIAN_POINT('Ctrl Pts',(-3.77572337177431,51.145,-4.7095447400518));
#40707=CARTESIAN_POINT('Ctrl Pts',(-3.75683893603616,51.145,-4.69169578253132));
#40708=CARTESIAN_POINT('Ctrl Pts',(-3.74375974890886,51.145,-4.67832660775287));
#40709=CARTESIAN_POINT('Ctrl Pts',(-3.73509073349858,51.145,-4.66881533805013));
#40710=CARTESIAN_POINT('Ctrl Pts',(-3.72981733050578,51.145,-4.66270326064959));
#40711=CARTESIAN_POINT('Ctrl Pts',(-3.72730711280926,51.145,-4.65970441290367));
#40712=CARTESIAN_POINT('Origin',(0.,54.32,0.));
#40713=CARTESIAN_POINT('',(-4.69328497730872,51.145,-2.58480949428933));
#40714=CARTESIAN_POINT('Origin',(0.,51.145,0.));
#40715=CARTESIAN_POINT('',(-4.69328497730872,54.32,-2.58480949428933));
#40716=CARTESIAN_POINT('Origin',(-5.22677443144495,57.495,-2.87862685522556));
#40717=CARTESIAN_POINT('',(-5.22677443144495,51.145,-2.87862685522556));
#40718=CARTESIAN_POINT('',(-5.22677443144495,51.145,-2.87862685522556));
#40719=CARTESIAN_POINT('',(-5.22677443144495,57.495,-2.87862685522556));
#40720=CARTESIAN_POINT('Origin',(-1.50487931058895E-12,57.495,-6.22890783902202E-13));
#40721=CARTESIAN_POINT('',(-6.50167680247051,51.145,-2.96056324982543));
#40722=CARTESIAN_POINT('',(-6.50167680247051,57.495,-2.96056324982543));
#40723=CARTESIAN_POINT('',(-6.69081410619341,51.145,-2.50394540602692));
#40724=CARTESIAN_POINT('Origin',(-1.50487931058895E-12,51.145,-6.22890783902202E-13));
#40725=CARTESIAN_POINT('',(-6.69081410619341,57.495,-2.50394540602692));
#40726=CARTESIAN_POINT('Ctrl Pts',(-5.73138421404289,57.495,-1.66039107437148));
#40727=CARTESIAN_POINT('Ctrl Pts',(-5.73138421404289,49.875,-1.66039107437148));
#40728=CARTESIAN_POINT('Ctrl Pts',(-5.73511540682056,57.495,-1.66156260377487));
#40729=CARTESIAN_POINT('Ctrl Pts',(-5.73511540682056,49.875,-1.66156260377487));
#40730=CARTESIAN_POINT('Ctrl Pts',(-5.7427802739896,57.495,-1.66409560210805));
#40731=CARTESIAN_POINT('Ctrl Pts',(-5.7427802739896,49.875,-1.66409560210805));
#40732=CARTESIAN_POINT('Ctrl Pts',(-5.75488502996861,57.495,-1.6684649226766));
#40733=CARTESIAN_POINT('Ctrl Pts',(-5.75488502996861,49.875,-1.6684649226766));
#40734=CARTESIAN_POINT('Ctrl Pts',(-5.77224172513541,57.495,-1.67543235427329));
#40735=CARTESIAN_POINT('Ctrl Pts',(-5.77224172513541,49.875,-1.67543235427329));
#40736=CARTESIAN_POINT('Ctrl Pts',(-5.79595877235177,57.495,-1.68604879760674));
#40737=CARTESIAN_POINT('Ctrl Pts',(-5.79595877235177,49.875,-1.68604879760674));
#40738=CARTESIAN_POINT('Ctrl Pts',(-5.82165132013192,57.495,-1.69856379474191));
#40739=CARTESIAN_POINT('Ctrl Pts',(-5.82165132013192,49.875,-1.69856379474191));
#40740=CARTESIAN_POINT('Ctrl Pts',(-5.84921363316513,57.495,-1.71294534020683));
#40741=CARTESIAN_POINT('Ctrl Pts',(-5.84921363316513,49.875,-1.71294534020683));
#40742=CARTESIAN_POINT('Ctrl Pts',(-5.87844620539462,57.495,-1.7291220610224));
#40743=CARTESIAN_POINT('Ctrl Pts',(-5.87844620539462,49.875,-1.7291220610224));
#40744=CARTESIAN_POINT('Ctrl Pts',(-5.90906068827411,57.495,-1.74698425466387));
#40745=CARTESIAN_POINT('Ctrl Pts',(-5.90906068827411,49.875,-1.74698425466387));
#40746=CARTESIAN_POINT('Ctrl Pts',(-5.94073262861949,57.495,-1.76640606389864));
#40747=CARTESIAN_POINT('Ctrl Pts',(-5.94073262861949,49.875,-1.76640606389864));
#40748=CARTESIAN_POINT('Ctrl Pts',(-5.97314358084403,57.495,-1.78726264793636));
#40749=CARTESIAN_POINT('Ctrl Pts',(-5.97314358084403,49.875,-1.78726264793636));
#40750=CARTESIAN_POINT('Ctrl Pts',(-6.00602283509639,57.495,-1.80944727788364));
#40751=CARTESIAN_POINT('Ctrl Pts',(-6.00602283509639,49.875,-1.80944727788364));
#40752=CARTESIAN_POINT('Ctrl Pts',(-6.03920034699149,57.495,-1.83289254541003));
#40753=CARTESIAN_POINT('Ctrl Pts',(-6.03920034699149,49.875,-1.83289254541003));
#40754=CARTESIAN_POINT('Ctrl Pts',(-6.07260331771232,57.495,-1.85756929242873));
#40755=CARTESIAN_POINT('Ctrl Pts',(-6.07260331771232,49.875,-1.85756929242873));
#40756=CARTESIAN_POINT('Ctrl Pts',(-6.10621926889299,57.495,-1.88347219921808));
#40757=CARTESIAN_POINT('Ctrl Pts',(-6.10621926889299,49.875,-1.88347219921808));
#40758=CARTESIAN_POINT('Ctrl Pts',(-6.14006878432982,57.495,-1.91060895733317));
#40759=CARTESIAN_POINT('Ctrl Pts',(-6.14006878432982,49.875,-1.91060895733317));
#40760=CARTESIAN_POINT('Ctrl Pts',(-6.17417680788945,57.495,-1.93898880419737));
#40761=CARTESIAN_POINT('Ctrl Pts',(-6.17417680788945,49.875,-1.93898880419737));
#40762=CARTESIAN_POINT('Ctrl Pts',(-6.20853885514981,57.495,-1.96860861168851));
#40763=CARTESIAN_POINT('Ctrl Pts',(-6.20853885514981,49.875,-1.96860861168851));
#40764=CARTESIAN_POINT('Ctrl Pts',(-6.24311798195985,57.495,-1.99945211810837));
#40765=CARTESIAN_POINT('Ctrl Pts',(-6.24311798195985,49.875,-1.99945211810837));
#40766=CARTESIAN_POINT('Ctrl Pts',(-6.27785854554194,57.495,-2.03149622201768));
#40767=CARTESIAN_POINT('Ctrl Pts',(-6.27785854554194,49.875,-2.03149622201768));
#40768=CARTESIAN_POINT('Ctrl Pts',(-6.31269482043467,57.495,-2.06471490843563));
#40769=CARTESIAN_POINT('Ctrl Pts',(-6.31269482043467,49.875,-2.06471490843563));
#40770=CARTESIAN_POINT('Ctrl Pts',(-6.34756091533115,57.495,-2.09908352929888));
#40771=CARTESIAN_POINT('Ctrl Pts',(-6.34756091533115,49.875,-2.09908352929888));
#40772=CARTESIAN_POINT('Ctrl Pts',(-6.38240181135703,57.495,-2.13458349574329));
#40773=CARTESIAN_POINT('Ctrl Pts',(-6.38240181135703,49.875,-2.13458349574329));
#40774=CARTESIAN_POINT('Ctrl Pts',(-6.41717671306138,57.495,-2.17120312938042));
#40775=CARTESIAN_POINT('Ctrl Pts',(-6.41717671306138,49.875,-2.17120312938042));
#40776=CARTESIAN_POINT('Ctrl Pts',(-6.45185553518375,57.495,-2.20893514043555));
#40777=CARTESIAN_POINT('Ctrl Pts',(-6.45185553518375,49.875,-2.20893514043555));
#40778=CARTESIAN_POINT('Ctrl Pts',(-6.48641743997175,57.495,-2.24777479550457));
#40779=CARTESIAN_POINT('Ctrl Pts',(-6.48641743997175,49.875,-2.24777479550457));
#40780=CARTESIAN_POINT('Ctrl Pts',(-6.52084865967127,57.495,-2.2877177827968));
#40781=CARTESIAN_POINT('Ctrl Pts',(-6.52084865967127,49.875,-2.2877177827968));
#40782=CARTESIAN_POINT('Ctrl Pts',(-6.55514062276556,57.495,-2.32875748935421));
#40783=CARTESIAN_POINT('Ctrl Pts',(-6.55514062276556,49.875,-2.32875748935421));
#40784=CARTESIAN_POINT('Ctrl Pts',(-6.58928830924802,57.495,-2.37088387159981));
#40785=CARTESIAN_POINT('Ctrl Pts',(-6.58928830924802,49.875,-2.37088387159981));
#40786=CARTESIAN_POINT('Ctrl Pts',(-6.6232894242584,57.495,-2.41408612451229));
#40787=CARTESIAN_POINT('Ctrl Pts',(-6.6232894242584,49.875,-2.41408612451229));
#40788=CARTESIAN_POINT('Ctrl Pts',(-6.65037263123018,57.495,-2.4495007016118));
#40789=CARTESIAN_POINT('Ctrl Pts',(-6.65037263123018,49.875,-2.4495007016118));
#40790=CARTESIAN_POINT('Ctrl Pts',(-6.67061900235304,57.495,-2.47653809829358));
#40791=CARTESIAN_POINT('Ctrl Pts',(-6.67061900235304,49.875,-2.47653809829358));
#40792=CARTESIAN_POINT('Ctrl Pts',(-6.68408728750664,57.495,-2.49477440711619));
#40793=CARTESIAN_POINT('Ctrl Pts',(-6.68408728750664,49.875,-2.49477440711619));
#40794=CARTESIAN_POINT('Ctrl Pts',(-6.69081410619341,57.495,-2.50394540602692));
#40795=CARTESIAN_POINT('Ctrl Pts',(-6.69081410619341,49.875,-2.50394540602692));
#40796=CARTESIAN_POINT('',(-5.73138421404289,51.145,-1.66039107437148));
#40797=CARTESIAN_POINT('Ctrl Pts',(-5.73138421404289,51.145,-1.66039107437148));
#40798=CARTESIAN_POINT('Ctrl Pts',(-5.73511540682056,51.145,-1.66156260377487));
#40799=CARTESIAN_POINT('Ctrl Pts',(-5.7427802739896,51.145,-1.66409560210805));
#40800=CARTESIAN_POINT('Ctrl Pts',(-5.75488502996861,51.145,-1.6684649226766));
#40801=CARTESIAN_POINT('Ctrl Pts',(-5.77224172513541,51.145,-1.67543235427329));
#40802=CARTESIAN_POINT('Ctrl Pts',(-5.79595877235177,51.145,-1.68604879760674));
#40803=CARTESIAN_POINT('Ctrl Pts',(-5.82165132013192,51.145,-1.69856379474191));
#40804=CARTESIAN_POINT('Ctrl Pts',(-5.84921363316513,51.145,-1.71294534020683));
#40805=CARTESIAN_POINT('Ctrl Pts',(-5.87844620539462,51.145,-1.7291220610224));
#40806=CARTESIAN_POINT('Ctrl Pts',(-5.90906068827411,51.145,-1.74698425466387));
#40807=CARTESIAN_POINT('Ctrl Pts',(-5.94073262861949,51.145,-1.76640606389864));
#40808=CARTESIAN_POINT('Ctrl Pts',(-5.97314358084403,51.145,-1.78726264793636));
#40809=CARTESIAN_POINT('Ctrl Pts',(-6.00602283509639,51.145,-1.80944727788364));
#40810=CARTESIAN_POINT('Ctrl Pts',(-6.03920034699149,51.145,-1.83289254541003));
#40811=CARTESIAN_POINT('Ctrl Pts',(-6.07260331771232,51.145,-1.85756929242873));
#40812=CARTESIAN_POINT('Ctrl Pts',(-6.10621926889299,51.145,-1.88347219921808));
#40813=CARTESIAN_POINT('Ctrl Pts',(-6.14006878432982,51.145,-1.91060895733317));
#40814=CARTESIAN_POINT('Ctrl Pts',(-6.17417680788945,51.145,-1.93898880419737));
#40815=CARTESIAN_POINT('Ctrl Pts',(-6.20853885514981,51.145,-1.96860861168851));
#40816=CARTESIAN_POINT('Ctrl Pts',(-6.24311798195985,51.145,-1.99945211810837));
#40817=CARTESIAN_POINT('Ctrl Pts',(-6.27785854554194,51.145,-2.03149622201768));
#40818=CARTESIAN_POINT('Ctrl Pts',(-6.31269482043467,51.145,-2.06471490843563));
#40819=CARTESIAN_POINT('Ctrl Pts',(-6.34756091533115,51.145,-2.09908352929888));
#40820=CARTESIAN_POINT('Ctrl Pts',(-6.38240181135703,51.145,-2.13458349574329));
#40821=CARTESIAN_POINT('Ctrl Pts',(-6.41717671306138,51.145,-2.17120312938042));
#40822=CARTESIAN_POINT('Ctrl Pts',(-6.45185553518375,51.145,-2.20893514043555));
#40823=CARTESIAN_POINT('Ctrl Pts',(-6.48641743997175,51.145,-2.24777479550457));
#40824=CARTESIAN_POINT('Ctrl Pts',(-6.52084865967127,51.145,-2.2877177827968));
#40825=CARTESIAN_POINT('Ctrl Pts',(-6.55514062276556,51.145,-2.32875748935421));
#40826=CARTESIAN_POINT('Ctrl Pts',(-6.58928830924802,51.145,-2.37088387159981));
#40827=CARTESIAN_POINT('Ctrl Pts',(-6.6232894242584,51.145,-2.41408612451229));
#40828=CARTESIAN_POINT('Ctrl Pts',(-6.65037263123018,51.145,-2.4495007016118));
#40829=CARTESIAN_POINT('Ctrl Pts',(-6.67061900235304,51.145,-2.47653809829358));
#40830=CARTESIAN_POINT('Ctrl Pts',(-6.68408728750664,51.145,-2.49477440711619));
#40831=CARTESIAN_POINT('Ctrl Pts',(-6.69081410619341,51.145,-2.50394540602692));
#40832=CARTESIAN_POINT('',(-5.73138421404289,57.495,-1.66039107437148));
#40833=CARTESIAN_POINT('Origin',(-5.00231408838243,57.495,-1.44917830551339));
#40834=CARTESIAN_POINT('',(-5.1463899549833,51.145,-1.4909173120086));
#40835=CARTESIAN_POINT('',(-5.1463899549833,54.32,-1.4909173120086));
#40836=CARTESIAN_POINT('',(-5.00231408838243,51.145,-1.44917830551339));
#40837=CARTESIAN_POINT('Ctrl Pts',(-6.50167680247051,57.495,-2.96056324982543));
#40838=CARTESIAN_POINT('Ctrl Pts',(-6.50167680247051,49.875,-2.96056324982543));
#40839=CARTESIAN_POINT('Ctrl Pts',(-6.49043534784131,57.495,-2.96229154623625));
#40840=CARTESIAN_POINT('Ctrl Pts',(-6.49043534784131,49.875,-2.96229154623625));
#40841=CARTESIAN_POINT('Ctrl Pts',(-6.46801681444607,57.495,-2.96566304810549));
#40842=CARTESIAN_POINT('Ctrl Pts',(-6.46801681444607,49.875,-2.96566304810549));
#40843=CARTESIAN_POINT('Ctrl Pts',(-6.43458214159149,57.495,-2.97046502832945));
#40844=CARTESIAN_POINT('Ctrl Pts',(-6.43458214159149,49.875,-2.97046502832945));
#40845=CARTESIAN_POINT('Ctrl Pts',(-6.39038953466561,57.495,-2.97635619664337));
#40846=CARTESIAN_POINT('Ctrl Pts',(-6.39038953466561,49.875,-2.97635619664337));
#40847=CARTESIAN_POINT('Ctrl Pts',(-6.33579850967689,57.495,-2.98286238364857));
#40848=CARTESIAN_POINT('Ctrl Pts',(-6.33579850967689,49.875,-2.98286238364857));
#40849=CARTESIAN_POINT('Ctrl Pts',(-6.28186459845047,57.495,-2.98850417352769));
#40850=CARTESIAN_POINT('Ctrl Pts',(-6.28186459845047,49.875,-2.98850417352769));
#40851=CARTESIAN_POINT('Ctrl Pts',(-6.22859706400147,57.495,-2.99327554868811));
#40852=CARTESIAN_POINT('Ctrl Pts',(-6.22859706400147,49.875,-2.99327554868811));
#40853=CARTESIAN_POINT('Ctrl Pts',(-6.17600655789209,57.495,-2.99717295692919));
#40854=CARTESIAN_POINT('Ctrl Pts',(-6.17600655789209,49.875,-2.99717295692919));
#40855=CARTESIAN_POINT('Ctrl Pts',(-6.12410381716742,57.495,-3.00019778316108));
#40856=CARTESIAN_POINT('Ctrl Pts',(-6.12410381716742,49.875,-3.00019778316108));
#40857=CARTESIAN_POINT('Ctrl Pts',(-6.07290162599622,57.495,-3.00235671375967));
#40858=CARTESIAN_POINT('Ctrl Pts',(-6.07290162599622,49.875,-3.00235671375967));
#40859=CARTESIAN_POINT('Ctrl Pts',(-6.02241806591666,57.495,-3.00366113621883));
#40860=CARTESIAN_POINT('Ctrl Pts',(-6.02241806591666,49.875,-3.00366113621883));
#40861=CARTESIAN_POINT('Ctrl Pts',(-5.97267956506952,57.495,-3.00412716938109));
#40862=CARTESIAN_POINT('Ctrl Pts',(-5.97267956506952,49.875,-3.00412716938109));
#40863=CARTESIAN_POINT('Ctrl Pts',(-5.9237232280624,57.495,-3.00377540211877));
#40864=CARTESIAN_POINT('Ctrl Pts',(-5.9237232280624,49.875,-3.00377540211877));
#40865=CARTESIAN_POINT('Ctrl Pts',(-5.87560110342631,57.495,-3.00263159433912));
#40866=CARTESIAN_POINT('Ctrl Pts',(-5.87560110342631,49.875,-3.00263159433912));
#40867=CARTESIAN_POINT('Ctrl Pts',(-5.82837721216385,57.495,-3.00072490941932));
#40868=CARTESIAN_POINT('Ctrl Pts',(-5.82837721216385,49.875,-3.00072490941932));
#40869=CARTESIAN_POINT('Ctrl Pts',(-5.78211642456387,57.495,-2.99808342690946));
#40870=CARTESIAN_POINT('Ctrl Pts',(-5.78211642456387,49.875,-2.99808342690946));
#40871=CARTESIAN_POINT('Ctrl Pts',(-5.73687442119613,57.495,-2.9947301570106));
#40872=CARTESIAN_POINT('Ctrl Pts',(-5.73687442119613,49.875,-2.9947301570106));
#40873=CARTESIAN_POINT('Ctrl Pts',(-5.69268882427748,57.495,-2.9906797244254));
#40874=CARTESIAN_POINT('Ctrl Pts',(-5.69268882427748,49.875,-2.9906797244254));
#40875=CARTESIAN_POINT('Ctrl Pts',(-5.64956501668959,57.495,-2.98593308820271));
#40876=CARTESIAN_POINT('Ctrl Pts',(-5.64956501668959,49.875,-2.98593308820271));
#40877=CARTESIAN_POINT('Ctrl Pts',(-5.6074788286105,57.495,-2.98047914221));
#40878=CARTESIAN_POINT('Ctrl Pts',(-5.6074788286105,49.875,-2.98047914221));
#40879=CARTESIAN_POINT('Ctrl Pts',(-5.56641026634749,57.495,-2.97430877025609));
#40880=CARTESIAN_POINT('Ctrl Pts',(-5.56641026634749,49.875,-2.97430877025609));
#40881=CARTESIAN_POINT('Ctrl Pts',(-5.52637191504895,57.495,-2.96742703426683));
#40882=CARTESIAN_POINT('Ctrl Pts',(-5.52637191504895,49.875,-2.96742703426683));
#40883=CARTESIAN_POINT('Ctrl Pts',(-5.48743586913296,57.495,-2.9598647928985));
#40884=CARTESIAN_POINT('Ctrl Pts',(-5.48743586913296,49.875,-2.9598647928985));
#40885=CARTESIAN_POINT('Ctrl Pts',(-5.44977003302482,57.495,-2.95169462080131));
#40886=CARTESIAN_POINT('Ctrl Pts',(-5.44977003302482,49.875,-2.95169462080131));
#40887=CARTESIAN_POINT('Ctrl Pts',(-5.41364129622045,57.495,-2.94303247002258));
#40888=CARTESIAN_POINT('Ctrl Pts',(-5.41364129622045,49.875,-2.94303247002258));
#40889=CARTESIAN_POINT('Ctrl Pts',(-5.37936310952307,57.495,-2.93401523982671));
#40890=CARTESIAN_POINT('Ctrl Pts',(-5.37936310952307,49.875,-2.93401523982671));
#40891=CARTESIAN_POINT('Ctrl Pts',(-5.34725389048201,57.495,-2.92478335875774));
#40892=CARTESIAN_POINT('Ctrl Pts',(-5.34725389048201,49.875,-2.92478335875774));
#40893=CARTESIAN_POINT('Ctrl Pts',(-5.31759510370885,57.495,-2.91546314862891));
#40894=CARTESIAN_POINT('Ctrl Pts',(-5.31759510370885,49.875,-2.91546314862891));
#40895=CARTESIAN_POINT('Ctrl Pts',(-5.29057828960676,57.495,-2.90614521320837));
#40896=CARTESIAN_POINT('Ctrl Pts',(-5.29057828960676,49.875,-2.90614521320837));
#40897=CARTESIAN_POINT('Ctrl Pts',(-5.26630084561719,57.495,-2.89688168736508));
#40898=CARTESIAN_POINT('Ctrl Pts',(-5.26630084561719,49.875,-2.89688168736508));
#40899=CARTESIAN_POINT('Ctrl Pts',(-5.24910109063628,57.495,-2.88953536864313));
#40900=CARTESIAN_POINT('Ctrl Pts',(-5.24910109063628,49.875,-2.88953536864313));
#40901=CARTESIAN_POINT('Ctrl Pts',(-5.23745215939571,57.495,-2.884065589809));
#40902=CARTESIAN_POINT('Ctrl Pts',(-5.23745215939571,49.875,-2.884065589809));
#40903=CARTESIAN_POINT('Ctrl Pts',(-5.23024117954545,57.495,-2.88043681055505));
#40904=CARTESIAN_POINT('Ctrl Pts',(-5.23024117954545,49.875,-2.88043681055505));
#40905=CARTESIAN_POINT('Ctrl Pts',(-5.22677443144495,57.495,-2.87862685522556));
#40906=CARTESIAN_POINT('Ctrl Pts',(-5.22677443144495,49.875,-2.87862685522556));
#40907=CARTESIAN_POINT('Ctrl Pts',(-6.50167680247051,51.145,-2.96056324982543));
#40908=CARTESIAN_POINT('Ctrl Pts',(-6.49043534784131,51.145,-2.96229154623625));
#40909=CARTESIAN_POINT('Ctrl Pts',(-6.46801681444607,51.145,-2.96566304810549));
#40910=CARTESIAN_POINT('Ctrl Pts',(-6.43458214159149,51.145,-2.97046502832945));
#40911=CARTESIAN_POINT('Ctrl Pts',(-6.39038953466561,51.145,-2.97635619664337));
#40912=CARTESIAN_POINT('Ctrl Pts',(-6.33579850967689,51.145,-2.98286238364857));
#40913=CARTESIAN_POINT('Ctrl Pts',(-6.28186459845047,51.145,-2.98850417352769));
#40914=CARTESIAN_POINT('Ctrl Pts',(-6.22859706400147,51.145,-2.99327554868811));
#40915=CARTESIAN_POINT('Ctrl Pts',(-6.17600655789209,51.145,-2.99717295692919));
#40916=CARTESIAN_POINT('Ctrl Pts',(-6.12410381716742,51.145,-3.00019778316108));
#40917=CARTESIAN_POINT('Ctrl Pts',(-6.07290162599622,51.145,-3.00235671375967));
#40918=CARTESIAN_POINT('Ctrl Pts',(-6.02241806591666,51.145,-3.00366113621883));
#40919=CARTESIAN_POINT('Ctrl Pts',(-5.97267956506952,51.145,-3.00412716938109));
#40920=CARTESIAN_POINT('Ctrl Pts',(-5.9237232280624,51.145,-3.00377540211877));
#40921=CARTESIAN_POINT('Ctrl Pts',(-5.87560110342631,51.145,-3.00263159433912));
#40922=CARTESIAN_POINT('Ctrl Pts',(-5.82837721216385,51.145,-3.00072490941932));
#40923=CARTESIAN_POINT('Ctrl Pts',(-5.78211642456387,51.145,-2.99808342690946));
#40924=CARTESIAN_POINT('Ctrl Pts',(-5.73687442119613,51.145,-2.9947301570106));
#40925=CARTESIAN_POINT('Ctrl Pts',(-5.69268882427748,51.145,-2.9906797244254));
#40926=CARTESIAN_POINT('Ctrl Pts',(-5.64956501668959,51.145,-2.98593308820271));
#40927=CARTESIAN_POINT('Ctrl Pts',(-5.6074788286105,51.145,-2.98047914221));
#40928=CARTESIAN_POINT('Ctrl Pts',(-5.56641026634749,51.145,-2.97430877025609));
#40929=CARTESIAN_POINT('Ctrl Pts',(-5.52637191504895,51.145,-2.96742703426683));
#40930=CARTESIAN_POINT('Ctrl Pts',(-5.48743586913296,51.145,-2.9598647928985));
#40931=CARTESIAN_POINT('Ctrl Pts',(-5.44977003302482,51.145,-2.95169462080131));
#40932=CARTESIAN_POINT('Ctrl Pts',(-5.41364129622045,51.145,-2.94303247002258));
#40933=CARTESIAN_POINT('Ctrl Pts',(-5.37936310952307,51.145,-2.93401523982671));
#40934=CARTESIAN_POINT('Ctrl Pts',(-5.34725389048201,51.145,-2.92478335875774));
#40935=CARTESIAN_POINT('Ctrl Pts',(-5.31759510370885,51.145,-2.91546314862891));
#40936=CARTESIAN_POINT('Ctrl Pts',(-5.29057828960676,51.145,-2.90614521320837));
#40937=CARTESIAN_POINT('Ctrl Pts',(-5.26630084561719,51.145,-2.89688168736508));
#40938=CARTESIAN_POINT('Ctrl Pts',(-5.24910109063628,51.145,-2.88953536864313));
#40939=CARTESIAN_POINT('Ctrl Pts',(-5.23745215939571,51.145,-2.884065589809));
#40940=CARTESIAN_POINT('Ctrl Pts',(-5.23024117954545,51.145,-2.88043681055505));
#40941=CARTESIAN_POINT('Ctrl Pts',(-5.22677443144495,51.145,-2.87862685522556));
#40942=CARTESIAN_POINT('Origin',(0.,54.32,0.));
#40943=CARTESIAN_POINT('',(-5.32519370006274,51.145,-0.592010183030743));
#40944=CARTESIAN_POINT('Origin',(0.,51.145,0.));
#40945=CARTESIAN_POINT('',(-5.32519370006274,54.32,-0.592010183030743));
#40946=CARTESIAN_POINT('Origin',(-5.93051272372135,57.495,-0.659304453656786));
#40947=CARTESIAN_POINT('',(-5.93051272372135,51.145,-0.659304453656786));
#40948=CARTESIAN_POINT('',(-5.93051272372135,51.145,-0.659304453656786));
#40949=CARTESIAN_POINT('',(-5.93051272372135,57.495,-0.659304453656786));
#40950=CARTESIAN_POINT('Origin',(-1.6286971771251E-12,57.495,4.16333634234533E-16));
#40951=CARTESIAN_POINT('',(-7.13972463098307,51.145,-0.247119796320916));
#40952=CARTESIAN_POINT('',(-7.13972463098307,57.495,-0.247119796320916));
#40953=CARTESIAN_POINT('',(-7.13972463098307,51.145,0.24711979632092));
#40954=CARTESIAN_POINT('Origin',(-1.6286971771251E-12,51.145,4.16333634234533E-16));
#40955=CARTESIAN_POINT('',(-7.13972463098307,57.495,0.24711979632092));
#40956=CARTESIAN_POINT('Ctrl Pts',(-5.93051272372135,57.495,0.659304453656788));
#40957=CARTESIAN_POINT('Ctrl Pts',(-5.93051272372135,49.875,0.659304453656788));
#40958=CARTESIAN_POINT('Ctrl Pts',(-5.9344082212537,57.495,0.659649967278237));
#40959=CARTESIAN_POINT('Ctrl Pts',(-5.9344082212537,49.875,0.659649967278237));
#40960=CARTESIAN_POINT('Ctrl Pts',(-5.94245897164691,57.495,0.660242999639201));
#40961=CARTESIAN_POINT('Ctrl Pts',(-5.94245897164691,49.875,0.660242999639201));
#40962=CARTESIAN_POINT('Ctrl Pts',(-5.95531437453424,57.495,0.660838563360922));
#40963=CARTESIAN_POINT('Ctrl Pts',(-5.95531437453424,49.875,0.660838563360922));
#40964=CARTESIAN_POINT('Ctrl Pts',(-5.97401619058907,57.495,0.661043615595512));
#40965=CARTESIAN_POINT('Ctrl Pts',(-5.97401619058907,49.875,0.661043615595512));
#40966=CARTESIAN_POINT('Ctrl Pts',(-5.99999062205823,57.495,0.660311421925997));
#40967=CARTESIAN_POINT('Ctrl Pts',(-5.99999062205823,49.875,0.660311421925997));
#40968=CARTESIAN_POINT('Ctrl Pts',(-6.0285167231501,57.495,0.658581184594089));
#40969=CARTESIAN_POINT('Ctrl Pts',(-6.0285167231501,49.875,0.658581184594089));
#40970=CARTESIAN_POINT('Ctrl Pts',(-6.05948455921138,57.495,0.655842009648634));
#40971=CARTESIAN_POINT('Ctrl Pts',(-6.05948455921138,49.875,0.655842009648634));
#40972=CARTESIAN_POINT('Ctrl Pts',(-6.09268249742298,57.495,0.65208348946162));
#40973=CARTESIAN_POINT('Ctrl Pts',(-6.09268249742298,49.875,0.65208348946162));
#40974=CARTESIAN_POINT('Ctrl Pts',(-6.12780215712604,57.495,0.64729662973892));
#40975=CARTESIAN_POINT('Ctrl Pts',(-6.12780215712604,49.875,0.64729662973892));
#40976=CARTESIAN_POINT('Ctrl Pts',(-6.16449561918676,57.495,0.641473544543615));
#40977=CARTESIAN_POINT('Ctrl Pts',(-6.16449561918676,49.875,0.641473544543615));
#40978=CARTESIAN_POINT('Ctrl Pts',(-6.20242090374318,57.495,0.634607707876565));
#40979=CARTESIAN_POINT('Ctrl Pts',(-6.20242090374318,49.875,0.634607707876565));
#40980=CARTESIAN_POINT('Ctrl Pts',(-6.24128706412515,57.495,0.626694128202842));
#40981=CARTESIAN_POINT('Ctrl Pts',(-6.24128706412515,49.875,0.626694128202842));
#40982=CARTESIAN_POINT('Ctrl Pts',(-6.2809112037544,57.495,0.617730009530307));
#40983=CARTESIAN_POINT('Ctrl Pts',(-6.2809112037544,49.875,0.617730009530307));
#40984=CARTESIAN_POINT('Ctrl Pts',(-6.32121490697716,57.495,0.607714431517402));
#40985=CARTESIAN_POINT('Ctrl Pts',(-6.32121490697716,49.875,0.607714431517402));
#40986=CARTESIAN_POINT('Ctrl Pts',(-6.36218460951727,57.495,0.596647533682211));
#40987=CARTESIAN_POINT('Ctrl Pts',(-6.36218460951727,49.875,0.596647533682211));
#40988=CARTESIAN_POINT('Ctrl Pts',(-6.40384227175352,57.495,0.584530087032238));
#40989=CARTESIAN_POINT('Ctrl Pts',(-6.40384227175352,49.875,0.584530087032238));
#40990=CARTESIAN_POINT('Ctrl Pts',(-6.44621447382266,57.495,0.57136310290558));
#40991=CARTESIAN_POINT('Ctrl Pts',(-6.44621447382266,49.875,0.57136310290558));
#40992=CARTESIAN_POINT('Ctrl Pts',(-6.4892958755784,57.495,0.557147755196277));
#40993=CARTESIAN_POINT('Ctrl Pts',(-6.4892958755784,49.875,0.557147755196277));
#40994=CARTESIAN_POINT('Ctrl Pts',(-6.53304612199323,57.495,0.54188492983995));
#40995=CARTESIAN_POINT('Ctrl Pts',(-6.53304612199323,49.875,0.54188492983995));
#40996=CARTESIAN_POINT('Ctrl Pts',(-6.57740496530571,57.495,0.525574676214356));
#40997=CARTESIAN_POINT('Ctrl Pts',(-6.57740496530571,49.875,0.525574676214356));
#40998=CARTESIAN_POINT('Ctrl Pts',(-6.62230172760513,57.495,0.508215876982669));
#40999=CARTESIAN_POINT('Ctrl Pts',(-6.62230172760513,49.875,0.508215876982669));
#41000=CARTESIAN_POINT('Ctrl Pts',(-6.66766610085618,57.495,0.489806088474623));
#41001=CARTESIAN_POINT('Ctrl Pts',(-6.66766610085618,49.875,0.489806088474623));
#41002=CARTESIAN_POINT('Ctrl Pts',(-6.71344014059664,57.495,0.470341429749656));
#41003=CARTESIAN_POINT('Ctrl Pts',(-6.71344014059664,49.875,0.470341429749656));
#41004=CARTESIAN_POINT('Ctrl Pts',(-6.75958168761858,57.495,0.449817078488629));
#41005=CARTESIAN_POINT('Ctrl Pts',(-6.75958168761858,49.875,0.449817078488629));
#41006=CARTESIAN_POINT('Ctrl Pts',(-6.80606015708966,57.495,0.428228256434473));
#41007=CARTESIAN_POINT('Ctrl Pts',(-6.80606015708966,49.875,0.428228256434473));
#41008=CARTESIAN_POINT('Ctrl Pts',(-6.85285448604159,57.495,0.405571362419756));
#41009=CARTESIAN_POINT('Ctrl Pts',(-6.85285448604159,49.875,0.405571362419756));
#41010=CARTESIAN_POINT('Ctrl Pts',(-6.89995030467727,57.495,0.381845111328235));
#41011=CARTESIAN_POINT('Ctrl Pts',(-6.89995030467727,49.875,0.381845111328235));
#41012=CARTESIAN_POINT('Ctrl Pts',(-6.94733716327837,57.495,0.357052332559036));
#41013=CARTESIAN_POINT('Ctrl Pts',(-6.94733716327837,49.875,0.357052332559036));
#41014=CARTESIAN_POINT('Ctrl Pts',(-6.99500658045299,57.495,0.331200384094009));
#41015=CARTESIAN_POINT('Ctrl Pts',(-6.99500658045299,49.875,0.331200384094009));
#41016=CARTESIAN_POINT('Ctrl Pts',(-7.0429523011241,57.495,0.304298370266205));
#41017=CARTESIAN_POINT('Ctrl Pts',(-7.0429523011241,49.875,0.304298370266205));
#41018=CARTESIAN_POINT('Ctrl Pts',(-7.0815264936403,57.495,0.28194386193484));
#41019=CARTESIAN_POINT('Ctrl Pts',(-7.0815264936403,49.875,0.28194386193484));
#41020=CARTESIAN_POINT('Ctrl Pts',(-7.11057846529273,57.495,0.264712515322387));
#41021=CARTESIAN_POINT('Ctrl Pts',(-7.11057846529273,49.875,0.264712515322387));
#41022=CARTESIAN_POINT('Ctrl Pts',(-7.13000027153808,57.495,0.253018452443276));
#41023=CARTESIAN_POINT('Ctrl Pts',(-7.13000027153808,49.875,0.253018452443276));
#41024=CARTESIAN_POINT('Ctrl Pts',(-7.13972463098307,57.495,0.247119796320917));
#41025=CARTESIAN_POINT('Ctrl Pts',(-7.13972463098307,49.875,0.247119796320917));
#41026=CARTESIAN_POINT('',(-5.93051272372135,51.145,0.659304453656788));
#41027=CARTESIAN_POINT('Ctrl Pts',(-5.93051272372135,51.145,0.659304453656788));
#41028=CARTESIAN_POINT('Ctrl Pts',(-5.9344082212537,51.145,0.659649967278237));
#41029=CARTESIAN_POINT('Ctrl Pts',(-5.94245897164691,51.145,0.660242999639201));
#41030=CARTESIAN_POINT('Ctrl Pts',(-5.95531437453424,51.145,0.660838563360922));
#41031=CARTESIAN_POINT('Ctrl Pts',(-5.97401619058907,51.145,0.661043615595512));
#41032=CARTESIAN_POINT('Ctrl Pts',(-5.99999062205823,51.145,0.660311421925997));
#41033=CARTESIAN_POINT('Ctrl Pts',(-6.0285167231501,51.145,0.658581184594089));
#41034=CARTESIAN_POINT('Ctrl Pts',(-6.05948455921138,51.145,0.655842009648634));
#41035=CARTESIAN_POINT('Ctrl Pts',(-6.09268249742298,51.145,0.65208348946162));
#41036=CARTESIAN_POINT('Ctrl Pts',(-6.12780215712604,51.145,0.64729662973892));
#41037=CARTESIAN_POINT('Ctrl Pts',(-6.16449561918676,51.145,0.641473544543615));
#41038=CARTESIAN_POINT('Ctrl Pts',(-6.20242090374318,51.145,0.634607707876565));
#41039=CARTESIAN_POINT('Ctrl Pts',(-6.24128706412515,51.145,0.626694128202842));
#41040=CARTESIAN_POINT('Ctrl Pts',(-6.2809112037544,51.145,0.617730009530307));
#41041=CARTESIAN_POINT('Ctrl Pts',(-6.32121490697716,51.145,0.607714431517402));
#41042=CARTESIAN_POINT('Ctrl Pts',(-6.36218460951727,51.145,0.596647533682211));
#41043=CARTESIAN_POINT('Ctrl Pts',(-6.40384227175352,51.145,0.584530087032238));
#41044=CARTESIAN_POINT('Ctrl Pts',(-6.44621447382266,51.145,0.57136310290558));
#41045=CARTESIAN_POINT('Ctrl Pts',(-6.4892958755784,51.145,0.557147755196277));
#41046=CARTESIAN_POINT('Ctrl Pts',(-6.53304612199323,51.145,0.54188492983995));
#41047=CARTESIAN_POINT('Ctrl Pts',(-6.57740496530571,51.145,0.525574676214356));
#41048=CARTESIAN_POINT('Ctrl Pts',(-6.62230172760513,51.145,0.508215876982669));
#41049=CARTESIAN_POINT('Ctrl Pts',(-6.66766610085618,51.145,0.489806088474623));
#41050=CARTESIAN_POINT('Ctrl Pts',(-6.71344014059664,51.145,0.470341429749656));
#41051=CARTESIAN_POINT('Ctrl Pts',(-6.75958168761858,51.145,0.449817078488629));
#41052=CARTESIAN_POINT('Ctrl Pts',(-6.80606015708966,51.145,0.428228256434473));
#41053=CARTESIAN_POINT('Ctrl Pts',(-6.85285448604159,51.145,0.405571362419756));
#41054=CARTESIAN_POINT('Ctrl Pts',(-6.89995030467727,51.145,0.381845111328235));
#41055=CARTESIAN_POINT('Ctrl Pts',(-6.94733716327837,51.145,0.357052332559036));
#41056=CARTESIAN_POINT('Ctrl Pts',(-6.99500658045299,51.145,0.331200384094009));
#41057=CARTESIAN_POINT('Ctrl Pts',(-7.0429523011241,51.145,0.304298370266205));
#41058=CARTESIAN_POINT('Ctrl Pts',(-7.0815264936403,51.145,0.28194386193484));
#41059=CARTESIAN_POINT('Ctrl Pts',(-7.11057846529273,51.145,0.264712515322387));
#41060=CARTESIAN_POINT('Ctrl Pts',(-7.13000027153808,51.145,0.253018452443276));
#41061=CARTESIAN_POINT('Ctrl Pts',(-7.13972463098307,51.145,0.247119796320917));
#41062=CARTESIAN_POINT('',(-5.93051272372135,57.495,0.659304453656788));
#41063=CARTESIAN_POINT('Origin',(-5.17611212951227,57.495,0.575436549687218));
#41064=CARTESIAN_POINT('',(-5.32519370006274,51.145,0.592010183030744));
#41065=CARTESIAN_POINT('',(-5.32519370006274,54.32,0.592010183030744));
#41066=CARTESIAN_POINT('',(-5.17611212951227,51.145,0.575436549687218));
#41067=CARTESIAN_POINT('Ctrl Pts',(-7.13972463098307,57.495,-0.247119796320916));
#41068=CARTESIAN_POINT('Ctrl Pts',(-7.13972463098307,49.875,-0.247119796320916));
#41069=CARTESIAN_POINT('Ctrl Pts',(-7.13000027153814,57.495,-0.253018452443266));
#41070=CARTESIAN_POINT('Ctrl Pts',(-7.13000027153814,49.875,-0.253018452443266));
#41071=CARTESIAN_POINT('Ctrl Pts',(-7.1105784652929,57.495,-0.264712515322364));
#41072=CARTESIAN_POINT('Ctrl Pts',(-7.1105784652929,49.875,-0.264712515322364));
#41073=CARTESIAN_POINT('Ctrl Pts',(-7.0815264936406,57.495,-0.281943861934803));
#41074=CARTESIAN_POINT('Ctrl Pts',(-7.0815264936406,49.875,-0.281943861934803));
#41075=CARTESIAN_POINT('Ctrl Pts',(-7.04295230112448,57.495,-0.304298370266162));
#41076=CARTESIAN_POINT('Ctrl Pts',(-7.04295230112448,49.875,-0.304298370266162));
#41077=CARTESIAN_POINT('Ctrl Pts',(-6.99500658045334,57.495,-0.331200384093975));
#41078=CARTESIAN_POINT('Ctrl Pts',(-6.99500658045334,49.875,-0.331200384093975));
#41079=CARTESIAN_POINT('Ctrl Pts',(-6.94733716327859,57.495,-0.357052332559016));
#41080=CARTESIAN_POINT('Ctrl Pts',(-6.94733716327859,49.875,-0.357052332559016));
#41081=CARTESIAN_POINT('Ctrl Pts',(-6.89995030467732,57.495,-0.381845111328231));
#41082=CARTESIAN_POINT('Ctrl Pts',(-6.89995030467732,49.875,-0.381845111328231));
#41083=CARTESIAN_POINT('Ctrl Pts',(-6.85285448604147,57.495,-0.405571362419762));
#41084=CARTESIAN_POINT('Ctrl Pts',(-6.85285448604147,49.875,-0.405571362419762));
#41085=CARTESIAN_POINT('Ctrl Pts',(-6.80606015708944,57.495,-0.428228256434481));
#41086=CARTESIAN_POINT('Ctrl Pts',(-6.80606015708944,49.875,-0.428228256434481));
#41087=CARTESIAN_POINT('Ctrl Pts',(-6.75958168761835,57.495,-0.449817078488634));
#41088=CARTESIAN_POINT('Ctrl Pts',(-6.75958168761835,49.875,-0.449817078488634));
#41089=CARTESIAN_POINT('Ctrl Pts',(-6.71344014059646,57.495,-0.470341429749656));
#41090=CARTESIAN_POINT('Ctrl Pts',(-6.71344014059646,49.875,-0.470341429749656));
#41091=CARTESIAN_POINT('Ctrl Pts',(-6.66766610085612,57.495,-0.48980608847462));
#41092=CARTESIAN_POINT('Ctrl Pts',(-6.66766610085612,49.875,-0.48980608847462));
#41093=CARTESIAN_POINT('Ctrl Pts',(-6.62230172760518,57.495,-0.508215876982667));
#41094=CARTESIAN_POINT('Ctrl Pts',(-6.62230172760518,49.875,-0.508215876982667));
#41095=CARTESIAN_POINT('Ctrl Pts',(-6.57740496530586,57.495,-0.52557467621436));
#41096=CARTESIAN_POINT('Ctrl Pts',(-6.57740496530586,49.875,-0.52557467621436));
#41097=CARTESIAN_POINT('Ctrl Pts',(-6.53304612199338,57.495,-0.541884929839958));
#41098=CARTESIAN_POINT('Ctrl Pts',(-6.53304612199338,49.875,-0.541884929839958));
#41099=CARTESIAN_POINT('Ctrl Pts',(-6.48929587557851,57.495,-0.557147755196287));
#41100=CARTESIAN_POINT('Ctrl Pts',(-6.48929587557851,49.875,-0.557147755196287));
#41101=CARTESIAN_POINT('Ctrl Pts',(-6.4462144738227,57.495,-0.571363102905585));
#41102=CARTESIAN_POINT('Ctrl Pts',(-6.4462144738227,49.875,-0.571363102905585));
#41103=CARTESIAN_POINT('Ctrl Pts',(-6.40384227175349,57.495,-0.584530087032233));
#41104=CARTESIAN_POINT('Ctrl Pts',(-6.40384227175349,49.875,-0.584530087032233));
#41105=CARTESIAN_POINT('Ctrl Pts',(-6.36218460951721,57.495,-0.596647533682195));
#41106=CARTESIAN_POINT('Ctrl Pts',(-6.36218460951721,49.875,-0.596647533682195));
#41107=CARTESIAN_POINT('Ctrl Pts',(-6.32121490697708,57.495,-0.607714431517378));
#41108=CARTESIAN_POINT('Ctrl Pts',(-6.32121490697708,49.875,-0.607714431517378));
#41109=CARTESIAN_POINT('Ctrl Pts',(-6.28091120375433,57.495,-0.617730009530283));
#41110=CARTESIAN_POINT('Ctrl Pts',(-6.28091120375433,49.875,-0.617730009530283));
#41111=CARTESIAN_POINT('Ctrl Pts',(-6.24128706412512,57.495,-0.626694128202827));
#41112=CARTESIAN_POINT('Ctrl Pts',(-6.24128706412512,49.875,-0.626694128202827));
#41113=CARTESIAN_POINT('Ctrl Pts',(-6.2024209037432,57.495,-0.63460770787657));
#41114=CARTESIAN_POINT('Ctrl Pts',(-6.2024209037432,49.875,-0.63460770787657));
#41115=CARTESIAN_POINT('Ctrl Pts',(-6.16449561918681,57.495,-0.641473544543642));
#41116=CARTESIAN_POINT('Ctrl Pts',(-6.16449561918681,49.875,-0.641473544543642));
#41117=CARTESIAN_POINT('Ctrl Pts',(-6.12780215712609,57.495,-0.647296629738964));
#41118=CARTESIAN_POINT('Ctrl Pts',(-6.12780215712609,49.875,-0.647296629738964));
#41119=CARTESIAN_POINT('Ctrl Pts',(-6.092682497423,57.495,-0.652083489461663));
#41120=CARTESIAN_POINT('Ctrl Pts',(-6.092682497423,49.875,-0.652083489461663));
#41121=CARTESIAN_POINT('Ctrl Pts',(-6.05948455921138,57.495,-0.655842009648654));
#41122=CARTESIAN_POINT('Ctrl Pts',(-6.05948455921138,49.875,-0.655842009648654));
#41123=CARTESIAN_POINT('Ctrl Pts',(-6.02851672315009,57.495,-0.658581184594065));
#41124=CARTESIAN_POINT('Ctrl Pts',(-6.02851672315009,49.875,-0.658581184594065));
#41125=CARTESIAN_POINT('Ctrl Pts',(-5.99999062205821,57.495,-0.660311421925919));
#41126=CARTESIAN_POINT('Ctrl Pts',(-5.99999062205821,49.875,-0.660311421925919));
#41127=CARTESIAN_POINT('Ctrl Pts',(-5.97401619058905,57.495,-0.661043615595395));
#41128=CARTESIAN_POINT('Ctrl Pts',(-5.97401619058905,49.875,-0.661043615595395));
#41129=CARTESIAN_POINT('Ctrl Pts',(-5.95531437453421,57.495,-0.660838563360812));
#41130=CARTESIAN_POINT('Ctrl Pts',(-5.95531437453421,49.875,-0.660838563360812));
#41131=CARTESIAN_POINT('Ctrl Pts',(-5.94245897164689,57.495,-0.660242999639131));
#41132=CARTESIAN_POINT('Ctrl Pts',(-5.94245897164689,49.875,-0.660242999639131));
#41133=CARTESIAN_POINT('Ctrl Pts',(-5.93440822125369,57.495,-0.659649967278209));
#41134=CARTESIAN_POINT('Ctrl Pts',(-5.93440822125369,49.875,-0.659649967278209));
#41135=CARTESIAN_POINT('Ctrl Pts',(-5.93051272372135,57.495,-0.659304453656786));
#41136=CARTESIAN_POINT('Ctrl Pts',(-5.93051272372135,49.875,-0.659304453656786));
#41137=CARTESIAN_POINT('Ctrl Pts',(-7.13972463098307,51.145,-0.247119796320916));
#41138=CARTESIAN_POINT('Ctrl Pts',(-7.13000027153814,51.145,-0.253018452443266));
#41139=CARTESIAN_POINT('Ctrl Pts',(-7.1105784652929,51.145,-0.264712515322364));
#41140=CARTESIAN_POINT('Ctrl Pts',(-7.0815264936406,51.145,-0.281943861934803));
#41141=CARTESIAN_POINT('Ctrl Pts',(-7.04295230112448,51.145,-0.304298370266162));
#41142=CARTESIAN_POINT('Ctrl Pts',(-6.99500658045334,51.145,-0.331200384093975));
#41143=CARTESIAN_POINT('Ctrl Pts',(-6.94733716327859,51.145,-0.357052332559016));
#41144=CARTESIAN_POINT('Ctrl Pts',(-6.89995030467732,51.145,-0.381845111328231));
#41145=CARTESIAN_POINT('Ctrl Pts',(-6.85285448604147,51.145,-0.405571362419762));
#41146=CARTESIAN_POINT('Ctrl Pts',(-6.80606015708944,51.145,-0.428228256434481));
#41147=CARTESIAN_POINT('Ctrl Pts',(-6.75958168761835,51.145,-0.449817078488634));
#41148=CARTESIAN_POINT('Ctrl Pts',(-6.71344014059646,51.145,-0.470341429749656));
#41149=CARTESIAN_POINT('Ctrl Pts',(-6.66766610085612,51.145,-0.48980608847462));
#41150=CARTESIAN_POINT('Ctrl Pts',(-6.62230172760518,51.145,-0.508215876982667));
#41151=CARTESIAN_POINT('Ctrl Pts',(-6.57740496530586,51.145,-0.52557467621436));
#41152=CARTESIAN_POINT('Ctrl Pts',(-6.53304612199338,51.145,-0.541884929839958));
#41153=CARTESIAN_POINT('Ctrl Pts',(-6.48929587557851,51.145,-0.557147755196287));
#41154=CARTESIAN_POINT('Ctrl Pts',(-6.4462144738227,51.145,-0.571363102905585));
#41155=CARTESIAN_POINT('Ctrl Pts',(-6.40384227175349,51.145,-0.584530087032233));
#41156=CARTESIAN_POINT('Ctrl Pts',(-6.36218460951721,51.145,-0.596647533682195));
#41157=CARTESIAN_POINT('Ctrl Pts',(-6.32121490697708,51.145,-0.607714431517378));
#41158=CARTESIAN_POINT('Ctrl Pts',(-6.28091120375433,51.145,-0.617730009530283));
#41159=CARTESIAN_POINT('Ctrl Pts',(-6.24128706412512,51.145,-0.626694128202827));
#41160=CARTESIAN_POINT('Ctrl Pts',(-6.2024209037432,51.145,-0.63460770787657));
#41161=CARTESIAN_POINT('Ctrl Pts',(-6.16449561918681,51.145,-0.641473544543642));
#41162=CARTESIAN_POINT('Ctrl Pts',(-6.12780215712609,51.145,-0.647296629738964));
#41163=CARTESIAN_POINT('Ctrl Pts',(-6.092682497423,51.145,-0.652083489461663));
#41164=CARTESIAN_POINT('Ctrl Pts',(-6.05948455921138,51.145,-0.655842009648654));
#41165=CARTESIAN_POINT('Ctrl Pts',(-6.02851672315009,51.145,-0.658581184594065));
#41166=CARTESIAN_POINT('Ctrl Pts',(-5.99999062205821,51.145,-0.660311421925919));
#41167=CARTESIAN_POINT('Ctrl Pts',(-5.97401619058905,51.145,-0.661043615595395));
#41168=CARTESIAN_POINT('Ctrl Pts',(-5.95531437453421,51.145,-0.660838563360812));
#41169=CARTESIAN_POINT('Ctrl Pts',(-5.94245897164689,51.145,-0.660242999639131));
#41170=CARTESIAN_POINT('Ctrl Pts',(-5.93440822125369,51.145,-0.659649967278209));
#41171=CARTESIAN_POINT('Ctrl Pts',(-5.93051272372135,51.145,-0.659304453656786));
#41172=CARTESIAN_POINT('Origin',(0.,54.32,0.));
#41173=CARTESIAN_POINT('',(-5.1463899549833,51.145,1.4909173120086));
#41174=CARTESIAN_POINT('Origin',(0.,51.145,0.));
#41175=CARTESIAN_POINT('',(-5.1463899549833,54.32,1.4909173120086));
#41176=CARTESIAN_POINT('Origin',(-5.73138421404289,57.495,1.66039107437148));
#41177=CARTESIAN_POINT('',(-5.73138421404289,51.145,1.66039107437148));
#41178=CARTESIAN_POINT('',(-5.73138421404289,51.145,1.66039107437148));
#41179=CARTESIAN_POINT('',(-5.73138421404289,57.495,1.66039107437148));
#41180=CARTESIAN_POINT('Origin',(-1.50456066262064E-12,57.495,6.23660068148933E-13));
#41181=CARTESIAN_POINT('',(-6.69081410619341,51.145,2.50394540602692));
#41182=CARTESIAN_POINT('',(-6.69081410619341,57.495,2.50394540602692));
#41183=CARTESIAN_POINT('',(-6.5016768024705,51.145,2.96056324982543));
#41184=CARTESIAN_POINT('Origin',(-1.50456066262064E-12,51.145,6.23660068148933E-13));
#41185=CARTESIAN_POINT('',(-6.5016768024705,57.495,2.96056324982543));
#41186=CARTESIAN_POINT('Ctrl Pts',(-5.22677443144495,57.495,2.87862685522557));
#41187=CARTESIAN_POINT('Ctrl Pts',(-5.22677443144495,49.875,2.87862685522557));
#41188=CARTESIAN_POINT('Ctrl Pts',(-5.23024117954545,57.495,2.88043681055507));
#41189=CARTESIAN_POINT('Ctrl Pts',(-5.23024117954545,49.875,2.88043681055507));
#41190=CARTESIAN_POINT('Ctrl Pts',(-5.2374521593957,57.495,2.88406558980908));
#41191=CARTESIAN_POINT('Ctrl Pts',(-5.2374521593957,49.875,2.88406558980908));
#41192=CARTESIAN_POINT('Ctrl Pts',(-5.24910109063627,57.495,2.88953536864324));
#41193=CARTESIAN_POINT('Ctrl Pts',(-5.24910109063627,49.875,2.88953536864324));
#41194=CARTESIAN_POINT('Ctrl Pts',(-5.26630084561717,57.495,2.8968816873652));
#41195=CARTESIAN_POINT('Ctrl Pts',(-5.26630084561717,49.875,2.8968816873652));
#41196=CARTESIAN_POINT('Ctrl Pts',(-5.29057828960674,57.495,2.90614521320845));
#41197=CARTESIAN_POINT('Ctrl Pts',(-5.29057828960674,49.875,2.90614521320845));
#41198=CARTESIAN_POINT('Ctrl Pts',(-5.31759510370885,57.495,2.91546314862894));
#41199=CARTESIAN_POINT('Ctrl Pts',(-5.31759510370885,49.875,2.91546314862894));
#41200=CARTESIAN_POINT('Ctrl Pts',(-5.34725389048201,57.495,2.92478335875772));
#41201=CARTESIAN_POINT('Ctrl Pts',(-5.34725389048201,49.875,2.92478335875772));
#41202=CARTESIAN_POINT('Ctrl Pts',(-5.37936310952307,57.495,2.93401523982666));
#41203=CARTESIAN_POINT('Ctrl Pts',(-5.37936310952307,49.875,2.93401523982666));
#41204=CARTESIAN_POINT('Ctrl Pts',(-5.41364129622042,57.495,2.94303247002252));
#41205=CARTESIAN_POINT('Ctrl Pts',(-5.41364129622042,49.875,2.94303247002252));
#41206=CARTESIAN_POINT('Ctrl Pts',(-5.44977003302479,57.495,2.95169462080126));
#41207=CARTESIAN_POINT('Ctrl Pts',(-5.44977003302479,49.875,2.95169462080126));
#41208=CARTESIAN_POINT('Ctrl Pts',(-5.48743586913294,57.495,2.95986479289848));
#41209=CARTESIAN_POINT('Ctrl Pts',(-5.48743586913294,49.875,2.95986479289848));
#41210=CARTESIAN_POINT('Ctrl Pts',(-5.52637191504897,57.495,2.96742703426686));
#41211=CARTESIAN_POINT('Ctrl Pts',(-5.52637191504897,49.875,2.96742703426686));
#41212=CARTESIAN_POINT('Ctrl Pts',(-5.56641026634754,57.495,2.97430877025613));
#41213=CARTESIAN_POINT('Ctrl Pts',(-5.56641026634754,49.875,2.97430877025613));
#41214=CARTESIAN_POINT('Ctrl Pts',(-5.60747882861056,57.495,2.98047914221005));
#41215=CARTESIAN_POINT('Ctrl Pts',(-5.60747882861056,49.875,2.98047914221005));
#41216=CARTESIAN_POINT('Ctrl Pts',(-5.64956501668965,57.495,2.98593308820275));
#41217=CARTESIAN_POINT('Ctrl Pts',(-5.64956501668965,49.875,2.98593308820275));
#41218=CARTESIAN_POINT('Ctrl Pts',(-5.6926888242775,57.495,2.99067972442542));
#41219=CARTESIAN_POINT('Ctrl Pts',(-5.6926888242775,49.875,2.99067972442542));
#41220=CARTESIAN_POINT('Ctrl Pts',(-5.7368744211961,57.495,2.99473015701058));
#41221=CARTESIAN_POINT('Ctrl Pts',(-5.7368744211961,49.875,2.99473015701058));
#41222=CARTESIAN_POINT('Ctrl Pts',(-5.78211642456377,57.495,2.99808342690941));
#41223=CARTESIAN_POINT('Ctrl Pts',(-5.78211642456377,49.875,2.99808342690941));
#41224=CARTESIAN_POINT('Ctrl Pts',(-5.82837721216372,57.495,3.00072490941925));
#41225=CARTESIAN_POINT('Ctrl Pts',(-5.82837721216372,49.875,3.00072490941925));
#41226=CARTESIAN_POINT('Ctrl Pts',(-5.87560110342618,57.495,3.00263159433907));
#41227=CARTESIAN_POINT('Ctrl Pts',(-5.87560110342618,49.875,3.00263159433907));
#41228=CARTESIAN_POINT('Ctrl Pts',(-5.92372322806235,57.495,3.00377540211876));
#41229=CARTESIAN_POINT('Ctrl Pts',(-5.92372322806235,49.875,3.00377540211876));
#41230=CARTESIAN_POINT('Ctrl Pts',(-5.97267956506957,57.495,3.00412716938111));
#41231=CARTESIAN_POINT('Ctrl Pts',(-5.97267956506957,49.875,3.00412716938111));
#41232=CARTESIAN_POINT('Ctrl Pts',(-6.02241806591683,57.495,3.00366113621889));
#41233=CARTESIAN_POINT('Ctrl Pts',(-6.02241806591683,49.875,3.00366113621889));
#41234=CARTESIAN_POINT('Ctrl Pts',(-6.07290162599645,57.495,3.00235671375975));
#41235=CARTESIAN_POINT('Ctrl Pts',(-6.07290162599645,49.875,3.00235671375975));
#41236=CARTESIAN_POINT('Ctrl Pts',(-6.12410381716763,57.495,3.00019778316116));
#41237=CARTESIAN_POINT('Ctrl Pts',(-6.12410381716763,49.875,3.00019778316116));
#41238=CARTESIAN_POINT('Ctrl Pts',(-6.1760065578922,57.495,2.99717295692923));
#41239=CARTESIAN_POINT('Ctrl Pts',(-6.1760065578922,49.875,2.99717295692923));
#41240=CARTESIAN_POINT('Ctrl Pts',(-6.22859706400143,57.495,2.9932755486881));
#41241=CARTESIAN_POINT('Ctrl Pts',(-6.22859706400143,49.875,2.9932755486881));
#41242=CARTESIAN_POINT('Ctrl Pts',(-6.28186459845025,57.495,2.98850417352762));
#41243=CARTESIAN_POINT('Ctrl Pts',(-6.28186459845025,49.875,2.98850417352762));
#41244=CARTESIAN_POINT('Ctrl Pts',(-6.33579850967655,57.495,2.98286238364847));
#41245=CARTESIAN_POINT('Ctrl Pts',(-6.33579850967655,49.875,2.98286238364847));
#41246=CARTESIAN_POINT('Ctrl Pts',(-6.39038953466525,57.495,2.97635619664327));
#41247=CARTESIAN_POINT('Ctrl Pts',(-6.39038953466525,49.875,2.97635619664327));
#41248=CARTESIAN_POINT('Ctrl Pts',(-6.43458214159119,57.495,2.97046502832937));
#41249=CARTESIAN_POINT('Ctrl Pts',(-6.43458214159119,49.875,2.97046502832937));
#41250=CARTESIAN_POINT('Ctrl Pts',(-6.4680168144459,57.495,2.96566304810545));
#41251=CARTESIAN_POINT('Ctrl Pts',(-6.4680168144459,49.875,2.96566304810545));
#41252=CARTESIAN_POINT('Ctrl Pts',(-6.49043534784125,57.495,2.96229154623624));
#41253=CARTESIAN_POINT('Ctrl Pts',(-6.49043534784125,49.875,2.96229154623624));
#41254=CARTESIAN_POINT('Ctrl Pts',(-6.5016768024705,57.495,2.96056324982543));
#41255=CARTESIAN_POINT('Ctrl Pts',(-6.5016768024705,49.875,2.96056324982543));
#41256=CARTESIAN_POINT('',(-5.22677443144495,51.145,2.87862685522557));
#41257=CARTESIAN_POINT('Ctrl Pts',(-5.22677443144495,51.145,2.87862685522557));
#41258=CARTESIAN_POINT('Ctrl Pts',(-5.23024117954545,51.145,2.88043681055507));
#41259=CARTESIAN_POINT('Ctrl Pts',(-5.2374521593957,51.145,2.88406558980908));
#41260=CARTESIAN_POINT('Ctrl Pts',(-5.24910109063627,51.145,2.88953536864324));
#41261=CARTESIAN_POINT('Ctrl Pts',(-5.26630084561717,51.145,2.8968816873652));
#41262=CARTESIAN_POINT('Ctrl Pts',(-5.29057828960674,51.145,2.90614521320845));
#41263=CARTESIAN_POINT('Ctrl Pts',(-5.31759510370885,51.145,2.91546314862894));
#41264=CARTESIAN_POINT('Ctrl Pts',(-5.34725389048201,51.145,2.92478335875772));
#41265=CARTESIAN_POINT('Ctrl Pts',(-5.37936310952307,51.145,2.93401523982666));
#41266=CARTESIAN_POINT('Ctrl Pts',(-5.41364129622042,51.145,2.94303247002252));
#41267=CARTESIAN_POINT('Ctrl Pts',(-5.44977003302479,51.145,2.95169462080126));
#41268=CARTESIAN_POINT('Ctrl Pts',(-5.48743586913294,51.145,2.95986479289848));
#41269=CARTESIAN_POINT('Ctrl Pts',(-5.52637191504897,51.145,2.96742703426686));
#41270=CARTESIAN_POINT('Ctrl Pts',(-5.56641026634754,51.145,2.97430877025613));
#41271=CARTESIAN_POINT('Ctrl Pts',(-5.60747882861056,51.145,2.98047914221005));
#41272=CARTESIAN_POINT('Ctrl Pts',(-5.64956501668965,51.145,2.98593308820275));
#41273=CARTESIAN_POINT('Ctrl Pts',(-5.6926888242775,51.145,2.99067972442542));
#41274=CARTESIAN_POINT('Ctrl Pts',(-5.7368744211961,51.145,2.99473015701058));
#41275=CARTESIAN_POINT('Ctrl Pts',(-5.78211642456377,51.145,2.99808342690941));
#41276=CARTESIAN_POINT('Ctrl Pts',(-5.82837721216372,51.145,3.00072490941925));
#41277=CARTESIAN_POINT('Ctrl Pts',(-5.87560110342618,51.145,3.00263159433907));
#41278=CARTESIAN_POINT('Ctrl Pts',(-5.92372322806235,51.145,3.00377540211876));
#41279=CARTESIAN_POINT('Ctrl Pts',(-5.97267956506957,51.145,3.00412716938111));
#41280=CARTESIAN_POINT('Ctrl Pts',(-6.02241806591683,51.145,3.00366113621889));
#41281=CARTESIAN_POINT('Ctrl Pts',(-6.07290162599645,51.145,3.00235671375975));
#41282=CARTESIAN_POINT('Ctrl Pts',(-6.12410381716763,51.145,3.00019778316116));
#41283=CARTESIAN_POINT('Ctrl Pts',(-6.1760065578922,51.145,2.99717295692923));
#41284=CARTESIAN_POINT('Ctrl Pts',(-6.22859706400143,51.145,2.9932755486881));
#41285=CARTESIAN_POINT('Ctrl Pts',(-6.28186459845025,51.145,2.98850417352762));
#41286=CARTESIAN_POINT('Ctrl Pts',(-6.33579850967655,51.145,2.98286238364847));
#41287=CARTESIAN_POINT('Ctrl Pts',(-6.39038953466525,51.145,2.97635619664327));
#41288=CARTESIAN_POINT('Ctrl Pts',(-6.43458214159119,51.145,2.97046502832937));
#41289=CARTESIAN_POINT('Ctrl Pts',(-6.4680168144459,51.145,2.96566304810545));
#41290=CARTESIAN_POINT('Ctrl Pts',(-6.49043534784125,51.145,2.96229154623624));
#41291=CARTESIAN_POINT('Ctrl Pts',(-6.5016768024705,51.145,2.96056324982543));
#41292=CARTESIAN_POINT('',(-5.22677443144495,57.495,2.87862685522557));
#41293=CARTESIAN_POINT('Origin',(-4.56189402049717,57.495,2.51244640654327));
#41294=CARTESIAN_POINT('',(-4.69328497730872,51.145,2.58480949428933));
#41295=CARTESIAN_POINT('',(-4.69328497730872,54.32,2.58480949428933));
#41296=CARTESIAN_POINT('',(-4.56189402049717,51.145,2.51244640654327));
#41297=CARTESIAN_POINT('Ctrl Pts',(-6.69081410619341,57.495,2.50394540602692));
#41298=CARTESIAN_POINT('Ctrl Pts',(-6.69081410619341,49.875,2.50394540602692));
#41299=CARTESIAN_POINT('Ctrl Pts',(-6.6840872875067,57.495,2.49477440711622));
#41300=CARTESIAN_POINT('Ctrl Pts',(-6.6840872875067,49.875,2.49477440711622));
#41301=CARTESIAN_POINT('Ctrl Pts',(-6.67061900235319,57.495,2.47653809829367));
#41302=CARTESIAN_POINT('Ctrl Pts',(-6.67061900235319,49.875,2.47653809829367));
#41303=CARTESIAN_POINT('Ctrl Pts',(-6.65037263123044,57.495,2.44950070161195));
#41304=CARTESIAN_POINT('Ctrl Pts',(-6.65037263123044,49.875,2.44950070161195));
#41305=CARTESIAN_POINT('Ctrl Pts',(-6.62328942425873,57.495,2.41408612451247));
#41306=CARTESIAN_POINT('Ctrl Pts',(-6.62328942425873,49.875,2.41408612451247));
#41307=CARTESIAN_POINT('Ctrl Pts',(-6.58928830924833,57.495,2.37088387159997));
#41308=CARTESIAN_POINT('Ctrl Pts',(-6.58928830924833,49.875,2.37088387159997));
#41309=CARTESIAN_POINT('Ctrl Pts',(-6.55514062276576,57.495,2.32875748935431));
#41310=CARTESIAN_POINT('Ctrl Pts',(-6.55514062276576,49.875,2.32875748935431));
#41311=CARTESIAN_POINT('Ctrl Pts',(-6.52084865967131,57.495,2.28771778279682));
#41312=CARTESIAN_POINT('Ctrl Pts',(-6.52084865967131,49.875,2.28771778279682));
#41313=CARTESIAN_POINT('Ctrl Pts',(-6.48641743997165,57.495,2.24777479550452));
#41314=CARTESIAN_POINT('Ctrl Pts',(-6.48641743997165,49.875,2.24777479550452));
#41315=CARTESIAN_POINT('Ctrl Pts',(-6.45185553518355,57.495,2.20893514043546));
#41316=CARTESIAN_POINT('Ctrl Pts',(-6.45185553518355,49.875,2.20893514043546));
#41317=CARTESIAN_POINT('Ctrl Pts',(-6.41717671306116,57.495,2.17120312938032));
#41318=CARTESIAN_POINT('Ctrl Pts',(-6.41717671306116,49.875,2.17120312938032));
#41319=CARTESIAN_POINT('Ctrl Pts',(-6.38240181135686,57.495,2.13458349574322));
#41320=CARTESIAN_POINT('Ctrl Pts',(-6.38240181135686,49.875,2.13458349574322));
#41321=CARTESIAN_POINT('Ctrl Pts',(-6.34756091533109,57.495,2.09908352929886));
#41322=CARTESIAN_POINT('Ctrl Pts',(-6.34756091533109,49.875,2.09908352929886));
#41323=CARTESIAN_POINT('Ctrl Pts',(-6.31269482043472,57.495,2.06471490843565));
#41324=CARTESIAN_POINT('Ctrl Pts',(-6.31269482043472,49.875,2.06471490843565));
#41325=CARTESIAN_POINT('Ctrl Pts',(-6.27785854554207,57.495,2.03149622201774));
#41326=CARTESIAN_POINT('Ctrl Pts',(-6.27785854554207,49.875,2.03149622201774));
#41327=CARTESIAN_POINT('Ctrl Pts',(-6.24311798195999,57.495,1.99945211810842));
#41328=CARTESIAN_POINT('Ctrl Pts',(-6.24311798195999,49.875,1.99945211810842));
#41329=CARTESIAN_POINT('Ctrl Pts',(-6.20853885514991,57.495,1.96860861168855));
#41330=CARTESIAN_POINT('Ctrl Pts',(-6.20853885514991,49.875,1.96860861168855));
#41331=CARTESIAN_POINT('Ctrl Pts',(-6.17417680788948,57.495,1.93898880419738));
#41332=CARTESIAN_POINT('Ctrl Pts',(-6.17417680788948,49.875,1.93898880419738));
#41333=CARTESIAN_POINT('Ctrl Pts',(-6.14006878432979,57.495,1.91060895733316));
#41334=CARTESIAN_POINT('Ctrl Pts',(-6.14006878432979,49.875,1.91060895733316));
#41335=CARTESIAN_POINT('Ctrl Pts',(-6.10621926889293,57.495,1.88347219921807));
#41336=CARTESIAN_POINT('Ctrl Pts',(-6.10621926889293,49.875,1.88347219921807));
#41337=CARTESIAN_POINT('Ctrl Pts',(-6.07260331771224,57.495,1.85756929242873));
#41338=CARTESIAN_POINT('Ctrl Pts',(-6.07260331771224,49.875,1.85756929242873));
#41339=CARTESIAN_POINT('Ctrl Pts',(-6.03920034699142,57.495,1.83289254541003));
#41340=CARTESIAN_POINT('Ctrl Pts',(-6.03920034699142,49.875,1.83289254541003));
#41341=CARTESIAN_POINT('Ctrl Pts',(-6.00602283509636,57.495,1.80944727788364));
#41342=CARTESIAN_POINT('Ctrl Pts',(-6.00602283509636,49.875,1.80944727788364));
#41343=CARTESIAN_POINT('Ctrl Pts',(-5.97314358084405,57.495,1.78726264793637));
#41344=CARTESIAN_POINT('Ctrl Pts',(-5.97314358084405,49.875,1.78726264793637));
#41345=CARTESIAN_POINT('Ctrl Pts',(-5.94073262861954,57.495,1.76640606389863));
#41346=CARTESIAN_POINT('Ctrl Pts',(-5.94073262861954,49.875,1.76640606389863));
#41347=CARTESIAN_POINT('Ctrl Pts',(-5.90906068827417,57.495,1.74698425466385));
#41348=CARTESIAN_POINT('Ctrl Pts',(-5.90906068827417,49.875,1.74698425466385));
#41349=CARTESIAN_POINT('Ctrl Pts',(-5.87844620539466,57.495,1.72912206102237));
#41350=CARTESIAN_POINT('Ctrl Pts',(-5.87844620539466,49.875,1.72912206102237));
#41351=CARTESIAN_POINT('Ctrl Pts',(-5.84921363316514,57.495,1.71294534020681));
#41352=CARTESIAN_POINT('Ctrl Pts',(-5.84921363316514,49.875,1.71294534020681));
#41353=CARTESIAN_POINT('Ctrl Pts',(-5.8216513201319,57.495,1.69856379474193));
#41354=CARTESIAN_POINT('Ctrl Pts',(-5.8216513201319,49.875,1.69856379474193));
#41355=CARTESIAN_POINT('Ctrl Pts',(-5.79595877235173,57.495,1.68604879760681));
#41356=CARTESIAN_POINT('Ctrl Pts',(-5.79595877235173,49.875,1.68604879760681));
#41357=CARTESIAN_POINT('Ctrl Pts',(-5.77224172513534,57.495,1.67543235427339));
#41358=CARTESIAN_POINT('Ctrl Pts',(-5.77224172513534,49.875,1.67543235427339));
#41359=CARTESIAN_POINT('Ctrl Pts',(-5.75488502996854,57.495,1.66846492267669));
#41360=CARTESIAN_POINT('Ctrl Pts',(-5.75488502996854,49.875,1.66846492267669));
#41361=CARTESIAN_POINT('Ctrl Pts',(-5.74278027398956,57.495,1.6640956021081));
#41362=CARTESIAN_POINT('Ctrl Pts',(-5.74278027398956,49.875,1.6640956021081));
#41363=CARTESIAN_POINT('Ctrl Pts',(-5.73511540682054,57.495,1.66156260377489));
#41364=CARTESIAN_POINT('Ctrl Pts',(-5.73511540682054,49.875,1.66156260377489));
#41365=CARTESIAN_POINT('Ctrl Pts',(-5.73138421404289,57.495,1.66039107437148));
#41366=CARTESIAN_POINT('Ctrl Pts',(-5.73138421404289,49.875,1.66039107437148));
#41367=CARTESIAN_POINT('Ctrl Pts',(-6.69081410619341,51.145,2.50394540602692));
#41368=CARTESIAN_POINT('Ctrl Pts',(-6.6840872875067,51.145,2.49477440711622));
#41369=CARTESIAN_POINT('Ctrl Pts',(-6.67061900235319,51.145,2.47653809829367));
#41370=CARTESIAN_POINT('Ctrl Pts',(-6.65037263123044,51.145,2.44950070161195));
#41371=CARTESIAN_POINT('Ctrl Pts',(-6.62328942425873,51.145,2.41408612451247));
#41372=CARTESIAN_POINT('Ctrl Pts',(-6.58928830924833,51.145,2.37088387159997));
#41373=CARTESIAN_POINT('Ctrl Pts',(-6.55514062276576,51.145,2.32875748935431));
#41374=CARTESIAN_POINT('Ctrl Pts',(-6.52084865967131,51.145,2.28771778279682));
#41375=CARTESIAN_POINT('Ctrl Pts',(-6.48641743997165,51.145,2.24777479550452));
#41376=CARTESIAN_POINT('Ctrl Pts',(-6.45185553518355,51.145,2.20893514043546));
#41377=CARTESIAN_POINT('Ctrl Pts',(-6.41717671306116,51.145,2.17120312938032));
#41378=CARTESIAN_POINT('Ctrl Pts',(-6.38240181135686,51.145,2.13458349574322));
#41379=CARTESIAN_POINT('Ctrl Pts',(-6.34756091533109,51.145,2.09908352929886));
#41380=CARTESIAN_POINT('Ctrl Pts',(-6.31269482043472,51.145,2.06471490843565));
#41381=CARTESIAN_POINT('Ctrl Pts',(-6.27785854554207,51.145,2.03149622201774));
#41382=CARTESIAN_POINT('Ctrl Pts',(-6.24311798195999,51.145,1.99945211810842));
#41383=CARTESIAN_POINT('Ctrl Pts',(-6.20853885514991,51.145,1.96860861168855));
#41384=CARTESIAN_POINT('Ctrl Pts',(-6.17417680788948,51.145,1.93898880419738));
#41385=CARTESIAN_POINT('Ctrl Pts',(-6.14006878432979,51.145,1.91060895733316));
#41386=CARTESIAN_POINT('Ctrl Pts',(-6.10621926889293,51.145,1.88347219921807));
#41387=CARTESIAN_POINT('Ctrl Pts',(-6.07260331771224,51.145,1.85756929242873));
#41388=CARTESIAN_POINT('Ctrl Pts',(-6.03920034699142,51.145,1.83289254541003));
#41389=CARTESIAN_POINT('Ctrl Pts',(-6.00602283509636,51.145,1.80944727788364));
#41390=CARTESIAN_POINT('Ctrl Pts',(-5.97314358084405,51.145,1.78726264793637));
#41391=CARTESIAN_POINT('Ctrl Pts',(-5.94073262861954,51.145,1.76640606389863));
#41392=CARTESIAN_POINT('Ctrl Pts',(-5.90906068827417,51.145,1.74698425466385));
#41393=CARTESIAN_POINT('Ctrl Pts',(-5.87844620539466,51.145,1.72912206102237));
#41394=CARTESIAN_POINT('Ctrl Pts',(-5.84921363316514,51.145,1.71294534020681));
#41395=CARTESIAN_POINT('Ctrl Pts',(-5.8216513201319,51.145,1.69856379474193));
#41396=CARTESIAN_POINT('Ctrl Pts',(-5.79595877235173,51.145,1.68604879760681));
#41397=CARTESIAN_POINT('Ctrl Pts',(-5.77224172513534,51.145,1.67543235427339));
#41398=CARTESIAN_POINT('Ctrl Pts',(-5.75488502996854,51.145,1.66846492267669));
#41399=CARTESIAN_POINT('Ctrl Pts',(-5.74278027398956,51.145,1.6640956021081));
#41400=CARTESIAN_POINT('Ctrl Pts',(-5.73511540682054,51.145,1.66156260377489));
#41401=CARTESIAN_POINT('Ctrl Pts',(-5.73138421404289,51.145,1.66039107437148));
#41402=CARTESIAN_POINT('Origin',(0.,54.32,0.));
#41403=CARTESIAN_POINT('',(-4.18409499139877,51.145,3.34686616149372));
#41404=CARTESIAN_POINT('Origin',(0.,51.145,0.));
#41405=CARTESIAN_POINT('',(-4.18409499139877,54.32,3.34686616149372));
#41406=CARTESIAN_POINT('Origin',(-4.65970441290367,57.495,3.72730711280926));
#41407=CARTESIAN_POINT('',(-4.65970441290367,51.145,3.72730711280926));
#41408=CARTESIAN_POINT('',(-4.65970441290367,51.145,3.72730711280926));
#41409=CARTESIAN_POINT('',(-4.65970441290367,57.495,3.72730711280926));
#41410=CARTESIAN_POINT('Origin',(-1.15136842610855E-12,57.495,1.15195721078055E-12));
#41411=CARTESIAN_POINT('',(-5.22328778611671,51.145,4.87380761862879));
#41412=CARTESIAN_POINT('',(-5.22328778611671,57.495,4.87380761862879));
#41413=CARTESIAN_POINT('',(-4.87380761862879,51.145,5.22328778611671));
#41414=CARTESIAN_POINT('Origin',(-1.15136842610855E-12,51.145,1.15195721078055E-12));
#41415=CARTESIAN_POINT('',(-4.87380761862879,57.495,5.22328778611671));
#41416=CARTESIAN_POINT('Ctrl Pts',(-3.72730711280926,57.495,4.65970441290367));
#41417=CARTESIAN_POINT('Ctrl Pts',(-3.72730711280926,49.875,4.65970441290367));
#41418=CARTESIAN_POINT('Ctrl Pts',(-3.72981733050576,57.495,4.66270326064961));
#41419=CARTESIAN_POINT('Ctrl Pts',(-3.72981733050576,49.875,4.66270326064961));
#41420=CARTESIAN_POINT('Ctrl Pts',(-3.73509073349854,57.495,4.6688153380502));
#41421=CARTESIAN_POINT('Ctrl Pts',(-3.73509073349854,49.875,4.6688153380502));
#41422=CARTESIAN_POINT('Ctrl Pts',(-3.7437597489088,57.495,4.67832660775297));
#41423=CARTESIAN_POINT('Ctrl Pts',(-3.7437597489088,49.875,4.67832660775297));
#41424=CARTESIAN_POINT('Ctrl Pts',(-3.7568389360361,57.495,4.69169578253142));
#41425=CARTESIAN_POINT('Ctrl Pts',(-3.7568389360361,49.875,4.69169578253142));
#41426=CARTESIAN_POINT('Ctrl Pts',(-3.77572337177426,57.495,4.70954474005187));
#41427=CARTESIAN_POINT('Ctrl Pts',(-3.77572337177426,49.875,4.70954474005187));
#41428=CARTESIAN_POINT('Ctrl Pts',(-3.79711783384759,57.495,4.72849227702429));
#41429=CARTESIAN_POINT('Ctrl Pts',(-3.79711783384759,49.875,4.72849227702429));
#41430=CARTESIAN_POINT('Ctrl Pts',(-3.82095228990398,57.495,4.74845295472311));
#41431=CARTESIAN_POINT('Ctrl Pts',(-3.82095228990398,49.875,4.74845295472311));
#41432=CARTESIAN_POINT('Ctrl Pts',(-3.84708445224628,57.495,4.76926976684248));
#41433=CARTESIAN_POINT('Ctrl Pts',(-3.84708445224628,49.875,4.76926976684248));
#41434=CARTESIAN_POINT('Ctrl Pts',(-3.87530262274579,57.495,4.79071829540097));
#41435=CARTESIAN_POINT('Ctrl Pts',(-3.87530262274579,49.875,4.79071829540097));
#41436=CARTESIAN_POINT('Ctrl Pts',(-3.90536636162316,57.495,4.81254694822028));
#41437=CARTESIAN_POINT('Ctrl Pts',(-3.90536636162316,49.875,4.81254694822028));
#41438=CARTESIAN_POINT('Ctrl Pts',(-3.93703846717723,57.495,4.83450929444277));
#41439=CARTESIAN_POINT('Ctrl Pts',(-3.93703846717723,49.875,4.83450929444277));
#41440=CARTESIAN_POINT('Ctrl Pts',(-3.97011673859275,57.495,4.85639607415679));
#41441=CARTESIAN_POINT('Ctrl Pts',(-3.97011673859275,49.875,4.85639607415679));
#41442=CARTESIAN_POINT('Ctrl Pts',(-4.00447382552398,57.495,4.8780759828866));
#41443=CARTESIAN_POINT('Ctrl Pts',(-4.00447382552398,49.875,4.8780759828866));
#41444=CARTESIAN_POINT('Ctrl Pts',(-4.04005493051016,57.495,4.89949292161193));
#41445=CARTESIAN_POINT('Ctrl Pts',(-4.04005493051016,49.875,4.89949292161193));
#41446=CARTESIAN_POINT('Ctrl Pts',(-4.07685036350543,57.495,4.92063739759527));
#41447=CARTESIAN_POINT('Ctrl Pts',(-4.07685036350543,49.875,4.92063739759527));
#41448=CARTESIAN_POINT('Ctrl Pts',(-4.11487510765792,57.495,4.94152548435404));
#41449=CARTESIAN_POINT('Ctrl Pts',(-4.11487510765792,49.875,4.94152548435404));
#41450=CARTESIAN_POINT('Ctrl Pts',(-4.15414724283855,57.495,4.9621766920072));
#41451=CARTESIAN_POINT('Ctrl Pts',(-4.15414724283855,49.875,4.9621766920072));
#41452=CARTESIAN_POINT('Ctrl Pts',(-4.19466216292523,57.495,4.98258807456953));
#41453=CARTESIAN_POINT('Ctrl Pts',(-4.19466216292523,49.875,4.98258807456953));
#41454=CARTESIAN_POINT('Ctrl Pts',(-4.23639070615327,57.495,5.00273172317852));
#41455=CARTESIAN_POINT('Ctrl Pts',(-4.23639070615327,49.875,5.00273172317852));
#41456=CARTESIAN_POINT('Ctrl Pts',(-4.27929023600664,57.495,5.02256507114883));
#41457=CARTESIAN_POINT('Ctrl Pts',(-4.27929023600664,49.875,5.02256507114883));
#41458=CARTESIAN_POINT('Ctrl Pts',(-4.32331156573186,57.495,5.04203735157409));
#41459=CARTESIAN_POINT('Ctrl Pts',(-4.32331156573186,49.875,5.04203735157409));
#41460=CARTESIAN_POINT('Ctrl Pts',(-4.36840670797621,57.495,5.06109712122993));
#41461=CARTESIAN_POINT('Ctrl Pts',(-4.36840670797621,49.875,5.06109712122993));
#41462=CARTESIAN_POINT('Ctrl Pts',(-4.41453743405689,57.495,5.07970066295481));
#41463=CARTESIAN_POINT('Ctrl Pts',(-4.41453743405689,49.875,5.07970066295481));
#41464=CARTESIAN_POINT('Ctrl Pts',(-4.46167734280668,57.495,5.09781475579234));
#41465=CARTESIAN_POINT('Ctrl Pts',(-4.46167734280668,49.875,5.09781475579234));
#41466=CARTESIAN_POINT('Ctrl Pts',(-4.50980818622117,57.495,5.11541439426219));
#41467=CARTESIAN_POINT('Ctrl Pts',(-4.50980818622117,49.875,5.11541439426219));
#41468=CARTESIAN_POINT('Ctrl Pts',(-4.55891761694258,57.495,5.13248213818673));
#41469=CARTESIAN_POINT('Ctrl Pts',(-4.55891761694258,49.875,5.13248213818673));
#41470=CARTESIAN_POINT('Ctrl Pts',(-4.60899638270436,57.495,5.14900691787061));
#41471=CARTESIAN_POINT('Ctrl Pts',(-4.60899638270436,49.875,5.14900691787061));
#41472=CARTESIAN_POINT('Ctrl Pts',(-4.66003509375248,57.495,5.16498334493441));
#41473=CARTESIAN_POINT('Ctrl Pts',(-4.66003509375248,49.875,5.16498334493441));
#41474=CARTESIAN_POINT('Ctrl Pts',(-4.71202254995837,57.495,5.1804106250073));
#41475=CARTESIAN_POINT('Ctrl Pts',(-4.71202254995837,49.875,5.1804106250073));
#41476=CARTESIAN_POINT('Ctrl Pts',(-4.764947890579,57.495,5.1952907728175));
#41477=CARTESIAN_POINT('Ctrl Pts',(-4.764947890579,49.875,5.1952907728175));
#41478=CARTESIAN_POINT('Ctrl Pts',(-4.8080309881172,57.495,5.2067598214933));
#41479=CARTESIAN_POINT('Ctrl Pts',(-4.8080309881172,49.875,5.2067598214933));
#41480=CARTESIAN_POINT('Ctrl Pts',(-4.84075823631812,57.495,5.21511826561693));
#41481=CARTESIAN_POINT('Ctrl Pts',(-4.84075823631812,49.875,5.21511826561693));
#41482=CARTESIAN_POINT('Ctrl Pts',(-4.86276047837854,57.495,5.22058260535447));
#41483=CARTESIAN_POINT('Ctrl Pts',(-4.86276047837854,49.875,5.22058260535447));
#41484=CARTESIAN_POINT('Ctrl Pts',(-4.87380761862879,57.495,5.22328778611671));
#41485=CARTESIAN_POINT('Ctrl Pts',(-4.87380761862879,49.875,5.22328778611671));
#41486=CARTESIAN_POINT('',(-3.72730711280926,51.145,4.65970441290367));
#41487=CARTESIAN_POINT('Ctrl Pts',(-3.72730711280926,51.145,4.65970441290367));
#41488=CARTESIAN_POINT('Ctrl Pts',(-3.72981733050576,51.145,4.66270326064961));
#41489=CARTESIAN_POINT('Ctrl Pts',(-3.73509073349854,51.145,4.6688153380502));
#41490=CARTESIAN_POINT('Ctrl Pts',(-3.7437597489088,51.145,4.67832660775297));
#41491=CARTESIAN_POINT('Ctrl Pts',(-3.7568389360361,51.145,4.69169578253142));
#41492=CARTESIAN_POINT('Ctrl Pts',(-3.77572337177426,51.145,4.70954474005187));
#41493=CARTESIAN_POINT('Ctrl Pts',(-3.79711783384759,51.145,4.72849227702429));
#41494=CARTESIAN_POINT('Ctrl Pts',(-3.82095228990398,51.145,4.74845295472311));
#41495=CARTESIAN_POINT('Ctrl Pts',(-3.84708445224628,51.145,4.76926976684248));
#41496=CARTESIAN_POINT('Ctrl Pts',(-3.87530262274579,51.145,4.79071829540097));
#41497=CARTESIAN_POINT('Ctrl Pts',(-3.90536636162316,51.145,4.81254694822028));
#41498=CARTESIAN_POINT('Ctrl Pts',(-3.93703846717723,51.145,4.83450929444277));
#41499=CARTESIAN_POINT('Ctrl Pts',(-3.97011673859275,51.145,4.85639607415679));
#41500=CARTESIAN_POINT('Ctrl Pts',(-4.00447382552398,51.145,4.8780759828866));
#41501=CARTESIAN_POINT('Ctrl Pts',(-4.04005493051016,51.145,4.89949292161193));
#41502=CARTESIAN_POINT('Ctrl Pts',(-4.07685036350543,51.145,4.92063739759527));
#41503=CARTESIAN_POINT('Ctrl Pts',(-4.11487510765792,51.145,4.94152548435404));
#41504=CARTESIAN_POINT('Ctrl Pts',(-4.15414724283855,51.145,4.9621766920072));
#41505=CARTESIAN_POINT('Ctrl Pts',(-4.19466216292523,51.145,4.98258807456953));
#41506=CARTESIAN_POINT('Ctrl Pts',(-4.23639070615327,51.145,5.00273172317852));
#41507=CARTESIAN_POINT('Ctrl Pts',(-4.27929023600664,51.145,5.02256507114883));
#41508=CARTESIAN_POINT('Ctrl Pts',(-4.32331156573186,51.145,5.04203735157409));
#41509=CARTESIAN_POINT('Ctrl Pts',(-4.36840670797621,51.145,5.06109712122993));
#41510=CARTESIAN_POINT('Ctrl Pts',(-4.41453743405689,51.145,5.07970066295481));
#41511=CARTESIAN_POINT('Ctrl Pts',(-4.46167734280668,51.145,5.09781475579234));
#41512=CARTESIAN_POINT('Ctrl Pts',(-4.50980818622117,51.145,5.11541439426219));
#41513=CARTESIAN_POINT('Ctrl Pts',(-4.55891761694258,51.145,5.13248213818673));
#41514=CARTESIAN_POINT('Ctrl Pts',(-4.60899638270436,51.145,5.14900691787061));
#41515=CARTESIAN_POINT('Ctrl Pts',(-4.66003509375248,51.145,5.16498334493441));
#41516=CARTESIAN_POINT('Ctrl Pts',(-4.71202254995837,51.145,5.1804106250073));
#41517=CARTESIAN_POINT('Ctrl Pts',(-4.764947890579,51.145,5.1952907728175));
#41518=CARTESIAN_POINT('Ctrl Pts',(-4.8080309881172,51.145,5.2067598214933));
#41519=CARTESIAN_POINT('Ctrl Pts',(-4.84075823631812,51.145,5.21511826561693));
#41520=CARTESIAN_POINT('Ctrl Pts',(-4.86276047837854,51.145,5.22058260535447));
#41521=CARTESIAN_POINT('Ctrl Pts',(-4.87380761862879,51.145,5.22328778611671));
#41522=CARTESIAN_POINT('',(-3.72730711280926,57.495,4.65970441290367));
#41523=CARTESIAN_POINT('Origin',(-3.25316890053365,57.495,4.06695907338649));
#41524=CARTESIAN_POINT('',(-3.34686616149372,51.145,4.18409499139877));
#41525=CARTESIAN_POINT('',(-3.34686616149372,54.32,4.18409499139877));
#41526=CARTESIAN_POINT('',(-3.25316890053365,51.145,4.06695907338649));
#41527=CARTESIAN_POINT('Ctrl Pts',(-5.22328778611671,57.495,4.87380761862879));
#41528=CARTESIAN_POINT('Ctrl Pts',(-5.22328778611671,49.875,4.87380761862879));
#41529=CARTESIAN_POINT('Ctrl Pts',(-5.22058260535451,57.495,4.86276047837859));
#41530=CARTESIAN_POINT('Ctrl Pts',(-5.22058260535451,49.875,4.86276047837859));
#41531=CARTESIAN_POINT('Ctrl Pts',(-5.21511826561704,57.495,4.84075823631825));
#41532=CARTESIAN_POINT('Ctrl Pts',(-5.21511826561704,49.875,4.84075823631825));
#41533=CARTESIAN_POINT('Ctrl Pts',(-5.20675982149348,57.495,4.80803098811744));
#41534=CARTESIAN_POINT('Ctrl Pts',(-5.20675982149348,49.875,4.80803098811744));
#41535=CARTESIAN_POINT('Ctrl Pts',(-5.19529077281773,57.495,4.7649478905793));
#41536=CARTESIAN_POINT('Ctrl Pts',(-5.19529077281773,49.875,4.7649478905793));
#41537=CARTESIAN_POINT('Ctrl Pts',(-5.18041062500752,57.495,4.71202254995864));
#41538=CARTESIAN_POINT('Ctrl Pts',(-5.18041062500752,49.875,4.71202254995864));
#41539=CARTESIAN_POINT('Ctrl Pts',(-5.16498334493456,57.495,4.66003509375265));
#41540=CARTESIAN_POINT('Ctrl Pts',(-5.16498334493456,49.875,4.66003509375265));
#41541=CARTESIAN_POINT('Ctrl Pts',(-5.14900691787064,57.495,4.60899638270439));
#41542=CARTESIAN_POINT('Ctrl Pts',(-5.14900691787064,49.875,4.60899638270439));
#41543=CARTESIAN_POINT('Ctrl Pts',(-5.13248213818666,57.495,4.5589176169425));
#41544=CARTESIAN_POINT('Ctrl Pts',(-5.13248213818666,49.875,4.5589176169425));
#41545=CARTESIAN_POINT('Ctrl Pts',(-5.11541439426204,57.495,4.50980818622101));
#41546=CARTESIAN_POINT('Ctrl Pts',(-5.11541439426204,49.875,4.50980818622101));
#41547=CARTESIAN_POINT('Ctrl Pts',(-5.09781475579217,57.495,4.4616773428065));
#41548=CARTESIAN_POINT('Ctrl Pts',(-5.09781475579217,49.875,4.4616773428065));
#41549=CARTESIAN_POINT('Ctrl Pts',(-5.07970066295468,57.495,4.41453743405677));
#41550=CARTESIAN_POINT('Ctrl Pts',(-5.07970066295468,49.875,4.41453743405677));
#41551=CARTESIAN_POINT('Ctrl Pts',(-5.06109712122989,57.495,4.36840670797617));
#41552=CARTESIAN_POINT('Ctrl Pts',(-5.06109712122989,49.875,4.36840670797617));
#41553=CARTESIAN_POINT('Ctrl Pts',(-5.04203735157413,57.495,4.3233115657319));
#41554=CARTESIAN_POINT('Ctrl Pts',(-5.04203735157413,49.875,4.3233115657319));
#41555=CARTESIAN_POINT('Ctrl Pts',(-5.02256507114894,57.495,4.27929023600674));
#41556=CARTESIAN_POINT('Ctrl Pts',(-5.02256507114894,49.875,4.27929023600674));
#41557=CARTESIAN_POINT('Ctrl Pts',(-5.00273172317863,57.495,4.23639070615337));
#41558=CARTESIAN_POINT('Ctrl Pts',(-5.00273172317863,49.875,4.23639070615337));
#41559=CARTESIAN_POINT('Ctrl Pts',(-4.98258807456962,57.495,4.1946621629253));
#41560=CARTESIAN_POINT('Ctrl Pts',(-4.98258807456962,49.875,4.1946621629253));
#41561=CARTESIAN_POINT('Ctrl Pts',(-4.96217669200723,57.495,4.15414724283858));
#41562=CARTESIAN_POINT('Ctrl Pts',(-4.96217669200723,49.875,4.15414724283858));
#41563=CARTESIAN_POINT('Ctrl Pts',(-4.94152548435402,57.495,4.11487510765791));
#41564=CARTESIAN_POINT('Ctrl Pts',(-4.94152548435402,49.875,4.11487510765791));
#41565=CARTESIAN_POINT('Ctrl Pts',(-4.92063739759521,57.495,4.07685036350539));
#41566=CARTESIAN_POINT('Ctrl Pts',(-4.92063739759521,49.875,4.07685036350539));
#41567=CARTESIAN_POINT('Ctrl Pts',(-4.89949292161185,57.495,4.04005493051012));
#41568=CARTESIAN_POINT('Ctrl Pts',(-4.89949292161185,49.875,4.04005493051012));
#41569=CARTESIAN_POINT('Ctrl Pts',(-4.87807598288654,57.495,4.00447382552396));
#41570=CARTESIAN_POINT('Ctrl Pts',(-4.87807598288654,49.875,4.00447382552396));
#41571=CARTESIAN_POINT('Ctrl Pts',(-4.85639607415676,57.495,3.97011673859274));
#41572=CARTESIAN_POINT('Ctrl Pts',(-4.85639607415676,49.875,3.97011673859274));
#41573=CARTESIAN_POINT('Ctrl Pts',(-4.83450929444279,57.495,3.93703846717724));
#41574=CARTESIAN_POINT('Ctrl Pts',(-4.83450929444279,49.875,3.93703846717724));
#41575=CARTESIAN_POINT('Ctrl Pts',(-4.81254694822034,57.495,3.90536636162318));
#41576=CARTESIAN_POINT('Ctrl Pts',(-4.81254694822034,49.875,3.90536636162318));
#41577=CARTESIAN_POINT('Ctrl Pts',(-4.79071829540103,57.495,3.8753026227458));
#41578=CARTESIAN_POINT('Ctrl Pts',(-4.79071829540103,49.875,3.8753026227458));
#41579=CARTESIAN_POINT('Ctrl Pts',(-4.76926976684252,57.495,3.84708445224627));
#41580=CARTESIAN_POINT('Ctrl Pts',(-4.76926976684252,49.875,3.84708445224627));
#41581=CARTESIAN_POINT('Ctrl Pts',(-4.74845295472312,57.495,3.82095228990397));
#41582=CARTESIAN_POINT('Ctrl Pts',(-4.74845295472312,49.875,3.82095228990397));
#41583=CARTESIAN_POINT('Ctrl Pts',(-4.72849227702427,57.495,3.7971178338476));
#41584=CARTESIAN_POINT('Ctrl Pts',(-4.72849227702427,49.875,3.7971178338476));
#41585=CARTESIAN_POINT('Ctrl Pts',(-4.7095447400518,57.495,3.77572337177431));
#41586=CARTESIAN_POINT('Ctrl Pts',(-4.7095447400518,49.875,3.77572337177431));
#41587=CARTESIAN_POINT('Ctrl Pts',(-4.69169578253132,57.495,3.75683893603616));
#41588=CARTESIAN_POINT('Ctrl Pts',(-4.69169578253132,49.875,3.75683893603616));
#41589=CARTESIAN_POINT('Ctrl Pts',(-4.67832660775287,57.495,3.74375974890886));
#41590=CARTESIAN_POINT('Ctrl Pts',(-4.67832660775287,49.875,3.74375974890886));
#41591=CARTESIAN_POINT('Ctrl Pts',(-4.66881533805013,57.495,3.73509073349858));
#41592=CARTESIAN_POINT('Ctrl Pts',(-4.66881533805013,49.875,3.73509073349858));
#41593=CARTESIAN_POINT('Ctrl Pts',(-4.66270326064959,57.495,3.72981733050578));
#41594=CARTESIAN_POINT('Ctrl Pts',(-4.66270326064959,49.875,3.72981733050578));
#41595=CARTESIAN_POINT('Ctrl Pts',(-4.65970441290367,57.495,3.72730711280926));
#41596=CARTESIAN_POINT('Ctrl Pts',(-4.65970441290367,49.875,3.72730711280926));
#41597=CARTESIAN_POINT('Ctrl Pts',(-5.22328778611671,51.145,4.87380761862879));
#41598=CARTESIAN_POINT('Ctrl Pts',(-5.22058260535451,51.145,4.86276047837859));
#41599=CARTESIAN_POINT('Ctrl Pts',(-5.21511826561704,51.145,4.84075823631825));
#41600=CARTESIAN_POINT('Ctrl Pts',(-5.20675982149348,51.145,4.80803098811744));
#41601=CARTESIAN_POINT('Ctrl Pts',(-5.19529077281773,51.145,4.7649478905793));
#41602=CARTESIAN_POINT('Ctrl Pts',(-5.18041062500752,51.145,4.71202254995864));
#41603=CARTESIAN_POINT('Ctrl Pts',(-5.16498334493456,51.145,4.66003509375265));
#41604=CARTESIAN_POINT('Ctrl Pts',(-5.14900691787064,51.145,4.60899638270439));
#41605=CARTESIAN_POINT('Ctrl Pts',(-5.13248213818666,51.145,4.5589176169425));
#41606=CARTESIAN_POINT('Ctrl Pts',(-5.11541439426204,51.145,4.50980818622101));
#41607=CARTESIAN_POINT('Ctrl Pts',(-5.09781475579217,51.145,4.4616773428065));
#41608=CARTESIAN_POINT('Ctrl Pts',(-5.07970066295468,51.145,4.41453743405677));
#41609=CARTESIAN_POINT('Ctrl Pts',(-5.06109712122989,51.145,4.36840670797617));
#41610=CARTESIAN_POINT('Ctrl Pts',(-5.04203735157413,51.145,4.3233115657319));
#41611=CARTESIAN_POINT('Ctrl Pts',(-5.02256507114894,51.145,4.27929023600674));
#41612=CARTESIAN_POINT('Ctrl Pts',(-5.00273172317863,51.145,4.23639070615337));
#41613=CARTESIAN_POINT('Ctrl Pts',(-4.98258807456962,51.145,4.1946621629253));
#41614=CARTESIAN_POINT('Ctrl Pts',(-4.96217669200723,51.145,4.15414724283858));
#41615=CARTESIAN_POINT('Ctrl Pts',(-4.94152548435402,51.145,4.11487510765791));
#41616=CARTESIAN_POINT('Ctrl Pts',(-4.92063739759521,51.145,4.07685036350539));
#41617=CARTESIAN_POINT('Ctrl Pts',(-4.89949292161185,51.145,4.04005493051012));
#41618=CARTESIAN_POINT('Ctrl Pts',(-4.87807598288654,51.145,4.00447382552396));
#41619=CARTESIAN_POINT('Ctrl Pts',(-4.85639607415676,51.145,3.97011673859274));
#41620=CARTESIAN_POINT('Ctrl Pts',(-4.83450929444279,51.145,3.93703846717724));
#41621=CARTESIAN_POINT('Ctrl Pts',(-4.81254694822034,51.145,3.90536636162318));
#41622=CARTESIAN_POINT('Ctrl Pts',(-4.79071829540103,51.145,3.8753026227458));
#41623=CARTESIAN_POINT('Ctrl Pts',(-4.76926976684252,51.145,3.84708445224627));
#41624=CARTESIAN_POINT('Ctrl Pts',(-4.74845295472312,51.145,3.82095228990397));
#41625=CARTESIAN_POINT('Ctrl Pts',(-4.72849227702427,51.145,3.7971178338476));
#41626=CARTESIAN_POINT('Ctrl Pts',(-4.7095447400518,51.145,3.77572337177431));
#41627=CARTESIAN_POINT('Ctrl Pts',(-4.69169578253132,51.145,3.75683893603616));
#41628=CARTESIAN_POINT('Ctrl Pts',(-4.67832660775287,51.145,3.74375974890886));
#41629=CARTESIAN_POINT('Ctrl Pts',(-4.66881533805013,51.145,3.73509073349858));
#41630=CARTESIAN_POINT('Ctrl Pts',(-4.66270326064959,51.145,3.72981733050578));
#41631=CARTESIAN_POINT('Ctrl Pts',(-4.65970441290367,51.145,3.72730711280926));
#41632=CARTESIAN_POINT('Origin',(0.,54.32,0.));
#41633=CARTESIAN_POINT('',(-2.58480949428933,51.145,4.69328497730872));
#41634=CARTESIAN_POINT('Origin',(0.,51.145,0.));
#41635=CARTESIAN_POINT('',(-2.58480949428933,54.32,4.69328497730872));
#41636=CARTESIAN_POINT('Origin',(-1.4491783055134,57.495,5.00231408838243));
#41637=CARTESIAN_POINT('',(-1.4909173120086,51.145,5.1463899549833));
#41638=CARTESIAN_POINT('',(-1.4909173120086,54.32,5.1463899549833));
#41639=CARTESIAN_POINT('',(-1.66039107437148,51.145,5.73138421404289));
#41640=CARTESIAN_POINT('',(-1.66039107437148,57.495,5.73138421404289));
#41641=CARTESIAN_POINT('',(-1.4491783055134,51.145,5.00231408838243));
#41642=CARTESIAN_POINT('Origin',(-2.87862685522557,57.495,5.22677443144495));
#41643=CARTESIAN_POINT('',(-2.87862685522557,51.145,5.22677443144495));
#41644=CARTESIAN_POINT('',(-2.87862685522557,51.145,5.22677443144495));
#41645=CARTESIAN_POINT('',(-2.87862685522557,57.495,5.22677443144495));
#41646=CARTESIAN_POINT('Origin',(-6.22890783902202E-13,57.495,1.50487931058895E-12));
#41647=CARTESIAN_POINT('',(-2.96056324982543,51.145,6.50167680247051));
#41648=CARTESIAN_POINT('',(-2.96056324982543,57.495,6.50167680247051));
#41649=CARTESIAN_POINT('',(-2.50394540602692,51.145,6.69081410619341));
#41650=CARTESIAN_POINT('Origin',(-6.22890783902202E-13,51.145,1.50487931058895E-12));
#41651=CARTESIAN_POINT('',(-2.50394540602692,57.495,6.69081410619341));
#41652=CARTESIAN_POINT('Ctrl Pts',(-1.66039107437148,57.495,5.73138421404289));
#41653=CARTESIAN_POINT('Ctrl Pts',(-1.66039107437148,49.875,5.73138421404289));
#41654=CARTESIAN_POINT('Ctrl Pts',(-1.66156260377487,57.495,5.73511540682056));
#41655=CARTESIAN_POINT('Ctrl Pts',(-1.66156260377487,49.875,5.73511540682056));
#41656=CARTESIAN_POINT('Ctrl Pts',(-1.66409560210805,57.495,5.7427802739896));
#41657=CARTESIAN_POINT('Ctrl Pts',(-1.66409560210805,49.875,5.7427802739896));
#41658=CARTESIAN_POINT('Ctrl Pts',(-1.6684649226766,57.495,5.75488502996861));
#41659=CARTESIAN_POINT('Ctrl Pts',(-1.6684649226766,49.875,5.75488502996861));
#41660=CARTESIAN_POINT('Ctrl Pts',(-1.67543235427329,57.495,5.77224172513541));
#41661=CARTESIAN_POINT('Ctrl Pts',(-1.67543235427329,49.875,5.77224172513541));
#41662=CARTESIAN_POINT('Ctrl Pts',(-1.68604879760674,57.495,5.79595877235177));
#41663=CARTESIAN_POINT('Ctrl Pts',(-1.68604879760674,49.875,5.79595877235177));
#41664=CARTESIAN_POINT('Ctrl Pts',(-1.69856379474191,57.495,5.82165132013192));
#41665=CARTESIAN_POINT('Ctrl Pts',(-1.69856379474191,49.875,5.82165132013192));
#41666=CARTESIAN_POINT('Ctrl Pts',(-1.71294534020683,57.495,5.84921363316513));
#41667=CARTESIAN_POINT('Ctrl Pts',(-1.71294534020683,49.875,5.84921363316513));
#41668=CARTESIAN_POINT('Ctrl Pts',(-1.7291220610224,57.495,5.87844620539462));
#41669=CARTESIAN_POINT('Ctrl Pts',(-1.7291220610224,49.875,5.87844620539462));
#41670=CARTESIAN_POINT('Ctrl Pts',(-1.74698425466387,57.495,5.90906068827411));
#41671=CARTESIAN_POINT('Ctrl Pts',(-1.74698425466387,49.875,5.90906068827411));
#41672=CARTESIAN_POINT('Ctrl Pts',(-1.76640606389864,57.495,5.94073262861949));
#41673=CARTESIAN_POINT('Ctrl Pts',(-1.76640606389864,49.875,5.94073262861949));
#41674=CARTESIAN_POINT('Ctrl Pts',(-1.78726264793636,57.495,5.97314358084403));
#41675=CARTESIAN_POINT('Ctrl Pts',(-1.78726264793636,49.875,5.97314358084403));
#41676=CARTESIAN_POINT('Ctrl Pts',(-1.80944727788364,57.495,6.0060228350964));
#41677=CARTESIAN_POINT('Ctrl Pts',(-1.80944727788364,49.875,6.0060228350964));
#41678=CARTESIAN_POINT('Ctrl Pts',(-1.83289254541003,57.495,6.03920034699149));
#41679=CARTESIAN_POINT('Ctrl Pts',(-1.83289254541003,49.875,6.03920034699149));
#41680=CARTESIAN_POINT('Ctrl Pts',(-1.85756929242873,57.495,6.07260331771232));
#41681=CARTESIAN_POINT('Ctrl Pts',(-1.85756929242873,49.875,6.07260331771232));
#41682=CARTESIAN_POINT('Ctrl Pts',(-1.88347219921808,57.495,6.10621926889299));
#41683=CARTESIAN_POINT('Ctrl Pts',(-1.88347219921808,49.875,6.10621926889299));
#41684=CARTESIAN_POINT('Ctrl Pts',(-1.91060895733317,57.495,6.14006878432982));
#41685=CARTESIAN_POINT('Ctrl Pts',(-1.91060895733317,49.875,6.14006878432982));
#41686=CARTESIAN_POINT('Ctrl Pts',(-1.93898880419737,57.495,6.17417680788945));
#41687=CARTESIAN_POINT('Ctrl Pts',(-1.93898880419737,49.875,6.17417680788945));
#41688=CARTESIAN_POINT('Ctrl Pts',(-1.96860861168851,57.495,6.20853885514981));
#41689=CARTESIAN_POINT('Ctrl Pts',(-1.96860861168851,49.875,6.20853885514981));
#41690=CARTESIAN_POINT('Ctrl Pts',(-1.99945211810837,57.495,6.24311798195985));
#41691=CARTESIAN_POINT('Ctrl Pts',(-1.99945211810837,49.875,6.24311798195985));
#41692=CARTESIAN_POINT('Ctrl Pts',(-2.03149622201768,57.495,6.27785854554194));
#41693=CARTESIAN_POINT('Ctrl Pts',(-2.03149622201768,49.875,6.27785854554194));
#41694=CARTESIAN_POINT('Ctrl Pts',(-2.06471490843563,57.495,6.31269482043467));
#41695=CARTESIAN_POINT('Ctrl Pts',(-2.06471490843563,49.875,6.31269482043467));
#41696=CARTESIAN_POINT('Ctrl Pts',(-2.09908352929888,57.495,6.34756091533115));
#41697=CARTESIAN_POINT('Ctrl Pts',(-2.09908352929888,49.875,6.34756091533115));
#41698=CARTESIAN_POINT('Ctrl Pts',(-2.13458349574329,57.495,6.38240181135703));
#41699=CARTESIAN_POINT('Ctrl Pts',(-2.13458349574329,49.875,6.38240181135703));
#41700=CARTESIAN_POINT('Ctrl Pts',(-2.17120312938042,57.495,6.41717671306138));
#41701=CARTESIAN_POINT('Ctrl Pts',(-2.17120312938042,49.875,6.41717671306138));
#41702=CARTESIAN_POINT('Ctrl Pts',(-2.20893514043555,57.495,6.45185553518375));
#41703=CARTESIAN_POINT('Ctrl Pts',(-2.20893514043555,49.875,6.45185553518375));
#41704=CARTESIAN_POINT('Ctrl Pts',(-2.24777479550457,57.495,6.48641743997175));
#41705=CARTESIAN_POINT('Ctrl Pts',(-2.24777479550457,49.875,6.48641743997175));
#41706=CARTESIAN_POINT('Ctrl Pts',(-2.2877177827968,57.495,6.52084865967127));
#41707=CARTESIAN_POINT('Ctrl Pts',(-2.2877177827968,49.875,6.52084865967127));
#41708=CARTESIAN_POINT('Ctrl Pts',(-2.32875748935421,57.495,6.55514062276556));
#41709=CARTESIAN_POINT('Ctrl Pts',(-2.32875748935421,49.875,6.55514062276556));
#41710=CARTESIAN_POINT('Ctrl Pts',(-2.37088387159981,57.495,6.58928830924802));
#41711=CARTESIAN_POINT('Ctrl Pts',(-2.37088387159981,49.875,6.58928830924802));
#41712=CARTESIAN_POINT('Ctrl Pts',(-2.41408612451229,57.495,6.6232894242584));
#41713=CARTESIAN_POINT('Ctrl Pts',(-2.41408612451229,49.875,6.6232894242584));
#41714=CARTESIAN_POINT('Ctrl Pts',(-2.4495007016118,57.495,6.65037263123018));
#41715=CARTESIAN_POINT('Ctrl Pts',(-2.4495007016118,49.875,6.65037263123018));
#41716=CARTESIAN_POINT('Ctrl Pts',(-2.47653809829358,57.495,6.67061900235304));
#41717=CARTESIAN_POINT('Ctrl Pts',(-2.47653809829358,49.875,6.67061900235304));
#41718=CARTESIAN_POINT('Ctrl Pts',(-2.49477440711619,57.495,6.68408728750664));
#41719=CARTESIAN_POINT('Ctrl Pts',(-2.49477440711619,49.875,6.68408728750664));
#41720=CARTESIAN_POINT('Ctrl Pts',(-2.50394540602692,57.495,6.69081410619341));
#41721=CARTESIAN_POINT('Ctrl Pts',(-2.50394540602692,49.875,6.69081410619341));
#41722=CARTESIAN_POINT('Ctrl Pts',(-1.66039107437148,51.145,5.73138421404289));
#41723=CARTESIAN_POINT('Ctrl Pts',(-1.66156260377487,51.145,5.73511540682056));
#41724=CARTESIAN_POINT('Ctrl Pts',(-1.66409560210805,51.145,5.7427802739896));
#41725=CARTESIAN_POINT('Ctrl Pts',(-1.6684649226766,51.145,5.75488502996861));
#41726=CARTESIAN_POINT('Ctrl Pts',(-1.67543235427329,51.145,5.77224172513541));
#41727=CARTESIAN_POINT('Ctrl Pts',(-1.68604879760674,51.145,5.79595877235177));
#41728=CARTESIAN_POINT('Ctrl Pts',(-1.69856379474191,51.145,5.82165132013192));
#41729=CARTESIAN_POINT('Ctrl Pts',(-1.71294534020683,51.145,5.84921363316513));
#41730=CARTESIAN_POINT('Ctrl Pts',(-1.7291220610224,51.145,5.87844620539462));
#41731=CARTESIAN_POINT('Ctrl Pts',(-1.74698425466387,51.145,5.90906068827411));
#41732=CARTESIAN_POINT('Ctrl Pts',(-1.76640606389864,51.145,5.94073262861949));
#41733=CARTESIAN_POINT('Ctrl Pts',(-1.78726264793636,51.145,5.97314358084403));
#41734=CARTESIAN_POINT('Ctrl Pts',(-1.80944727788364,51.145,6.0060228350964));
#41735=CARTESIAN_POINT('Ctrl Pts',(-1.83289254541003,51.145,6.03920034699149));
#41736=CARTESIAN_POINT('Ctrl Pts',(-1.85756929242873,51.145,6.07260331771232));
#41737=CARTESIAN_POINT('Ctrl Pts',(-1.88347219921808,51.145,6.10621926889299));
#41738=CARTESIAN_POINT('Ctrl Pts',(-1.91060895733317,51.145,6.14006878432982));
#41739=CARTESIAN_POINT('Ctrl Pts',(-1.93898880419737,51.145,6.17417680788945));
#41740=CARTESIAN_POINT('Ctrl Pts',(-1.96860861168851,51.145,6.20853885514981));
#41741=CARTESIAN_POINT('Ctrl Pts',(-1.99945211810837,51.145,6.24311798195985));
#41742=CARTESIAN_POINT('Ctrl Pts',(-2.03149622201768,51.145,6.27785854554194));
#41743=CARTESIAN_POINT('Ctrl Pts',(-2.06471490843563,51.145,6.31269482043467));
#41744=CARTESIAN_POINT('Ctrl Pts',(-2.09908352929888,51.145,6.34756091533115));
#41745=CARTESIAN_POINT('Ctrl Pts',(-2.13458349574329,51.145,6.38240181135703));
#41746=CARTESIAN_POINT('Ctrl Pts',(-2.17120312938042,51.145,6.41717671306138));
#41747=CARTESIAN_POINT('Ctrl Pts',(-2.20893514043555,51.145,6.45185553518375));
#41748=CARTESIAN_POINT('Ctrl Pts',(-2.24777479550457,51.145,6.48641743997175));
#41749=CARTESIAN_POINT('Ctrl Pts',(-2.2877177827968,51.145,6.52084865967127));
#41750=CARTESIAN_POINT('Ctrl Pts',(-2.32875748935421,51.145,6.55514062276556));
#41751=CARTESIAN_POINT('Ctrl Pts',(-2.37088387159981,51.145,6.58928830924802));
#41752=CARTESIAN_POINT('Ctrl Pts',(-2.41408612451229,51.145,6.6232894242584));
#41753=CARTESIAN_POINT('Ctrl Pts',(-2.4495007016118,51.145,6.65037263123018));
#41754=CARTESIAN_POINT('Ctrl Pts',(-2.47653809829358,51.145,6.67061900235304));
#41755=CARTESIAN_POINT('Ctrl Pts',(-2.49477440711619,51.145,6.68408728750664));
#41756=CARTESIAN_POINT('Ctrl Pts',(-2.50394540602692,51.145,6.69081410619341));
#41757=CARTESIAN_POINT('Ctrl Pts',(-2.96056324982543,57.495,6.50167680247051));
#41758=CARTESIAN_POINT('Ctrl Pts',(-2.96056324982543,49.875,6.50167680247051));
#41759=CARTESIAN_POINT('Ctrl Pts',(-2.96229154623625,57.495,6.49043534784131));
#41760=CARTESIAN_POINT('Ctrl Pts',(-2.96229154623625,49.875,6.49043534784131));
#41761=CARTESIAN_POINT('Ctrl Pts',(-2.96566304810549,57.495,6.46801681444607));
#41762=CARTESIAN_POINT('Ctrl Pts',(-2.96566304810549,49.875,6.46801681444607));
#41763=CARTESIAN_POINT('Ctrl Pts',(-2.97046502832945,57.495,6.43458214159149));
#41764=CARTESIAN_POINT('Ctrl Pts',(-2.97046502832945,49.875,6.43458214159149));
#41765=CARTESIAN_POINT('Ctrl Pts',(-2.97635619664337,57.495,6.39038953466561));
#41766=CARTESIAN_POINT('Ctrl Pts',(-2.97635619664337,49.875,6.39038953466561));
#41767=CARTESIAN_POINT('Ctrl Pts',(-2.98286238364857,57.495,6.33579850967689));
#41768=CARTESIAN_POINT('Ctrl Pts',(-2.98286238364857,49.875,6.33579850967689));
#41769=CARTESIAN_POINT('Ctrl Pts',(-2.98850417352769,57.495,6.28186459845047));
#41770=CARTESIAN_POINT('Ctrl Pts',(-2.98850417352769,49.875,6.28186459845047));
#41771=CARTESIAN_POINT('Ctrl Pts',(-2.99327554868811,57.495,6.22859706400147));
#41772=CARTESIAN_POINT('Ctrl Pts',(-2.99327554868811,49.875,6.22859706400147));
#41773=CARTESIAN_POINT('Ctrl Pts',(-2.99717295692919,57.495,6.17600655789209));
#41774=CARTESIAN_POINT('Ctrl Pts',(-2.99717295692919,49.875,6.17600655789209));
#41775=CARTESIAN_POINT('Ctrl Pts',(-3.00019778316108,57.495,6.12410381716742));
#41776=CARTESIAN_POINT('Ctrl Pts',(-3.00019778316108,49.875,6.12410381716742));
#41777=CARTESIAN_POINT('Ctrl Pts',(-3.00235671375967,57.495,6.07290162599622));
#41778=CARTESIAN_POINT('Ctrl Pts',(-3.00235671375967,49.875,6.07290162599622));
#41779=CARTESIAN_POINT('Ctrl Pts',(-3.00366113621883,57.495,6.02241806591666));
#41780=CARTESIAN_POINT('Ctrl Pts',(-3.00366113621883,49.875,6.02241806591666));
#41781=CARTESIAN_POINT('Ctrl Pts',(-3.00412716938109,57.495,5.97267956506952));
#41782=CARTESIAN_POINT('Ctrl Pts',(-3.00412716938109,49.875,5.97267956506952));
#41783=CARTESIAN_POINT('Ctrl Pts',(-3.00377540211877,57.495,5.9237232280624));
#41784=CARTESIAN_POINT('Ctrl Pts',(-3.00377540211877,49.875,5.9237232280624));
#41785=CARTESIAN_POINT('Ctrl Pts',(-3.00263159433912,57.495,5.87560110342631));
#41786=CARTESIAN_POINT('Ctrl Pts',(-3.00263159433912,49.875,5.87560110342631));
#41787=CARTESIAN_POINT('Ctrl Pts',(-3.00072490941932,57.495,5.82837721216385));
#41788=CARTESIAN_POINT('Ctrl Pts',(-3.00072490941932,49.875,5.82837721216385));
#41789=CARTESIAN_POINT('Ctrl Pts',(-2.99808342690946,57.495,5.78211642456387));
#41790=CARTESIAN_POINT('Ctrl Pts',(-2.99808342690946,49.875,5.78211642456387));
#41791=CARTESIAN_POINT('Ctrl Pts',(-2.9947301570106,57.495,5.73687442119613));
#41792=CARTESIAN_POINT('Ctrl Pts',(-2.9947301570106,49.875,5.73687442119613));
#41793=CARTESIAN_POINT('Ctrl Pts',(-2.9906797244254,57.495,5.69268882427748));
#41794=CARTESIAN_POINT('Ctrl Pts',(-2.9906797244254,49.875,5.69268882427748));
#41795=CARTESIAN_POINT('Ctrl Pts',(-2.98593308820271,57.495,5.64956501668959));
#41796=CARTESIAN_POINT('Ctrl Pts',(-2.98593308820271,49.875,5.64956501668959));
#41797=CARTESIAN_POINT('Ctrl Pts',(-2.98047914221,57.495,5.6074788286105));
#41798=CARTESIAN_POINT('Ctrl Pts',(-2.98047914221,49.875,5.6074788286105));
#41799=CARTESIAN_POINT('Ctrl Pts',(-2.97430877025609,57.495,5.56641026634749));
#41800=CARTESIAN_POINT('Ctrl Pts',(-2.97430877025609,49.875,5.56641026634749));
#41801=CARTESIAN_POINT('Ctrl Pts',(-2.96742703426683,57.495,5.52637191504895));
#41802=CARTESIAN_POINT('Ctrl Pts',(-2.96742703426683,49.875,5.52637191504895));
#41803=CARTESIAN_POINT('Ctrl Pts',(-2.9598647928985,57.495,5.48743586913296));
#41804=CARTESIAN_POINT('Ctrl Pts',(-2.9598647928985,49.875,5.48743586913296));
#41805=CARTESIAN_POINT('Ctrl Pts',(-2.95169462080131,57.495,5.44977003302482));
#41806=CARTESIAN_POINT('Ctrl Pts',(-2.95169462080131,49.875,5.44977003302482));
#41807=CARTESIAN_POINT('Ctrl Pts',(-2.94303247002258,57.495,5.41364129622045));
#41808=CARTESIAN_POINT('Ctrl Pts',(-2.94303247002258,49.875,5.41364129622045));
#41809=CARTESIAN_POINT('Ctrl Pts',(-2.93401523982671,57.495,5.37936310952307));
#41810=CARTESIAN_POINT('Ctrl Pts',(-2.93401523982671,49.875,5.37936310952307));
#41811=CARTESIAN_POINT('Ctrl Pts',(-2.92478335875774,57.495,5.34725389048201));
#41812=CARTESIAN_POINT('Ctrl Pts',(-2.92478335875774,49.875,5.34725389048201));
#41813=CARTESIAN_POINT('Ctrl Pts',(-2.91546314862891,57.495,5.31759510370885));
#41814=CARTESIAN_POINT('Ctrl Pts',(-2.91546314862891,49.875,5.31759510370885));
#41815=CARTESIAN_POINT('Ctrl Pts',(-2.90614521320837,57.495,5.29057828960676));
#41816=CARTESIAN_POINT('Ctrl Pts',(-2.90614521320837,49.875,5.29057828960676));
#41817=CARTESIAN_POINT('Ctrl Pts',(-2.89688168736508,57.495,5.26630084561719));
#41818=CARTESIAN_POINT('Ctrl Pts',(-2.89688168736508,49.875,5.26630084561719));
#41819=CARTESIAN_POINT('Ctrl Pts',(-2.88953536864313,57.495,5.24910109063628));
#41820=CARTESIAN_POINT('Ctrl Pts',(-2.88953536864313,49.875,5.24910109063628));
#41821=CARTESIAN_POINT('Ctrl Pts',(-2.884065589809,57.495,5.23745215939571));
#41822=CARTESIAN_POINT('Ctrl Pts',(-2.884065589809,49.875,5.23745215939571));
#41823=CARTESIAN_POINT('Ctrl Pts',(-2.88043681055505,57.495,5.23024117954545));
#41824=CARTESIAN_POINT('Ctrl Pts',(-2.88043681055505,49.875,5.23024117954545));
#41825=CARTESIAN_POINT('Ctrl Pts',(-2.87862685522557,57.495,5.22677443144495));
#41826=CARTESIAN_POINT('Ctrl Pts',(-2.87862685522557,49.875,5.22677443144495));
#41827=CARTESIAN_POINT('Ctrl Pts',(-2.96056324982543,51.145,6.50167680247051));
#41828=CARTESIAN_POINT('Ctrl Pts',(-2.96229154623625,51.145,6.49043534784131));
#41829=CARTESIAN_POINT('Ctrl Pts',(-2.96566304810549,51.145,6.46801681444607));
#41830=CARTESIAN_POINT('Ctrl Pts',(-2.97046502832945,51.145,6.43458214159149));
#41831=CARTESIAN_POINT('Ctrl Pts',(-2.97635619664337,51.145,6.39038953466561));
#41832=CARTESIAN_POINT('Ctrl Pts',(-2.98286238364857,51.145,6.33579850967689));
#41833=CARTESIAN_POINT('Ctrl Pts',(-2.98850417352769,51.145,6.28186459845047));
#41834=CARTESIAN_POINT('Ctrl Pts',(-2.99327554868811,51.145,6.22859706400147));
#41835=CARTESIAN_POINT('Ctrl Pts',(-2.99717295692919,51.145,6.17600655789209));
#41836=CARTESIAN_POINT('Ctrl Pts',(-3.00019778316108,51.145,6.12410381716742));
#41837=CARTESIAN_POINT('Ctrl Pts',(-3.00235671375967,51.145,6.07290162599622));
#41838=CARTESIAN_POINT('Ctrl Pts',(-3.00366113621883,51.145,6.02241806591666));
#41839=CARTESIAN_POINT('Ctrl Pts',(-3.00412716938109,51.145,5.97267956506952));
#41840=CARTESIAN_POINT('Ctrl Pts',(-3.00377540211877,51.145,5.9237232280624));
#41841=CARTESIAN_POINT('Ctrl Pts',(-3.00263159433912,51.145,5.87560110342631));
#41842=CARTESIAN_POINT('Ctrl Pts',(-3.00072490941932,51.145,5.82837721216385));
#41843=CARTESIAN_POINT('Ctrl Pts',(-2.99808342690946,51.145,5.78211642456387));
#41844=CARTESIAN_POINT('Ctrl Pts',(-2.9947301570106,51.145,5.73687442119613));
#41845=CARTESIAN_POINT('Ctrl Pts',(-2.9906797244254,51.145,5.69268882427748));
#41846=CARTESIAN_POINT('Ctrl Pts',(-2.98593308820271,51.145,5.64956501668959));
#41847=CARTESIAN_POINT('Ctrl Pts',(-2.98047914221,51.145,5.6074788286105));
#41848=CARTESIAN_POINT('Ctrl Pts',(-2.97430877025609,51.145,5.56641026634749));
#41849=CARTESIAN_POINT('Ctrl Pts',(-2.96742703426683,51.145,5.52637191504895));
#41850=CARTESIAN_POINT('Ctrl Pts',(-2.9598647928985,51.145,5.48743586913296));
#41851=CARTESIAN_POINT('Ctrl Pts',(-2.95169462080131,51.145,5.44977003302482));
#41852=CARTESIAN_POINT('Ctrl Pts',(-2.94303247002258,51.145,5.41364129622045));
#41853=CARTESIAN_POINT('Ctrl Pts',(-2.93401523982671,51.145,5.37936310952307));
#41854=CARTESIAN_POINT('Ctrl Pts',(-2.92478335875774,51.145,5.34725389048201));
#41855=CARTESIAN_POINT('Ctrl Pts',(-2.91546314862891,51.145,5.31759510370885));
#41856=CARTESIAN_POINT('Ctrl Pts',(-2.90614521320837,51.145,5.29057828960676));
#41857=CARTESIAN_POINT('Ctrl Pts',(-2.89688168736508,51.145,5.26630084561719));
#41858=CARTESIAN_POINT('Ctrl Pts',(-2.88953536864313,51.145,5.24910109063628));
#41859=CARTESIAN_POINT('Ctrl Pts',(-2.884065589809,51.145,5.23745215939571));
#41860=CARTESIAN_POINT('Ctrl Pts',(-2.88043681055505,51.145,5.23024117954545));
#41861=CARTESIAN_POINT('Ctrl Pts',(-2.87862685522557,51.145,5.22677443144495));
#41862=CARTESIAN_POINT('Origin',(3.261,51.145,0.));
#41863=CARTESIAN_POINT('',(0.592010183030744,51.145,5.32519370006274));
#41864=CARTESIAN_POINT('Origin',(0.,51.145,0.));
#41865=CARTESIAN_POINT('',(0.659304453656788,51.145,5.93051272372135));
#41866=CARTESIAN_POINT('',(0.575436549687218,51.145,5.17611212951227));
#41867=CARTESIAN_POINT('',(0.24711979632092,51.145,7.13972463098307));
#41868=CARTESIAN_POINT('Ctrl Pts',(0.659304453656788,51.145,5.93051272372135));
#41869=CARTESIAN_POINT('Ctrl Pts',(0.659649967278236,51.145,5.9344082212537));
#41870=CARTESIAN_POINT('Ctrl Pts',(0.660242999639201,51.145,5.94245897164691));
#41871=CARTESIAN_POINT('Ctrl Pts',(0.660838563360921,51.145,5.95531437453424));
#41872=CARTESIAN_POINT('Ctrl Pts',(0.661043615595512,51.145,5.97401619058907));
#41873=CARTESIAN_POINT('Ctrl Pts',(0.660311421925997,51.145,5.99999062205823));
#41874=CARTESIAN_POINT('Ctrl Pts',(0.658581184594088,51.145,6.0285167231501));
#41875=CARTESIAN_POINT('Ctrl Pts',(0.655842009648633,51.145,6.05948455921138));
#41876=CARTESIAN_POINT('Ctrl Pts',(0.652083489461619,51.145,6.09268249742298));
#41877=CARTESIAN_POINT('Ctrl Pts',(0.64729662973892,51.145,6.12780215712604));
#41878=CARTESIAN_POINT('Ctrl Pts',(0.641473544543614,51.145,6.16449561918676));
#41879=CARTESIAN_POINT('Ctrl Pts',(0.634607707876564,51.145,6.20242090374318));
#41880=CARTESIAN_POINT('Ctrl Pts',(0.626694128202842,51.145,6.24128706412515));
#41881=CARTESIAN_POINT('Ctrl Pts',(0.617730009530307,51.145,6.2809112037544));
#41882=CARTESIAN_POINT('Ctrl Pts',(0.607714431517401,51.145,6.32121490697716));
#41883=CARTESIAN_POINT('Ctrl Pts',(0.596647533682211,51.145,6.36218460951727));
#41884=CARTESIAN_POINT('Ctrl Pts',(0.584530087032237,51.145,6.40384227175352));
#41885=CARTESIAN_POINT('Ctrl Pts',(0.571363102905579,51.145,6.44621447382266));
#41886=CARTESIAN_POINT('Ctrl Pts',(0.557147755196277,51.145,6.4892958755784));
#41887=CARTESIAN_POINT('Ctrl Pts',(0.541884929839949,51.145,6.53304612199323));
#41888=CARTESIAN_POINT('Ctrl Pts',(0.525574676214356,51.145,6.57740496530571));
#41889=CARTESIAN_POINT('Ctrl Pts',(0.508215876982668,51.145,6.62230172760513));
#41890=CARTESIAN_POINT('Ctrl Pts',(0.489806088474622,51.145,6.66766610085618));
#41891=CARTESIAN_POINT('Ctrl Pts',(0.470341429749655,51.145,6.71344014059664));
#41892=CARTESIAN_POINT('Ctrl Pts',(0.449817078488629,51.145,6.75958168761858));
#41893=CARTESIAN_POINT('Ctrl Pts',(0.428228256434473,51.145,6.80606015708966));
#41894=CARTESIAN_POINT('Ctrl Pts',(0.405571362419756,51.145,6.85285448604159));
#41895=CARTESIAN_POINT('Ctrl Pts',(0.381845111328234,51.145,6.89995030467727));
#41896=CARTESIAN_POINT('Ctrl Pts',(0.357052332559035,51.145,6.94733716327837));
#41897=CARTESIAN_POINT('Ctrl Pts',(0.331200384094009,51.145,6.99500658045299));
#41898=CARTESIAN_POINT('Ctrl Pts',(0.304298370266204,51.145,7.0429523011241));
#41899=CARTESIAN_POINT('Ctrl Pts',(0.28194386193484,51.145,7.0815264936403));
#41900=CARTESIAN_POINT('Ctrl Pts',(0.264712515322387,51.145,7.11057846529273));
#41901=CARTESIAN_POINT('Ctrl Pts',(0.253018452443275,51.145,7.13000027153808));
#41902=CARTESIAN_POINT('Ctrl Pts',(0.247119796320917,51.145,7.13972463098307));
#41903=CARTESIAN_POINT('',(-0.247119796320916,51.145,7.13972463098307));
#41904=CARTESIAN_POINT('Origin',(4.16333634234434E-16,51.145,1.6286971771251E-12));
#41905=CARTESIAN_POINT('',(-0.659304453656787,51.145,5.93051272372135));
#41906=CARTESIAN_POINT('Ctrl Pts',(-0.247119796320916,51.145,7.13972463098307));
#41907=CARTESIAN_POINT('Ctrl Pts',(-0.253018452443266,51.145,7.13000027153814));
#41908=CARTESIAN_POINT('Ctrl Pts',(-0.264712515322364,51.145,7.1105784652929));
#41909=CARTESIAN_POINT('Ctrl Pts',(-0.281943861934804,51.145,7.0815264936406));
#41910=CARTESIAN_POINT('Ctrl Pts',(-0.304298370266163,51.145,7.04295230112448));
#41911=CARTESIAN_POINT('Ctrl Pts',(-0.331200384093975,51.145,6.99500658045334));
#41912=CARTESIAN_POINT('Ctrl Pts',(-0.357052332559017,51.145,6.94733716327859));
#41913=CARTESIAN_POINT('Ctrl Pts',(-0.381845111328231,51.145,6.89995030467732));
#41914=CARTESIAN_POINT('Ctrl Pts',(-0.405571362419762,51.145,6.85285448604147));
#41915=CARTESIAN_POINT('Ctrl Pts',(-0.428228256434482,51.145,6.80606015708944));
#41916=CARTESIAN_POINT('Ctrl Pts',(-0.449817078488635,51.145,6.75958168761835));
#41917=CARTESIAN_POINT('Ctrl Pts',(-0.470341429749656,51.145,6.71344014059646));
#41918=CARTESIAN_POINT('Ctrl Pts',(-0.48980608847462,51.145,6.66766610085612));
#41919=CARTESIAN_POINT('Ctrl Pts',(-0.508215876982667,51.145,6.62230172760518));
#41920=CARTESIAN_POINT('Ctrl Pts',(-0.52557467621436,51.145,6.57740496530586));
#41921=CARTESIAN_POINT('Ctrl Pts',(-0.541884929839958,51.145,6.53304612199338));
#41922=CARTESIAN_POINT('Ctrl Pts',(-0.557147755196287,51.145,6.48929587557851));
#41923=CARTESIAN_POINT('Ctrl Pts',(-0.571363102905585,51.145,6.4462144738227));
#41924=CARTESIAN_POINT('Ctrl Pts',(-0.584530087032233,51.145,6.40384227175349));
#41925=CARTESIAN_POINT('Ctrl Pts',(-0.596647533682196,51.145,6.36218460951721));
#41926=CARTESIAN_POINT('Ctrl Pts',(-0.607714431517378,51.145,6.32121490697708));
#41927=CARTESIAN_POINT('Ctrl Pts',(-0.617730009530283,51.145,6.28091120375433));
#41928=CARTESIAN_POINT('Ctrl Pts',(-0.626694128202828,51.145,6.24128706412512));
#41929=CARTESIAN_POINT('Ctrl Pts',(-0.63460770787657,51.145,6.2024209037432));
#41930=CARTESIAN_POINT('Ctrl Pts',(-0.641473544543643,51.145,6.16449561918681));
#41931=CARTESIAN_POINT('Ctrl Pts',(-0.647296629738964,51.145,6.12780215712609));
#41932=CARTESIAN_POINT('Ctrl Pts',(-0.652083489461663,51.145,6.092682497423));
#41933=CARTESIAN_POINT('Ctrl Pts',(-0.655842009648655,51.145,6.05948455921138));
#41934=CARTESIAN_POINT('Ctrl Pts',(-0.658581184594065,51.145,6.02851672315009));
#41935=CARTESIAN_POINT('Ctrl Pts',(-0.660311421925919,51.145,5.99999062205821));
#41936=CARTESIAN_POINT('Ctrl Pts',(-0.661043615595395,51.145,5.97401619058905));
#41937=CARTESIAN_POINT('Ctrl Pts',(-0.660838563360812,51.145,5.95531437453421));
#41938=CARTESIAN_POINT('Ctrl Pts',(-0.660242999639131,51.145,5.94245897164689));
#41939=CARTESIAN_POINT('Ctrl Pts',(-0.65964996727821,51.145,5.93440822125369));
#41940=CARTESIAN_POINT('Ctrl Pts',(-0.659304453656787,51.145,5.93051272372135));
#41941=CARTESIAN_POINT('',(-0.592010183030743,51.145,5.32519370006274));
#41942=CARTESIAN_POINT('',(-0.659304453656787,51.145,5.93051272372135));
#41943=CARTESIAN_POINT('Origin',(0.,51.145,0.));
#41944=CARTESIAN_POINT('',(-3.261,51.145,-3.99357321201952E-16));
#41945=CARTESIAN_POINT('Origin',(0.,51.145,0.));
#41946=CARTESIAN_POINT('Origin',(0.,54.32,0.));
#41947=CARTESIAN_POINT('',(0.592010183030744,54.32,5.32519370006274));
#41948=CARTESIAN_POINT('Origin',(0.575436549687218,57.495,5.17611212951227));
#41949=CARTESIAN_POINT('',(0.659304453656788,57.495,5.93051272372135));
#41950=CARTESIAN_POINT('Origin',(4.16333634234434E-16,57.495,1.6286971771251E-12));
#41951=CARTESIAN_POINT('',(-0.247119796320916,57.495,7.13972463098307));
#41952=CARTESIAN_POINT('',(0.24711979632092,57.495,7.13972463098307));
#41953=CARTESIAN_POINT('Ctrl Pts',(0.659304453656788,57.495,5.93051272372135));
#41954=CARTESIAN_POINT('Ctrl Pts',(0.659304453656788,49.875,5.93051272372135));
#41955=CARTESIAN_POINT('Ctrl Pts',(0.659649967278236,57.495,5.9344082212537));
#41956=CARTESIAN_POINT('Ctrl Pts',(0.659649967278236,49.875,5.9344082212537));
#41957=CARTESIAN_POINT('Ctrl Pts',(0.660242999639201,57.495,5.94245897164691));
#41958=CARTESIAN_POINT('Ctrl Pts',(0.660242999639201,49.875,5.94245897164691));
#41959=CARTESIAN_POINT('Ctrl Pts',(0.660838563360921,57.495,5.95531437453424));
#41960=CARTESIAN_POINT('Ctrl Pts',(0.660838563360921,49.875,5.95531437453424));
#41961=CARTESIAN_POINT('Ctrl Pts',(0.661043615595512,57.495,5.97401619058907));
#41962=CARTESIAN_POINT('Ctrl Pts',(0.661043615595512,49.875,5.97401619058907));
#41963=CARTESIAN_POINT('Ctrl Pts',(0.660311421925997,57.495,5.99999062205823));
#41964=CARTESIAN_POINT('Ctrl Pts',(0.660311421925997,49.875,5.99999062205823));
#41965=CARTESIAN_POINT('Ctrl Pts',(0.658581184594088,57.495,6.0285167231501));
#41966=CARTESIAN_POINT('Ctrl Pts',(0.658581184594088,49.875,6.0285167231501));
#41967=CARTESIAN_POINT('Ctrl Pts',(0.655842009648633,57.495,6.05948455921138));
#41968=CARTESIAN_POINT('Ctrl Pts',(0.655842009648633,49.875,6.05948455921138));
#41969=CARTESIAN_POINT('Ctrl Pts',(0.652083489461619,57.495,6.09268249742298));
#41970=CARTESIAN_POINT('Ctrl Pts',(0.652083489461619,49.875,6.09268249742298));
#41971=CARTESIAN_POINT('Ctrl Pts',(0.64729662973892,57.495,6.12780215712604));
#41972=CARTESIAN_POINT('Ctrl Pts',(0.64729662973892,49.875,6.12780215712604));
#41973=CARTESIAN_POINT('Ctrl Pts',(0.641473544543614,57.495,6.16449561918676));
#41974=CARTESIAN_POINT('Ctrl Pts',(0.641473544543614,49.875,6.16449561918676));
#41975=CARTESIAN_POINT('Ctrl Pts',(0.634607707876564,57.495,6.20242090374318));
#41976=CARTESIAN_POINT('Ctrl Pts',(0.634607707876564,49.875,6.20242090374318));
#41977=CARTESIAN_POINT('Ctrl Pts',(0.626694128202842,57.495,6.24128706412515));
#41978=CARTESIAN_POINT('Ctrl Pts',(0.626694128202842,49.875,6.24128706412515));
#41979=CARTESIAN_POINT('Ctrl Pts',(0.617730009530307,57.495,6.2809112037544));
#41980=CARTESIAN_POINT('Ctrl Pts',(0.617730009530307,49.875,6.2809112037544));
#41981=CARTESIAN_POINT('Ctrl Pts',(0.607714431517401,57.495,6.32121490697716));
#41982=CARTESIAN_POINT('Ctrl Pts',(0.607714431517401,49.875,6.32121490697716));
#41983=CARTESIAN_POINT('Ctrl Pts',(0.596647533682211,57.495,6.36218460951727));
#41984=CARTESIAN_POINT('Ctrl Pts',(0.596647533682211,49.875,6.36218460951727));
#41985=CARTESIAN_POINT('Ctrl Pts',(0.584530087032237,57.495,6.40384227175352));
#41986=CARTESIAN_POINT('Ctrl Pts',(0.584530087032237,49.875,6.40384227175352));
#41987=CARTESIAN_POINT('Ctrl Pts',(0.571363102905579,57.495,6.44621447382266));
#41988=CARTESIAN_POINT('Ctrl Pts',(0.571363102905579,49.875,6.44621447382266));
#41989=CARTESIAN_POINT('Ctrl Pts',(0.557147755196277,57.495,6.4892958755784));
#41990=CARTESIAN_POINT('Ctrl Pts',(0.557147755196277,49.875,6.4892958755784));
#41991=CARTESIAN_POINT('Ctrl Pts',(0.541884929839949,57.495,6.53304612199323));
#41992=CARTESIAN_POINT('Ctrl Pts',(0.541884929839949,49.875,6.53304612199323));
#41993=CARTESIAN_POINT('Ctrl Pts',(0.525574676214356,57.495,6.57740496530571));
#41994=CARTESIAN_POINT('Ctrl Pts',(0.525574676214356,49.875,6.57740496530571));
#41995=CARTESIAN_POINT('Ctrl Pts',(0.508215876982668,57.495,6.62230172760513));
#41996=CARTESIAN_POINT('Ctrl Pts',(0.508215876982668,49.875,6.62230172760513));
#41997=CARTESIAN_POINT('Ctrl Pts',(0.489806088474622,57.495,6.66766610085618));
#41998=CARTESIAN_POINT('Ctrl Pts',(0.489806088474622,49.875,6.66766610085618));
#41999=CARTESIAN_POINT('Ctrl Pts',(0.470341429749655,57.495,6.71344014059664));
#42000=CARTESIAN_POINT('Ctrl Pts',(0.470341429749655,49.875,6.71344014059664));
#42001=CARTESIAN_POINT('Ctrl Pts',(0.449817078488629,57.495,6.75958168761858));
#42002=CARTESIAN_POINT('Ctrl Pts',(0.449817078488629,49.875,6.75958168761858));
#42003=CARTESIAN_POINT('Ctrl Pts',(0.428228256434473,57.495,6.80606015708966));
#42004=CARTESIAN_POINT('Ctrl Pts',(0.428228256434473,49.875,6.80606015708966));
#42005=CARTESIAN_POINT('Ctrl Pts',(0.405571362419756,57.495,6.85285448604159));
#42006=CARTESIAN_POINT('Ctrl Pts',(0.405571362419756,49.875,6.85285448604159));
#42007=CARTESIAN_POINT('Ctrl Pts',(0.381845111328234,57.495,6.89995030467727));
#42008=CARTESIAN_POINT('Ctrl Pts',(0.381845111328234,49.875,6.89995030467727));
#42009=CARTESIAN_POINT('Ctrl Pts',(0.357052332559035,57.495,6.94733716327837));
#42010=CARTESIAN_POINT('Ctrl Pts',(0.357052332559035,49.875,6.94733716327837));
#42011=CARTESIAN_POINT('Ctrl Pts',(0.331200384094009,57.495,6.99500658045299));
#42012=CARTESIAN_POINT('Ctrl Pts',(0.331200384094009,49.875,6.99500658045299));
#42013=CARTESIAN_POINT('Ctrl Pts',(0.304298370266204,57.495,7.0429523011241));
#42014=CARTESIAN_POINT('Ctrl Pts',(0.304298370266204,49.875,7.0429523011241));
#42015=CARTESIAN_POINT('Ctrl Pts',(0.28194386193484,57.495,7.0815264936403));
#42016=CARTESIAN_POINT('Ctrl Pts',(0.28194386193484,49.875,7.0815264936403));
#42017=CARTESIAN_POINT('Ctrl Pts',(0.264712515322387,57.495,7.11057846529273));
#42018=CARTESIAN_POINT('Ctrl Pts',(0.264712515322387,49.875,7.11057846529273));
#42019=CARTESIAN_POINT('Ctrl Pts',(0.253018452443275,57.495,7.13000027153808));
#42020=CARTESIAN_POINT('Ctrl Pts',(0.253018452443275,49.875,7.13000027153808));
#42021=CARTESIAN_POINT('Ctrl Pts',(0.247119796320917,57.495,7.13972463098307));
#42022=CARTESIAN_POINT('Ctrl Pts',(0.247119796320917,49.875,7.13972463098307));
#42023=CARTESIAN_POINT('Origin',(-0.659304453656787,57.495,5.93051272372135));
#42024=CARTESIAN_POINT('',(-0.592010183030743,54.32,5.32519370006274));
#42025=CARTESIAN_POINT('',(-0.659304453656787,57.495,5.93051272372135));
#42026=CARTESIAN_POINT('Ctrl Pts',(-0.247119796320916,57.495,7.13972463098307));
#42027=CARTESIAN_POINT('Ctrl Pts',(-0.247119796320916,49.875,7.13972463098307));
#42028=CARTESIAN_POINT('Ctrl Pts',(-0.253018452443266,57.495,7.13000027153814));
#42029=CARTESIAN_POINT('Ctrl Pts',(-0.253018452443266,49.875,7.13000027153814));
#42030=CARTESIAN_POINT('Ctrl Pts',(-0.264712515322364,57.495,7.1105784652929));
#42031=CARTESIAN_POINT('Ctrl Pts',(-0.264712515322364,49.875,7.1105784652929));
#42032=CARTESIAN_POINT('Ctrl Pts',(-0.281943861934804,57.495,7.0815264936406));
#42033=CARTESIAN_POINT('Ctrl Pts',(-0.281943861934804,49.875,7.0815264936406));
#42034=CARTESIAN_POINT('Ctrl Pts',(-0.304298370266163,57.495,7.04295230112448));
#42035=CARTESIAN_POINT('Ctrl Pts',(-0.304298370266163,49.875,7.04295230112448));
#42036=CARTESIAN_POINT('Ctrl Pts',(-0.331200384093975,57.495,6.99500658045334));
#42037=CARTESIAN_POINT('Ctrl Pts',(-0.331200384093975,49.875,6.99500658045334));
#42038=CARTESIAN_POINT('Ctrl Pts',(-0.357052332559017,57.495,6.94733716327859));
#42039=CARTESIAN_POINT('Ctrl Pts',(-0.357052332559017,49.875,6.94733716327859));
#42040=CARTESIAN_POINT('Ctrl Pts',(-0.381845111328231,57.495,6.89995030467732));
#42041=CARTESIAN_POINT('Ctrl Pts',(-0.381845111328231,49.875,6.89995030467732));
#42042=CARTESIAN_POINT('Ctrl Pts',(-0.405571362419762,57.495,6.85285448604147));
#42043=CARTESIAN_POINT('Ctrl Pts',(-0.405571362419762,49.875,6.85285448604147));
#42044=CARTESIAN_POINT('Ctrl Pts',(-0.428228256434482,57.495,6.80606015708944));
#42045=CARTESIAN_POINT('Ctrl Pts',(-0.428228256434482,49.875,6.80606015708944));
#42046=CARTESIAN_POINT('Ctrl Pts',(-0.449817078488635,57.495,6.75958168761835));
#42047=CARTESIAN_POINT('Ctrl Pts',(-0.449817078488635,49.875,6.75958168761835));
#42048=CARTESIAN_POINT('Ctrl Pts',(-0.470341429749656,57.495,6.71344014059646));
#42049=CARTESIAN_POINT('Ctrl Pts',(-0.470341429749656,49.875,6.71344014059646));
#42050=CARTESIAN_POINT('Ctrl Pts',(-0.48980608847462,57.495,6.66766610085612));
#42051=CARTESIAN_POINT('Ctrl Pts',(-0.48980608847462,49.875,6.66766610085612));
#42052=CARTESIAN_POINT('Ctrl Pts',(-0.508215876982667,57.495,6.62230172760518));
#42053=CARTESIAN_POINT('Ctrl Pts',(-0.508215876982667,49.875,6.62230172760518));
#42054=CARTESIAN_POINT('Ctrl Pts',(-0.52557467621436,57.495,6.57740496530586));
#42055=CARTESIAN_POINT('Ctrl Pts',(-0.52557467621436,49.875,6.57740496530586));
#42056=CARTESIAN_POINT('Ctrl Pts',(-0.541884929839958,57.495,6.53304612199338));
#42057=CARTESIAN_POINT('Ctrl Pts',(-0.541884929839958,49.875,6.53304612199338));
#42058=CARTESIAN_POINT('Ctrl Pts',(-0.557147755196287,57.495,6.48929587557851));
#42059=CARTESIAN_POINT('Ctrl Pts',(-0.557147755196287,49.875,6.48929587557851));
#42060=CARTESIAN_POINT('Ctrl Pts',(-0.571363102905585,57.495,6.4462144738227));
#42061=CARTESIAN_POINT('Ctrl Pts',(-0.571363102905585,49.875,6.4462144738227));
#42062=CARTESIAN_POINT('Ctrl Pts',(-0.584530087032233,57.495,6.40384227175349));
#42063=CARTESIAN_POINT('Ctrl Pts',(-0.584530087032233,49.875,6.40384227175349));
#42064=CARTESIAN_POINT('Ctrl Pts',(-0.596647533682196,57.495,6.36218460951721));
#42065=CARTESIAN_POINT('Ctrl Pts',(-0.596647533682196,49.875,6.36218460951721));
#42066=CARTESIAN_POINT('Ctrl Pts',(-0.607714431517378,57.495,6.32121490697708));
#42067=CARTESIAN_POINT('Ctrl Pts',(-0.607714431517378,49.875,6.32121490697708));
#42068=CARTESIAN_POINT('Ctrl Pts',(-0.617730009530283,57.495,6.28091120375433));
#42069=CARTESIAN_POINT('Ctrl Pts',(-0.617730009530283,49.875,6.28091120375433));
#42070=CARTESIAN_POINT('Ctrl Pts',(-0.626694128202828,57.495,6.24128706412512));
#42071=CARTESIAN_POINT('Ctrl Pts',(-0.626694128202828,49.875,6.24128706412512));
#42072=CARTESIAN_POINT('Ctrl Pts',(-0.63460770787657,57.495,6.2024209037432));
#42073=CARTESIAN_POINT('Ctrl Pts',(-0.63460770787657,49.875,6.2024209037432));
#42074=CARTESIAN_POINT('Ctrl Pts',(-0.641473544543643,57.495,6.16449561918681));
#42075=CARTESIAN_POINT('Ctrl Pts',(-0.641473544543643,49.875,6.16449561918681));
#42076=CARTESIAN_POINT('Ctrl Pts',(-0.647296629738964,57.495,6.12780215712609));
#42077=CARTESIAN_POINT('Ctrl Pts',(-0.647296629738964,49.875,6.12780215712609));
#42078=CARTESIAN_POINT('Ctrl Pts',(-0.652083489461663,57.495,6.092682497423));
#42079=CARTESIAN_POINT('Ctrl Pts',(-0.652083489461663,49.875,6.092682497423));
#42080=CARTESIAN_POINT('Ctrl Pts',(-0.655842009648655,57.495,6.05948455921138));
#42081=CARTESIAN_POINT('Ctrl Pts',(-0.655842009648655,49.875,6.05948455921138));
#42082=CARTESIAN_POINT('Ctrl Pts',(-0.658581184594065,57.495,6.02851672315009));
#42083=CARTESIAN_POINT('Ctrl Pts',(-0.658581184594065,49.875,6.02851672315009));
#42084=CARTESIAN_POINT('Ctrl Pts',(-0.660311421925919,57.495,5.99999062205821));
#42085=CARTESIAN_POINT('Ctrl Pts',(-0.660311421925919,49.875,5.99999062205821));
#42086=CARTESIAN_POINT('Ctrl Pts',(-0.661043615595395,57.495,5.97401619058905));
#42087=CARTESIAN_POINT('Ctrl Pts',(-0.661043615595395,49.875,5.97401619058905));
#42088=CARTESIAN_POINT('Ctrl Pts',(-0.660838563360812,57.495,5.95531437453421));
#42089=CARTESIAN_POINT('Ctrl Pts',(-0.660838563360812,49.875,5.95531437453421));
#42090=CARTESIAN_POINT('Ctrl Pts',(-0.660242999639131,57.495,5.94245897164689));
#42091=CARTESIAN_POINT('Ctrl Pts',(-0.660242999639131,49.875,5.94245897164689));
#42092=CARTESIAN_POINT('Ctrl Pts',(-0.65964996727821,57.495,5.93440822125369));
#42093=CARTESIAN_POINT('Ctrl Pts',(-0.65964996727821,49.875,5.93440822125369));
#42094=CARTESIAN_POINT('Ctrl Pts',(-0.659304453656787,57.495,5.93051272372135));
#42095=CARTESIAN_POINT('Ctrl Pts',(-0.659304453656787,49.875,5.93051272372135));
#42096=CARTESIAN_POINT('Origin',(0.,54.32,0.));
#42097=CARTESIAN_POINT('Origin',(1.6,53.935,0.));
#42098=CARTESIAN_POINT('',(-3.261,53.935,-3.99357321201952E-16));
#42099=CARTESIAN_POINT('Origin',(0.,53.935,0.));
#42100=CARTESIAN_POINT('',(-1.6,53.935,-1.95943487863577E-16));
#42101=CARTESIAN_POINT('Origin',(0.,53.935,0.));
#42102=CARTESIAN_POINT('Origin',(0.,54.825,0.));
#42103=CARTESIAN_POINT('',(-1.6,55.715,-1.95943487863577E-16));
#42104=CARTESIAN_POINT('Origin',(0.,55.715,0.));
#42105=CARTESIAN_POINT('',(-1.6,54.825,-1.95943487863577E-16));
#42106=CARTESIAN_POINT('Origin',(4.477,55.715,0.));
#42107=CARTESIAN_POINT('',(-4.477,55.715,-5.4827437197827E-16));
#42108=CARTESIAN_POINT('Origin',(0.,55.715,0.));
#42109=CARTESIAN_POINT('Origin',(0.,56.605,0.));
#42110=CARTESIAN_POINT('',(-4.477,56.605,-5.4827437197827E-16));
#42111=CARTESIAN_POINT('Origin',(0.,52.54,0.));
#42112=CARTESIAN_POINT('',(-3.261,52.54,-3.99357321201952E-16));
#42113=CARTESIAN_POINT('',(0.,0.,0.));
#42114=CARTESIAN_POINT('Origin',(0.,56.5393671147362,0.));
#42115=CARTESIAN_POINT('',(0.188938462403162,55.3284942881797,1.16249615910107));
#42116=CARTESIAN_POINT('',(0.188938462403162,55.4271602664287,1.16249615910107));
#42117=CARTESIAN_POINT('',(0.188938462403162,56.5393671147362,1.16249615910107));
#42118=CARTESIAN_POINT('',(-0.684640367384077,55.614964185794,-0.958312386358538));
#42119=CARTESIAN_POINT('Ctrl Pts',(-0.684640367384077,55.614964185794,-0.958312386358538));
#42120=CARTESIAN_POINT('Ctrl Pts',(-0.647016272926218,55.6118230807353,
-0.985191903120293));
#42121=CARTESIAN_POINT('Ctrl Pts',(-0.607717364810166,55.6086819756767,
-1.00991601482877));
#42122=CARTESIAN_POINT('Ctrl Pts',(-0.567023115628078,55.605540870618,-1.03226927148076));
#42123=CARTESIAN_POINT('Ctrl Pts',(-0.526385256289338,55.6024041181749,
-1.05459155332265));
#42124=CARTESIAN_POINT('Ctrl Pts',(-0.484356373687067,55.5992673657318,
-1.07454920089206));
#42125=CARTESIAN_POINT('Ctrl Pts',(-0.441245462063377,55.5961306132887,
-1.09196955301349));
#42126=CARTESIAN_POINT('Ctrl Pts',(-0.398174263826859,55.5929967503939,
-1.10937385766195));
#42127=CARTESIAN_POINT('Ctrl Pts',(-0.354023535299063,55.5898628874992,
-1.12424527627553));
#42128=CARTESIAN_POINT('Ctrl Pts',(-0.309124864566901,55.5867290246045,
-1.13645804172723));
#42129=CARTESIAN_POINT('Ctrl Pts',(-0.26424670437289,55.5835965933159,-1.14866522816317));
#42130=CARTESIAN_POINT('Ctrl Pts',(-0.218621829054994,55.5804641620274,
-1.15821601686914));
#42131=CARTESIAN_POINT('Ctrl Pts',(-0.172596925041673,55.5773317307388,
-1.16503449046205));
#42132=CARTESIAN_POINT('Ctrl Pts',(-0.12653809012124,55.5741969901302,-1.17185799083337));
#42133=CARTESIAN_POINT('Ctrl Pts',(-0.0800792025826789,55.5710622495215,
-1.17594506164065));
#42134=CARTESIAN_POINT('Ctrl Pts',(-0.0335749533691129,55.5679275089129,
-1.17727133024051));
#42135=CARTESIAN_POINT('Ctrl Pts',(0.0129453684527582,55.564791684888,-1.17859805721989));
#42136=CARTESIAN_POINT('Ctrl Pts',(0.0595105110444984,55.5616558608632,
-1.17716209426211));
#42137=CARTESIAN_POINT('Ctrl Pts',(0.105766738775078,55.5585200368383,-1.17299124441271));
#42138=CARTESIAN_POINT('Ctrl Pts',(0.152111686939792,55.5553781982359,-1.1688123947841));
#42139=CARTESIAN_POINT('Ctrl Pts',(0.198145970424446,55.5522363596335,-1.16188826620853));
#42140=CARTESIAN_POINT('Ctrl Pts',(0.243523695834775,55.5490945210311,-1.15229825655816));
#42141=CARTESIAN_POINT('Ctrl Pts',(0.278383235246138,55.5466809349469,-1.14493113279117));
#42142=CARTESIAN_POINT('Ctrl Pts',(0.312855447910416,55.5442673488626,-1.13599183356545));
#42143=CARTESIAN_POINT('Ctrl Pts',(0.346790549164388,55.5418537627784,-1.12553604007613));
#42144=CARTESIAN_POINT('Ctrl Pts',(0.393291000554971,55.5385464839361,-1.11120871824907));
#42145=CARTESIAN_POINT('Ctrl Pts',(0.439006879213796,55.5352392050939,-1.09396260540427));
#42146=CARTESIAN_POINT('Ctrl Pts',(0.483548219927332,55.5319319262516,-1.07390697060086));
#42147=CARTESIAN_POINT('Ctrl Pts',(0.526316168415577,55.5287563251382,-1.05464984132655));
#42148=CARTESIAN_POINT('Ctrl Pts',(0.568000781192846,55.5255807240248,-1.03280295445645));
#42149=CARTESIAN_POINT('Ctrl Pts',(0.608272338989886,55.5224051229114,-1.00851367076494));
#42150=CARTESIAN_POINT('Ctrl Pts',(0.648504802011408,55.5192326046044,-0.984247966595691));
#42151=CARTESIAN_POINT('Ctrl Pts',(0.687326451093157,55.5160600862973,-0.957544844920675));
#42152=CARTESIAN_POINT('Ctrl Pts',(0.724431565086706,55.5128875679902,-0.928597851605326));
#42153=CARTESIAN_POINT('Ctrl Pts',(0.761516894341772,55.5097167412948,-0.899666293054378));
#42154=CARTESIAN_POINT('Ctrl Pts',(0.796887063896899,55.5065459145994,-0.868493574724687));
#42155=CARTESIAN_POINT('Ctrl Pts',(0.830267046673704,55.5033750879041,-0.835315325914547));
#42156=CARTESIAN_POINT('Ctrl Pts',(0.863643835958174,55.5002045645645,-0.802140251296675));
#42157=CARTESIAN_POINT('Ctrl Pts',(0.895030423834373,55.4970340412249,-0.766960420664583));
#42158=CARTESIAN_POINT('Ctrl Pts',(0.924188459928365,55.4938635178853,-0.730048459374607));
#42159=CARTESIAN_POINT('Ctrl Pts',(0.95337682602575,55.4906896965875,-0.693098102497646));
#42160=CARTESIAN_POINT('Ctrl Pts',(0.98033167090894,55.4875158752897,-0.65441245809238));
#42161=CARTESIAN_POINT('Ctrl Pts',(1.0048560484622,55.484342053992,-0.614295844336366));
#42162=CARTESIAN_POINT('Ctrl Pts',(1.02939562062652,55.4811662662842,-0.574154375460518));
#42163=CARTESIAN_POINT('Ctrl Pts',(1.05150146772164,55.4779904785765,-0.532580664218136));
#42164=CARTESIAN_POINT('Ctrl Pts',(1.07102278465128,55.4748146908688,-0.489903314193535));
#42165=CARTESIAN_POINT('Ctrl Pts',(1.09057979993358,55.4716330956435,-0.447147920710251));
#42166=CARTESIAN_POINT('Ctrl Pts',(1.10754265868973,55.4684515004183,-0.403285381548701));
#42167=CARTESIAN_POINT('Ctrl Pts',(1.12180949365165,55.4652699051931,-0.358662128545834));
#42168=CARTESIAN_POINT('Ctrl Pts',(1.12598102546066,55.4643396269835,-0.345614573161628));
#42169=CARTESIAN_POINT('Ctrl Pts',(1.12992239508094,55.4634093487738,-0.332502056502935));
#42170=CARTESIAN_POINT('Ctrl Pts',(1.13363188304037,55.4624790705642,-0.319333393578473));
#42171=CARTESIAN_POINT('Ctrl Pts',(1.14681967021722,55.459171791722,-0.272516817827044));
#42172=CARTESIAN_POINT('Ctrl Pts',(1.15713407792882,55.4558645128797,-0.224769515073597));
#42173=CARTESIAN_POINT('Ctrl Pts',(1.16445277277936,55.4525572340374,-0.176478900910198));
#42174=CARTESIAN_POINT('Ctrl Pts',(1.17145972512115,55.4493908299583,-0.130245243282809));
#42175=CARTESIAN_POINT('Ctrl Pts',(1.17572092205889,55.4462244258792,-0.0835142477685342));
#42176=CARTESIAN_POINT('Ctrl Pts',(1.17717990049274,55.4430580218,-0.036640747480296));
#42177=CARTESIAN_POINT('Ctrl Pts',(1.17863739219239,55.439894844363,0.0101849875812261));
#42178=CARTESIAN_POINT('Ctrl Pts',(1.17729829867796,55.4367316669259,0.0571523830733597));
#42179=CARTESIAN_POINT('Ctrl Pts',(1.17315794086361,55.4335684894889,0.103901435450357));
#42180=CARTESIAN_POINT('Ctrl Pts',(1.1690199609782,55.4304071287574,0.150623638475473));
#42181=CARTESIAN_POINT('Ctrl Pts',(1.16208395236843,55.4272457680259,0.197127190023575));
#42182=CARTESIAN_POINT('Ctrl Pts',(1.1523972490899,55.4240844072944,0.243054814373266));
#42183=CARTESIAN_POINT('Ctrl Pts',(1.14271180180873,55.4209234564713,0.288976483655171));
#42184=CARTESIAN_POINT('Ctrl Pts',(1.13027648513076,55.4177625056482,0.33432182682512));
#42185=CARTESIAN_POINT('Ctrl Pts',(1.11518964427477,55.4146015548251,0.378744135007149));
#42186=CARTESIAN_POINT('Ctrl Pts',(1.10008747635315,55.41143739272,0.423211572824966));
#42187=CARTESIAN_POINT('Ctrl Pts',(1.08232859089022,55.4082732306148,0.466753573942334));
#42188=CARTESIAN_POINT('Ctrl Pts',(1.06206046209759,55.4051090685097,0.509040899485549));
#42189=CARTESIAN_POINT('Ctrl Pts',(1.04178013088903,55.4019430014225,0.551353684090131));
#42190=CARTESIAN_POINT('Ctrl Pts',(1.01898782249414,55.3987769343353,0.592409800546224));
#42191=CARTESIAN_POINT('Ctrl Pts',(0.993876485028458,55.3956108672481,0.631905526963863));
#42192=CARTESIAN_POINT('Ctrl Pts',(0.968719019986005,55.3924389843415,0.671473803963676));
#42193=CARTESIAN_POINT('Ctrl Pts',(0.941234358404224,55.3892671014349,0.709475521691732));
#42194=CARTESIAN_POINT('Ctrl Pts',(0.911657005503707,55.3860952185284,0.745638361953041));
#42195=CARTESIAN_POINT('Ctrl Pts',(0.902360620356654,55.3850982718023,0.757004615458256));
#42196=CARTESIAN_POINT('Ctrl Pts',(0.892857777331687,55.3841013250762,0.768189478144198));
#42197=CARTESIAN_POINT('Ctrl Pts',(0.883156488284739,55.3831043783501,0.779185266609019));
#42198=CARTESIAN_POINT('Ctrl Pts',(0.852248865205178,55.3799281763535,0.814217073587308));
#42199=CARTESIAN_POINT('Ctrl Pts',(0.819184199229053,55.3767519743569,0.847485712092019));
#42200=CARTESIAN_POINT('Ctrl Pts',(0.784191415269272,55.3735757723602,0.878714337380457));
#42201=CARTESIAN_POINT('Ctrl Pts',(0.74925332271959,55.3704045345576,0.909894154390182));
#42202=CARTESIAN_POINT('Ctrl Pts',(0.712393490439458,55.3672332967549,0.939039901289795));
#42203=CARTESIAN_POINT('Ctrl Pts',(0.673879087458413,55.3640620589522,0.965909953352908));
#42204=CARTESIAN_POINT('Ctrl Pts',(0.635404732883913,55.3608941186957,0.992752065147301));
#42205=CARTESIAN_POINT('Ctrl Pts',(0.595279668954922,55.3577261784391,1.01732284814064));
#42206=CARTESIAN_POINT('Ctrl Pts',(0.553803662632633,55.3545582381826,1.03942126481744));
#42207=CARTESIAN_POINT('Ctrl Pts',(0.512354162410747,55.3513923224638,1.06150555904361));
#42208=CARTESIAN_POINT('Ctrl Pts',(0.469555923238035,55.3482264067451,1.08112035744595));
#42209=CARTESIAN_POINT('Ctrl Pts',(0.425734792304054,55.3450604910264,1.09810971634069));
#42210=CARTESIAN_POINT('Ctrl Pts',(0.381901834291521,55.3418937208446,1.11510366056852));
#42211=CARTESIAN_POINT('Ctrl Pts',(0.337045950356933,55.3387269506629,1.12947053881549));
#42212=CARTESIAN_POINT('Ctrl Pts',(0.291512454949672,55.3355601804812,1.14110277850385));
#42213=CARTESIAN_POINT('Ctrl Pts',(0.25764674359953,55.3332048830474,1.1497543012591));
#42214=CARTESIAN_POINT('Ctrl Pts',(0.223406641651077,55.3308495856135,1.15689410636484));
#42215=CARTESIAN_POINT('Ctrl Pts',(0.188938462403162,55.3284942881797,1.16249615910107));
#42216=CARTESIAN_POINT('',(0.68466442453933,55.615,-0.95829519891849));
#42217=CARTESIAN_POINT('Origin',(0.,55.615,0.));
#42218=CARTESIAN_POINT('Ctrl Pts',(0.684664424539327,55.615,-0.958295198918492));
#42219=CARTESIAN_POINT('Ctrl Pts',(0.724491644158765,55.6116927211578,-0.929840208814693));
#42220=CARTESIAN_POINT('Ctrl Pts',(0.762577693494652,55.6083854423155,-0.898873238001395));
#42221=CARTESIAN_POINT('Ctrl Pts',(0.798605536024659,55.6050781634733,-0.865635177387546));
#42222=CARTESIAN_POINT('Ctrl Pts',(0.833972646537794,55.6018315384161,-0.83300668563167));
#42223=CARTESIAN_POINT('Ctrl Pts',(0.867356039942348,55.598584913359,-0.798190103847066));
#42224=CARTESIAN_POINT('Ctrl Pts',(0.898489640855875,55.5953382883019,-0.761453496790632));
#42225=CARTESIAN_POINT('Ctrl Pts',(0.929615873800169,55.5920924315797,-0.724725583691292));
#42226=CARTESIAN_POINT('Ctrl Pts',(0.958493033710041,55.5888465748576,-0.68607894503007));
#42227=CARTESIAN_POINT('Ctrl Pts',(0.984894406991033,55.5856007181354,-0.645815817069992));
#42228=CARTESIAN_POINT('Ctrl Pts',(1.01129880611503,55.5823544894078,-0.605548074580864));
#42229=CARTESIAN_POINT('Ctrl Pts',(1.03522657059234,55.5791082606803,-0.563663912248202));
#42230=CARTESIAN_POINT('Ctrl Pts',(1.05649480049989,55.5758620319527,-0.520493803053117));
#42231=CARTESIAN_POINT('Ctrl Pts',(1.07846295627206,55.5725089716055,-0.475902989072758));
#42232=CARTESIAN_POINT('Ctrl Pts',(1.0975931380115,55.5691559112582,-0.429940607285958));
#42233=CARTESIAN_POINT('Ctrl Pts',(1.11373706389611,55.565802850911,-0.382994536519876));
#42234=CARTESIAN_POINT('Ctrl Pts',(1.12939933028093,55.5625498302555,-0.337449117684684));
#42235=CARTESIAN_POINT('Ctrl Pts',(1.1422510072811,55.5592968096001,-0.290978437028156));
#42236=CARTESIAN_POINT('Ctrl Pts',(1.15220793960971,55.5560437889446,-0.243950663865372));
#42237=CARTESIAN_POINT('Ctrl Pts',(1.16262417817091,55.5526407087515,-0.194753532851553));
#42238=CARTESIAN_POINT('Ctrl Pts',(1.16987195765063,55.5492376285584,-0.14494728700097));
#42239=CARTESIAN_POINT('Ctrl Pts',(1.17391550254619,55.5458345483652,-0.0949602831805714));
#42240=CARTESIAN_POINT('Ctrl Pts',(1.17795904744174,55.5424314681721,-0.044973279360173));
#42241=CARTESIAN_POINT('Ctrl Pts',(1.17879841864133,55.539028387979,0.00519383608882129));
#42242=CARTESIAN_POINT('Ctrl Pts',(1.17645967332693,55.5356253077858,0.0551153294056635));
#42243=CARTESIAN_POINT('Ctrl Pts',(1.1741867668843,55.5323180289436,0.103631464568754));
#42244=CARTESIAN_POINT('Ctrl Pts',(1.16890102684614,55.5290107501013,0.152144359487931));
#42245=CARTESIAN_POINT('Ctrl Pts',(1.16060215900468,55.5257034712591,0.200244078598303));
#42246=CARTESIAN_POINT('Ctrl Pts',(1.15272296429482,55.5225634412627,0.245911398478554));
#42247=CARTESIAN_POINT('Ctrl Pts',(1.14212813743633,55.5194234112664,0.291205668470788));
#42248=CARTESIAN_POINT('Ctrl Pts',(1.12887062961706,55.51628338127,0.335776955862037));
#42249=CARTESIAN_POINT('Ctrl Pts',(1.1156282331403,55.5131469303829,0.38029743943716));
#42250=CARTESIAN_POINT('Ctrl Pts',(1.09972931778738,55.5100104794958,0.424096026327618));
#42251=CARTESIAN_POINT('Ctrl Pts',(1.08127775043472,55.5068740286087,0.466833470216989));
#42252=CARTESIAN_POINT('Ctrl Pts',(1.06283867095998,55.5037397004473,0.50954198973522));
#42253=CARTESIAN_POINT('Ctrl Pts',(1.04185058337518,55.5006053722858,0.551190264866365));
#42254=CARTESIAN_POINT('Ctrl Pts',(1.0184660634825,55.4974710441244,0.591457471027685));
#42255=CARTESIAN_POINT('Ctrl Pts',(0.995086543685758,55.4943373861474,0.631716067224168));
#42256=CARTESIAN_POINT('Ctrl Pts',(0.969311894910547,55.4912037281704,0.670593687699813));
#42257=CARTESIAN_POINT('Ctrl Pts',(0.941339996565052,55.4880700701934,0.707795219937878));
#42258=CARTESIAN_POINT('Ctrl Pts',(0.913341175156714,55.4849333960583,0.745032558797928));
#42259=CARTESIAN_POINT('Ctrl Pts',(0.883141227727676,55.4817967219231,0.780590133779324));
#42260=CARTESIAN_POINT('Ctrl Pts',(0.850979345249718,55.4786600477879,0.814204652687739));
#42261=CARTESIAN_POINT('Ctrl Pts',(0.818799488802416,55.475521620693,0.847837957384976));
#42262=CARTESIAN_POINT('Ctrl Pts',(0.784655935250263,55.4723831935981,0.879525658594153));
#42263=CARTESIAN_POINT('Ctrl Pts',(0.748823119591442,55.4692447665031,0.909042902213829));
#42264=CARTESIAN_POINT('Ctrl Pts',(0.712923282008741,55.4661004692744,0.938615355071704));
#42265=CARTESIAN_POINT('Ctrl Pts',(0.675328343043641,55.4629561720457,0.96600892074501));
#42266=CARTESIAN_POINT('Ctrl Pts',(0.636342349023049,55.459811874817,0.991041612314956));
#42267=CARTESIAN_POINT('Ctrl Pts',(0.621623720179923,55.4586247884019,1.00049236265283));
#42268=CARTESIAN_POINT('Ctrl Pts',(0.60670706636262,55.4574377019868,1.00960708054128));
#42269=CARTESIAN_POINT('Ctrl Pts',(0.591609558792355,55.4562506155717,1.01837772581961));
#42270=CARTESIAN_POINT('Ctrl Pts',(0.551182570661861,55.4530719234471,1.0418631104709));
#42271=CARTESIAN_POINT('Ctrl Pts',(0.509264752294662,55.4498932313226,1.06298989543228));
#42272=CARTESIAN_POINT('Ctrl Pts',(0.466161294741415,55.446714539198,1.08156770929286));
#42273=CARTESIAN_POINT('Ctrl Pts',(0.421968236020381,55.4434554937365,1.10061514691047));
#42274=CARTESIAN_POINT('Ctrl Pts',(0.376529229329588,55.4401964482749,1.11698257955201));
#42275=CARTESIAN_POINT('Ctrl Pts',(0.330202278749991,55.4369374028134,1.13051382902126));
#42276=CARTESIAN_POINT('Ctrl Pts',(0.283875328170395,55.4336783573518,1.14404507849051));
#42277=CARTESIAN_POINT('Ctrl Pts',(0.236661020821678,55.4304193118903,1.15473989535864));
#42278=CARTESIAN_POINT('Ctrl Pts',(0.188938462403162,55.4271602664287,1.16249615910107));
#42279=CARTESIAN_POINT('Origin',(0.,56.5393671147362,0.));
#42280=CARTESIAN_POINT('',(0.189250941525368,54.8284605668479,1.16440479426641));
#42281=CARTESIAN_POINT('',(0.188938369713633,54.9278857931129,1.16249617416573));
#42282=CARTESIAN_POINT('',(0.188938462403162,56.5393671147362,1.16249615910107));
#42283=CARTESIAN_POINT('',(-1.17764273048215,55.1906328852639,0.000476299562157373));
#42284=CARTESIAN_POINT('Ctrl Pts',(-1.17600680867674,55.1906328852639,0.000475637910860929));
#42285=CARTESIAN_POINT('Ctrl Pts',(-1.17519815942166,55.1754153574118,-0.225531174543087));
#42286=CARTESIAN_POINT('Ctrl Pts',(-1.00351486996816,55.1337395988216,-0.845634366230089));
#42287=CARTESIAN_POINT('Ctrl Pts',(0.000480427458435629,55.0656056094933,
-1.39199102275273));
#42288=CARTESIAN_POINT('Ctrl Pts',(1.16966281939467,54.9862309172792,-0.7546848720392));
#42289=CARTESIAN_POINT('Ctrl Pts',(1.26807427992724,54.9071825697306,0.567794313718899));
#42290=CARTESIAN_POINT('Ctrl Pts',(0.5691936499357,54.8545924529201,1.10219607268075));
#42291=CARTESIAN_POINT('Ctrl Pts',(0.189250941523835,54.8284605668477,1.16440479426666));
#42292=CARTESIAN_POINT('Ctrl Pts',(0.188938462403162,55.3284942881797,1.16249615910107));
#42293=CARTESIAN_POINT('Ctrl Pts',(0.142549417821131,55.3253244080164,1.17003568917784));
#42294=CARTESIAN_POINT('Ctrl Pts',(0.095747458468686,55.3221545278532,1.1747878985975));
#42295=CARTESIAN_POINT('Ctrl Pts',(0.0488931096339062,55.3189846476899,
1.17673468816481));
#42296=CARTESIAN_POINT('Ctrl Pts',(0.00194900551908925,55.3158086952305,
1.17868520704747));
#42297=CARTESIAN_POINT('Ctrl Pts',(-0.0450471295304053,55.312632742771,
1.17781958621838));
#42298=CARTESIAN_POINT('Ctrl Pts',(-0.091736027286698,55.3094567903116,
1.17417186297307));
#42299=CARTESIAN_POINT('Ctrl Pts',(-0.119800278322794,55.3075477555864,
1.17197925132906));
#42300=CARTESIAN_POINT('Ctrl Pts',(-0.147753625345882,55.3056387208611,
1.16878244602835));
#42301=CARTESIAN_POINT('Ctrl Pts',(-0.175519889908964,55.3037296861359,
1.16459771197884));
#42302=CARTESIAN_POINT('Ctrl Pts',(-0.223623142355883,55.3004224072937,
1.15734793165822));
#42303=CARTESIAN_POINT('Ctrl Pts',(-0.271388793313158,55.2971151284514,
1.14709587817919));
#42304=CARTESIAN_POINT('Ctrl Pts',(-0.318414151538062,55.2938078496091,
1.1338904226601));
#42305=CARTESIAN_POINT('Ctrl Pts',(-0.363498247483417,55.2906370991402,
1.12123010392787));
#42306=CARTESIAN_POINT('Ctrl Pts',(-0.407901374096596,55.2874663486713,
1.10585562577166));
#42307=CARTESIAN_POINT('Ctrl Pts',(-0.451276259215418,55.2842955982024,
1.08786249147975));
#42308=CARTESIAN_POINT('Ctrl Pts',(-0.49460777251013,55.2811280182602,1.06988734905235));
#42309=CARTESIAN_POINT('Ctrl Pts',(-0.536912565939944,55.277960438318,1.04929894564495));
#42310=CARTESIAN_POINT('Ctrl Pts',(-0.577860079704023,55.2747928583758,
1.02624207221516));
#42311=CARTESIAN_POINT('Ctrl Pts',(-0.618784722772805,55.2716270476437,
1.00319807689879));
#42312=CARTESIAN_POINT('Ctrl Pts',(-0.658353102238453,55.2684612369116,
0.977688615881606));
#42313=CARTESIAN_POINT('Ctrl Pts',(-0.696258635227587,55.2652954261795,
0.949904719101352));
#42314=CARTESIAN_POINT('Ctrl Pts',(-0.734159726669883,55.2621299863984,
0.922124077874288));
#42315=CARTESIAN_POINT('Ctrl Pts',(-0.770397909701557,55.2589645466174,
0.892069861365488));
#42316=CARTESIAN_POINT('Ctrl Pts',(-0.804697283430426,55.2557991068363,
0.859975199956192));
#42317=CARTESIAN_POINT('Ctrl Pts',(-0.839031720245098,55.2526304311336,
0.82784772926368));
#42318=CARTESIAN_POINT('Ctrl Pts',(-0.871422985776287,55.2494617554309,
0.79367603466084));
#42319=CARTESIAN_POINT('Ctrl Pts',(-0.901631355149056,55.2462930797282,
0.757730797785122));
#42320=CARTESIAN_POINT('Ctrl Pts',(-0.931858072785087,55.2431224794033,
0.72176372812985));
#42321=CARTESIAN_POINT('Ctrl Pts',(-0.959898923042567,55.2399518790785,
0.684021420872171));
#42322=CARTESIAN_POINT('Ctrl Pts',(-0.985556165895788,55.2367812787536,
0.644805479477954));
#42323=CARTESIAN_POINT('Ctrl Pts',(-1.01126033365124,55.233604879672,0.605517815481799));
#42324=CARTESIAN_POINT('Ctrl Pts',(-1.03457192321865,55.2304284805904,0.564751626343542));
#42325=CARTESIAN_POINT('Ctrl Pts',(-1.05533892193599,55.2272520815088,0.522833455650063));
#42326=CARTESIAN_POINT('Ctrl Pts',(-1.06165255074023,55.2262863856465,0.510089400839168));
#42327=CARTESIAN_POINT('Ctrl Pts',(-1.06773132417528,55.2253206897841,0.497239002137502));
#42328=CARTESIAN_POINT('Ctrl Pts',(-1.07357187213201,55.2243549939217,0.48429174870833));
#42329=CARTESIAN_POINT('Ctrl Pts',(-1.09455578960903,55.2208854423601,0.43777486373032));
#42330=CARTESIAN_POINT('Ctrl Pts',(-1.11254274872739,55.2174158907984,0.389825311477729));
#42331=CARTESIAN_POINT('Ctrl Pts',(-1.12735565804714,55.2139463392368,0.34082881739827));
#42332=CARTESIAN_POINT('Ctrl Pts',(-1.14212128857713,55.2104878615429,0.291988706841628));
#42333=CARTESIAN_POINT('Ctrl Pts',(-1.15373290134083,55.2070293838491,0.242108664695996));
#42334=CARTESIAN_POINT('Ctrl Pts',(-1.16206153173208,55.2035709061552,0.191593473188655));
#42335=CARTESIAN_POINT('Ctrl Pts',(-1.17035053482328,55.2001288837639,0.141318631001286));
#42336=CARTESIAN_POINT('Ctrl Pts',(-1.17538757117384,55.1966868613726,0.090415031031693));
#42337=CARTESIAN_POINT('Ctrl Pts',(-1.17709415451836,55.1932448389814,0.0392990317781458));
#42338=CARTESIAN_POINT('Ctrl Pts',(-1.1775258306479,55.1923741877422,0.0263693633936804));
#42339=CARTESIAN_POINT('Ctrl Pts',(-1.1777446660894,55.1915035365031,0.0134261765406657));
#42340=CARTESIAN_POINT('Ctrl Pts',(-1.17774990367116,55.1906328852639,0.000476342908532011));
#42341=CARTESIAN_POINT('',(-1.17774976291499,55.2893671147362,0.000747297585740462));
#42342=CARTESIAN_POINT('Ctrl Pts',(0.188938462403162,55.4271602664287,1.16249615910107));
#42343=CARTESIAN_POINT('Ctrl Pts',(0.142543930805798,55.4239919139209,1.17003658097282));
#42344=CARTESIAN_POINT('Ctrl Pts',(0.0956696598006374,55.4208235614131,
1.17479983966314));
#42345=CARTESIAN_POINT('Ctrl Pts',(0.0486749169602797,55.4176552089053,
1.17674373376658));
#42346=CARTESIAN_POINT('Ctrl Pts',(0.00168609975638459,55.4144872558998,
1.17868738276154));
#42347=CARTESIAN_POINT('Ctrl Pts',(-0.0454226027776017,55.4113193028942,
1.17781235185769));
#42348=CARTESIAN_POINT('Ctrl Pts',(-0.0922896021824091,55.4081513498887,
1.17412848182344));
#42349=CARTESIAN_POINT('Ctrl Pts',(-0.139203317783593,55.4049802391236,
1.17044093977267));
#42350=CARTESIAN_POINT('Ctrl Pts',(-0.185874293392765,55.4018091283585,
1.16393901702968));
#42351=CARTESIAN_POINT('Ctrl Pts',(-0.231945751086216,55.3986380175934,
1.15468447250885));
#42352=CARTESIAN_POINT('Ctrl Pts',(-0.278044691572742,55.3954650151803,
1.14542440741748));
#42353=CARTESIAN_POINT('Ctrl Pts',(-0.32354286360166,55.3922920127672,1.13340859486404));
#42354=CARTESIAN_POINT('Ctrl Pts',(-0.368096945434806,55.3891190103542,
1.11874916816128));
#42355=CARTESIAN_POINT('Ctrl Pts',(-0.412730857375361,55.3859403226904,
1.10406347532173));
#42356=CARTESIAN_POINT('Ctrl Pts',(-0.456416788340362,55.3827616350266,
1.08672492693345));
#42357=CARTESIAN_POINT('Ctrl Pts',(-0.498831540903763,55.3795829473629,
1.06689369493852));
#42358=CARTESIAN_POINT('Ctrl Pts',(-0.510871913694729,55.3786806060277,
1.06126415776826));
#42359=CARTESIAN_POINT('Ctrl Pts',(-0.522810011508585,55.3777782646926,
1.05543403075502));
#42360=CARTESIAN_POINT('Ctrl Pts',(-0.534638847254805,55.3768759233575,
1.04940762599957));
#42361=CARTESIAN_POINT('Ctrl Pts',(-0.577994123876299,55.3735686445152,
1.02731953121062));
#42362=CARTESIAN_POINT('Ctrl Pts',(-0.620075992746351,55.3702613656729,
1.0024903915763));
#42363=CARTESIAN_POINT('Ctrl Pts',(-0.660518998568138,55.3669540868307,
0.975094721055623));
#42364=CARTESIAN_POINT('Ctrl Pts',(-0.699351774441889,55.3637784866144,
0.948789803514913));
#42365=CARTESIAN_POINT('Ctrl Pts',(-0.736673220398442,55.3606028863982,
0.920119228874442));
#42366=CARTESIAN_POINT('Ctrl Pts',(-0.772183766357654,55.357427286182,0.889284708894574));
#42367=CARTESIAN_POINT('Ctrl Pts',(-0.807659839148315,55.3542547687964,
0.858480122659056));
#42368=CARTESIAN_POINT('Ctrl Pts',(-0.841328073571308,55.3510822514109,
0.825516112446977));
#42369=CARTESIAN_POINT('Ctrl Pts',(-0.872920461126642,55.3479097340253,
0.790635776477672));
#42370=CARTESIAN_POINT('Ctrl Pts',(-0.904496003142526,55.3447389082741,
0.755774039231701));
#42371=CARTESIAN_POINT('Ctrl Pts',(-0.933997518313652,55.3415680825229,
0.718998412134455));
#42372=CARTESIAN_POINT('Ctrl Pts',(-0.961194453248968,55.3383972567717,
0.680588190863916));
#42373=CARTESIAN_POINT('Ctrl Pts',(-0.988388786049864,55.3352267343971,
0.642181644586867));
#42374=CARTESIAN_POINT('Ctrl Pts',(-1.0132786570209,55.3320562120225,0.602141269663834));
#42375=CARTESIAN_POINT('Ctrl Pts',(-1.03567598964635,55.3288856896479,0.560776521414766));
#42376=CARTESIAN_POINT('Ctrl Pts',(-1.05809661967185,55.3257118693392,0.519368746118527));
#42377=CARTESIAN_POINT('Ctrl Pts',(-1.07801927427464,55.3225380490305,0.476634339451388));
#42378=CARTESIAN_POINT('Ctrl Pts',(-1.09530210207445,55.3193642287217,0.432906881085622));
#42379=CARTESIAN_POINT('Ctrl Pts',(-1.11259563774696,55.3161884420181,0.38915233062226));
#42380=CARTESIAN_POINT('Ctrl Pts',(-1.12724591887537,55.3130126553145,0.344404032875954));
#42381=CARTESIAN_POINT('Ctrl Pts',(-1.13916071576251,55.3098368686109,0.299011581988799));
#42382=CARTESIAN_POINT('Ctrl Pts',(-1.15109730102877,55.3066552744022,0.253536122726543));
#42383=CARTESIAN_POINT('Ctrl Pts',(-1.16028831698053,55.3034736801934,0.2074147058952));
#42384=CARTESIAN_POINT('Ctrl Pts',(-1.16669280385812,55.3002920859846,0.161006099032543));
#42385=CARTESIAN_POINT('Ctrl Pts',(-1.16856544925066,55.2993618010375,0.147436414922553));
#42386=CARTESIAN_POINT('Ctrl Pts',(-1.17020019917895,55.2984315160904,0.133842194630304));
#42387=CARTESIAN_POINT('Ctrl Pts',(-1.17159687104713,55.2975012311433,0.120232417644254));
#42388=CARTESIAN_POINT('Ctrl Pts',(-1.17566755626888,55.2947898590076,0.0805658937377747));
#42389=CARTESIAN_POINT('Ctrl Pts',(-1.17772442049394,55.2920784868719,0.0406872504911861));
#42390=CARTESIAN_POINT('Ctrl Pts',(-1.17774976291499,55.2893671147362,0.000747297585740462));
#42391=CARTESIAN_POINT('Ctrl Pts',(-1.17774972874626,55.2885481328136,0.000799336045316526));
#42392=CARTESIAN_POINT('Ctrl Pts',(-1.17778530487014,55.2852174150181,-0.051618880917269));
#42393=CARTESIAN_POINT('Ctrl Pts',(-1.17432137139241,55.2819926037606,-0.10398580942958));
#42394=CARTESIAN_POINT('Ctrl Pts',(-1.1587786970635,55.2747462179935,-0.220330615351294));
#42395=CARTESIAN_POINT('Ctrl Pts',(-1.14486848757003,55.2707271841678,-0.283881467269182));
#42396=CARTESIAN_POINT('Ctrl Pts',(-1.11931942068765,55.265134021753,-0.367021293189932));
#42397=CARTESIAN_POINT('Ctrl Pts',(-1.11225733971495,55.2637009571437,-0.38789702920972));
#42398=CARTESIAN_POINT('Ctrl Pts',(-1.10054657903341,55.2614760122246,-0.41955903527872));
#42399=CARTESIAN_POINT('Ctrl Pts',(-1.09631501846142,55.2606979448457,-0.430494971257066));
#42400=CARTESIAN_POINT('Ctrl Pts',(-1.08819702403083,55.2592502692773,-0.450578568722361));
#42401=CARTESIAN_POINT('Ctrl Pts',(-1.08435669222204,55.2585822762506,-0.45974380169608));
#42402=CARTESIAN_POINT('Ctrl Pts',(-1.07557087268419,55.2570897808557,-0.479989132667856));
#42403=CARTESIAN_POINT('Ctrl Pts',(-1.0705692668619,55.2562634068242,-0.491043475727912));
#42404=CARTESIAN_POINT('Ctrl Pts',(-1.05541525070416,55.2538245170324,-0.523203777585702));
#42405=CARTESIAN_POINT('Ctrl Pts',(-1.04480354524958,55.2521963460117,-0.544085434046534));
#42406=CARTESIAN_POINT('Ctrl Pts',(-0.98770991405417,55.2438129378895,-0.648596489679292));
#42407=CARTESIAN_POINT('Ctrl Pts',(-0.931787961229544,55.2367288952388,
-0.726645559822832));
#42408=CARTESIAN_POINT('Ctrl Pts',(-0.847041755646844,55.2275602474045,
-0.818834730872675));
#42409=CARTESIAN_POINT('Ctrl Pts',(-0.826208375415139,55.2254089250753,
-0.839851167168879));
#42410=CARTESIAN_POINT('Ctrl Pts',(-0.790816708665306,55.221944009966,-0.872960755202389));
#42411=CARTESIAN_POINT('Ctrl Pts',(-0.776719694477919,55.2206094571155,
-0.885527052501541));
#42412=CARTESIAN_POINT('Ctrl Pts',(-0.756441480146934,55.2187597522089,
-0.902746331614095));
#42413=CARTESIAN_POINT('Ctrl Pts',(-0.75050809089568,55.2182266690644,-0.90768511383862));
#42414=CARTESIAN_POINT('Ctrl Pts',(-0.740134558982428,55.2173092992901,
-0.916148472535086));
#42415=CARTESIAN_POINT('Ctrl Pts',(-0.735716919748619,55.2169231761976,
-0.919699846616618));
#42416=CARTESIAN_POINT('Ctrl Pts',(-0.725993337747847,55.2160832438266,
-0.927401805320577));
#42417=CARTESIAN_POINT('Ctrl Pts',(-0.720677221317361,55.21563034924,-0.931538932736155));
#42418=CARTESIAN_POINT('Ctrl Pts',(-0.705256120349612,55.2143337065174,
-0.943328963369739));
#42419=CARTESIAN_POINT('Ctrl Pts',(-0.695062371261651,55.2134974906239,
-0.950864901207265));
#42420=CARTESIAN_POINT('Ctrl Pts',(-0.636008765151356,55.2087587667034,
-0.993064213690707));
#42421=CARTESIAN_POINT('Ctrl Pts',(-0.584676757987412,55.205043857207,-1.02412814811633));
#42422=CARTESIAN_POINT('Ctrl Pts',(-0.479610441148176,55.1977680151588,
-1.07722320166086));
#42423=CARTESIAN_POINT('Ctrl Pts',(-0.426176031116877,55.1942151416033,
-1.09945875934819));
#42424=CARTESIAN_POINT('Ctrl Pts',(-0.338318494431742,55.1883644377274,
-1.12864762459242));
#42425=CARTESIAN_POINT('Ctrl Pts',(-0.304843402711826,55.1861342775744,
-1.13814542969933));
#42426=CARTESIAN_POINT('Ctrl Pts',(-0.257511752177355,55.1829498565127,
-1.1493366977338));
#42427=CARTESIAN_POINT('Ctrl Pts',(-0.243969430545393,55.1820353480674,
-1.15228730680109));
#42428=CARTESIAN_POINT('Ctrl Pts',(-0.220380934470313,55.1804349118546,
-1.1569923237817));
#42429=CARTESIAN_POINT('Ctrl Pts',(-0.210358025114565,55.1797525465398,
-1.15885654144547));
#42430=CARTESIAN_POINT('Ctrl Pts',(-0.189567257571492,55.1783316803772,
-1.16244493020561));
#42431=CARTESIAN_POINT('Ctrl Pts',(-0.178797164414031,55.1775926492275,
-1.16415012818113));
#42432=CARTESIAN_POINT('Ctrl Pts',(-0.150570151604026,55.1756472309721,
-1.16821829680702));
#42433=CARTESIAN_POINT('Ctrl Pts',(-0.133081741600732,55.1744334106545,
-1.17033950247483));
#42434=CARTESIAN_POINT('Ctrl Pts',(-0.0228882669816492,55.1667278577028,
-1.18120338186185));
#42435=CARTESIAN_POINT('Ctrl Pts',(0.0705179241507803,55.1599034126684,
-1.17931602784043));
#42436=CARTESIAN_POINT('Ctrl Pts',(0.199696341161701,55.1503301409976,-1.16129726466999));
#42437=CARTESIAN_POINT('Ctrl Pts',(0.236422329441821,55.1475981298246,-1.15438067831659));
#42438=CARTESIAN_POINT('Ctrl Pts',(0.287477912709399,55.1438308716834,-1.14222608477471));
#42439=CARTESIAN_POINT('Ctrl Pts',(0.302128398210021,55.142753585537,-1.13843860365688));
#42440=CARTESIAN_POINT('Ctrl Pts',(0.327959306863097,55.1408653242706,-1.13122692153458));
#42441=CARTESIAN_POINT('Ctrl Pts',(0.339169243463613,55.1400496455071,-1.12791662154292));
#42442=CARTESIAN_POINT('Ctrl Pts',(0.356505868577216,55.138795983177,-1.12251525216569));
#42443=CARTESIAN_POINT('Ctrl Pts',(0.362667397416046,55.1383519749648,-1.12053973135057));
#42444=CARTESIAN_POINT('Ctrl Pts',(0.374304986737848,55.1375167075187,-1.11670241630598));
#42445=CARTESIAN_POINT('Ctrl Pts',(0.379783834396527,55.1371249413078,-1.11485099909677));
#42446=CARTESIAN_POINT('Ctrl Pts',(0.391892151841738,55.1362620378887,-1.11065972328108));
#42447=CARTESIAN_POINT('Ctrl Pts',(0.398514642205714,55.1357920035062,-1.1083007559317));
#42448=CARTESIAN_POINT('Ctrl Pts',(0.421970704264982,55.1341326984923,-1.09970814217985));
#42449=CARTESIAN_POINT('Ctrl Pts',(0.438683322208201,55.1329605474249,-1.09314879974131));
#42450=CARTESIAN_POINT('Ctrl Pts',(0.529358251229775,55.1266226838263,-1.05514609639314));
#42451=CARTESIAN_POINT('Ctrl Pts',(0.600109195413689,55.1217457685267,-1.01657514608013));
#42452=CARTESIAN_POINT('Ctrl Pts',(0.705275321940152,55.1138337369647,-0.944407956330997));
#42453=CARTESIAN_POINT('Ctrl Pts',(0.742523673309843,55.110880311461,-0.915411205695369));
#42454=CARTESIAN_POINT('Ctrl Pts',(0.794690351953948,55.1064125720665,-0.869517425825553));
#42455=CARTESIAN_POINT('Ctrl Pts',(0.81102593353514,55.1049609202146,-0.854300966380128));
#42456=CARTESIAN_POINT('Ctrl Pts',(0.835342213669571,55.1027101026158,-0.83032427253948));
#42457=CARTESIAN_POINT('Ctrl Pts',(0.843640010916647,55.1019250696309,-0.821892040613529));
#42458=CARTESIAN_POINT('Ctrl Pts',(0.858719244636236,55.1004656984753,-0.806099525332553));
#42459=CARTESIAN_POINT('Ctrl Pts',(0.865536652797595,55.09979301014,-0.798774985727742));
#42460=CARTESIAN_POINT('Ctrl Pts',(0.880455702471621,55.0982913370803,-0.7823308773912));
#42461=CARTESIAN_POINT('Ctrl Pts',(0.888510557994411,55.0974604866322,-0.773170624405136));
#42462=CARTESIAN_POINT('Ctrl Pts',(0.912175700863119,55.0949573044256,-0.745399585917283));
#42463=CARTESIAN_POINT('Ctrl Pts',(0.927353181809483,55.0932678729912,-0.726430297473123));
#42464=CARTESIAN_POINT('Ctrl Pts',(0.994336376675785,55.0854069795649,-0.637189755074405));
#42465=CARTESIAN_POINT('Ctrl Pts',(1.03880891099775,55.078974589261,-0.561771538500964));
#42466=CARTESIAN_POINT('Ctrl Pts',(1.08845369282136,55.0700790176018,-0.451131278540514));
#42467=CARTESIAN_POINT('Ctrl Pts',(1.10102277128972,55.0675976218426,-0.419523533730215));
#42468=CARTESIAN_POINT('Ctrl Pts',(1.11901939451923,55.0636764178484,-0.367858019628456));
#42469=CARTESIAN_POINT('Ctrl Pts',(1.12531504105737,55.0622094017894,-0.348123699700449));
#42470=CARTESIAN_POINT('Ctrl Pts',(1.13332276159006,55.0602095675463,-0.320529118524553));
#42471=CARTESIAN_POINT('Ctrl Pts',(1.13547947811581,55.0596551756115,-0.312803071691913));
#42472=CARTESIAN_POINT('Ctrl Pts',(1.13903960171143,55.0587127053363,-0.299527302380195));
#42473=CARTESIAN_POINT('Ctrl Pts',(1.14048175790144,55.0583225162112,-0.293988409249102));
#42474=CARTESIAN_POINT('Ctrl Pts',(1.14349859068343,55.0574878604059,-0.282045248826515));
#42475=CARTESIAN_POINT('Ctrl Pts',(1.14505993746908,55.0570441303354,-0.275637976589591));
#42476=CARTESIAN_POINT('Ctrl Pts',(1.14931652314479,55.0557991903506,-0.257509666811821));
#42477=CARTESIAN_POINT('Ctrl Pts',(1.15188625205993,55.0550046342972,-0.245759615852099));
#42478=CARTESIAN_POINT('Ctrl Pts',(1.16866286949696,55.0494811374149,-0.162993878607308));
#42479=CARTESIAN_POINT('Ctrl Pts',(1.17647457772493,55.0450357830271,-0.0908306980814718));
#42480=CARTESIAN_POINT('Ctrl Pts',(1.17861992250281,55.0365543817954,0.0464771725981341));
#42481=CARTESIAN_POINT('Ctrl Pts',(1.17427072198975,55.0325376066607,0.111320340806615));
#42482=CARTESIAN_POINT('Ctrl Pts',(1.16131534920626,55.0269445488811,0.197304866431528));
#42483=CARTESIAN_POINT('Ctrl Pts',(1.15741269030201,55.0255083145317,0.219039527545507));
#42484=CARTESIAN_POINT('Ctrl Pts',(1.15049587333197,55.0232768939478,0.252176406502493));
#42485=CARTESIAN_POINT('Ctrl Pts',(1.14791741253601,55.022495491184,0.263665112773433));
#42486=CARTESIAN_POINT('Ctrl Pts',(1.14283262324068,55.0210405404852,0.284830729511583));
#42487=CARTESIAN_POINT('Ctrl Pts',(1.14037448914068,55.0203686010731,0.294518188008761));
#42488=CARTESIAN_POINT('Ctrl Pts',(1.13463569169775,55.0188656632129,0.315984811844149));
#42489=CARTESIAN_POINT('Ctrl Pts',(1.13129432004946,55.0180327591753,0.327746389496244));
#42490=CARTESIAN_POINT('Ctrl Pts',(1.12093920459054,55.0155676414008,0.362149323748651));
#42491=CARTESIAN_POINT('Ctrl Pts',(1.11342476060808,55.0139194431366,0.384632285434582));
#42492=CARTESIAN_POINT('Ctrl Pts',(1.07497959076489,55.0060831839344,0.489065762650575));
#42493=CARTESIAN_POINT('Ctrl Pts',(1.03565070053304,54.9996300485901,0.56761746655025));
#42494=CARTESIAN_POINT('Ctrl Pts',(0.969442531588526,54.990707116571,0.669654610185804));
#42495=CARTESIAN_POINT('Ctrl Pts',(0.949662429277538,54.9882198945523,0.697422151102629));
#42496=CARTESIAN_POINT('Ctrl Pts',(0.915953401506806,54.9842911252898,0.740644560120905));
#42497=CARTESIAN_POINT('Ctrl Pts',(0.902771317562335,54.982822225183,0.756656507838739));
#42498=CARTESIAN_POINT('Ctrl Pts',(0.883913089836965,54.980820630026,0.778368188113838));
#42499=CARTESIAN_POINT('Ctrl Pts',(0.878591895189533,54.980266284748,0.784369605151189));
#42500=CARTESIAN_POINT('Ctrl Pts',(0.869370039852177,54.9793239666549,0.794558705080641));
#42501=CARTESIAN_POINT('Ctrl Pts',(0.865499503476447,54.9789338830451,0.798773069888746));
#42502=CARTESIAN_POINT('Ctrl Pts',(0.857100945073473,54.9780992021727,0.807784961597127));
#42503=CARTESIAN_POINT('Ctrl Pts',(0.852563133054223,54.9776553437771,0.812572878971173));
#42504=CARTESIAN_POINT('Ctrl Pts',(0.839643177793984,54.9764106544644,0.825977538676623));
#42505=CARTESIAN_POINT('Ctrl Pts',(0.831168742760805,54.9756164608695,0.834504708796131));
#42506=CARTESIAN_POINT('Ctrl Pts',(0.759887831500031,54.96910190012,0.904065865912003));
#42507=CARTESIAN_POINT('Ctrl Pts',(0.690575612665228,54.9637969538521,0.958057510733683));
#42508=CARTESIAN_POINT('Ctrl Pts',(0.564118631517385,54.9546026258532,1.03564331340699));
#42509=CARTESIAN_POINT('Ctrl Pts',(0.509953626425511,54.9507945419868,1.06335925664925));
#42510=CARTESIAN_POINT('Ctrl Pts',(0.439022031967292,54.9457910238096,1.09298424626383));
#42511=CARTESIAN_POINT('Ctrl Pts',(0.424022193437949,54.9447324721056,1.09889037001887));
#42512=CARTESIAN_POINT('Ctrl Pts',(0.398974666808698,54.9429614303825,1.10816354301393));
#42513=CARTESIAN_POINT('Ctrl Pts',(0.388994032596335,54.9422548527236,1.1117062799895));
#42514=CARTESIAN_POINT('Ctrl Pts',(0.369290280166225,54.9408575239399,1.1184025262171));
#42515=CARTESIAN_POINT('Ctrl Pts',(0.35957118745721,54.9401671421677,1.1215650098626));
#42516=CARTESIAN_POINT('Ctrl Pts',(0.337993190246875,54.9386313406715,1.12827695021194));
#42517=CARTESIAN_POINT('Ctrl Pts',(0.326117142671027,54.9377840575074,1.13176669936527));
#42518=CARTESIAN_POINT('Ctrl Pts',(0.283985485277921,54.9347701025525,1.1434288060589));
#42519=CARTESIAN_POINT('Ctrl Pts',(0.253463298716431,54.9325715292742,1.15057951998783));
#42520=CARTESIAN_POINT('Ctrl Pts',(0.211467917550879,54.9295255765537,1.15866608436263));
#42521=CARTESIAN_POINT('Ctrl Pts',(0.200214607584779,54.9287074012446,1.16066346791927));
#42522=CARTESIAN_POINT('Ctrl Pts',(0.188938369713642,54.9278857931129,1.16249617416573));
#42523=CARTESIAN_POINT('Origin',(0.,56.5393671147362,0.));
#42524=CARTESIAN_POINT('',(0.188938462403164,54.3284116054606,1.16249615910106));
#42525=CARTESIAN_POINT('',(0.188938462297913,54.4261253209981,1.16249615911817));
#42526=CARTESIAN_POINT('',(0.188938462403162,56.5393671147362,1.16249615910107));
#42527=CARTESIAN_POINT('',(-1.17774953014575,54.6906328852638,-0.00105201780795915));
#42528=CARTESIAN_POINT('Ctrl Pts',(-1.17774953014575,54.6906328852638,-0.00105201780795915));
#42529=CARTESIAN_POINT('Ctrl Pts',(-1.17769714698767,54.6866752250911,-0.0596957397588973));
#42530=CARTESIAN_POINT('Ctrl Pts',(-1.17326078513928,54.6827175649183,-0.118144736281013));
#42531=CARTESIAN_POINT('Ctrl Pts',(-1.16455024767417,54.6787599047456,-0.175834533417163));
#42532=CARTESIAN_POINT('Ctrl Pts',(-1.1571934473316,54.6754173193045,-0.224558543965765));
#42533=CARTESIAN_POINT('Ctrl Pts',(-1.14678867429975,54.6720747338635,-0.272741503821657));
#42534=CARTESIAN_POINT('Ctrl Pts',(-1.13342818814217,54.6687321484224,-0.320055627703607));
#42535=CARTESIAN_POINT('Ctrl Pts',(-1.12020882427835,54.6654248695802,-0.366869988507296));
#42536=CARTESIAN_POINT('Ctrl Pts',(-1.10405318292451,54.6621175907379,-0.412973781673877));
#42537=CARTESIAN_POINT('Ctrl Pts',(-1.08506006393155,54.6588103118957,-0.457973492858332));
#42538=CARTESIAN_POINT('Ctrl Pts',(-1.06685448075384,54.6556401669565,-0.501107323865514));
#42539=CARTESIAN_POINT('Ctrl Pts',(-1.04604235028559,54.6524700220173,-0.543226257802928));
#42540=CARTESIAN_POINT('Ctrl Pts',(-1.0227617720575,54.6492998770781,-0.583997791192575));
#42541=CARTESIAN_POINT('Ctrl Pts',(-0.999504564628519,54.6461329145694,
-0.624728395043999));
#42542=CARTESIAN_POINT('Ctrl Pts',(-0.973784089242021,54.6429659520607,
-0.664113792576353));
#42543=CARTESIAN_POINT('Ctrl Pts',(-0.945785259301189,54.6397989895519,
-0.701844217607143));
#42544=CARTESIAN_POINT('Ctrl Pts',(-0.917802165167313,54.6366338069286,
-0.739553437513079));
#42545=CARTESIAN_POINT('Ctrl Pts',(-0.887543584916521,54.6334686243054,
-0.77560907957072));
#42546=CARTESIAN_POINT('Ctrl Pts',(-0.855237312034212,54.6303034416821,
-0.809730944576343));
#42547=CARTESIAN_POINT('Ctrl Pts',(-0.822934921954927,54.6271386394735,
-0.843848708567865));
#42548=CARTESIAN_POINT('Ctrl Pts',(-0.788585712944688,54.6239738372649,
-0.876032752989566));
#42549=CARTESIAN_POINT('Ctrl Pts',(-0.752455412507077,54.6208090350563,
-0.906038583443777));
#42550=CARTESIAN_POINT('Ctrl Pts',(-0.716288276356329,54.6176410062555,
-0.93607500556619));
#42551=CARTESIAN_POINT('Ctrl Pts',(-0.678336856667729,54.6144729774547,
-0.963928426297382));
#42552=CARTESIAN_POINT('Ctrl Pts',(-0.638899611772667,54.6113049486539,
-0.989394940646421));
#42553=CARTESIAN_POINT('Ctrl Pts',(-0.599438485017693,54.6081350014022,
-1.01487687665409));
#42554=CARTESIAN_POINT('Ctrl Pts',(-0.558490229227848,54.6049650541504,
-1.03796875576431));
#42555=CARTESIAN_POINT('Ctrl Pts',(-0.516378727411899,54.6017951068987,
-1.05851219755677));
#42556=CARTESIAN_POINT('Ctrl Pts',(-0.47419022450317,54.5986193633824,-1.07909320313584));
#42557=CARTESIAN_POINT('Ctrl Pts',(-0.430834748697438,54.5954436198662,
-1.09711626416715));
#42558=CARTESIAN_POINT('Ctrl Pts',(-0.38665520238492,54.5922678763499,-1.11247149040714));
#42559=CARTESIAN_POINT('Ctrl Pts',(-0.373159040957775,54.5912977363027,
-1.11716227221416));
#42560=CARTESIAN_POINT('Ctrl Pts',(-0.359586067085624,54.5903275962555,
-1.12160444674893));
#42561=CARTESIAN_POINT('Ctrl Pts',(-0.345946256988187,54.5893574562082,
-1.12579582952499));
#42562=CARTESIAN_POINT('Ctrl Pts',(-0.299447140209867,54.586050177366,-1.14008456197615));
#42563=CARTESIAN_POINT('Ctrl Pts',(-0.251952195345861,54.5827428985237,
-1.151521109822));
#42564=CARTESIAN_POINT('Ctrl Pts',(-0.203845604152202,54.5794356196815,
-1.15997501359634));
#42565=CARTESIAN_POINT('Ctrl Pts',(-0.157733757229438,54.5762654774635,
-1.16807837546566));
#42566=CARTESIAN_POINT('Ctrl Pts',(-0.11106060852584,54.5730953352455,-1.17344147846441));
#42567=CARTESIAN_POINT('Ctrl Pts',(-0.0641804021668466,54.5699251930276,
-1.17599997384256));
#42568=CARTESIAN_POINT('Ctrl Pts',(-0.0173472578631847,54.5667582332489,
-1.1785559008009));
#42569=CARTESIAN_POINT('Ctrl Pts',(0.029691977687938,54.5635912734702,-1.1783127619046));
#42570=CARTESIAN_POINT('Ctrl Pts',(0.076576767781138,54.5604243136914,-1.17525787005925));
#42571=CARTESIAN_POINT('Ctrl Pts',(0.123435207772002,54.5572591338016,-1.17220469511851));
#42572=CARTESIAN_POINT('Ctrl Pts',(0.170138817970292,54.5540939539117,-1.16634293350421));
#42573=CARTESIAN_POINT('Ctrl Pts',(0.216328640527614,54.5509287740218,-1.15771195976697));
#42574=CARTESIAN_POINT('Ctrl Pts',(0.26251291168148,54.5477639745445,-1.14908202335819));
#42575=CARTESIAN_POINT('Ctrl Pts',(0.308182969548269,54.5445991750672,-1.13768363999169));
#42576=CARTESIAN_POINT('Ctrl Pts',(0.352989274454559,54.54143437559,-1.12360742015174));
#42577=CARTESIAN_POINT('Ctrl Pts',(0.397841260845054,54.5382663494968,-1.10951684914813));
#42578=CARTESIAN_POINT('Ctrl Pts',(0.441827203933968,54.5350983234035,-1.09274316305695));
#42579=CARTESIAN_POINT('Ctrl Pts',(0.484613908187637,54.5319302973103,-1.07342648676614));
#42580=CARTESIAN_POINT('Ctrl Pts',(0.52742652278707,54.5287603527555,-1.0540981128751));
#42581=CARTESIAN_POINT('Ctrl Pts',(0.569037959078233,54.5255904082006,-1.03222394445421));
#42582=CARTESIAN_POINT('Ctrl Pts',(0.609139474858335,54.5224204636457,-1.00799016000619));
#42583=CARTESIAN_POINT('Ctrl Pts',(0.649314317073937,54.5192447227829,-0.983712063591465));
#42584=CARTESIAN_POINT('Ctrl Pts',(0.687973273422185,54.5160689819201,-0.957066063031638));
#42585=CARTESIAN_POINT('Ctrl Pts',(0.724838020934945,54.5128932410573,-0.928280618082222));
#42586=CARTESIAN_POINT('Ctrl Pts',(0.736099855229156,54.5119230820362,-0.919486934875976));
#42587=CARTESIAN_POINT('Ctrl Pts',(0.747194496707031,54.5109529230151,-0.910493858644433));
#42588=CARTESIAN_POINT('Ctrl Pts',(0.758114698226789,54.5099827639941,-0.90130858579762));
#42589=CARTESIAN_POINT('Ctrl Pts',(0.795341741067799,54.5066754851518,-0.869995926854831));
#42590=CARTESIAN_POINT('Ctrl Pts',(0.83071287117427,54.5033682063096,-0.836299528044534));
#42591=CARTESIAN_POINT('Ctrl Pts',(0.863910092825719,54.5000609274673,-0.800471369890178));
#42592=CARTESIAN_POINT('Ctrl Pts',(0.895730772895249,54.4968907868138,-0.766128846588667));
#42593=CARTESIAN_POINT('Ctrl Pts',(0.925553863000638,54.4937206461603,-0.729828340555749));
#42594=CARTESIAN_POINT('Ctrl Pts',(0.953133146393215,54.4905505055069,-0.691832543139285));
#42595=CARTESIAN_POINT('Ctrl Pts',(0.980684743215,54.4873835473263,-0.653874889329382));
#42596=CARTESIAN_POINT('Ctrl Pts',(1.00599666473445,54.4842165891458,-0.614225762145114));
#42597=CARTESIAN_POINT('Ctrl Pts',(1.02886268130304,54.4810496309653,-0.57318116291616));
#42598=CARTESIAN_POINT('Ctrl Pts',(1.05171584652856,54.4778844527041,-0.532159631903922));
#42599=CARTESIAN_POINT('Ctrl Pts',(1.07212555832836,54.4747192744429,-0.489744669280312));
#42600=CARTESIAN_POINT('Ctrl Pts',(1.08993018001366,54.4715540961818,-0.446259190600479));
#42601=CARTESIAN_POINT('Ctrl Pts',(1.10773266166441,54.4683892983607,-0.402778938677412));
#42602=CARTESIAN_POINT('Ctrl Pts',(1.12293046516394,54.4652245005396,-0.358228943358692));
#42603=CARTESIAN_POINT('Ctrl Pts',(1.13541010551767,54.4620597027184,-0.312952000773857));
#42604=CARTESIAN_POINT('Ctrl Pts',(1.14790246916459,54.4588916783099,-0.267628897258153));
#42605=CARTESIAN_POINT('Ctrl Pts',(1.15767099281451,54.4557236539014,-0.221577907227785));
#42606=CARTESIAN_POINT('Ctrl Pts',(1.16465265388608,54.4525556294928,-0.175154955100094));
#42607=CARTESIAN_POINT('Ctrl Pts',(1.17163854280376,54.4493856866412,-0.128703890880537));
#42608=CARTESIAN_POINT('Ctrl Pts',(1.17583416122577,54.4462157437895,-0.081880972708021));
#42609=CARTESIAN_POINT('Ctrl Pts',(1.17722844039909,54.4430458009378,-0.0350465635337289));
#42610=CARTESIAN_POINT('Ctrl Pts',(1.17862526903709,54.4398700617883,0.0118734832045577));
#42611=CARTESIAN_POINT('Ctrl Pts',(1.17721055979432,54.4366943226388,0.0588045053487816));
#42612=CARTESIAN_POINT('Ctrl Pts',(1.17302526479399,54.4335185834894,0.105388759623576));
#42613=CARTESIAN_POINT('Ctrl Pts',(1.17174668055132,54.4325484129195,0.119619989075107));
#42614=CARTESIAN_POINT('Ctrl Pts',(1.17020988885955,54.4315782423497,0.133818920283906));
#42615=CARTESIAN_POINT('Ctrl Pts',(1.16841700426522,54.4306080717799,0.147975560968334));
#42616=CARTESIAN_POINT('Ctrl Pts',(1.16230512098418,54.4273007929376,0.196235072923688));
#42617=CARTESIAN_POINT('Ctrl Pts',(1.15318394782368,54.4239935140954,0.244228494460377));
#42618=CARTESIAN_POINT('Ctrl Pts',(1.1410926766969,54.4206862352531,0.291551994828893));
#42619=CARTESIAN_POINT('Ctrl Pts',(1.1295027712319,54.4175160930302,0.336913221931717));
#42620=CARTESIAN_POINT('Ctrl Pts',(1.11518439637597,54.4143459508072,0.381658386778636));
#42621=CARTESIAN_POINT('Ctrl Pts',(1.09822467823407,54.4111758085843,0.425438148991927));
#42622=CARTESIAN_POINT('Ctrl Pts',(1.08128198566579,54.4080088488134,0.469173961443887));
#42623=CARTESIAN_POINT('Ctrl Pts',(1.06170339831795,54.4048418890425,0.511945770956285));
#42624=CARTESIAN_POINT('Ctrl Pts',(1.03962571650836,54.4016749292716,0.55341976118899));
#42625=CARTESIAN_POINT('Ctrl Pts',(1.01756044284565,54.3985097494023,0.594870442119264));
#42626=CARTESIAN_POINT('Ctrl Pts',(0.992999118661742,54.3953445695331,0.63502425644045));
#42627=CARTESIAN_POINT('Ctrl Pts',(0.966125343888607,54.3921793896638,0.673570250527828));
#42628=CARTESIAN_POINT('Ctrl Pts',(0.939254799095291,54.38901459022,0.712111611742302));
#42629=CARTESIAN_POINT('Ctrl Pts',(0.910072676264339,54.3858497907761,0.749045079670299));
#42630=CARTESIAN_POINT('Ctrl Pts',(0.878805396448503,54.3826849913323,0.78408936842237));
#42631=CARTESIAN_POINT('Ctrl Pts',(0.847506238811093,54.3795169652914,0.819169385756862));
#42632=CARTESIAN_POINT('Ctrl Pts',(0.814118055742262,54.3763489392505,0.852355964318174));
#42633=CARTESIAN_POINT('Ctrl Pts',(0.778905670317124,54.3731809132097,0.883403089901678));
#42634=CARTESIAN_POINT('Ctrl Pts',(0.743671961449416,54.3700109687182,0.914469016585741));
#42635=CARTESIAN_POINT('Ctrl Pts',(0.70661229246037,54.3668410242268,0.943392568656226));
#42636=CARTESIAN_POINT('Ctrl Pts',(0.668023397274221,54.3636710797353,0.969968970222352));
#42637=CARTESIAN_POINT('Ctrl Pts',(0.629363941700992,54.3604953389518,0.996593967146614));
#42638=CARTESIAN_POINT('Ctrl Pts',(0.589170160888317,54.3573195981681,1.02086296610438));
#42639=CARTESIAN_POINT('Ctrl Pts',(0.547764806441438,54.3541438573845,1.04261631453003));
#42640=CARTESIAN_POINT('Ctrl Pts',(0.535115855754481,54.3531736981116,1.04926176015386));
#42641=CARTESIAN_POINT('Ctrl Pts',(0.522353977954967,54.3522035388387,1.05567277334354));
#42642=CARTESIAN_POINT('Ctrl Pts',(0.509488714157003,54.3512333795657,1.06184571037729));
#42643=CARTESIAN_POINT('Ctrl Pts',(0.46737285401055,54.3480574561722,1.08205350066351));
#42644=CARTESIAN_POINT('Ctrl Pts',(0.423958030108927,54.3448815327787,1.09979725698727));
#42645=CARTESIAN_POINT('Ctrl Pts',(0.379562947566655,54.3417056093853,1.11491122127931));
#42646=CARTESIAN_POINT('Ctrl Pts',(0.335244821753066,54.3385351913014,1.12999898624514));
#42647=CARTESIAN_POINT('Ctrl Pts',(0.289950328535312,54.3353647732175,1.14246581355573));
#42648=CARTESIAN_POINT('Ctrl Pts',(0.244019505938903,54.3321943551337,1.15219336190647));
#42649=CARTESIAN_POINT('Ctrl Pts',(0.225752219673109,54.330933438576,1.15606213455939));
#42650=CARTESIAN_POINT('Ctrl Pts',(0.20738449580817,54.3296725220183,1.15949815763526));
#42651=CARTESIAN_POINT('Ctrl Pts',(0.188938462403164,54.3284116054606,1.16249615910106));
#42652=CARTESIAN_POINT('Ctrl Pts',(0.189250941523835,54.8284605668477,1.16440479426666));
#42653=CARTESIAN_POINT('Ctrl Pts',(0.184506076350226,54.8281342221821,1.16518167980759));
#42654=CARTESIAN_POINT('Ctrl Pts',(-0.205344558386595,54.8013496467784,
1.22634143776596));
#42655=CARTESIAN_POINT('Ctrl Pts',(-0.929401945135899,54.7554070862504,
0.962178865328913));
#42656=CARTESIAN_POINT('Ctrl Pts',(-1.17480714037443,54.7097908703881,0.282712264297831));
#42657=CARTESIAN_POINT('Ctrl Pts',(-1.17726285833084,54.6906328852638,-0.00105158309123631));
#42658=CARTESIAN_POINT('Ctrl Pts',(0.188938369713642,54.9278857931129,1.16249617416573));
#42659=CARTESIAN_POINT('Ctrl Pts',(0.108581669493369,54.9220308511459,1.17555640117773));
#42660=CARTESIAN_POINT('Ctrl Pts',(0.0270620916905724,54.9159800893122,
1.18025324761532));
#42661=CARTESIAN_POINT('Ctrl Pts',(-0.077617854509977,54.9083565733959,
1.17542123889652));
#42662=CARTESIAN_POINT('Ctrl Pts',(-0.100893065296731,54.9066724863899,
1.17365256173212));
#42663=CARTESIAN_POINT('Ctrl Pts',(-0.14005917505716,54.9038719617761,1.16950245545791));
#42664=CARTESIAN_POINT('Ctrl Pts',(-0.155981514105395,54.9027428553921,
1.16748550112007));
#42665=CARTESIAN_POINT('Ctrl Pts',(-0.179072317711987,54.9011236996199,
1.16407960968587));
#42666=CARTESIAN_POINT('Ctrl Pts',(-0.186276257296968,54.9006211569238,
1.16294857823349));
#42667=CARTESIAN_POINT('Ctrl Pts',(-0.19905645408507,54.8997348032224,1.16082025773074));
#42668=CARTESIAN_POINT('Ctrl Pts',(-0.204636607717194,54.8993496028971,
1.15984956150082));
#42669=CARTESIAN_POINT('Ctrl Pts',(-0.217214822377719,54.8984853764831,
1.15756791011367));
#42670=CARTESIAN_POINT('Ctrl Pts',(-0.224208271457074,54.8980076380246,
1.1562337147267));
#42671=CARTESIAN_POINT('Ctrl Pts',(-0.245980185316471,54.8965277735199,
1.15187514313082));
#42672=CARTESIAN_POINT('Ctrl Pts',(-0.260713552500866,54.8955370300955,
1.14863009369191));
#42673=CARTESIAN_POINT('Ctrl Pts',(-0.347820091324163,54.8897212876633,
1.12768217855371));
#42674=CARTESIAN_POINT('Ctrl Pts',(-0.418450900997335,54.8851698085063,
1.10342527070036));
#42675=CARTESIAN_POINT('Ctrl Pts',(-0.527974751455495,54.8777351613088,
1.05376908114118));
#42676=CARTESIAN_POINT('Ctrl Pts',(-0.568489790798299,54.8748949739316,
1.03247545610662));
#42677=CARTESIAN_POINT('Ctrl Pts',(-0.633558495604673,54.8700680564544,
0.99328374925848));
#42678=CARTESIAN_POINT('Ctrl Pts',(-0.658842832371133,54.8681206356811,
0.976695888467234));
#42679=CARTESIAN_POINT('Ctrl Pts',(-0.694201584681734,54.8652725059112,
0.95150049994778));
#42680=CARTESIAN_POINT('Ctrl Pts',(-0.704813837404146,54.8644007708928,
0.943666505115941));
#42681=CARTESIAN_POINT('Ctrl Pts',(-0.723303031717886,54.8628503575778,
0.929531856295309));
#42682=CARTESIAN_POINT('Ctrl Pts',(-0.73123491696054,54.8621746190346,0.923305059502648));
#42683=CARTESIAN_POINT('Ctrl Pts',(-0.747772405007723,54.8607425859896,
0.909975809455529));
#42684=CARTESIAN_POINT('Ctrl Pts',(-0.75635894686126,54.8599854487067,0.902851411910783));
#42685=CARTESIAN_POINT('Ctrl Pts',(-0.779239708303687,54.8579300140871,
0.883311371016615));
#42686=CARTESIAN_POINT('Ctrl Pts',(-0.793337355154101,54.8566226121273,
0.870671734589314));
#42687=CARTESIAN_POINT('Ctrl Pts',(-0.867104472317129,54.8495538179979,
0.801254354402917));
#42688=CARTESIAN_POINT('Ctrl Pts',(-0.920989442588037,54.8435432644789,
0.738683132758252));
#42689=CARTESIAN_POINT('Ctrl Pts',(-1.00312490803696,54.8329487937804,0.620207925566341));
#42690=CARTESIAN_POINT('Ctrl Pts',(-1.03429751970192,54.8284055593831,0.566698794979591));
#42691=CARTESIAN_POINT('Ctrl Pts',(-1.06606476437224,54.823253417583,0.50072999928577));
#42692=CARTESIAN_POINT('Ctrl Pts',(-1.07085436532039,54.8224594372652,0.490403473146365));
#42693=CARTESIAN_POINT('Ctrl Pts',(-1.07809910779166,54.8212325815254,0.474171109776234));
#42694=CARTESIAN_POINT('Ctrl Pts',(-1.08065700117231,54.8207940213225,0.468312265745476));
#42695=CARTESIAN_POINT('Ctrl Pts',(-1.08541558695512,54.8199681200594,0.457166117124832));
#42696=CARTESIAN_POINT('Ctrl Pts',(-1.08762559530859,54.8195802720838,0.451883193769292));
#42697=CARTESIAN_POINT('Ctrl Pts',(-1.09298637632923,54.8186283091335,0.438801310182127));
#42698=CARTESIAN_POINT('Ctrl Pts',(-1.09609237283216,54.8180667946752,0.430984140251647));
#42699=CARTESIAN_POINT('Ctrl Pts',(-1.10700727185474,54.8160542896141,0.402632079139013));
#42700=CARTESIAN_POINT('Ctrl Pts',(-1.11432548104744,54.8146287099396,0.381911711804298));
#42701=CARTESIAN_POINT('Ctrl Pts',(-1.14439677534529,54.8083525859727,0.288526705492827));
#42702=CARTESIAN_POINT('Ctrl Pts',(-1.16065296617681,54.8037277940154,0.21395851718434));
#42703=CARTESIAN_POINT('Ctrl Pts',(-1.17500700128451,54.7961443342316,0.092600222495293));
#42704=CARTESIAN_POINT('Ctrl Pts',(-1.17772883794596,54.7932584919118,0.0465884156002357));
#42705=CARTESIAN_POINT('Ctrl Pts',(-1.17775905422434,54.7890057452512,-0.0195486318965704));
#42706=CARTESIAN_POINT('Ctrl Pts',(-1.1772543585512,54.7877008649724,-0.0396312800953101));
#42707=CARTESIAN_POINT('Ctrl Pts',(-1.17560237447178,54.7855579377134,-0.072184705846541));
#42708=CARTESIAN_POINT('Ctrl Pts',(-1.17476930470118,54.7847295782293,-0.0846677938813687));
#42709=CARTESIAN_POINT('Ctrl Pts',(-1.17291149514694,54.7832267674816,-0.10711679915608));
#42710=CARTESIAN_POINT('Ctrl Pts',(-1.17195814144035,54.7825546175109,-0.117087523376365));
#42711=CARTESIAN_POINT('Ctrl Pts',(-1.16963011200334,54.7810975712469,-0.138543276299966));
#42712=CARTESIAN_POINT('Ctrl Pts',(-1.16821318832554,54.7803114094776,-0.150022558999053));
#42713=CARTESIAN_POINT('Ctrl Pts',(-1.16375058502073,54.7780839065945,-0.182263304119424));
#42714=CARTESIAN_POINT('Ctrl Pts',(-1.16031893835141,54.7766306519293,-0.202966004753446));
#42715=CARTESIAN_POINT('Ctrl Pts',(-1.15122345551503,54.7732739204956,-0.250010230692414));
#42716=CARTESIAN_POINT('Ctrl Pts',(-1.14520520299659,54.7713606084661,-0.276270551289992));
#42717=CARTESIAN_POINT('Ctrl Pts',(-1.1188945800364,54.7639958192158,-0.375341658136661));
#42718=CARTESIAN_POINT('Ctrl Pts',(-1.09251201653423,54.7583975787809,-0.446343184072841));
#42719=CARTESIAN_POINT('Ctrl Pts',(-1.04185166901587,54.7499215403512,-0.550705009782923));
#42720=CARTESIAN_POINT('Ctrl Pts',(-1.02232476271566,54.7469973203523,-0.586160087344906));
#42721=CARTESIAN_POINT('Ctrl Pts',(-0.995716171738834,54.7434572921974,
-0.629082921543322));
#42722=CARTESIAN_POINT('Ctrl Pts',(-0.990312910763654,54.7427586216219,
-0.637554995829922));
#42723=CARTESIAN_POINT('Ctrl Pts',(-0.98145111325753,54.7416458264976,-0.651065352990109));
#42724=CARTESIAN_POINT('Ctrl Pts',(-0.978060773390028,54.7412275500888,
-0.656147475368266));
#42725=CARTESIAN_POINT('Ctrl Pts',(-0.971284256245348,54.7404064328614,
-0.666136241299758));
#42726=CARTESIAN_POINT('Ctrl Pts',(-0.967900093340072,54.7400034950416,
-0.671043970757845));
#42727=CARTESIAN_POINT('Ctrl Pts',(-0.959113326017375,54.7389748023258,
-0.68358181002923));
#42728=CARTESIAN_POINT('Ctrl Pts',(-0.953656732186058,54.7383525660555,
-0.691173866745431));
#42729=CARTESIAN_POINT('Ctrl Pts',(-0.928554737045014,54.7355598758739,
-0.725236325850173));
#42730=CARTESIAN_POINT('Ctrl Pts',(-0.907892009083777,54.7334494814902,
-0.750942172714864));
#42731=CARTESIAN_POINT('Ctrl Pts',(-0.831956102099352,54.7261844494736,
-0.837687424251704));
#42732=CARTESIAN_POINT('Ctrl Pts',(-0.771391268898121,54.72120722517,-0.893771644464102));
#42733=CARTESIAN_POINT('Ctrl Pts',(-0.672745192382404,54.7134752931164,
-0.967563538040086));
#42734=CARTESIAN_POINT('Ctrl Pts',(-0.638770769926838,54.7108721146176,
-0.990321503259062));
#42735=CARTESIAN_POINT('Ctrl Pts',(-0.590897797535063,54.7072321195802,
-1.01889971555601));
#42736=CARTESIAN_POINT('Ctrl Pts',(-0.577967668195078,54.7062517953168,
-1.02628952009828));
#42737=CARTESIAN_POINT('Ctrl Pts',(-0.555906764961072,54.7045818328036,
-1.03834859646736));
#42738=CARTESIAN_POINT('Ctrl Pts',(-0.546848612388174,54.7038968872125,
-1.04314750773779));
#42739=CARTESIAN_POINT('Ctrl Pts',(-0.528349280265607,54.7024988845071,
-1.05264108546199));
#42740=CARTESIAN_POINT('Ctrl Pts',(-0.518905411456307,54.7017856479119,
-1.05732841544101));
#42741=CARTESIAN_POINT('Ctrl Pts',(-0.49507510755737,54.699986338297,-1.06876009004839));
#42742=CARTESIAN_POINT('Ctrl Pts',(-0.480613126983862,54.6988947656863,
-1.07534109525262));
#42743=CARTESIAN_POINT('Ctrl Pts',(-0.414079332678504,54.6938721156605,
-1.10400742266151));
#42744=CARTESIAN_POINT('Ctrl Pts',(-0.360598570169302,54.6898276151714,
-1.12261350612172));
#42745=CARTESIAN_POINT('Ctrl Pts',(-0.236607282692602,54.6804765777453,
-1.15597373823385));
#42746=CARTESIAN_POINT('Ctrl Pts',(-0.165658220731116,54.6751400775437,
-1.16825318048703));
#42747=CARTESIAN_POINT('Ctrl Pts',(-0.0677973196773159,54.6680488363,-1.17609154216601));
#42748=CARTESIAN_POINT('Ctrl Pts',(-0.0414962503687463,54.6661706621978,
-1.17731307788736));
#42749=CARTESIAN_POINT('Ctrl Pts',(-0.00620822457986493,54.6637056175882,
-1.17776777186951));
#42750=CARTESIAN_POINT('Ctrl Pts',(0.00275923744179654,54.6630839576747,
-1.17778090728269));
#42751=CARTESIAN_POINT('Ctrl Pts',(0.0170288891855195,54.6621032106605,
-1.17763882388204));
#42752=CARTESIAN_POINT('Ctrl Pts',(0.0223311839644545,54.6617406504017,
-1.17755021281724));
#42753=CARTESIAN_POINT('Ctrl Pts',(0.0336688795939275,54.6609696451615,
-1.17728413008523));
#42754=CARTESIAN_POINT('Ctrl Pts',(0.0397039171113984,54.6605618117028,
-1.17709605364665));
#42755=CARTESIAN_POINT('Ctrl Pts',(0.0554425579326808,54.6595043162332,
-1.1764843889278));
#42756=CARTESIAN_POINT('Ctrl Pts',(0.0651430615232246,54.658858565791,-1.17598715616429));
#42757=CARTESIAN_POINT('Ctrl Pts',(0.112739746730623,54.6557148767919,-1.17295663925994));
#42758=CARTESIAN_POINT('Ctrl Pts',(0.150507990496832,54.6532972017246,-1.16871103171584));
#42759=CARTESIAN_POINT('Ctrl Pts',(0.236534609546935,54.6478346404813,-1.15479989239462));
#42760=CARTESIAN_POINT('Ctrl Pts',(0.284523181011152,54.6448186888625,-1.14392232147804));
#42761=CARTESIAN_POINT('Ctrl Pts',(0.393870105687706,54.6377672939315,-1.11182753881352));
#42762=CARTESIAN_POINT('Ctrl Pts',(0.45442784818955,54.6337207868725,-1.08847968366745));
#42763=CARTESIAN_POINT('Ctrl Pts',(0.527600976521416,54.6284347459268,-1.05309270401104));
#42764=CARTESIAN_POINT('Ctrl Pts',(0.542294454486342,54.6273525355407,-1.04560208217233));
#42765=CARTESIAN_POINT('Ctrl Pts',(0.566220449129681,54.6255529572428,-1.03276480680303));
#42766=CARTESIAN_POINT('Ctrl Pts',(0.575546495912091,54.6248419195946,-1.02759669205789));
#42767=CARTESIAN_POINT('Ctrl Pts',(0.593728197322663,54.6234360254039,-1.01719598292522));
#42768=CARTESIAN_POINT('Ctrl Pts',(0.60258802423958,54.6227415474659,-1.01197257933475));
#42769=CARTESIAN_POINT('Ctrl Pts',(0.623778198427206,54.6210571287002,-0.999102749447694));
#42770=CARTESIAN_POINT('Ctrl Pts',(0.636037599809329,54.6200631178208,-0.991343373117623));
#42771=CARTESIAN_POINT('Ctrl Pts',(0.681740789331787,54.6162812688511,-0.961219581866173));
#42772=CARTESIAN_POINT('Ctrl Pts',(0.714171268817931,54.6134393373115,-0.937375240573873));
#42773=CARTESIAN_POINT('Ctrl Pts',(0.805441476021531,54.604966194094,-0.862779855198039));
#42774=CARTESIAN_POINT('Ctrl Pts',(0.860557351021353,54.5992073911695,-0.807814554644207));
#42775=CARTESIAN_POINT('Ctrl Pts',(0.933963449342101,54.5907728932945,-0.718504433795098));
#42776=CARTESIAN_POINT('Ctrl Pts',(0.956639811387714,54.5880335490278,-0.688024117740916));
#42777=CARTESIAN_POINT('Ctrl Pts',(0.983350729976969,54.5846755841962,-0.64824019699935));
#42778=CARTESIAN_POINT('Ctrl Pts',(0.988790913662792,54.5839840689516,-0.639911366386337));
#42779=CARTESIAN_POINT('Ctrl Pts',(0.997389461945781,54.5828798356126,-0.626375594541597));
#42780=CARTESIAN_POINT('Ctrl Pts',(1.00061398592784,54.5824630742235,-0.621211541796408));
#42781=CARTESIAN_POINT('Ctrl Pts',(1.00692590964027,54.5816422844805,-0.610926368321388));
#42782=CARTESIAN_POINT('Ctrl Pts',(1.01001462078615,54.5812381885914,-0.605806309022732));
#42783=CARTESIAN_POINT('Ctrl Pts',(1.01787711737896,54.5802025548088,-0.592545601026591));
#42784=CARTESIAN_POINT('Ctrl Pts',(1.02259241760102,54.579574629722,-0.584370496326));
#42785=CARTESIAN_POINT('Ctrl Pts',(1.04387846456012,54.5767036294536,-0.546419218456751));
#42786=CARTESIAN_POINT('Ctrl Pts',(1.05925180605185,54.5745248492067,-0.515986704178548));
#42787=CARTESIAN_POINT('Ctrl Pts',(1.11047992812902,54.566694263782,-0.40260403237415));
#42788=CARTESIAN_POINT('Ctrl Pts',(1.13808041660133,54.5612500644246,-0.316274726700439));
#42789=CARTESIAN_POINT('Ctrl Pts',(1.16204987914672,54.5534084638769,-0.194599410206666));
#42790=CARTESIAN_POINT('Ctrl Pts',(1.16713771155286,54.551249007355,-0.161301271577753));
#42791=CARTESIAN_POINT('Ctrl Pts',(1.1723121967252,54.548129177481,-0.113909414185334));
#42792=CARTESIAN_POINT('Ctrl Pts',(1.17358389329953,54.547205354255,-0.0999602868893795));
#42793=CARTESIAN_POINT('Ctrl Pts',(1.17535126702935,54.5455952498521,-0.0758189479226175));
#42794=CARTESIAN_POINT('Ctrl Pts',(1.17596383084177,54.5449126934121,-0.0656366597614956));
#42795=CARTESIAN_POINT('Ctrl Pts',(1.17695327134181,54.5434977355447,-0.0446436200955752));
#42796=CARTESIAN_POINT('Ctrl Pts',(1.17731362158029,54.5427648827179,-0.0338330981236268));
#42797=CARTESIAN_POINT('Ctrl Pts',(1.17786231659242,54.5408505364274,-0.00576544268209311));
#42798=CARTESIAN_POINT('Ctrl Pts',(1.17782033085533,54.5396620020008,0.0114930477235766));
#42799=CARTESIAN_POINT('Ctrl Pts',(1.17689309380546,54.5370198203333,0.0494746363727649));
#42800=CARTESIAN_POINT('Ctrl Pts',(1.17583957954222,54.5355615004583,0.0701875126270989));
#42801=CARTESIAN_POINT('Ctrl Pts',(1.17075091672426,54.5308759401054,0.13595091066353));
#42802=CARTESIAN_POINT('Ctrl Pts',(1.16466799213186,54.527595840425,0.180798628272209));
#42803=CARTESIAN_POINT('Ctrl Pts',(1.14205207629161,54.5189339489643,0.296902610729511));
#42804=CARTESIAN_POINT('Ctrl Pts',(1.12143712644088,54.5135130500848,0.367169973399234));
#42805=CARTESIAN_POINT('Ctrl Pts',(1.08889429953316,54.5072422613434,0.449032090634663));
#42806=CARTESIAN_POINT('Ctrl Pts',(1.08307956631484,54.5061834682992,0.46288153659903));
#42807=CARTESIAN_POINT('Ctrl Pts',(1.07407486069448,54.5046348216219,0.483229289108244));
#42808=CARTESIAN_POINT('Ctrl Pts',(1.07108759180195,54.5041346880911,0.489814995240465));
#42809=CARTESIAN_POINT('Ctrl Pts',(1.06561034432849,54.5032422018361,0.50160032275441));
#42810=CARTESIAN_POINT('Ctrl Pts',(1.06314249258167,54.5028485846098,0.506809960468223));
#42811=CARTESIAN_POINT('Ctrl Pts',(1.05789437667232,54.5020293351275,0.517681690848827));
#42812=CARTESIAN_POINT('Ctrl Pts',(1.05510672374399,54.5016041534072,0.523339900446246));
#42813=CARTESIAN_POINT('Ctrl Pts',(1.04734369320552,54.5004462676145,0.538782640181988));
#42814=CARTESIAN_POINT('Ctrl Pts',(1.04227663931822,54.4997189388052,0.54852071399552));
#42815=CARTESIAN_POINT('Ctrl Pts',(1.00717831862028,54.4948579261839,0.613731042242867));
#42816=CARTESIAN_POINT('Ctrl Pts',(0.972864593137731,54.4909461546723,0.666791207534335));
#42817=CARTESIAN_POINT('Ctrl Pts',(0.884724827568501,54.4819959243063,0.781686773891485));
#42818=CARTESIAN_POINT('Ctrl Pts',(0.82838195215865,54.4769783437578,0.84116225721547));
#42819=CARTESIAN_POINT('Ctrl Pts',(0.751927443845804,54.4704648228739,0.90667547904812));
#42820=CARTESIAN_POINT('Ctrl Pts',(0.737219192660802,54.4692245407684,0.918674643985659));
#42821=CARTESIAN_POINT('Ctrl Pts',(0.713407547253337,54.4672320583351,0.937160298928722));
#42822=CARTESIAN_POINT('Ctrl Pts',(0.704490340064837,54.4664892138377,0.943881931515761));
#42823=CARTESIAN_POINT('Ctrl Pts',(0.68734329257481,54.4650662011728,0.956428718205439));
#42824=CARTESIAN_POINT('Ctrl Pts',(0.679131552459769,54.4643870157674,0.962276996676362));
#42825=CARTESIAN_POINT('Ctrl Pts',(0.660020805452485,54.4628110531842,0.975520918261391));
#42826=CARTESIAN_POINT('Ctrl Pts',(0.649070973082307,54.4619114963118,0.982840461512534));
#42827=CARTESIAN_POINT('Ctrl Pts',(0.612695893329041,54.4589330231006,1.00628282084194));
#42828=CARTESIAN_POINT('Ctrl Pts',(0.586776890231113,54.4568258196721,1.02161341641516));
#42829=CARTESIAN_POINT('Ctrl Pts',(0.520339466511532,54.4514596410861,1.0575471570204));
#42830=CARTESIAN_POINT('Ctrl Pts',(0.479164326107252,54.4481638963685,1.07682868089076));
#42831=CARTESIAN_POINT('Ctrl Pts',(0.368592864083023,54.4394435625942,1.12100762906506));
#42832=CARTESIAN_POINT('Ctrl Pts',(0.297789053653392,54.4339796611412,1.14185877667398));
#42833=CARTESIAN_POINT('Ctrl Pts',(0.21334758840768,54.4278627005996,1.15833118914294));
#42834=CARTESIAN_POINT('Ctrl Pts',(0.201159235894327,54.4269895694131,1.16050993821474));
#42835=CARTESIAN_POINT('Ctrl Pts',(0.188938462297913,54.4261253209981,1.16249615911817));
#42836=CARTESIAN_POINT('Origin',(0.,56.5393671147362,0.));
#42837=CARTESIAN_POINT('',(0.188938462962337,53.8275149312419,1.16249615901018));
#42838=CARTESIAN_POINT('',(0.188938426235786,53.9273245270844,1.16249616497928));
#42839=CARTESIAN_POINT('',(0.188938462403162,56.5393671147362,1.16249615910107));
#42840=CARTESIAN_POINT('',(-1.17774998792321,54.1906328852639,0.000168662017078135));
#42841=CARTESIAN_POINT('Ctrl Pts',(0.188938462962337,53.8275149312419,1.16249615901018));
#42842=CARTESIAN_POINT('Ctrl Pts',(0.189897639249771,53.8275777423717,1.16234026576955));
#42843=CARTESIAN_POINT('Ctrl Pts',(0.190856653239826,53.8276405882925,1.16218318042302));
#42844=CARTESIAN_POINT('Ctrl Pts',(0.210455175505641,53.828925852409,1.15894805147591));
#42845=CARTESIAN_POINT('Ctrl Pts',(0.229017209989778,53.8301605467417,1.15542330758652));
#42846=CARTESIAN_POINT('Ctrl Pts',(0.258387312155716,53.8321463248688,1.14911069794213));
#42847=CARTESIAN_POINT('Ctrl Pts',(0.269254828374231,53.8328881692897,1.14661293477084));
#42848=CARTESIAN_POINT('Ctrl Pts',(0.289884212587121,53.8343107124266,1.14156208239429));
#42849=CARTESIAN_POINT('Ctrl Pts',(0.299651983091371,53.8349904484463,1.13903710330027));
#42850=CARTESIAN_POINT('Ctrl Pts',(0.322133920444049,53.836569853095,1.13291630709004));
#42851=CARTESIAN_POINT('Ctrl Pts',(0.334822206125474,53.837472338609,1.12923145851975));
#42852=CARTESIAN_POINT('Ctrl Pts',(0.3764559888895,53.8404717192991,1.11637708415354));
#42853=CARTESIAN_POINT('Ctrl Pts',(0.405106892572755,53.8425974539408,1.10630241004607));
#42854=CARTESIAN_POINT('Ctrl Pts',(0.476148948615423,53.8480272187007,1.07819169208433));
#42855=CARTESIAN_POINT('Ctrl Pts',(0.51792920499476,53.8513692073833,1.0587557666041));
#42856=CARTESIAN_POINT('Ctrl Pts',(0.624846357842988,53.8602658250449,1.00117299845565));
#42857=CARTESIAN_POINT('Ctrl Pts',(0.687647566758462,53.8658603700334,0.959125839624569));
#42858=CARTESIAN_POINT('Ctrl Pts',(0.756981068135981,53.8722076462129,0.902372484951482));
#42859=CARTESIAN_POINT('Ctrl Pts',(0.767799334606846,53.8732030540073,0.89318568358655));
#42860=CARTESIAN_POINT('Ctrl Pts',(0.783668183433016,53.8746675084701,0.879208510087267));
#42861=CARTESIAN_POINT('Ctrl Pts',(0.788846230534145,53.8751460712782,0.874565638840407));
#42862=CARTESIAN_POINT('Ctrl Pts',(0.79775202792912,53.8759699302324,0.866436844092695));
#42863=CARTESIAN_POINT('Ctrl Pts',(0.801498575625582,53.8763167242912,0.862972269783275));
#42864=CARTESIAN_POINT('Ctrl Pts',(0.810441151674094,53.8771450615838,0.854594252444472));
#42865=CARTESIAN_POINT('Ctrl Pts',(0.815615113787397,53.8776248520316,0.849657689516876));
#42866=CARTESIAN_POINT('Ctrl Pts',(0.831685292066203,53.8791180043831,0.834042790325199));
#42867=CARTESIAN_POINT('Ctrl Pts',(0.842419658972177,53.880119689121,0.823199230203634));
#42868=CARTESIAN_POINT('Ctrl Pts',(0.867930019453822,53.8825201866217,0.7964075761164));
#42869=CARTESIAN_POINT('Ctrl Pts',(0.882481348775273,53.8839065432435,0.780252730743327));
#42870=CARTESIAN_POINT('Ctrl Pts',(0.946069181071393,53.8900931502315,0.705601441695176));
#42871=CARTESIAN_POINT('Ctrl Pts',(0.98979692783405,53.8947207961409,0.642824522778941));
#42872=CARTESIAN_POINT('Ctrl Pts',(1.04983483772091,53.902384688117,0.535810188895795));
#42873=CARTESIAN_POINT('Ctrl Pts',(1.07011476638204,53.9053231991769,0.494064195936099));
#42874=CARTESIAN_POINT('Ctrl Pts',(1.0938613077573,53.9093623800676,0.436813734239895));
#42875=CARTESIAN_POINT('Ctrl Pts',(1.09955522464394,53.9103885928817,0.422276058150287));
#42876=CARTESIAN_POINT('Ctrl Pts',(1.10822674474456,53.9120510285451,0.398770263743154));
#42877=CARTESIAN_POINT('Ctrl Pts',(1.11138844363077,53.9126810824535,0.389871721903961));
#42878=CARTESIAN_POINT('Ctrl Pts',(1.11775903401152,53.9140026823846,0.371234334629821));
#42879=CARTESIAN_POINT('Ctrl Pts',(1.12094842104168,53.914694809176,0.361489716459661));
#42880=CARTESIAN_POINT('Ctrl Pts',(1.12828375179494,53.9163631632894,0.338046812101474));
#42881=CARTESIAN_POINT('Ctrl Pts',(1.13230793958074,53.9173432638144,0.324312457399663));
#42882=CARTESIAN_POINT('Ctrl Pts',(1.14623074235185,53.9209898976618,0.273372088435909));
#42883=CARTESIAN_POINT('Ctrl Pts',(1.15455269352216,53.9237055268266,0.235764122619588));
#42884=CARTESIAN_POINT('Ctrl Pts',(1.17284800863217,53.9315212581504,0.128387594307932));
#42885=CARTESIAN_POINT('Ctrl Pts',(1.17842512749248,53.9367233397907,0.0580386173100602));
#42886=CARTESIAN_POINT('Ctrl Pts',(1.17719406156194,53.9453055518037,-0.0590789737077564));
#42887=CARTESIAN_POINT('Ctrl Pts',(1.17392578973604,53.9486985923327,-0.105713439042868));
#42888=CARTESIAN_POINT('Ctrl Pts',(1.16656638533144,53.9526978841541,-0.162246666670006));
#42889=CARTESIAN_POINT('Ctrl Pts',(1.16510308156413,53.9534144184061,-0.172441119994811));
#42890=CARTESIAN_POINT('Ctrl Pts',(1.16255042512915,53.9545487457405,-0.188704972689162));
#42891=CARTESIAN_POINT('Ctrl Pts',(1.16154684606806,53.954970962947,-0.194787028516905));
#42892=CARTESIAN_POINT('Ctrl Pts',(1.15948547955847,53.9557934887811,-0.206696784265587));
#42893=CARTESIAN_POINT('Ctrl Pts',(1.15843140720323,53.9561939650385,-0.212524857710682));
#42894=CARTESIAN_POINT('Ctrl Pts',(1.15563649841637,53.9572073230373,-0.22733922774901));
#42895=CARTESIAN_POINT('Ctrl Pts',(1.1538347394827,53.9578168939249,-0.236313875792791));
#42896=CARTESIAN_POINT('Ctrl Pts',(1.14554327633093,53.9604466462181,-0.275255822113258));
#42897=CARTESIAN_POINT('Ctrl Pts',(1.13798883547569,53.9624150798674,-0.304986758619145));
#42898=CARTESIAN_POINT('Ctrl Pts',(1.10968073766334,53.968715581962,-0.400586741195724));
#42899=CARTESIAN_POINT('Ctrl Pts',(1.08429662152824,53.9729174156476,-0.464933195086711));
#42900=CARTESIAN_POINT('Ctrl Pts',(1.02914757691913,53.9805815446967,-0.575235967531483));
#42901=CARTESIAN_POINT('Ctrl Pts',(1.0015503143283,53.9839992066261,-0.622042691239074));
#42902=CARTESIAN_POINT('Ctrl Pts',(0.961733264705776,53.9885776501915,-0.680016297896189));
#42903=CARTESIAN_POINT('Ctrl Pts',(0.952370572936345,53.9896324951966,-0.693068026083361));
#42904=CARTESIAN_POINT('Ctrl Pts',(0.936403532666097,53.9913990266495,-0.714391627175366));
#42905=CARTESIAN_POINT('Ctrl Pts',(0.929949172021173,53.9921048629762,-0.722773476273312));
#42906=CARTESIAN_POINT('Ctrl Pts',(0.916959915571681,53.9935100108338,-0.73917971222927));
#42907=CARTESIAN_POINT('Ctrl Pts',(0.910430427055062,53.9942090658191,-0.747207172953837));
#42908=CARTESIAN_POINT('Ctrl Pts',(0.894276147606383,53.9959217233004,-0.766541381636501));
#42909=CARTESIAN_POINT('Ctrl Pts',(0.884541892172662,53.9969397356197,-0.77775389653972));
#42910=CARTESIAN_POINT('Ctrl Pts',(0.845521438562907,54.0009686764683,-0.82101980216904));
#42911=CARTESIAN_POINT('Ctrl Pts',(0.814687195453629,54.0040435141677,-0.851624325514253));
#42912=CARTESIAN_POINT('Ctrl Pts',(0.710896694080237,54.0140539845682,-0.943836736078548));
#42913=CARTESIAN_POINT('Ctrl Pts',(0.632124065275281,54.0211944805238,-0.998308210793504));
#42914=CARTESIAN_POINT('Ctrl Pts',(0.529841482324578,54.029471477815,-1.05203021150768));
#42915=CARTESIAN_POINT('Ctrl Pts',(0.511797970141039,54.0308959709475,-1.06092531016591));
#42916=CARTESIAN_POINT('Ctrl Pts',(0.486152891062619,54.0328626275226,-1.07276116602866));
#42917=CARTESIAN_POINT('Ctrl Pts',(0.478736169437238,54.0334247295666,-1.07609146561457));
#42918=CARTESIAN_POINT('Ctrl Pts',(0.466023960516743,54.0343761194926,-1.08164212659122));
#42919=CARTESIAN_POINT('Ctrl Pts',(0.460745751650601,54.0347676208057,-1.08390100101109));
#42920=CARTESIAN_POINT('Ctrl Pts',(0.449413118188616,54.0356004802199,-1.08865319410042));
#42921=CARTESIAN_POINT('Ctrl Pts',(0.443354135738027,54.0360411598537,-1.09113475029357));
#42922=CARTESIAN_POINT('Ctrl Pts',(0.426018833533182,54.0372897611191,-1.09806646646584));
#42923=CARTESIAN_POINT('Ctrl Pts',(0.414693713260905,54.0380908266133,-1.10239337977651));
#42924=CARTESIAN_POINT('Ctrl Pts',(0.388371010323977,54.0399235558791,-1.11198723577751));
#42925=CARTESIAN_POINT('Ctrl Pts',(0.373329373250857,54.0409492750934,-1.11712706667121));
#42926=CARTESIAN_POINT('Ctrl Pts',(0.319456235713969,54.04456211242,-1.13432613821075));
#42927=CARTESIAN_POINT('Ctrl Pts',(0.280107927518546,54.0470902970624,-1.14467814619456));
#42928=CARTESIAN_POINT('Ctrl Pts',(0.154906839829029,54.055003386667,-1.17077231023223));
#42929=CARTESIAN_POINT('Ctrl Pts',(0.0678091864489637,54.0603401839508,
-1.17902679397471));
#42930=CARTESIAN_POINT('Ctrl Pts',(-0.0378399366511146,54.0671831874009,
-1.17728645156745));
#42931=CARTESIAN_POINT('Ctrl Pts',(-0.0562710430862497,54.0683894806049,
-1.17654951407345));
#42932=CARTESIAN_POINT('Ctrl Pts',(-0.0857139400172132,54.0703405302249,
-1.17467889257891));
#42933=CARTESIAN_POINT('Ctrl Pts',(-0.0967406618192752,54.0710766219033,
-1.17382222267476));
#42934=CARTESIAN_POINT('Ctrl Pts',(-0.117824370854995,54.0724952218331,
-1.17188513142322));
#42935=CARTESIAN_POINT('Ctrl Pts',(-0.1278827478363,54.0731768677523,-1.17083019064873));
#42936=CARTESIAN_POINT('Ctrl Pts',(-0.151236721471257,54.0747714773031,
-1.16807626244645));
#42937=CARTESIAN_POINT('Ctrl Pts',(-0.16451914798825,54.07568743791,-1.16627960829197));
#42938=CARTESIAN_POINT('Ctrl Pts',(-0.20903954864328,54.0787893445294,-1.15948189565702));
#42939=CARTESIAN_POINT('Ctrl Pts',(-0.240103667940637,54.0810069530017,
-1.15344948000309));
#42940=CARTESIAN_POINT('Ctrl Pts',(-0.318762068102926,54.0867605798492,
-1.13485948723233));
#42941=CARTESIAN_POINT('Ctrl Pts',(-0.365878828505685,54.0903410072869,
-1.12055663477398));
#42942=CARTESIAN_POINT('Ctrl Pts',(-0.481249871133808,54.0993759852731,
-1.07748044935363));
#42943=CARTESIAN_POINT('Ctrl Pts',(-0.547953889721088,54.1048529763452,
-1.04513810374041));
#42944=CARTESIAN_POINT('Ctrl Pts',(-0.621361526312065,54.1109060948869,
-1.00057313229331));
#42945=CARTESIAN_POINT('Ctrl Pts',(-0.631442418895626,54.1117376620866,
-0.994242042129243));
#42946=CARTESIAN_POINT('Ctrl Pts',(-0.646937649859022,54.1130143064882,
-0.984179824575021));
#42947=CARTESIAN_POINT('Ctrl Pts',(-0.652419349300206,54.1134656328785,
-0.980554561363219));
#42948=CARTESIAN_POINT('Ctrl Pts',(-0.662626985096187,54.11430505645,-0.973680350341557));
#42949=CARTESIAN_POINT('Ctrl Pts',(-0.667359744904649,54.114693791915,-0.970442640431005));
#42950=CARTESIAN_POINT('Ctrl Pts',(-0.678705322247402,54.1156249069678,
-0.962558806067729));
#42951=CARTESIAN_POINT('Ctrl Pts',(-0.685294277562477,54.1161650456547,
-0.957878975610734));
#42952=CARTESIAN_POINT('Ctrl Pts',(-0.70893767622444,54.1181031128308,-0.940717309300394));
#42953=CARTESIAN_POINT('Ctrl Pts',(-0.725704601582507,54.119477274236,-0.927844084599255));
#42954=CARTESIAN_POINT('Ctrl Pts',(-0.76936795765327,54.12308220813,-0.892412247099435));
#42955=CARTESIAN_POINT('Ctrl Pts',(-0.795618617882556,54.125277781174,-0.869090335595293));
#42956=CARTESIAN_POINT('Ctrl Pts',(-0.886613703514892,54.1331534953056,
-0.780663561580546));
#42957=CARTESIAN_POINT('Ctrl Pts',(-0.944729291851585,54.1387334805242,
-0.709228374402788));
#42958=CARTESIAN_POINT('Ctrl Pts',(-1.00481623244013,54.145959319556,-0.61469414260531));
#42959=CARTESIAN_POINT('Ctrl Pts',(-1.01522867198601,54.1472785103206,-0.597340116843526));
#42960=CARTESIAN_POINT('Ctrl Pts',(-1.03086601720554,54.1493748299363,-0.569687069983775));
#42961=CARTESIAN_POINT('Ctrl Pts',(-1.03639561436579,54.1501410202253,-0.559564310671721));
#42962=CARTESIAN_POINT('Ctrl Pts',(-1.04645097994152,54.151583007999,-0.540495958099178));
#42963=CARTESIAN_POINT('Ctrl Pts',(-1.05101296456143,54.15225744378,-0.531570570760875));
#42964=CARTESIAN_POINT('Ctrl Pts',(-1.06103623641148,54.153786547287,-0.511326783209443));
#42965=CARTESIAN_POINT('Ctrl Pts',(-1.06643132925464,54.1546434279743,-0.499977172202175));
#42966=CARTESIAN_POINT('Ctrl Pts',(-1.08258753978806,54.1573189034295,-0.464537769734686));
#42967=CARTESIAN_POINT('Ctrl Pts',(-1.09272091758728,54.1591583261945,-0.440172608069373));
#42968=CARTESIAN_POINT('Ctrl Pts',(-1.11514324121102,54.1636503044806,-0.380700552506169));
#42969=CARTESIAN_POINT('Ctrl Pts',(-1.12660365050337,54.1663254443192,-0.345313111725471));
#42970=CARTESIAN_POINT('Ctrl Pts',(-1.16059464478777,54.1757412837487,-0.220488715912945));
#42971=CARTESIAN_POINT('Ctrl Pts',(-1.17428946966783,54.1826340072538,-0.128996109111037));
#42972=CARTESIAN_POINT('Ctrl Pts',(-1.17741520442044,54.1896916024278,-0.0291228858599911));
#42973=CARTESIAN_POINT('Ctrl Pts',(-1.17758086629596,54.1902340427651,-0.0214013192409408));
#42974=CARTESIAN_POINT('Ctrl Pts',(-1.17772387952764,54.1910933528807,-0.00908834702228301));
#42975=CARTESIAN_POINT('Ctrl Pts',(-1.1777503576629,54.1914124590411,-0.00449788311559384));
#42976=CARTESIAN_POINT('Ctrl Pts',(-1.17774999635204,54.1917302397619,9.26971843876522E-5));
#42977=CARTESIAN_POINT('Ctrl Pts',(0.188938462403164,54.3284116054606,1.16249615910106));
#42978=CARTESIAN_POINT('Ctrl Pts',(0.142620439045754,54.3252454416958,1.17002414622273));
#42979=CARTESIAN_POINT('Ctrl Pts',(0.0958081067186543,54.3220792779311,
1.17478673301896));
#42980=CARTESIAN_POINT('Ctrl Pts',(0.0488592103140385,54.3189131141663,
1.17673609618618));
#42981=CARTESIAN_POINT('Ctrl Pts',(0.00192930161990609,54.3157482309045,
1.17868467096547));
#42982=CARTESIAN_POINT('Ctrl Pts',(-0.045136504388877,54.3125833476426,
1.17782225392417));
#42983=CARTESIAN_POINT('Ctrl Pts',(-0.0919770848434641,54.3094184643808,
1.17415300466494));
#42984=CARTESIAN_POINT('Ctrl Pts',(-0.138855738355257,54.3062510086321,
1.17048077295896));
#42985=CARTESIAN_POINT('Ctrl Pts',(-0.185508242064195,54.3030835528833,
1.16399718778063));
#42986=CARTESIAN_POINT('Ctrl Pts',(-0.231577150488323,54.2999160971346,
1.15475845347489));
#42987=CARTESIAN_POINT('Ctrl Pts',(-0.277662214602198,54.2967475306056,
1.14551647928067));
#42988=CARTESIAN_POINT('Ctrl Pts',(-0.323162732754152,54.2935789640766,
1.13351756687537));
#42989=CARTESIAN_POINT('Ctrl Pts',(-0.367733709969507,54.2904103975476,
1.11886861652835));
#42990=CARTESIAN_POINT('Ctrl Pts',(-0.41239551487649,54.2872353740459,1.10418981423668));
#42991=CARTESIAN_POINT('Ctrl Pts',(-0.456123470704711,54.2840603505442,
1.08685038516034));
#42992=CARTESIAN_POINT('Ctrl Pts',(-0.498591310827326,54.2808853270425,
1.06700598277024));
#42993=CARTESIAN_POINT('Ctrl Pts',(-0.538836880772404,54.2778764471455,
1.04820000436156));
#42994=CARTESIAN_POINT('Ctrl Pts',(-0.577950596968587,54.2748675672485,
1.02714495758135));
#42995=CARTESIAN_POINT('Ctrl Pts',(-0.615678010633159,54.2718586873515,
1.00400978567083));
#42996=CARTESIAN_POINT('Ctrl Pts',(-0.657146956306185,54.2685514085093,
0.978580234744731));
#42997=CARTESIAN_POINT('Ctrl Pts',(-0.697135041118901,54.265244129667,0.950517495602211));
#42998=CARTESIAN_POINT('Ctrl Pts',(-0.735290338731114,54.2619368508247,
0.920023467238028));
#42999=CARTESIAN_POINT('Ctrl Pts',(-0.771863516366453,54.2587667092151,
0.890793882200711));
#43000=CARTESIAN_POINT('Ctrl Pts',(-0.806752426714082,54.2555965676055,
0.859331067332825));
#43001=CARTESIAN_POINT('Ctrl Pts',(-0.839674531761361,54.2524264259959,
0.825858185895944));
#43002=CARTESIAN_POINT('Ctrl Pts',(-0.872563586789607,54.249259466845,0.792418907394446));
#43003=CARTESIAN_POINT('Ctrl Pts',(-0.903489354314715,54.2460925076942,
0.756973952151734));
#43004=CARTESIAN_POINT('Ctrl Pts',(-0.932203886321935,54.2429255485433,
0.719785368583081));
#43005=CARTESIAN_POINT('Ctrl Pts',(-0.960902280072749,54.2397603692995,
0.682617685891267));
#43006=CARTESIAN_POINT('Ctrl Pts',(-0.987391559186291,54.2365951900557,
0.643708757115702));
#43007=CARTESIAN_POINT('Ctrl Pts',(-1.01146387124962,54.2334300108119,0.603353875977221));
#43008=CARTESIAN_POINT('Ctrl Pts',(-1.03553329001047,54.2302652119977,0.56300384517789));
#43009=CARTESIAN_POINT('Ctrl Pts',(-1.05718603420786,54.2271004131836,0.521208687330514));
#43010=CARTESIAN_POINT('Ctrl Pts',(-1.07625891199395,54.2239356143694,0.478290515119833));
#43011=CARTESIAN_POINT('Ctrl Pts',(-1.09535123507961,54.2207675889598,0.435328586705968));
#43012=CARTESIAN_POINT('Ctrl Pts',(-1.11185821763891,54.2175995635501,0.391241871058178));
#43013=CARTESIAN_POINT('Ctrl Pts',(-1.12566461737596,54.2144315381405,0.34637296616197));
#43014=CARTESIAN_POINT('Ctrl Pts',(-1.13947937780136,54.2112615942819,0.301476890175686));
#43015=CARTESIAN_POINT('Ctrl Pts',(-1.15059016927694,54.2080916504233,0.255798225177934));
#43016=CARTESIAN_POINT('Ctrl Pts',(-1.15893246591963,54.2049217065648,0.209691683043087));
#43017=CARTESIAN_POINT('Ctrl Pts',(-1.16729001659346,54.20174596641,0.163500834312681));
#43018=CARTESIAN_POINT('Ctrl Pts',(-1.17286891050182,54.1985702262552,0.116881101938893));
#43019=CARTESIAN_POINT('Ctrl Pts',(-1.17565645391774,54.1953944861004,0.0701923419010722));
#43020=CARTESIAN_POINT('Ctrl Pts',(-1.17650802651979,54.1944243224461,0.0559292927071424));
#43021=CARTESIAN_POINT('Ctrl Pts',(-1.17709946320061,54.1934541587918,0.0416597915932341));
#43022=CARTESIAN_POINT('Ctrl Pts',(-1.17743136929669,54.1924839951374,0.0273940339511899));
#43023=CARTESIAN_POINT('Ctrl Pts',(-1.17764246586402,54.1918669585129,0.0183208276915143));
#43024=CARTESIAN_POINT('Ctrl Pts',(-1.17774868810365,54.1912499218884,0.00924517196348502));
#43025=CARTESIAN_POINT('Ctrl Pts',(-1.17774998792321,54.1906328852639,0.000168662017078135));
#43026=CARTESIAN_POINT('',(-1.17774941770936,54.2897919344015,-0.00103887450448897));
#43027=CARTESIAN_POINT('Ctrl Pts',(0.188938462297913,54.4261253209981,1.16249615911817));
#43028=CARTESIAN_POINT('Ctrl Pts',(0.185376180620387,54.425873397806,1.16307513051274));
#43029=CARTESIAN_POINT('Ctrl Pts',(0.181811144134491,54.425622229853,1.16363774305742));
#43030=CARTESIAN_POINT('Ctrl Pts',(0.171047631672032,54.4248668821963,1.16528570060094));
#43031=CARTESIAN_POINT('Ctrl Pts',(0.163841499062352,54.4243651883774,1.16632072195973));
#43032=CARTESIAN_POINT('Ctrl Pts',(0.15101447896241,54.423479828719,1.16804184246133));
#43033=CARTESIAN_POINT('Ctrl Pts',(0.145397663283163,54.4230947836953,1.16875431203914));
#43034=CARTESIAN_POINT('Ctrl Pts',(0.132700621743155,54.4222303119995,1.17027192436718));
#43035=CARTESIAN_POINT('Ctrl Pts',(0.125617954789526,54.4217521811564,1.17105335826282));
#43036=CARTESIAN_POINT('Ctrl Pts',(0.103484336285499,54.4202695266035,1.1732922459694));
#43037=CARTESIAN_POINT('Ctrl Pts',(0.0884114918252079,54.419276450186,1.17452422811808));
#43038=CARTESIAN_POINT('Ctrl Pts',(0.0518891585044232,54.4169012084991,
1.1768022649539));
#43039=CARTESIAN_POINT('Ctrl Pts',(0.0304262537657303,54.4155311560299,
1.17755271824888));
#43040=CARTESIAN_POINT('Ctrl Pts',(-0.0650964392275349,54.4095016859618,
1.17827893604401));
#43041=CARTESIAN_POINT('Ctrl Pts',(-0.139037098298981,54.4050066306922,
1.17185685984141));
#43042=CARTESIAN_POINT('Ctrl Pts',(-0.260121184046763,54.3973314172581,
1.14971140316739));
#43043=CARTESIAN_POINT('Ctrl Pts',(-0.307751589403153,54.3942302627828,
1.1378872943589));
#43044=CARTESIAN_POINT('Ctrl Pts',(-0.369425438285785,54.3900159468323,
1.1184206564918));
#43045=CARTESIAN_POINT('Ctrl Pts',(-0.38425168999655,54.3889874537364,1.11341390332088));
#43046=CARTESIAN_POINT('Ctrl Pts',(-0.407862428420751,54.3873224371346,
1.10491292101191));
#43047=CARTESIAN_POINT('Ctrl Pts',(-0.416712554673629,54.3866921232087,
1.10160562882828));
#43048=CARTESIAN_POINT('Ctrl Pts',(-0.435074383660631,54.3853708587132,
1.09449088486819));
#43049=CARTESIAN_POINT('Ctrl Pts',(-0.444578073351309,54.3846793375231,
1.09066509136458));
#43050=CARTESIAN_POINT('Ctrl Pts',(-0.467201290406765,54.3830141593227,
1.081213101225));
#43051=CARTESIAN_POINT('Ctrl Pts',(-0.480270527937359,54.3820366636617,
1.07547152662546));
#43052=CARTESIAN_POINT('Ctrl Pts',(-0.527927316456104,54.3784130333616,
1.05349306064364));
#43053=CARTESIAN_POINT('Ctrl Pts',(-0.561820055704959,54.3757186155543,
1.03581491958072));
#43054=CARTESIAN_POINT('Ctrl Pts',(-0.654628921373838,54.3680053718203,
0.981510318193043));
#43055=CARTESIAN_POINT('Ctrl Pts',(-0.711254551174165,54.3628881865809,
0.94128473991522));
#43056=CARTESIAN_POINT('Ctrl Pts',(-0.800625837446264,54.354279080706,0.865105996390099));
#43057=CARTESIAN_POINT('Ctrl Pts',(-0.835300330812887,54.3507797944047,
0.831675681964896));
#43058=CARTESIAN_POINT('Ctrl Pts',(-0.874820721918252,54.3466785023147,
0.788600366502111));
#43059=CARTESIAN_POINT('Ctrl Pts',(-0.881706122671819,54.3459594715222,
0.780894464870655));
#43060=CARTESIAN_POINT('Ctrl Pts',(-0.8925398794021,54.3448222253155,0.768443686994296));
#43061=CARTESIAN_POINT('Ctrl Pts',(-0.896553730750785,54.3443995462266,
0.76375686490986));
#43062=CARTESIAN_POINT('Ctrl Pts',(-0.904342679677277,54.3435770595897,
0.754515980927527));
#43063=CARTESIAN_POINT('Ctrl Pts',(-0.908120615428342,54.3431770737615,
0.749964664452561));
#43064=CARTESIAN_POINT('Ctrl Pts',(-0.917636548614925,54.3421663367944,
0.738323380282736));
#43065=CARTESIAN_POINT('Ctrl Pts',(-0.923326923162854,54.3415588634717,
0.731194676570492));
#43066=CARTESIAN_POINT('Ctrl Pts',(-0.947539097564128,54.3389570901951,
0.700129061481728));
#43067=CARTESIAN_POINT('Ctrl Pts',(-0.965218758468685,54.3370131589482,
0.675547280251889));
#43068=CARTESIAN_POINT('Ctrl Pts',(-1.0189961486538,54.3308555319913,0.594346247301076));
#43069=CARTESIAN_POINT('Ctrl Pts',(-1.05120880700349,54.3267656687287,0.535314481664691));
#43070=CARTESIAN_POINT('Ctrl Pts',(-1.10103455299137,54.319077839153,0.421940641612684));
#43071=CARTESIAN_POINT('Ctrl Pts',(-1.12006903322628,54.3155129273234,0.368449771993778));
#43072=CARTESIAN_POINT('Ctrl Pts',(-1.13944798249799,54.3107777752394,0.298346159102283));
#43073=CARTESIAN_POINT('Ctrl Pts',(-1.14340375145628,54.3097247232611,0.282807277058497));
#43074=CARTESIAN_POINT('Ctrl Pts',(-1.14943919471797,54.3079605003848,0.25689754720494));
#43075=CARTESIAN_POINT('Ctrl Pts',(-1.15169865576376,54.3072551504005,0.246570488969655));
#43076=CARTESIAN_POINT('Ctrl Pts',(-1.15589418702773,54.3058504427375,0.226076918112123));
#43077=CARTESIAN_POINT('Ctrl Pts',(-1.15783587598494,54.3051513347103,0.215912521342131));
#43078=CARTESIAN_POINT('Ctrl Pts',(-1.16144923896333,54.3037451184607,0.195544409158177));
#43079=CARTESIAN_POINT('Ctrl Pts',(-1.16312098032593,54.3030380800881,0.185341640790745));
#43080=CARTESIAN_POINT('Ctrl Pts',(-1.16791037441324,54.3008219676272,0.153488878645139));
#43081=CARTESIAN_POINT('Ctrl Pts',(-1.17055923453074,54.2992985452284,0.131774227760274));
#43082=CARTESIAN_POINT('Ctrl Pts',(-1.17606481781418,54.2951455311782,0.0730844106249806));
#43083=CARTESIAN_POINT('Ctrl Pts',(-1.17778227202827,54.2924850287514,0.0360301381678281));
#43084=CARTESIAN_POINT('Ctrl Pts',(-1.17774954090924,54.2897920753539,-0.00103989810314145));
#43085=CARTESIAN_POINT('Ctrl Pts',(-1.17774954179877,54.2897921485752,-0.00103889017059593));
#43086=CARTESIAN_POINT('Ctrl Pts',(-1.17766684091552,54.2829813318646,-0.0947936778329939));
#43087=CARTESIAN_POINT('Ctrl Pts',(-1.1663900290375,54.2759661228186,-0.188203459049912));
#43088=CARTESIAN_POINT('Ctrl Pts',(-1.14237450165133,54.2687959593206,-0.286586760639395));
#43089=CARTESIAN_POINT('Ctrl Pts',(-1.14052361246705,54.2682669717101,-0.293866243541163));
#43090=CARTESIAN_POINT('Ctrl Pts',(-1.13614211928704,54.2670673336474,-0.310433240325928));
#43091=CARTESIAN_POINT('Ctrl Pts',(-1.13356699041024,54.2663987622565,-0.319708625680141));
#43092=CARTESIAN_POINT('Ctrl Pts',(-1.12919717017598,54.2653220718467,-0.334731299165248));
#43093=CARTESIAN_POINT('Ctrl Pts',(-1.12747167895214,54.2649102485041,-0.340498031226404));
#43094=CARTESIAN_POINT('Ctrl Pts',(-1.1241393656601,54.2641397040794,-0.35133175256226));
#43095=CARTESIAN_POINT('Ctrl Pts',(-1.12254231801381,54.2637804142805,-0.356401544458406));
#43096=CARTESIAN_POINT('Ctrl Pts',(-1.11813723377616,54.262815385421,-0.370061979057247));
#43097=CARTESIAN_POINT('Ctrl Pts',(-1.11526448272629,54.2622132850362,-0.378631599320267));
#43098=CARTESIAN_POINT('Ctrl Pts',(-1.10342494296863,54.2598334486448,-0.412645394256968));
#43099=CARTESIAN_POINT('Ctrl Pts',(-1.09368310167419,54.2580948566247,-0.437813139174948));
#43100=CARTESIAN_POINT('Ctrl Pts',(-1.05510173312101,54.2518609394231,-0.528138544164643));
#43101=CARTESIAN_POINT('Ctrl Pts',(-1.02123117189314,54.2475273420223,-0.590980661936369));
#43102=CARTESIAN_POINT('Ctrl Pts',(-0.961055019743536,54.2407605611066,
-0.681829436866348));
#43103=CARTESIAN_POINT('Ctrl Pts',(-0.938725412642028,54.2383983666429,
-0.712258684004632));
#43104=CARTESIAN_POINT('Ctrl Pts',(-0.898199303641413,54.2342880710835,
-0.762261748981371));
#43105=CARTESIAN_POINT('Ctrl Pts',(-0.880726642250142,54.2325647806703,
-0.782384417056916));
#43106=CARTESIAN_POINT('Ctrl Pts',(-0.854002632016679,54.2299852158688,
-0.811131032601916));
#43107=CARTESIAN_POINT('Ctrl Pts',(-0.845270117624524,54.2291505713396,
-0.820227075453378));
#43108=CARTESIAN_POINT('Ctrl Pts',(-0.829400471246059,54.2276470829838,
-0.836234764193481));
#43109=CARTESIAN_POINT('Ctrl Pts',(-0.822318654173583,54.2269807031806,
-0.84319970536502));
#43110=CARTESIAN_POINT('Ctrl Pts',(-0.806874662474305,54.225536579457,-0.858009198911631));
#43111=CARTESIAN_POINT('Ctrl Pts',(-0.798484392739496,54.2247575953504,
-0.865822825192788));
#43112=CARTESIAN_POINT('Ctrl Pts',(-0.775211877175748,54.2226110936378,
-0.886869874276522));
#43113=CARTESIAN_POINT('Ctrl Pts',(-0.760106546535356,54.2212332743819,
-0.899849755267083));
#43114=CARTESIAN_POINT('Ctrl Pts',(-0.667105256393696,54.212836440318,-0.975751988598445));
#43115=CARTESIAN_POINT('Ctrl Pts',(-0.581783021004237,54.2054364599915,
-1.02890370264148));
#43116=CARTESIAN_POINT('Ctrl Pts',(-0.463442687413733,54.1959077763105,
-1.08315332096214));
#43117=CARTESIAN_POINT('Ctrl Pts',(-0.435621230752485,54.1937197578759,
-1.09463902671949));
#43118=CARTESIAN_POINT('Ctrl Pts',(-0.394944545698714,54.1906203665715,
-1.10963497540972));
#43119=CARTESIAN_POINT('Ctrl Pts',(-0.382422978309536,54.189679564969,-1.11401241925848));
#43120=CARTESIAN_POINT('Ctrl Pts',(-0.359791593604102,54.1880060280508,
-1.12149759494009));
#43121=CARTESIAN_POINT('Ctrl Pts',(-0.349708896500555,54.1872698815079,
-1.12468242348174));
#43122=CARTESIAN_POINT('Ctrl Pts',(-0.333626868984732,54.1861121242617,
-1.12952506973644));
#43123=CARTESIAN_POINT('Ctrl Pts',(-0.327655197976916,54.1856857809238,
-1.13127178282946));
#43124=CARTESIAN_POINT('Ctrl Pts',(-0.31607999346285,54.1848666231083,-1.13455818043361));
#43125=CARTESIAN_POINT('Ctrl Pts',(-0.310478467253568,54.1844735047832,
-1.13610384661864));
#43126=CARTESIAN_POINT('Ctrl Pts',(-0.296283030140477,54.183485060024,-1.13990805761707));
#43127=CARTESIAN_POINT('Ctrl Pts',(-0.287674346371837,54.1828928142294,
-1.14211098242077));
#43128=CARTESIAN_POINT('Ctrl Pts',(-0.25415706300348,54.1806118060129,-1.15028487721212));
#43129=CARTESIAN_POINT('Ctrl Pts',(-0.229079475087171,54.1789581570558,
-1.15554053134203));
#43130=CARTESIAN_POINT('Ctrl Pts',(-0.13964001280887,54.1731830561818,-1.17125820342098));
#43131=CARTESIAN_POINT('Ctrl Pts',(-0.0746014270614816,54.1692011175891,
-1.17719194484021));
#43132=CARTESIAN_POINT('Ctrl Pts',(0.0539657533508229,54.1612410239696,
-1.17821837426728));
#43133=CARTESIAN_POINT('Ctrl Pts',(0.117263823350239,54.1572777906625,-1.17360923435909));
#43134=CARTESIAN_POINT('Ctrl Pts',(0.195924385368334,54.1520983672329,-1.16145266021968));
#43135=CARTESIAN_POINT('Ctrl Pts',(0.211915515601254,54.1510324683352,-1.15864162656984));
#43136=CARTESIAN_POINT('Ctrl Pts',(0.238253429830621,54.1492526834866,-1.15344829117014));
#43137=CARTESIAN_POINT('Ctrl Pts',(0.248635523393368,54.1485448410872,-1.15125497662715));
#43138=CARTESIAN_POINT('Ctrl Pts',(0.268937176917575,54.1471476578462,-1.1466786424988));
#43139=CARTESIAN_POINT('Ctrl Pts',(0.278858226687779,54.1464587199321,-1.14430642412277));
#43140=CARTESIAN_POINT('Ctrl Pts',(0.30067598604148,54.1449294797133,-1.13878901308675));
#43141=CARTESIAN_POINT('Ctrl Pts',(0.31255660328995,54.1440873680379,-1.13558567026202));
#43142=CARTESIAN_POINT('Ctrl Pts',(0.353973788409239,54.1411176660096,-1.12371927867764));
#43143=CARTESIAN_POINT('Ctrl Pts',(0.383216833466279,54.1389594169493,-1.11408573264574));
#43144=CARTESIAN_POINT('Ctrl Pts',(0.499769225508402,54.1301042297346,-1.07055792370054));
#43145=CARTESIAN_POINT('Ctrl Pts',(0.583265935471028,54.1231377960992,-1.02745337010706));
#43146=CARTESIAN_POINT('Ctrl Pts',(0.689305087021913,54.1138175285663,-0.955584866996923));
#43147=CARTESIAN_POINT('Ctrl Pts',(0.71698698016554,54.1113384961397,-0.934994154527784));
#43148=CARTESIAN_POINT('Ctrl Pts',(0.751068920691356,54.1082630616596,-0.907237663355813));
#43149=CARTESIAN_POINT('Ctrl Pts',(0.758338092624326,54.1076057253709,-0.90117037967133));
#43150=CARTESIAN_POINT('Ctrl Pts',(0.770082427739315,54.1065425021058,-0.891125101673072));
#43151=CARTESIAN_POINT('Ctrl Pts',(0.774601685184035,54.1061330725899,-0.887199597852913));
#43152=CARTESIAN_POINT('Ctrl Pts',(0.783650995858205,54.1053129763408,-0.879217352055635));
#43153=CARTESIAN_POINT('Ctrl Pts',(0.788179936488669,54.1049023953061,-0.875159658234565));
#43154=CARTESIAN_POINT('Ctrl Pts',(0.800009067356065,54.1038289723818,-0.864395061591423));
#43155=CARTESIAN_POINT('Ctrl Pts',(0.807256534274497,54.103170262677,-0.857630593220265));
#43156=CARTESIAN_POINT('Ctrl Pts',(0.841554027662472,54.1000428784993,-0.824798772921333));
#43157=CARTESIAN_POINT('Ctrl Pts',(0.867434589949899,54.0976519162422,-0.797536212529927));
#43158=CARTESIAN_POINT('Ctrl Pts',(0.9429108036744,54.0904066028501,-0.709999835004306));
#43159=CARTESIAN_POINT('Ctrl Pts',(0.987856007182956,54.0856772664437,-0.646004340862252));
#43160=CARTESIAN_POINT('Ctrl Pts',(1.04592810268671,54.0782430386011,-0.542912814058478));
#43161=CARTESIAN_POINT('Ctrl Pts',(1.06389392214581,54.0756722397325,-0.506802858592426));
#43162=CARTESIAN_POINT('Ctrl Pts',(1.08576355994835,54.0720897232812,-0.456533998775625));
#43163=CARTESIAN_POINT('Ctrl Pts',(1.09130798818531,54.0711333354787,-0.443116964730434));
#43164=CARTESIAN_POINT('Ctrl Pts',(1.10035491472776,54.0694849719163,-0.420023729354373));
#43165=CARTESIAN_POINT('Ctrl Pts',(1.10398126968591,54.0687972263755,-0.41039763192229));
#43166=CARTESIAN_POINT('Ctrl Pts',(1.11110790112933,54.0673880949221,-0.390701834518759));
#43167=CARTESIAN_POINT('Ctrl Pts',(1.11459846428922,54.0666664613536,-0.380629664893257));
#43168=CARTESIAN_POINT('Ctrl Pts',(1.12313604720909,54.0648175466932,-0.354869065656975));
#43169=CARTESIAN_POINT('Ctrl Pts',(1.12799123046387,54.0636841156419,-0.339119993665832));
#43170=CARTESIAN_POINT('Ctrl Pts',(1.1502918907072,54.0580437115446,-0.260995113513728));
#43171=CARTESIAN_POINT('Ctrl Pts',(1.16289920877347,54.0533851067073,-0.197364897798639));
#43172=CARTESIAN_POINT('Ctrl Pts',(1.17699257633227,54.0442578329297,-0.0733914807488738));
#43173=CARTESIAN_POINT('Ctrl Pts',(1.1792033450439,54.0398149814453,-0.0133214262186355));
#43174=CARTESIAN_POINT('Ctrl Pts',(1.17568826191117,54.0333922515329,0.0753414138674756));
#43175=CARTESIAN_POINT('Ctrl Pts',(1.17350244581044,54.0313397903894,0.103978449477455));
#43176=CARTESIAN_POINT('Ctrl Pts',(1.1692629829283,54.0287078179411,0.141419778756764));
#43177=CARTESIAN_POINT('Ctrl Pts',(1.16815228031532,54.0280861143389,0.150318792941377));
#43178=CARTESIAN_POINT('Ctrl Pts',(1.16614455091309,54.0270653480333,0.165035075587939));
#43179=CARTESIAN_POINT('Ctrl Pts',(1.16530538651811,54.026663247275,0.170859742831504));
#43180=CARTESIAN_POINT('Ctrl Pts',(1.16349015208585,54.0258416113948,0.182823305420444));
#43181=CARTESIAN_POINT('Ctrl Pts',(1.16250908525541,54.0254223507497,0.188961176377939));
#43182=CARTESIAN_POINT('Ctrl Pts',(1.15973282558278,54.0242987772188,0.205489697610148));
#43183=CARTESIAN_POINT('Ctrl Pts',(1.15784656610734,54.0235993191851,0.215864751958692));
#43184=CARTESIAN_POINT('Ctrl Pts',(1.14450010534135,54.0190319640173,0.284057500630192));
#43185=CARTESIAN_POINT('Ctrl Pts',(1.12885120561852,54.015359904426,0.340977859062479));
#43186=CARTESIAN_POINT('Ctrl Pts',(1.08881848858547,54.0080013848744,0.452950587783391));
#43187=CARTESIAN_POINT('Ctrl Pts',(1.06435286590403,54.004324796566,0.507782009041369));
#43188=CARTESIAN_POINT('Ctrl Pts',(1.02390986872504,53.9989663945658,0.58252028165588));
#43189=CARTESIAN_POINT('Ctrl Pts',(1.01130238315197,53.9973725703271,0.604142920148731));
#43190=CARTESIAN_POINT('Ctrl Pts',(0.987464309694042,53.9944731696427,0.642187080362546));
#43191=CARTESIAN_POINT('Ctrl Pts',(0.976488242108731,53.9931762966754,0.658756895579183));
#43192=CARTESIAN_POINT('Ctrl Pts',(0.958595343158618,53.9911146143098,0.684338201931109));
#43193=CARTESIAN_POINT('Ctrl Pts',(0.951958122199495,53.9903603577457,0.693541292910036));
#43194=CARTESIAN_POINT('Ctrl Pts',(0.939196171379517,53.9889286171827,0.710708463925178));
#43195=CARTESIAN_POINT('Ctrl Pts',(0.933100454427328,53.9882523063521,0.718692910865464));
#43196=CARTESIAN_POINT('Ctrl Pts',(0.918978696362175,53.9867018720004,0.73670769146736));
#43197=CARTESIAN_POINT('Ctrl Pts',(0.910889307869518,53.9858252731211,0.746686489040031));
#43198=CARTESIAN_POINT('Ctrl Pts',(0.884614915766755,53.9830128911505,0.778035226371346));
#43199=CARTESIAN_POINT('Ctrl Pts',(0.865829942521421,53.9810530534614,0.798887128126904));
#43200=CARTESIAN_POINT('Ctrl Pts',(0.780107538218032,53.9723202302185,0.887463923732712));
#43201=CARTESIAN_POINT('Ctrl Pts',(0.705848335542372,53.9652484666891,0.947593454916767));
#43202=CARTESIAN_POINT('Ctrl Pts',(0.603676655810445,53.9564581320075,1.01158955078941));
#43203=CARTESIAN_POINT('Ctrl Pts',(0.581741326487007,53.9546221720533,1.0243613155366));
#43204=CARTESIAN_POINT('Ctrl Pts',(0.54443428749037,53.9516021305551,1.04449794274336));
#43205=CARTESIAN_POINT('Ctrl Pts',(0.529284876625989,53.9504029155016,1.05225578555052));
#43206=CARTESIAN_POINT('Ctrl Pts',(0.507264262148917,53.9487037660767,1.06293631269729));
#43207=CARTESIAN_POINT('Ctrl Pts',(0.500525828748918,53.9481896258823,1.06612594879634));
#43208=CARTESIAN_POINT('Ctrl Pts',(0.489102329775422,53.9473283332711,1.07140107492384));
#43209=CARTESIAN_POINT('Ctrl Pts',(0.484433288588264,53.9469792036017,1.07352025828005));
#43210=CARTESIAN_POINT('Ctrl Pts',(0.473621154818626,53.9461774718036,1.07834275796754));
#43211=CARTESIAN_POINT('Ctrl Pts',(0.467468596476372,53.9457261818297,1.08102415272247));
#43212=CARTESIAN_POINT('Ctrl Pts',(0.449735310626134,53.9444386031246,1.08857292173314));
#43213=CARTESIAN_POINT('Ctrl Pts',(0.43809880857781,53.9436096895887,1.09330797151054));
#43214=CARTESIAN_POINT('Ctrl Pts',(0.36689497933504,53.9386210636272,1.12096229853187));
#43215=CARTESIAN_POINT('Ctrl Pts',(0.305614416407989,53.9346761907162,1.13919717808827));
#43216=CARTESIAN_POINT('Ctrl Pts',(0.225156811893909,53.9295965595726,1.15617373162336));
#43217=CARTESIAN_POINT('Ctrl Pts',(0.207080778897662,53.9284619713002,1.15954752079153));
#43218=CARTESIAN_POINT('Ctrl Pts',(0.188938426235786,53.9273245270844,1.16249616497928));
#43219=CARTESIAN_POINT('Origin',(0.,56.5393671147362,0.));
#43220=CARTESIAN_POINT('',(0.188938471457153,53.3292711974063,1.16249615762954));
#43221=CARTESIAN_POINT('',(0.188938462305883,53.4282524383066,1.16249615911688));
#43222=CARTESIAN_POINT('',(0.188938462403162,56.5393671147362,1.16249615910107));
#43223=CARTESIAN_POINT('Ctrl Pts',(0.188938471457153,53.3292711974063,1.16249615762954));
#43224=CARTESIAN_POINT('Ctrl Pts',(0.272122176233244,53.3345992990564,1.14897645528266));
#43225=CARTESIAN_POINT('Ctrl Pts',(0.353630912953478,53.3396895031084,1.12656498632061));
#43226=CARTESIAN_POINT('Ctrl Pts',(0.471501764327728,53.347635044798,1.08008256925056));
#43227=CARTESIAN_POINT('Ctrl Pts',(0.510067277097042,53.3503336029397,1.06241379436842));
#43228=CARTESIAN_POINT('Ctrl Pts',(0.560646753858215,53.3540648695701,1.03585117118685));
#43229=CARTESIAN_POINT('Ctrl Pts',(0.573569293663219,53.3550357150435,1.0287519938264));
#43230=CARTESIAN_POINT('Ctrl Pts',(0.595312332050345,53.3567013656372,1.0162701272162));
#43231=CARTESIAN_POINT('Ctrl Pts',(0.604201671546006,53.3573917132986,1.01101042163278));
#43232=CARTESIAN_POINT('Ctrl Pts',(0.62207509894178,53.3587995423826,1.00011503653056));
#43233=CARTESIAN_POINT('Ctrl Pts',(0.631054520963015,53.3595171898599,0.994473576190354));
#43234=CARTESIAN_POINT('Ctrl Pts',(0.653548625453581,53.3613420287866,0.979913980767344));
#43235=CARTESIAN_POINT('Ctrl Pts',(0.666957465273019,53.3624550487913,0.970837220814244));
#43236=CARTESIAN_POINT('Ctrl Pts',(0.727329550561807,53.3675856572018,0.928128862192147));
#43237=CARTESIAN_POINT('Ctrl Pts',(0.77195987142941,53.3717214396069,0.891351588655386));
#43238=CARTESIAN_POINT('Ctrl Pts',(0.861436492330174,53.380743753696,0.805841687629467));
#43239=CARTESIAN_POINT('Ctrl Pts',(0.905244603161678,53.385638736311,0.756297388110092));
#43240=CARTESIAN_POINT('Ctrl Pts',(0.96261345677392,53.3926013877805,0.679244526714454));
#43241=CARTESIAN_POINT('Ctrl Pts',(0.979629330804129,53.3947524006647,0.65446504434324));
#43242=CARTESIAN_POINT('Ctrl Pts',(1.00053887171359,53.3974880734876,0.621369277726854));
#43243=CARTESIAN_POINT('Ctrl Pts',(1.00530854957296,53.3981189813882,0.613622478583465));
#43244=CARTESIAN_POINT('Ctrl Pts',(1.01302875683458,53.3991507465524,0.600751813210578));
#43245=CARTESIAN_POINT('Ctrl Pts',(1.01603125284886,53.3995547702384,0.595659720032469));
#43246=CARTESIAN_POINT('Ctrl Pts',(1.02209413131163,53.4003759925294,0.585198120890406));
#43247=CARTESIAN_POINT('Ctrl Pts',(1.02515081279963,53.4007929669845,0.579826758073099));
#43248=CARTESIAN_POINT('Ctrl Pts',(1.03322417193726,53.4019029711945,0.56537638825406));
#43249=CARTESIAN_POINT('Ctrl Pts',(1.03816355853133,53.4025913479283,0.556254522659361));
#43250=CARTESIAN_POINT('Ctrl Pts',(1.06691100482759,53.4066615852118,0.501447702315244));
#43251=CARTESIAN_POINT('Ctrl Pts',(1.08782407739506,53.40989443696,0.454300513866112));
#43252=CARTESIAN_POINT('Ctrl Pts',(1.12108297267133,53.4158838622824,0.363717164501314));
#43253=CARTESIAN_POINT('Ctrl Pts',(1.13415164373756,53.4186438147476,0.320651345897277));
#43254=CARTESIAN_POINT('Ctrl Pts',(1.15346907795142,53.4237473418666,0.24080418526473));
#43255=CARTESIAN_POINT('Ctrl Pts',(1.16049551032288,53.4260770541502,0.204272977605751));
#43256=CARTESIAN_POINT('Ctrl Pts',(1.16953393380883,53.4301377455298,0.14135622124496));
#43257=CARTESIAN_POINT('Ctrl Pts',(1.17240682712747,53.4318447750953,0.115122852564769));
#43258=CARTESIAN_POINT('Ctrl Pts',(1.1753439744265,53.4344048898237,0.0762858000488357));
#43259=CARTESIAN_POINT('Ctrl Pts',(1.1760909993527,53.4352368382902,0.0637410578943533));
#43260=CARTESIAN_POINT('Ctrl Pts',(1.17707277358854,53.4367437142993,0.0411730522257568));
#43261=CARTESIAN_POINT('Ctrl Pts',(1.17738054494792,53.4374162907847,0.0311540722878727));
#43262=CARTESIAN_POINT('Ctrl Pts',(1.17776735006515,53.4388715203704,0.00960038712419998));
#43263=CARTESIAN_POINT('Ctrl Pts',(1.17780488269599,53.4396554034839,-0.00193391429791517));
#43264=CARTESIAN_POINT('Ctrl Pts',(1.17744164016669,53.4418292146908,-0.033700084230902));
#43265=CARTESIAN_POINT('Ctrl Pts',(1.17668888010545,53.443229880684,-0.0539231191577857));
#43266=CARTESIAN_POINT('Ctrl Pts',(1.16858936821251,53.4522381478968,-0.18237491709975));
#43267=CARTESIAN_POINT('Ctrl Pts',(1.14683904003785,53.4603011077607,-0.289159778979795));
#43268=CARTESIAN_POINT('Ctrl Pts',(1.09872354760097,53.4708489978935,-0.425701765814891));
#43269=CARTESIAN_POINT('Ctrl Pts',(1.08506600892611,53.4734659236939,-0.459399284786602));
#43270=CARTESIAN_POINT('Ctrl Pts',(1.06585520517816,53.4766822709934,-0.501138687829624));
#43271=CARTESIAN_POINT('Ctrl Pts',(1.06173298685907,53.4773493246654,-0.509814066628288));
#43272=CARTESIAN_POINT('Ctrl Pts',(1.05485688357332,53.4784242687151,-0.523839866541042));
#43273=CARTESIAN_POINT('Ctrl Pts',(1.052167402681,53.4788358407283,-0.529221136903243));
#43274=CARTESIAN_POINT('Ctrl Pts',(1.04668983548114,53.4796561911237,-0.539974142309233));
#43275=CARTESIAN_POINT('Ctrl Pts',(1.04390134555481,53.4800649295153,-0.545345460215639));
#43276=CARTESIAN_POINT('Ctrl Pts',(1.03650166640205,53.4811273296619,-0.559334314833676));
#43277=CARTESIAN_POINT('Ctrl Pts',(1.03182429099254,53.4817770141004,-0.567916568078174));
#43278=CARTESIAN_POINT('Ctrl Pts',(1.0096743839441,53.4847593968217,-0.607380956792485));
#43279=CARTESIAN_POINT('Ctrl Pts',(0.99091719636382,53.4870229795918,-0.63752458781805));
#43280=CARTESIAN_POINT('Ctrl Pts',(0.925610335424598,53.4942689665555,-0.73261108350359));
#43281=CARTESIAN_POINT('Ctrl Pts',(0.873815855190618,53.4991052731634,-0.793675052818285));
#43282=CARTESIAN_POINT('Ctrl Pts',(0.786891554988415,53.5066783845719,-0.877242265770893));
#43283=CARTESIAN_POINT('Ctrl Pts',(0.756104247766958,53.5092737191256,-0.903912695655278));
#43284=CARTESIAN_POINT('Ctrl Pts',(0.712513635568641,53.5128849694348,-0.937886706854698));
#43285=CARTESIAN_POINT('Ctrl Pts',(0.700862312965438,53.5138443341537,-0.94662513335947));
#43286=CARTESIAN_POINT('Ctrl Pts',(0.680701840180331,53.515496366166,-0.961169126168438));
#43287=CARTESIAN_POINT('Ctrl Pts',(0.67227290828531,53.5161847580772,-0.96708335193797));
#43288=CARTESIAN_POINT('Ctrl Pts',(0.654969256897275,53.5175939318682,-0.978889055636462));
#43289=CARTESIAN_POINT('Ctrl Pts',(0.646090009504519,53.5183149456928,-0.984772155028817));
#43290=CARTESIAN_POINT('Ctrl Pts',(0.623316896738008,53.5201595687942,-0.99942030549462));
#43291=CARTESIAN_POINT('Ctrl Pts',(0.609317595911858,53.5212892674594,-1.00801632941558));
#43292=CARTESIAN_POINT('Ctrl Pts',(0.5395935567445,53.5268980044687,-1.04884595934508));
#43293=CARTESIAN_POINT('Ctrl Pts',(0.481478766636501,53.5315267741778,-1.07676129089872));
#43294=CARTESIAN_POINT('Ctrl Pts',(0.376051356931989,53.5397840076527,-1.1171558187886));
#43295=CARTESIAN_POINT('Ctrl Pts',(0.329689186797785,53.5433686889202,-1.13170524134979));
#43296=CARTESIAN_POINT('Ctrl Pts',(0.24467416959669,53.5497605181276,-1.15271538035918));
#43297=CARTESIAN_POINT('Ctrl Pts',(0.206340645603524,53.5525778105362,-1.16019065214295));
#43298=CARTESIAN_POINT('Ctrl Pts',(0.15802321779594,53.5559967426003,-1.16714153640258));
#43299=CARTESIAN_POINT('Ctrl Pts',(0.148325879528012,53.5566763002715,-1.16841351955232));
#43300=CARTESIAN_POINT('Ctrl Pts',(0.132602410435525,53.5577662551786,-1.17027701981836));
#43301=CARTESIAN_POINT('Ctrl Pts',(0.126585816008528,53.5581805167005,-1.17094309756986));
#43302=CARTESIAN_POINT('Ctrl Pts',(0.115296954872432,53.5589521921319,-1.17210482133907));
#43303=CARTESIAN_POINT('Ctrl Pts',(0.110026010116141,53.5593102126632,-1.17261135065402));
#43304=CARTESIAN_POINT('Ctrl Pts',(0.095869211128407,53.5602660900925,-1.17387549796522));
#43305=CARTESIAN_POINT('Ctrl Pts',(0.0869776545308116,53.5608604349539,
-1.17456778861695));
#43306=CARTESIAN_POINT('Ctrl Pts',(0.0522594913214459,53.5631606741977,
-1.17687449856718));
#43307=CARTESIAN_POINT('Ctrl Pts',(0.026388534705586,53.5648306990101,-1.17773872525583));
#43308=CARTESIAN_POINT('Ctrl Pts',(-0.08856760774046,53.5721384901364,-1.17778831877234));
#43309=CARTESIAN_POINT('Ctrl Pts',(-0.177364091779214,53.5775029464724,
-1.16772154689559));
#43310=CARTESIAN_POINT('Ctrl Pts',(-0.305542190075641,53.5857506853485,
-1.13821807438996));
#43311=CARTESIAN_POINT('Ctrl Pts',(-0.346354223354358,53.5884522341009,
-1.12646996967279));
#43312=CARTESIAN_POINT('Ctrl Pts',(-0.400372419152107,53.5921869724843,
-1.10770686869929));
#43313=CARTESIAN_POINT('Ctrl Pts',(-0.414211732449651,53.5931581412674,
-1.10260654343474));
#43314=CARTESIAN_POINT('Ctrl Pts',(-0.437574669955535,53.5948241761321,
-1.09349447698427));
#43315=CARTESIAN_POINT('Ctrl Pts',(-0.447148141338848,53.5955145796003,
-1.0896147443303));
#43316=CARTESIAN_POINT('Ctrl Pts',(-0.466442657689451,53.5969223750086,
-1.08149837502614));
#43317=CARTESIAN_POINT('Ctrl Pts',(-0.476159970997694,53.5976399311828,
-1.07725538163962));
#43318=CARTESIAN_POINT('Ctrl Pts',(-0.50056202684096,53.5994642321416,-1.066205733092));
#43319=CARTESIAN_POINT('Ctrl Pts',(-0.515165788622925,53.600576798437,-1.05922668609973));
#43320=CARTESIAN_POINT('Ctrl Pts',(-0.581017556140803,53.6056917609705,
-1.0260725713299));
#43321=CARTESIAN_POINT('Ctrl Pts',(-0.630441515002507,53.6098113730722,
-0.996467799001293));
#43322=CARTESIAN_POINT('Ctrl Pts',(-0.731652650436643,53.6188302216918,
-0.925290514198592));
#43323=CARTESIAN_POINT('Ctrl Pts',(-0.782497914598962,53.6237391554934,
-0.882708906811734));
#43324=CARTESIAN_POINT('Ctrl Pts',(-0.8508525149281,53.6307182917934,-0.81489270746091));
#43325=CARTESIAN_POINT('Ctrl Pts',(-0.871391574986299,53.6328721658634,
-0.792891655106744));
#43326=CARTESIAN_POINT('Ctrl Pts',(-0.897017799795665,53.6356108355229,
-0.763241079460414));
#43327=CARTESIAN_POINT('Ctrl Pts',(-0.902888706373137,53.6362419993615,
-0.756286900189999));
#43328=CARTESIAN_POINT('Ctrl Pts',(-0.912439620138181,53.6372740687119,
-0.744703935336704));
#43329=CARTESIAN_POINT('Ctrl Pts',(-0.916166347283998,53.6376781442489,
-0.740114343454668));
#43330=CARTESIAN_POINT('Ctrl Pts',(-0.923237464171409,53.6384471775105,
-0.731270759075751));
#43331=CARTESIAN_POINT('Ctrl Pts',(-0.926587341677578,53.6388125543855,
-0.727021484927079));
#43332=CARTESIAN_POINT('Ctrl Pts',(-0.935767166094992,53.6398172312023,
-0.715210483782094));
#43333=CARTESIAN_POINT('Ctrl Pts',(-0.941534777239932,53.6404523451065,
-0.70760052508435));
#43334=CARTESIAN_POINT('Ctrl Pts',(-0.966000327698649,53.6431675248616,
-0.674491072278882));
#43335=CARTESIAN_POINT('Ctrl Pts',(-0.983761316385715,53.6451933027415,
-0.648312334826286));
#43336=CARTESIAN_POINT('Ctrl Pts',(-1.04440787179169,53.6524430780907,-0.550679476528287));
#43337=CARTESIAN_POINT('Ctrl Pts',(-1.08073537181196,53.6574775114207,-0.47544496596454));
#43338=CARTESIAN_POINT('Ctrl Pts',(-1.12277739658354,53.6653057222121,-0.35802275616099));
#43339=CARTESIAN_POINT('Ctrl Pts',(-1.1346676590225,53.6679436807481,-0.318336520049744));
#43340=CARTESIAN_POINT('Ctrl Pts',(-1.14789995659898,53.6716045335986,-0.26388454087882));
#43341=CARTESIAN_POINT('Ctrl Pts',(-1.15109109409832,53.6725687152649,-0.249596921014044));
#43342=CARTESIAN_POINT('Ctrl Pts',(-1.15607440516219,53.6742264546652,-0.22515179072733));
#43343=CARTESIAN_POINT('Ctrl Pts',(-1.15800102013634,53.6749156608476,-0.215023219551279));
#43344=CARTESIAN_POINT('Ctrl Pts',(-1.16142569030614,53.6762399478473,-0.195635826823854));
#43345=CARTESIAN_POINT('Ctrl Pts',(-1.16294661208628,53.6768742437467,-0.186381810790098));
#43346=CARTESIAN_POINT('Ctrl Pts',(-1.16664739840601,53.678548067993,-0.162052212325414));
#43347=CARTESIAN_POINT('Ctrl Pts',(-1.16864553007423,53.6795932306927,-0.146951211712593));
#43348=CARTESIAN_POINT('Ctrl Pts',(-1.17531675937336,53.6837190752358,-0.0877197370874866));
#43349=CARTESIAN_POINT('Ctrl Pts',(-1.17778661101037,53.6868662939408,-0.0433830430605927));
#43350=CARTESIAN_POINT('Ctrl Pts',(-1.1776841270502,53.6957335960238,0.0794332951306981));
#43351=CARTESIAN_POINT('Ctrl Pts',(-1.16978077091275,53.7015631621963,0.157674418825063));
#43352=CARTESIAN_POINT('Ctrl Pts',(-1.14774802337991,53.7096006058311,0.266093840693275));
#43353=CARTESIAN_POINT('Ctrl Pts',(-1.14004540147492,53.7119115416153,0.297369000529171));
#43354=CARTESIAN_POINT('Ctrl Pts',(-1.12841346325165,53.7148319009299,0.337444739062884));
#43355=CARTESIAN_POINT('Ctrl Pts',(-1.12564572725268,53.7154937153235,0.346565444669406));
#43356=CARTESIAN_POINT('Ctrl Pts',(-1.12113455398268,53.7165215974492,0.3608068938321));
#43357=CARTESIAN_POINT('Ctrl Pts',(-1.11946611731128,53.7168917193444,0.365950704260894));
#43358=CARTESIAN_POINT('Ctrl Pts',(-1.11589856054584,53.7176623032736,0.376696765548133));
#43359=CARTESIAN_POINT('Ctrl Pts',(-1.11399255938596,53.7180623108859,0.382296521762411));
#43360=CARTESIAN_POINT('Ctrl Pts',(-1.10904208910941,53.7190727734424,0.396489358477497));
#43361=CARTESIAN_POINT('Ctrl Pts',(-1.10593980886366,53.7196799561819,0.405062117226059));
#43362=CARTESIAN_POINT('Ctrl Pts',(-1.09211305411378,53.7222808620585,0.441927089171468));
#43363=CARTESIAN_POINT('Ctrl Pts',(-1.08039924296611,53.7242242381574,0.46983857451692));
#43364=CARTESIAN_POINT('Ctrl Pts',(-1.03932202460243,53.7303753252218,0.558029961792834));
#43365=CARTESIAN_POINT('Ctrl Pts',(-1.00588533175447,53.7344595544153,0.616265644429291));
#43366=CARTESIAN_POINT('Ctrl Pts',(-0.935425080538271,53.7421327253014,
0.717827124140434));
#43367=CARTESIAN_POINT('Ctrl Pts',(-0.899871982936977,53.7456887324383,
0.761922022555255));
#43368=CARTESIAN_POINT('Ctrl Pts',(-0.850273572398811,53.7504216825328,
0.815101740249983));
#43369=CARTESIAN_POINT('Ctrl Pts',(-0.839014686615012,53.7514823717284,
0.826686342564799));
#43370=CARTESIAN_POINT('Ctrl Pts',(-0.819981260793099,53.7532559802974,
0.845480980680122));
#43371=CARTESIAN_POINT('Ctrl Pts',(-0.812341044367375,53.7539629484292,
0.852824349968331));
#43372=CARTESIAN_POINT('Ctrl Pts',(-0.797056428333644,53.7553682717022,
0.867123350873446));
#43373=CARTESIAN_POINT('Ctrl Pts',(-0.789417494873166,53.7560663439184,
0.874083441382371));
#43374=CARTESIAN_POINT('Ctrl Pts',(-0.77063784216132,53.7577728415555,0.890747232723807));
#43375=CARTESIAN_POINT('Ctrl Pts',(-0.75940446478982,53.7587856015193,0.900343345846582));
#43376=CARTESIAN_POINT('Ctrl Pts',(-0.715023622868079,53.7627580278213,
0.936834146825534));
#43377=CARTESIAN_POINT('Ctrl Pts',(-0.680607802062416,53.7657792736133,
0.962127463860813));
#43378=CARTESIAN_POINT('Ctrl Pts',(-0.569123416102032,53.7753791976557,
1.0350818136319));
#43379=CARTESIAN_POINT('Ctrl Pts',(-0.487889485123113,53.7821391770667,
1.07575919060754));
#43380=CARTESIAN_POINT('Ctrl Pts',(-0.379801043204749,53.7904295904191,
1.11509880772011));
#43381=CARTESIAN_POINT('Ctrl Pts',(-0.356542863596595,53.7921726735827,
1.12275178044642));
#43382=CARTESIAN_POINT('Ctrl Pts',(-0.324670490678888,53.794491858572,1.13214869207535));
#43383=CARTESIAN_POINT('Ctrl Pts',(-0.316252038783791,53.7950979383177,
1.1345290864782));
#43384=CARTESIAN_POINT('Ctrl Pts',(-0.302222408135289,53.7960963698605,
1.13832779066846));
#43385=CARTESIAN_POINT('Ctrl Pts',(-0.296626003080605,53.7964915871873,
1.139798913425));
#43386=CARTESIAN_POINT('Ctrl Pts',(-0.284943559473161,53.7973099550022,
1.14277799153259));
#43387=CARTESIAN_POINT('Ctrl Pts',(-0.278855953412043,53.7977327042798,
1.14427869500515));
#43388=CARTESIAN_POINT('Ctrl Pts',(-0.262256765872946,53.7988761189345,
1.14823035283336));
#43389=CARTESIAN_POINT('Ctrl Pts',(-0.251722726783744,53.7995916331148,
1.15058560904719));
#43390=CARTESIAN_POINT('Ctrl Pts',(-0.180026926831319,53.8044023807367,
1.16558390113029));
#43391=CARTESIAN_POINT('Ctrl Pts',(-0.117967759443314,53.808278849281,1.17349101941963));
#43392=CARTESIAN_POINT('Ctrl Pts',(0.0262064092789694,53.817201464806,1.18030087155895));
#43393=CARTESIAN_POINT('Ctrl Pts',(0.108148751295267,53.8222244615645,1.17562676922961));
#43394=CARTESIAN_POINT('Ctrl Pts',(0.188938462962337,53.8275149312419,1.16249615901018));
#43395=CARTESIAN_POINT('Ctrl Pts',(0.188938426235786,53.9273245270844,1.16249616497928));
#43396=CARTESIAN_POINT('Ctrl Pts',(0.152659231822772,53.9250499841622,1.1683925576763));
#43397=CARTESIAN_POINT('Ctrl Pts',(0.116114877842513,53.9227633969847,1.17258888333654));
#43398=CARTESIAN_POINT('Ctrl Pts',(0.0456482290779684,53.9182954063845,
1.17735185449536));
#43399=CARTESIAN_POINT('Ctrl Pts',(0.0117913650629317,53.916122848071,1.17817731794005));
#43400=CARTESIAN_POINT('Ctrl Pts',(-0.0357656519651533,53.9130075193054,
1.17728671715397));
#43401=CARTESIAN_POINT('Ctrl Pts',(-0.0494734003468065,53.9121022139423,
1.17679036061967));
#43402=CARTESIAN_POINT('Ctrl Pts',(-0.0733099531465983,53.9105135779761,
1.17551003868362));
#43403=CARTESIAN_POINT('Ctrl Pts',(-0.0834432595663409,53.9098336901031,
1.17483420601588));
#43404=CARTESIAN_POINT('Ctrl Pts',(-0.104454583854328,53.9084139273164,
1.1731596695673));
#43405=CARTESIAN_POINT('Ctrl Pts',(-0.115329942010815,53.9076734727027,
1.17214050386461));
#43406=CARTESIAN_POINT('Ctrl Pts',(-0.143867896688091,53.9057150173803,
1.16906512019708));
#43407=CARTESIAN_POINT('Ctrl Pts',(-0.161500244965537,53.9044893522484,
1.16675997423065));
#43408=CARTESIAN_POINT('Ctrl Pts',(-0.281602355997566,53.896029275183,1.14828404677168));
#43409=CARTESIAN_POINT('Ctrl Pts',(-0.381583162984285,53.888370178109,1.11903625172896));
#43410=CARTESIAN_POINT('Ctrl Pts',(-0.50437070093299,53.8785397948054,1.06472513181056));
#43411=CARTESIAN_POINT('Ctrl Pts',(-0.531835045507651,53.8763157614107,
1.05127594635854));
#43412=CARTESIAN_POINT('Ctrl Pts',(-0.570537534118971,53.8731715720721,
1.03041806824942));
#43413=CARTESIAN_POINT('Ctrl Pts',(-0.582219926352531,53.8722211710787,
1.02386252161253));
#43414=CARTESIAN_POINT('Ctrl Pts',(-0.60298785353048,53.8705324401875,1.01173819910354));
#43415=CARTESIAN_POINT('Ctrl Pts',(-0.61211438444692,53.8697906123593,1.00624278158637));
#43416=CARTESIAN_POINT('Ctrl Pts',(-0.62646580242538,53.8686260524972,0.99733373570745));
#43417=CARTESIAN_POINT('Ctrl Pts',(-0.63174004297222,53.8681984972616,0.994001259880188));
#43418=CARTESIAN_POINT('Ctrl Pts',(-0.641866888005468,53.8673787724929,
0.987489549405691));
#43419=CARTESIAN_POINT('Ctrl Pts',(-0.646722868723927,53.8669862782822,
0.984316130595538));
#43420=CARTESIAN_POINT('Ctrl Pts',(-0.658913118589361,53.8660019372149,
0.976220558450205));
#43421=CARTESIAN_POINT('Ctrl Pts',(-0.666216025571102,53.8654131166064,
0.971251407013234));
#43422=CARTESIAN_POINT('Ctrl Pts',(-0.694113894249522,53.8631642702005,
0.951805987794783));
#43423=CARTESIAN_POINT('Ctrl Pts',(-0.714300078526848,53.8615381041934,
0.936752015663351));
#43424=CARTESIAN_POINT('Ctrl Pts',(-0.804229254726047,53.8542202816923,
0.865087853597262));
#43425=CARTESIAN_POINT('Ctrl Pts',(-0.867839083162592,53.8488136827263,
0.801261030261879));
#43426=CARTESIAN_POINT('Ctrl Pts',(-0.94998998012497,53.8405128830896,0.697442273802732));
#43427=CARTESIAN_POINT('Ctrl Pts',(-0.974570109904326,53.8378039305937,
0.662660705222124));
#43428=CARTESIAN_POINT('Ctrl Pts',(-1.00506484963416,53.8340607525191,0.614131522796961));
#43429=CARTESIAN_POINT('Ctrl Pts',(-1.01268135675169,53.8330889425121,0.601489249140145));
#43430=CARTESIAN_POINT('Ctrl Pts',(-1.02522118955754,53.8314222896792,0.579761389482697));
#43431=CARTESIAN_POINT('Ctrl Pts',(-1.03026629340123,53.8307319214265,0.570747850910221));
#43432=CARTESIAN_POINT('Ctrl Pts',(-1.04024550701023,53.8293246223153,0.552355530816141));
#43433=CARTESIAN_POINT('Ctrl Pts',(-1.04517288060168,53.8286075325064,0.542974202069317));
#43434=CARTESIAN_POINT('Ctrl Pts',(-1.0572941351978,53.8267853134336,0.519119802392274));
#43435=CARTESIAN_POINT('Ctrl Pts',(-1.06431772422427,53.8256743863906,0.504563171442096));
#43436=CARTESIAN_POINT('Ctrl Pts',(-1.09469754669775,53.8206073469156,0.438141128454311));
#43437=CARTESIAN_POINT('Ctrl Pts',(-1.1145741661967,53.8165369645876,0.384776696895595));
#43438=CARTESIAN_POINT('Ctrl Pts',(-1.14714400783415,53.8080723856222,0.273263663605702));
#43439=CARTESIAN_POINT('Ctrl Pts',(-1.15944704481569,53.8036836305903,0.215162088572969));
#43440=CARTESIAN_POINT('Ctrl Pts',(-1.17218381204311,53.7966933668929,0.120087803411154));
#43441=CARTESIAN_POINT('Ctrl Pts',(-1.17535118299592,53.7940555075056,0.0835828638502875));
#43442=CARTESIAN_POINT('Ctrl Pts',(-1.17719623458976,53.7908180035941,0.0373720583644565));
#43443=CARTESIAN_POINT('Ctrl Pts',(-1.17746228524513,53.790149678217,0.0277529719767753));
#43444=CARTESIAN_POINT('Ctrl Pts',(-1.17770307870723,53.7890732826708,0.0121136865822064));
#43445=CARTESIAN_POINT('Ctrl Pts',(-1.17774960635718,53.7886615117446,0.00609524966651524));
#43446=CARTESIAN_POINT('Ctrl Pts',(-1.17775039039683,53.7878413875649,-0.0059687622322643));
#43447=CARTESIAN_POINT('Ctrl Pts',(-1.17770423813461,53.7874330672057,-0.0120141515325746));
#43448=CARTESIAN_POINT('Ctrl Pts',(-1.17746206087186,53.7863727301873,-0.0278062407918057));
#43449=CARTESIAN_POINT('Ctrl Pts',(-1.17719156796747,53.7857246642865,-0.037551559094287));
#43450=CARTESIAN_POINT('Ctrl Pts',(-1.17525224431485,53.782541654558,-0.0858083097293891));
#43451=CARTESIAN_POINT('Ctrl Pts',(-1.17181428826531,53.7800894395291,-0.124228835477599));
#43452=CARTESIAN_POINT('Ctrl Pts',(-1.15975156479247,53.7746092401423,-0.210865653479617));
#43453=CARTESIAN_POINT('Ctrl Pts',(-1.14999344817933,53.7716080262934,-0.258850100305046));
#43454=CARTESIAN_POINT('Ctrl Pts',(-1.1205163643538,53.7645892730672,-0.368372445157435));
#43455=CARTESIAN_POINT('Ctrl Pts',(-1.09866772038034,53.7605603460187,-0.429165452501773));
#43456=CARTESIAN_POINT('Ctrl Pts',(-1.0651429988736,53.7552963894138,-0.502827882172949));
#43457=CARTESIAN_POINT('Ctrl Pts',(-1.05801870236843,53.7542171676749,-0.517650334565637));
#43458=CARTESIAN_POINT('Ctrl Pts',(-1.04577188227245,53.7524212187868,-0.541820739238523));
#43459=CARTESIAN_POINT('Ctrl Pts',(-1.04082850731533,53.7517107690503,-0.551257243864777));
#43460=CARTESIAN_POINT('Ctrl Pts',(-1.03085937737525,53.7503050357582,-0.569675264801677));
#43461=CARTESIAN_POINT('Ctrl Pts',(-1.02584254679098,53.7496101179238,-0.578660540151756));
#43462=CARTESIAN_POINT('Ctrl Pts',(-1.01345363031929,53.7479228740344,-0.600181871574193));
#43463=CARTESIAN_POINT('Ctrl Pts',(-1.00596600388983,53.7469264437929,-0.612649088440841));
#43464=CARTESIAN_POINT('Ctrl Pts',(-0.976737521841124,53.7431205765336,
-0.659334750308995));
#43465=CARTESIAN_POINT('Ctrl Pts',(-0.953467991180597,53.7402561317173,
-0.692558033441009));
#43466=CARTESIAN_POINT('Ctrl Pts',(-0.879892091693928,53.7316561838714,
-0.786852811775211));
#43467=CARTESIAN_POINT('Ctrl Pts',(-0.82509672860188,53.7257876664316,-0.844133320142188));
#43468=CARTESIAN_POINT('Ctrl Pts',(-0.737307943179909,53.7173727795443,
-0.919128390621436));
#43469=CARTESIAN_POINT('Ctrl Pts',(-0.70854791604467,53.7147500030779,-0.941477757666481));
#43470=CARTESIAN_POINT('Ctrl Pts',(-0.670769588615357,53.7115117525278,
-0.968121734872099));
#43471=CARTESIAN_POINT('Ctrl Pts',(-0.662672166575706,53.7108291702538,
-0.97368226348867));
#43472=CARTESIAN_POINT('Ctrl Pts',(-0.649466831398828,53.7097356578704,
-0.982509355671043));
#43473=CARTESIAN_POINT('Ctrl Pts',(-0.644401793562308,53.7093208179043,
-0.985838796015544));
#43474=CARTESIAN_POINT('Ctrl Pts',(-0.634269148771241,53.7085003690883,
-0.992387903478384));
#43475=CARTESIAN_POINT('Ctrl Pts',(-0.629202193099903,53.708094730247,-0.995608210032243));
#43476=CARTESIAN_POINT('Ctrl Pts',(-0.616010497566849,53.707050005927,-1.00385126492851));
#43477=CARTESIAN_POINT('Ctrl Pts',(-0.607848688892706,53.7064146569309,
-1.00881429472247));
#43478=CARTESIAN_POINT('Ctrl Pts',(-0.568973502919236,53.7034357402132,
-1.03181037603517));
#43479=CARTESIAN_POINT('Ctrl Pts',(-0.53751000134393,53.701162556173,-1.04854518690345));
#43480=CARTESIAN_POINT('Ctrl Pts',(-0.411021291326211,53.6923638169503,
-1.10862902721096));
#43481=CARTESIAN_POINT('Ctrl Pts',(-0.311174234656337,53.6861006680883,
-1.14068766067955));
#43482=CARTESIAN_POINT('Ctrl Pts',(-0.18566564894933,53.6779159752707,-1.16325284113186));
#43483=CARTESIAN_POINT('Ctrl Pts',(-0.162811149525184,53.6764157686861,
-1.16667104267546));
#43484=CARTESIAN_POINT('Ctrl Pts',(-0.127842054805132,53.6740971291523,
-1.17085364712644));
#43485=CARTESIAN_POINT('Ctrl Pts',(-0.115790953119114,53.6732939332609,
-1.17210677451548));
#43486=CARTESIAN_POINT('Ctrl Pts',(-0.0937625018144055,53.6718171295385,
-1.17405436133281));
#43487=CARTESIAN_POINT('Ctrl Pts',(-0.0837914390509295,53.6711454498308,
-1.1748080839849));
#43488=CARTESIAN_POINT('Ctrl Pts',(-0.0619430650411083,53.6696660844722,
-1.17618006793515));
#43489=CARTESIAN_POINT('Ctrl Pts',(-0.0500636726413079,53.6688568172892,
-1.1767455570374));
#43490=CARTESIAN_POINT('Ctrl Pts',(-0.0155216484095266,53.6664885166175,
-1.17786586539288));
#43491=CARTESIAN_POINT('Ctrl Pts',(0.00714985271567457,53.6649150269079,
-1.17794638019866));
#43492=CARTESIAN_POINT('Ctrl Pts',(0.08368940932996,53.659535548023,-1.17600858175775));
#43493=CARTESIAN_POINT('Ctrl Pts',(0.137406833823505,53.6556435659775,-1.17094755463221));
#43494=CARTESIAN_POINT('Ctrl Pts',(0.258585755937825,53.6466595385097,-1.15107653050602));
#43495=CARTESIAN_POINT('Ctrl Pts',(0.325479484460857,53.6415491111313,-1.13397855320986));
#43496=CARTESIAN_POINT('Ctrl Pts',(0.410329347150613,53.635096902081,-1.10415888854439));
#43497=CARTESIAN_POINT('Ctrl Pts',(0.429974344367729,53.6336060852208,-1.09665820350503));
#43498=CARTESIAN_POINT('Ctrl Pts',(0.457057282400076,53.6315647643212,-1.08547784970786));
#43499=CARTESIAN_POINT('Ctrl Pts',(0.464672026240766,53.6309923923729,-1.08224001015246));
#43500=CARTESIAN_POINT('Ctrl Pts',(0.477530277115895,53.6300293263961,-1.07661185727455));
#43501=CARTESIAN_POINT('Ctrl Pts',(0.482791412411177,53.6296362770106,-1.07426287047756));
#43502=CARTESIAN_POINT('Ctrl Pts',(0.493928313695612,53.6288066227151,-1.06919212905545));
#43503=CARTESIAN_POINT('Ctrl Pts',(0.499799171704392,53.6283706147074,-1.06646039816956));
#43504=CARTESIAN_POINT('Ctrl Pts',(0.51628370097506,53.6271493452826,-1.05862405964244));
#43505=CARTESIAN_POINT('Ctrl Pts',(0.526844090655197,53.6263704786571,-1.05340832055091));
#43506=CARTESIAN_POINT('Ctrl Pts',(0.588258284704693,53.6218512658212,-1.02192140920936));
#43507=CARTESIAN_POINT('Ctrl Pts',(0.63722668266313,53.6182875568741,-0.99212645998877));
#43508=CARTESIAN_POINT('Ctrl Pts',(0.754771189948186,53.6093548498176,-0.908298358852658));
#43509=CARTESIAN_POINT('Ctrl Pts',(0.819864557515042,53.6040241618622,-0.850003470836564));
#43510=CARTESIAN_POINT('Ctrl Pts',(0.890234272667171,53.5971874920884,-0.771309652110807));
#43511=CARTESIAN_POINT('Ctrl Pts',(0.902210230398231,53.5959805301114,-0.757266319892999));
#43512=CARTESIAN_POINT('Ctrl Pts',(0.920827598299305,53.594028795696,-0.734366337528263));
#43513=CARTESIAN_POINT('Ctrl Pts',(0.927682953571771,53.5932927030396,-0.725687058619148));
#43514=CARTESIAN_POINT('Ctrl Pts',(0.940568701858436,53.591874368064,-0.70889194020726));
#43515=CARTESIAN_POINT('Ctrl Pts',(0.946618832718822,53.5911929912547,-0.70079243736782));
#43516=CARTESIAN_POINT('Ctrl Pts',(0.960439230683301,53.589599430457,-0.681785071767931));
#43517=CARTESIAN_POINT('Ctrl Pts',(0.96812906748496,53.5886842582153,-0.670820752986448));
#43518=CARTESIAN_POINT('Ctrl Pts',(0.993315958693978,53.5855874415137,-0.633573457437504));
#43519=CARTESIAN_POINT('Ctrl Pts',(1.00994145730019,53.5833742711981,-0.606720569476476));
#43520=CARTESIAN_POINT('Ctrl Pts',(1.04958723165269,53.5776363383147,-0.536532341734669));
#43521=CARTESIAN_POINT('Ctrl Pts',(1.07101446968706,53.5740674867239,-0.492369270769709));
#43522=CARTESIAN_POINT('Ctrl Pts',(1.11780681112742,53.5650230325015,-0.378307217113263));
#43523=CARTESIAN_POINT('Ctrl Pts',(1.13943069637904,53.5595238562637,-0.307095545735416));
#43524=CARTESIAN_POINT('Ctrl Pts',(1.15656784309077,53.5534528412819,-0.222681107322508));
#43525=CARTESIAN_POINT('Ctrl Pts',(1.15875419629785,53.5526233464698,-0.211008982933579));
#43526=CARTESIAN_POINT('Ctrl Pts',(1.16187461019135,53.5513492573521,-0.192835535692198));
#43527=CARTESIAN_POINT('Ctrl Pts',(1.16293139537067,53.5508984493367,-0.186356455546155));
#43528=CARTESIAN_POINT('Ctrl Pts',(1.16480972565689,53.5500595626198,-0.174201741319826));
#43529=CARTESIAN_POINT('Ctrl Pts',(1.16564403702173,53.5496708519765,-0.168528704012624));
#43530=CARTESIAN_POINT('Ctrl Pts',(1.16755542371879,53.5487392497945,-0.154838071043752));
#43531=CARTESIAN_POINT('Ctrl Pts',(1.16859138766132,53.5481986078473,-0.146815100038312));
#43532=CARTESIAN_POINT('Ctrl Pts',(1.17204271997722,53.5462557133987,-0.117729968719078));
#43533=CARTESIAN_POINT('Ctrl Pts',(1.17397212427653,53.5448773880538,-0.0966129639201676));
#43534=CARTESIAN_POINT('Ctrl Pts',(1.17759007943259,53.5412574067993,-0.040256796115039));
#43535=CARTESIAN_POINT('Ctrl Pts',(1.17826762477489,53.5390513179674,-0.0049735429055084));
#43536=CARTESIAN_POINT('Ctrl Pts',(1.17498144957712,53.5311210256185,0.122763058998919));
#43537=CARTESIAN_POINT('Ctrl Pts',(1.16171698058323,53.5254968070784,0.214626721490528));
#43538=CARTESIAN_POINT('Ctrl Pts',(1.13276132659902,53.5182525368309,0.323008242973149));
#43539=CARTESIAN_POINT('Ctrl Pts',(1.12720476688198,53.5169682128172,0.341894558470876));
#43540=CARTESIAN_POINT('Ctrl Pts',(1.11768198656201,53.5149149956376,0.371500173670461));
#43541=CARTESIAN_POINT('Ctrl Pts',(1.11402842904227,53.5141562892186,0.382316682849085));
#43542=CARTESIAN_POINT('Ctrl Pts',(1.10720427810417,53.5127880798925,0.401590964814957));
#43543=CARTESIAN_POINT('Ctrl Pts',(1.10409250578537,53.512180573141,0.410068710424449));
#43544=CARTESIAN_POINT('Ctrl Pts',(1.09653885311686,53.5107428072886,0.42993848608389));
#43545=CARTESIAN_POINT('Ctrl Pts',(1.09201652441991,53.5099099044167,0.441298593736082));
#43546=CARTESIAN_POINT('Ctrl Pts',(1.07791438922034,53.5073920071606,0.475178373587465));
#43547=CARTESIAN_POINT('Ctrl Pts',(1.06780927616412,53.5056895949642,0.497470715302193));
#43548=CARTESIAN_POINT('Ctrl Pts',(1.01432040096068,53.4971432299624,0.606318121929986));
#43549=CARTESIAN_POINT('Ctrl Pts',(0.961076625213557,53.4899686094203,0.687599897175047));
#43550=CARTESIAN_POINT('Ctrl Pts',(0.8723168884384,53.4799374331565,0.792337745829489));
#43551=CARTESIAN_POINT('Ctrl Pts',(0.844548989662814,53.4770086703715,0.82187196328075));
#43552=CARTESIAN_POINT('Ctrl Pts',(0.808058928259811,53.4734641648204,0.85687620802663));
#43553=CARTESIAN_POINT('Ctrl Pts',(0.800717228437614,53.4727653167395,0.863740704499297));
#43554=CARTESIAN_POINT('Ctrl Pts',(0.788772247053147,53.4716522796479,0.874626054682852));
#43555=CARTESIAN_POINT('Ctrl Pts',(0.7842241556256,53.4712339368155,0.878706362378256));
#43556=CARTESIAN_POINT('Ctrl Pts',(0.775176536320685,53.4704127717297,0.886697204587074));
#43557=CARTESIAN_POINT('Ctrl Pts',(0.770678703017699,53.4700098517953,0.890609305338378));
#43558=CARTESIAN_POINT('Ctrl Pts',(0.759051820776676,53.4689812533735,0.900568028975325));
#43559=CARTESIAN_POINT('Ctrl Pts',(0.751879952810958,53.4683590923172,0.906564389198077));
#43560=CARTESIAN_POINT('Ctrl Pts',(0.719108673922144,53.4655673220435,0.933307821675175));
#43561=CARTESIAN_POINT('Ctrl Pts',(0.692714612460654,53.463457725435,0.953062253515281));
#43562=CARTESIAN_POINT('Ctrl Pts',(0.59767943733474,53.4561987284,1.01815351146247));
#43563=CARTESIAN_POINT('Ctrl Pts',(0.525153308653292,53.4512264342153,1.05738940345974));
#43564=CARTESIAN_POINT('Ctrl Pts',(0.411277463622825,53.4434955467889,1.10436517124263));
#43565=CARTESIAN_POINT('Ctrl Pts',(0.37264122855725,53.440887662107,1.11799355015461));
#43566=CARTESIAN_POINT('Ctrl Pts',(0.319085238406269,53.4372421731406,1.13379967621427));
#43567=CARTESIAN_POINT('Ctrl Pts',(0.304715699979462,53.4362612991878,1.13774575557498));
#43568=CARTESIAN_POINT('Ctrl Pts',(0.280340057740739,53.4345907073707,1.14394476071865));
#43569=CARTESIAN_POINT('Ctrl Pts',(0.270372144584672,53.4339056915133,1.14634159639856));
#43570=CARTESIAN_POINT('Ctrl Pts',(0.250095003439261,53.4325078074733,1.15093816047064));
#43571=CARTESIAN_POINT('Ctrl Pts',(0.239785016805525,53.4317947630238,1.15313021514289));
#43572=CARTESIAN_POINT('Ctrl Pts',(0.215987303652998,53.4301430568098,1.15785701435894));
#43573=CARTESIAN_POINT('Ctrl Pts',(0.202482313003292,53.4292014287768,1.16029490081215));
#43574=CARTESIAN_POINT('Ctrl Pts',(0.188938462305883,53.4282524383066,1.16249615911688));
#43575=CARTESIAN_POINT('Origin',(0.,56.5393671147362,0.));
#43576=CARTESIAN_POINT('',(0.188938518720844,52.8287166258961,1.16249614994785));
#43577=CARTESIAN_POINT('',(0.188938438127302,52.9266130464139,1.16249616304658));
#43578=CARTESIAN_POINT('',(0.188938462403162,56.5393671147362,1.16249615910107));
#43579=CARTESIAN_POINT('',(-1.17774981132563,53.18979291915,-0.000666650161686058));
#43580=CARTESIAN_POINT('Ctrl Pts',(0.188938518720853,52.8287166258961,1.16249614994785));
#43581=CARTESIAN_POINT('Ctrl Pts',(0.2006730995186,52.8295897176874,1.16058894852285));
#43582=CARTESIAN_POINT('Ctrl Pts',(0.212381401918546,52.8304621543522,1.15850364635666));
#43583=CARTESIAN_POINT('Ctrl Pts',(0.267010632734191,52.8345345518635,1.14791744976063));
#43584=CARTESIAN_POINT('Ctrl Pts',(0.309469407987332,52.8377059339504,1.13720649980803));
#43585=CARTESIAN_POINT('Ctrl Pts',(0.360959490409606,52.8414889103456,1.12111866210965));
#43586=CARTESIAN_POINT('Ctrl Pts',(0.370642167423009,52.8421974189029,1.11795492294123));
#43587=CARTESIAN_POINT('Ctrl Pts',(0.386094072421604,52.8433221207186,1.11268330125663));
#43588=CARTESIAN_POINT('Ctrl Pts',(0.391889736438981,52.8437426143387,1.11065530228121));
#43589=CARTESIAN_POINT('Ctrl Pts',(0.403260880691614,52.8445645842728,1.10657625668621));
#43590=CARTESIAN_POINT('Ctrl Pts',(0.408837163538314,52.8449661963987,1.10452819163131));
#43591=CARTESIAN_POINT('Ctrl Pts',(0.423048378346701,52.8459865072165,1.09918630704447));
#43592=CARTESIAN_POINT('Ctrl Pts',(0.431660700320431,52.8466018019491,1.0958327979896));
#43593=CARTESIAN_POINT('Ctrl Pts',(0.46960169037032,52.8493027398839,1.08054241916639));
#43594=CARTESIAN_POINT('Ctrl Pts',(0.498483985424261,52.8513330893003,1.06752600009715));
#43595=CARTESIAN_POINT('Ctrl Pts',(0.593337432878825,52.8580266417731,1.02008765996191));
#43596=CARTESIAN_POINT('Ctrl Pts',(0.656566379223215,52.8625411110672,0.980586433127076));
#43597=CARTESIAN_POINT('Ctrl Pts',(0.754224455601946,52.8702100380247,0.905869552532492));
#43598=CARTESIAN_POINT('Ctrl Pts',(0.790933302753439,52.8732827095672,0.874001086947903));
#43599=CARTESIAN_POINT('Ctrl Pts',(0.836747547604304,52.8774684280752,0.828971854586845));
#43600=CARTESIAN_POINT('Ctrl Pts',(0.847706445816414,52.8784987031842,0.817761907709031));
#43601=CARTESIAN_POINT('Ctrl Pts',(0.864910923710795,52.8801659611316,0.799445773687585));
#43602=CARTESIAN_POINT('Ctrl Pts',(0.871300523789437,52.8807967050165,0.792477027679491));
#43603=CARTESIAN_POINT('Ctrl Pts',(0.884437357022759,52.8821183724084,0.777798543247462));
#43604=CARTESIAN_POINT('Ctrl Pts',(0.8911692497593,52.882809861242,0.770076209935523));
#43605=CARTESIAN_POINT('Ctrl Pts',(0.907028756337303,52.8844740124996,0.751396862259263));
#43606=CARTESIAN_POINT('Ctrl Pts',(0.916059585857138,52.8854504977446,0.740360191567335));
#43607=CARTESIAN_POINT('Ctrl Pts',(0.948456625177196,52.8890634303193,0.699267008691656));
#43608=CARTESIAN_POINT('Ctrl Pts',(0.970559932785211,52.8917477722769,0.668249342853592));
#43609=CARTESIAN_POINT('Ctrl Pts',(1.02828932224789,52.899412415559,0.578316762190948));
#43610=CARTESIAN_POINT('Ctrl Pts',(1.06030967675751,52.9044893720213,0.517272734497527));
#43611=CARTESIAN_POINT('Ctrl Pts',(1.10561411067218,52.9131112608756,0.408769742506601));
#43612=CARTESIAN_POINT('Ctrl Pts',(1.12159847298634,52.9166611620149,0.362619806138691));
#43613=CARTESIAN_POINT('Ctrl Pts',(1.13744784911272,52.9208108259074,0.305637899272518));
#43614=CARTESIAN_POINT('Ctrl Pts',(1.14008935721792,52.9215308952189,0.295632222587381));
#43615=CARTESIAN_POINT('Ctrl Pts',(1.14409604138076,52.9226694610145,0.279602282609837));
#43616=CARTESIAN_POINT('Ctrl Pts',(1.14554623549847,52.9230924365349,0.273600100700102));
#43617=CARTESIAN_POINT('Ctrl Pts',(1.14829307666671,52.9239152281922,0.261826390607417));
#43618=CARTESIAN_POINT('Ctrl Pts',(1.14959356170063,52.9243152258021,0.256056036737968));
#43619=CARTESIAN_POINT('Ctrl Pts',(1.15278759123815,52.9253256263788,0.241368850269724));
#43620=CARTESIAN_POINT('Ctrl Pts',(1.15462124072121,52.9259327579675,0.232439144088306));
#43621=CARTESIAN_POINT('Ctrl Pts',(1.1620907742283,52.9285330512514,0.19379109163921));
#43622=CARTESIAN_POINT('Ctrl Pts',(1.16668480798187,52.9304758954287,0.163880592253115));
#43623=CARTESIAN_POINT('Ctrl Pts',(1.17773365483925,52.9366238649529,0.0672721995210272));
#43624=CARTESIAN_POINT('Ctrl Pts',(1.17965376705203,52.9407056477405,0.000189555242239093));
#43625=CARTESIAN_POINT('Ctrl Pts',(1.17265342603484,52.9483790633043,-0.123228654284533));
#43626=CARTESIAN_POINT('Ctrl Pts',(1.16537447955829,52.9519379905089,-0.179450750498619));
#43627=CARTESIAN_POINT('Ctrl Pts',(1.15085906525947,52.9566741898002,-0.250757771638523));
#43628=CARTESIAN_POINT('Ctrl Pts',(1.14731135900949,52.957734983924,-0.266519515351546));
#43629=CARTESIAN_POINT('Ctrl Pts',(1.14090150898911,52.9595087196088,-0.292491214293996));
#43630=CARTESIAN_POINT('Ctrl Pts',(1.13822361739693,52.9602157081075,-0.30274469106938));
#43631=CARTESIAN_POINT('Ctrl Pts',(1.13266181922262,52.9616210348736,-0.322922674878579));
#43632=CARTESIAN_POINT('Ctrl Pts',(1.12978491752607,52.9623190897455,-0.332848131945473));
#43633=CARTESIAN_POINT('Ctrl Pts',(1.12247906632206,52.9640254783519,-0.356866954416469));
#43634=CARTESIAN_POINT('Ctrl Pts',(1.1179149411176,52.9650381452989,-0.370917008369469));
#43635=CARTESIAN_POINT('Ctrl Pts',(1.0991433750963,52.9690095822471,-0.425205536805777));
#43636=CARTESIAN_POINT('Ctrl Pts',(1.08301904835391,52.9720298913571,-0.464741741315517));
#43637=CARTESIAN_POINT('Ctrl Pts',(1.02612121917154,52.9816230403571,-0.585112510950493));
#43638=CARTESIAN_POINT('Ctrl Pts',(0.978162190955798,52.9883768112269,-0.662176937680276));
#43639=CARTESIAN_POINT('Ctrl Pts',(0.906577877595465,52.9966676415709,-0.752206357595949));
#43640=CARTESIAN_POINT('Ctrl Pts',(0.89069928776084,52.998416204701,-0.770942814697882));
#43641=CARTESIAN_POINT('Ctrl Pts',(0.868377364399699,53.0007413496616,-0.795671104170916));
#43642=CARTESIAN_POINT('Ctrl Pts',(0.862436838404874,53.0013480982001,-0.802106267539213));
#43643=CARTESIAN_POINT('Ctrl Pts',(0.852451686046485,53.00234731473,-0.812683632040403));
#43644=CARTESIAN_POINT('Ctrl Pts',(0.848447385578473,53.0027426575487,-0.816863270375048));
#43645=CARTESIAN_POINT('Ctrl Pts',(0.840043934300118,53.0035609405267,-0.825506219450236));
#43646=CARTESIAN_POINT('Ctrl Pts',(0.835639711988269,53.0039834835219,-0.829964219847369));
#43647=CARTESIAN_POINT('Ctrl Pts',(0.823564169564346,53.0051257024392,-0.841993638963694));
#43648=CARTESIAN_POINT('Ctrl Pts',(0.815823954686229,53.0058402453446,-0.849495453100467));
#43649=CARTESIAN_POINT('Ctrl Pts',(0.762786259511501,53.0106282156251,-0.899505913155628));
#43650=CARTESIAN_POINT('Ctrl Pts',(0.714284081766245,53.0144851746573,-0.938484965679031));
#43651=CARTESIAN_POINT('Ctrl Pts',(0.594101508627504,53.0234745825206,-1.02032949163686));
#43652=CARTESIAN_POINT('Ctrl Pts',(0.520506789082438,53.0285823425829,-1.05976408288123));
#43653=CARTESIAN_POINT('Ctrl Pts',(0.425904987512413,53.0351900187235,-1.09820557622742));
#43654=CARTESIAN_POINT('Ctrl Pts',(0.408270675972368,53.0364223260745,-1.10488258960758));
#43655=CARTESIAN_POINT('Ctrl Pts',(0.379971739242383,53.0384051851033,-1.11482765773376));
#43656=CARTESIAN_POINT('Ctrl Pts',(0.369407428586212,53.0391465462902,-1.11837264200398));
#43657=CARTESIAN_POINT('Ctrl Pts',(0.349183728680285,53.0405687466225,-1.12484114737185));
#43658=CARTESIAN_POINT('Ctrl Pts',(0.339533910166088,53.0412486313885,-1.12779146832828));
#43659=CARTESIAN_POINT('Ctrl Pts',(0.31714955400953,53.0428292538764,-1.13432190655528));
#43660=CARTESIAN_POINT('Ctrl Pts',(0.30439044762799,53.0437328229255,-1.13781213636515));
#43661=CARTESIAN_POINT('Ctrl Pts',(0.262061611743417,53.0467403208364,-1.14862819548066));
#43662=CARTESIAN_POINT('Ctrl Pts',(0.232268586942874,53.0488733075452,-1.15502122571214));
#43663=CARTESIAN_POINT('Ctrl Pts',(0.156664191535607,53.0543281790943,-1.16820112986629));
#43664=CARTESIAN_POINT('Ctrl Pts',(0.110640043253869,53.0576885005965,-1.17345456225868));
#43665=CARTESIAN_POINT('Ctrl Pts',(-0.0115765761533891,53.0666567579805,
-1.18015058576851));
#43666=CARTESIAN_POINT('Ctrl Pts',(-0.0878115283503732,53.0723048533969,
-1.17693664445345));
#43667=CARTESIAN_POINT('Ctrl Pts',(-0.17656862787715,53.0786439264146,-1.16451733757324));
#43668=CARTESIAN_POINT('Ctrl Pts',(-0.1898985530457,53.0795891535347,-1.16241803501005));
#43669=CARTESIAN_POINT('Ctrl Pts',(-0.209908532292049,53.0809949450734,
-1.15891328062842));
#43670=CARTESIAN_POINT('Ctrl Pts',(-0.216616784493539,53.0814639956263,
-1.15767817567493));
#43671=CARTESIAN_POINT('Ctrl Pts',(-0.228896554039207,53.0823180467502,
-1.15530677987873));
#43672=CARTESIAN_POINT('Ctrl Pts',(-0.234470901157486,53.0827039544629,
-1.15418836709251));
#43673=CARTESIAN_POINT('Ctrl Pts',(-0.247540556601461,53.0836047773406,
-1.15146753059295));
#43674=CARTESIAN_POINT('Ctrl Pts',(-0.255028633944232,53.084117861702,-1.14983225079936));
#43675=CARTESIAN_POINT('Ctrl Pts',(-0.280343802733076,53.0858438361369,
-1.14404433593328));
#43676=CARTESIAN_POINT('Ctrl Pts',(-0.298090792901531,53.0870392746276,
-1.13954905867998));
#43677=CARTESIAN_POINT('Ctrl Pts',(-0.342906325355392,53.09003773247,-1.12707862822197));
#43678=CARTESIAN_POINT('Ctrl Pts',(-0.369806996218645,53.0918185551398,
-1.11854099995123));
#43679=CARTESIAN_POINT('Ctrl Pts',(-0.477661504512481,53.0989750930174,
-1.07999341288384));
#43680=CARTESIAN_POINT('Ctrl Pts',(-0.555503955156738,53.1041992107036,
-1.042094911211));
#43681=CARTESIAN_POINT('Ctrl Pts',(-0.654109799791452,53.1116010380592,
-0.979873452017202));
#43682=CARTESIAN_POINT('Ctrl Pts',(-0.679078846822568,53.1135490442023,
-0.962737397082373));
#43683=CARTESIAN_POINT('Ctrl Pts',(-0.713168118897791,53.1163337658918,
-0.937355785675274));
#43684=CARTESIAN_POINT('Ctrl Pts',(-0.72286296091537,53.1171406375484,-0.929899863447548));
#43685=CARTESIAN_POINT('Ctrl Pts',(-0.74041546657779,53.118630322848,-0.915960551827862));
#43686=CARTESIAN_POINT('Ctrl Pts',(-0.748308565487754,53.1193112601898,
-0.909523543029886));
#43687=CARTESIAN_POINT('Ctrl Pts',(-0.764276655294852,53.1207122720172,
-0.896152621115338));
#43688=CARTESIAN_POINT('Ctrl Pts',(-0.772343099562601,53.1214326633869,
-0.889210014410118));
#43689=CARTESIAN_POINT('Ctrl Pts',(-0.792585551049317,53.1232736352252,
-0.871304550059492));
#43690=CARTESIAN_POINT('Ctrl Pts',(-0.804628573098222,53.1244002566837,
-0.860195493290082));
#43691=CARTESIAN_POINT('Ctrl Pts',(-0.864896613328724,53.1302042905662,
-0.802228145526444));
#43692=CARTESIAN_POINT('Ctrl Pts',(-0.909269337253967,53.1350466833101,
-0.751560206045921));
#43693=CARTESIAN_POINT('Ctrl Pts',(-0.991809042942691,53.1452522320054,
-0.639233015411393));
#43694=CARTESIAN_POINT('Ctrl Pts',(-1.02911039010068,53.1506063499974,-0.577266524132677));
#43695=CARTESIAN_POINT('Ctrl Pts',(-1.06796373237299,53.1569762139058,-0.496832538305492));
#43696=CARTESIAN_POINT('Ctrl Pts',(-1.0750846390581,53.1581860170101,-0.481229880008048));
#43697=CARTESIAN_POINT('Ctrl Pts',(-1.08461638336148,53.1598624496257,-0.459076146974757));
#43698=CARTESIAN_POINT('Ctrl Pts',(-1.08731332925585,53.1603438158904,-0.452651452877882));
#43699=CARTESIAN_POINT('Ctrl Pts',(-1.09213634622688,53.1612172835387,-0.440870127773195));
#43700=CARTESIAN_POINT('Ctrl Pts',(-1.09428041212785,53.1616103971149,-0.43552112916146));
#43701=CARTESIAN_POINT('Ctrl Pts',(-1.09875157952514,53.1624403755978,-0.424124987647527));
#43702=CARTESIAN_POINT('Ctrl Pts',(-1.10106816727896,53.1628766409014,-0.418074077964121));
#43703=CARTESIAN_POINT('Ctrl Pts',(-1.10745939798681,53.1640990626195,-0.400958554817809));
#43704=CARTESIAN_POINT('Ctrl Pts',(-1.11141811817988,53.1648788071173,-0.389851091641765));
#43705=CARTESIAN_POINT('Ctrl Pts',(-1.14123400628228,53.1709506699302,-0.302044825141836));
#43706=CARTESIAN_POINT('Ctrl Pts',(-1.15929234383037,53.1758839538206,-0.222914798662539));
#43707=CARTESIAN_POINT('Ctrl Pts',(-1.17483202358449,53.1838233515734,-0.0954687539975504));
#43708=CARTESIAN_POINT('Ctrl Pts',(-1.17772296884976,53.1867715638193,-0.0480884055395803));
#43709=CARTESIAN_POINT('Ctrl Pts',(-1.17774981132563,53.18979291915,-0.000666650161686058));
#43710=CARTESIAN_POINT('Ctrl Pts',(-1.17774981213881,53.1897930107793,-0.000665211992267972));
#43711=CARTESIAN_POINT('Ctrl Pts',(-1.17775881074562,53.1908080729105,0.0152667128767563));
#43712=CARTESIAN_POINT('Ctrl Pts',(-1.17744453218618,53.1918307404128,0.0311967694603609));
#43713=CARTESIAN_POINT('Ctrl Pts',(-1.17628672381245,53.1937050423063,0.0601156220613494));
#43714=CARTESIAN_POINT('Ctrl Pts',(-1.1755508580111,53.1945535166369,0.073106114269657));
#43715=CARTESIAN_POINT('Ctrl Pts',(-1.17385945964058,53.19607422811,0.0961856340810697));
#43716=CARTESIAN_POINT('Ctrl Pts',(-1.17298863166316,53.196743851152,0.106279662253863));
#43717=CARTESIAN_POINT('Ctrl Pts',(-1.17105087815903,53.1980480573628,0.125796719961337));
#43718=CARTESIAN_POINT('Ctrl Pts',(-1.17000015236007,53.1986820889182,0.135220591887283));
#43719=CARTESIAN_POINT('Ctrl Pts',(-1.16753584597819,53.2000315893319,0.15513595615592));
#43720=CARTESIAN_POINT('Ctrl Pts',(-1.16609437843298,53.2007478837948,0.165623079140138));
#43721=CARTESIAN_POINT('Ctrl Pts',(-1.16210522261643,53.202564742239,0.192004156347377));
#43722=CARTESIAN_POINT('Ctrl Pts',(-1.15937275888079,53.2036710305287,0.207867519135568));
#43723=CARTESIAN_POINT('Ctrl Pts',(-1.14528736706233,53.208815527063,0.280685607510413));
#43724=CARTESIAN_POINT('Ctrl Pts',(-1.13005828750316,53.212973566722,0.336799700416078));
#43725=CARTESIAN_POINT('Ctrl Pts',(-1.09101171867704,53.2215357586388,0.447566318194352));
#43726=CARTESIAN_POINT('Ctrl Pts',(-1.06705928347146,53.2259311043804,0.502002469110884));
#43727=CARTESIAN_POINT('Ctrl Pts',(-1.02233577947957,53.23284979792,0.58582719210843));
#43728=CARTESIAN_POINT('Ctrl Pts',(-1.00414890491117,53.2354135532736,0.616481481327817));
#43729=CARTESIAN_POINT('Ctrl Pts',(-0.979356217176713,53.2385757476547,
0.654253570115244));
#43730=CARTESIAN_POINT('Ctrl Pts',(-0.974016657234918,53.2392391980329,
0.662176638376606));
#43731=CARTESIAN_POINT('Ctrl Pts',(-0.965164783229106,53.2403098210482,
0.674972638822706));
#43732=CARTESIAN_POINT('Ctrl Pts',(-0.961710676379634,53.2407206233373,
0.679885064873146));
#43733=CARTESIAN_POINT('Ctrl Pts',(-0.954693800564389,53.241540951109,0.689703973520671));
#43734=CARTESIAN_POINT('Ctrl Pts',(-0.951130422153745,53.2419504194311,
0.69460978122075));
#43735=CARTESIAN_POINT('Ctrl Pts',(-0.941693056909727,53.2430170464234,
0.707393673738016));
#43736=CARTESIAN_POINT('Ctrl Pts',(-0.9357579461752,53.2436701693493,0.715226331351325));
#43737=CARTESIAN_POINT('Ctrl Pts',(-0.907347060874671,53.2467196147501,
0.751761460492516));
#43738=CARTESIAN_POINT('Ctrl Pts',(-0.883642479901959,53.2490428235216,
0.779487324018403));
#43739=CARTESIAN_POINT('Ctrl Pts',(-0.80460934965297,53.2562894596543,0.863679333028259));
#43740=CARTESIAN_POINT('Ctrl Pts',(-0.744871180500709,53.2610766954214,
0.915699608718587));
#43741=CARTESIAN_POINT('Ctrl Pts',(-0.647290672665594,53.268586224422,0.984760080301541));
#43742=CARTESIAN_POINT('Ctrl Pts',(-0.613025492960796,53.271170467429,1.00644764598841));
#43743=CARTESIAN_POINT('Ctrl Pts',(-0.565039602314749,53.2747687997538,
1.03345867041337));
#43744=CARTESIAN_POINT('Ctrl Pts',(-0.552235426345082,53.2757268932295,
1.04035694774618));
#43745=CARTESIAN_POINT('Ctrl Pts',(-0.530156632796453,53.2773774206417,
1.05172950752944));
#43746=CARTESIAN_POINT('Ctrl Pts',(-0.520944877503815,53.2780655992446,
1.05632260006367));
#43747=CARTESIAN_POINT('Ctrl Pts',(-0.502075982933415,53.2794749404054,
1.06542401572055));
#43748=CARTESIAN_POINT('Ctrl Pts',(-0.4924155095044,53.2801963423577,1.06992316493672));
#43749=CARTESIAN_POINT('Ctrl Pts',(-0.467687136289251,53.2820432407385,
1.08103401140068));
#43750=CARTESIAN_POINT('Ctrl Pts',(-0.452539724155098,53.2831748567747,
1.0874619723675));
#43751=CARTESIAN_POINT('Ctrl Pts',(-0.37729648407676,53.2888003301564,1.11754792797804));
#43752=CARTESIAN_POINT('Ctrl Pts',(-0.315468594688774,53.2934449294353,
1.13654880284632));
#43753=CARTESIAN_POINT('Ctrl Pts',(-0.204528913663951,53.3017526016701,
1.16088991129994));
#43754=CARTESIAN_POINT('Ctrl Pts',(-0.156044862621687,53.3053722508415,
1.16839524138436));
#43755=CARTESIAN_POINT('Ctrl Pts',(-0.0690196570407146,53.3117479978521,
1.17635195597477));
#43756=CARTESIAN_POINT('Ctrl Pts',(-0.030652948524172,53.314516585301,1.17797649572207));
#43757=CARTESIAN_POINT('Ctrl Pts',(0.017466945641632,53.317886483501,1.17766073989571));
#43758=CARTESIAN_POINT('Ctrl Pts',(0.0272050718706771,53.318563152773,1.17747603466719));
#43759=CARTESIAN_POINT('Ctrl Pts',(0.0429816306332634,53.319649639649,1.17698095863901));
#43760=CARTESIAN_POINT('Ctrl Pts',(0.0490217064016686,53.3200632789158,
1.17674486361693));
#43761=CARTESIAN_POINT('Ctrl Pts',(0.0603547529825577,53.3208346982353,
1.17621446323108));
#43762=CARTESIAN_POINT('Ctrl Pts',(0.0656480315593585,53.3211930751927,
1.17593090713628));
#43763=CARTESIAN_POINT('Ctrl Pts',(0.0798730920925098,53.3221514251488,
1.17507253145257));
#43764=CARTESIAN_POINT('Ctrl Pts',(0.0888007484543166,53.3227478522903,
1.17443160902997));
#43765=CARTESIAN_POINT('Ctrl Pts',(0.123789388982842,53.3250686265806,1.1715184779065));
#43766=CARTESIAN_POINT('Ctrl Pts',(0.149780866389999,53.3267562775609,1.16847989940207));
#43767=CARTESIAN_POINT('Ctrl Pts',(0.180085150454982,53.3287037036864,1.16390914793015));
#43768=CARTESIAN_POINT('Ctrl Pts',(0.184514178616128,53.3289878115911,1.16321523022274));
#43769=CARTESIAN_POINT('Ctrl Pts',(0.188938471457153,53.3292711974063,1.16249615762954));
#43770=CARTESIAN_POINT('',(-1.17774959099604,53.2897949711755,0.000981533826876358));
#43771=CARTESIAN_POINT('Ctrl Pts',(0.188938462305883,53.4282524383066,1.16249615911688));
#43772=CARTESIAN_POINT('Ctrl Pts',(0.186813409162065,53.4281035400925,1.16284154027806));
#43773=CARTESIAN_POINT('Ctrl Pts',(0.18468739932223,53.4279544610923,1.1631810960855));
#43774=CARTESIAN_POINT('Ctrl Pts',(0.12687570163315,53.4238975029053,1.17225199893712));
#43775=CARTESIAN_POINT('Ctrl Pts',(0.070643708420418,53.4198673902119,1.17697918612135));
#43776=CARTESIAN_POINT('Ctrl Pts',(-0.0568402614405747,53.4105834797223,
1.17852680582014));
#43777=CARTESIAN_POINT('Ctrl Pts',(-0.127906998503584,53.405301100624,1.17294324984981));
#43778=CARTESIAN_POINT('Ctrl Pts',(-0.224735460402383,53.3982000323451,
1.15642669540633));
#43779=CARTESIAN_POINT('Ctrl Pts',(-0.251273366197439,53.3962655679825,
1.15095207204492));
#43780=CARTESIAN_POINT('Ctrl Pts',(-0.286395110472615,53.393740482604,1.14243371371532));
#43781=CARTESIAN_POINT('Ctrl Pts',(-0.29516476711775,53.3931129610262,1.14019942227426));
#43782=CARTESIAN_POINT('Ctrl Pts',(-0.3090453074787,53.3921253875346,1.13649211767734));
#43783=CARTESIAN_POINT('Ctrl Pts',(-0.314173259945425,53.3917617790438,
1.13508523962241));
#43784=CARTESIAN_POINT('Ctrl Pts',(-0.325082545142064,53.3909911283218,
1.1320126307487));
#43785=CARTESIAN_POINT('Ctrl Pts',(-0.330861025279416,53.3905846727771,
1.13033722540397));
#43786=CARTESIAN_POINT('Ctrl Pts',(-0.345837456957529,53.3895351682323,
1.12587028734485));
#43787=CARTESIAN_POINT('Ctrl Pts',(-0.35501474216169,53.3888959211898,1.12301023961493));
#43788=CARTESIAN_POINT('Ctrl Pts',(-0.398840073619962,53.3858572439161,
1.10876137297469));
#43789=CARTESIAN_POINT('Ctrl Pts',(-0.432984949879753,53.383531699539,1.09587853487723));
#43790=CARTESIAN_POINT('Ctrl Pts',(-0.554763663171177,53.3752058229106,
1.04334872328381));
#43791=CARTESIAN_POINT('Ctrl Pts',(-0.638050306622606,53.369419163093,0.994601349775795));
#43792=CARTESIAN_POINT('Ctrl Pts',(-0.736859786128382,53.361498645237,0.919197887893779));
#43793=CARTESIAN_POINT('Ctrl Pts',(-0.758611969887773,53.3596815343996,
0.90132945413712));
#43794=CARTESIAN_POINT('Ctrl Pts',(-0.789339855014467,53.3569892355088,
0.874187059736822));
#43795=CARTESIAN_POINT('Ctrl Pts',(-0.798837184083047,53.3561386211128,
0.865516928651321));
#43796=CARTESIAN_POINT('Ctrl Pts',(-0.815498224929902,53.3546116929156,
0.849799177300278));
#43797=CARTESIAN_POINT('Ctrl Pts',(-0.822717386727143,53.3539380070507,
0.8428120119045));
#43798=CARTESIAN_POINT('Ctrl Pts',(-0.837891726661008,53.3524953546382,
0.827744569677094));
#43799=CARTESIAN_POINT('Ctrl Pts',(-0.845821322760341,53.3517253538657,
0.819640099343704));
#43800=CARTESIAN_POINT('Ctrl Pts',(-0.867295829766628,53.3495943180387,
0.797048499563651));
#43801=CARTESIAN_POINT('Ctrl Pts',(-0.880593201602652,53.3482229853186,
0.782332344309234));
#43802=CARTESIAN_POINT('Ctrl Pts',(-0.90976972827318,53.3450922524266,0.748356093704944));
#43803=CARTESIAN_POINT('Ctrl Pts',(-0.925420523200168,53.3433248736112,
0.728913236267799));
#43804=CARTESIAN_POINT('Ctrl Pts',(-0.978867727163318,53.3369668465686,
0.658018005155726));
#43805=CARTESIAN_POINT('Ctrl Pts',(-1.01308388236413,53.3322713101378,0.6040111058606));
#43806=CARTESIAN_POINT('Ctrl Pts',(-1.06651438653906,53.3238301417344,0.502249629217621));
#43807=CARTESIAN_POINT('Ctrl Pts',(-1.08730657253335,53.3200925602846,0.45549202904627));
#43808=CARTESIAN_POINT('Ctrl Pts',(-1.10940960067704,53.3155805326032,0.395560476715898));
#43809=CARTESIAN_POINT('Ctrl Pts',(-1.11362864851105,53.3146878691113,0.383521862535381));
#43810=CARTESIAN_POINT('Ctrl Pts',(-1.11978074298935,53.3133384110953,0.365009228423059));
#43811=CARTESIAN_POINT('Ctrl Pts',(-1.12185492541622,53.3128742580437,0.358583576275452));
#43812=CARTESIAN_POINT('Ctrl Pts',(-1.12556000521974,53.3120282967825,0.346758622549607));
#43813=CARTESIAN_POINT('Ctrl Pts',(-1.12720747915799,53.3116456076217,0.341365154175699));
#43814=CARTESIAN_POINT('Ctrl Pts',(-1.1310201093161,53.3107438968264,0.328554811595778));
#43815=CARTESIAN_POINT('Ctrl Pts',(-1.1331511215039,53.3102268081991,0.321128161097478));
#43816=CARTESIAN_POINT('Ctrl Pts',(-1.14019184177094,53.308470333215,0.295647838116286));
#43817=CARTESIAN_POINT('Ctrl Pts',(-1.14474465707906,53.3072492474254,0.277497465428001));
#43818=CARTESIAN_POINT('Ctrl Pts',(-1.16798841165331,53.3004482943822,0.174491110350817));
#43819=CARTESIAN_POINT('Ctrl Pts',(-1.17767717262205,53.295202567577,0.0878768684682339));
#43820=CARTESIAN_POINT('Ctrl Pts',(-1.17774959099604,53.2897949711755,0.000981533826876358));
#43821=CARTESIAN_POINT('Ctrl Pts',(-1.17774959188343,53.2897949048769,0.000980468466004801));
#43822=CARTESIAN_POINT('Ctrl Pts',(-1.17778032745941,53.2874973357847,-0.0359394461675392));
#43823=CARTESIAN_POINT('Ctrl Pts',(-1.1760750282772,53.2851776679351,-0.0728387245586704));
#43824=CARTESIAN_POINT('Ctrl Pts',(-1.17060466416177,53.2814102869727,-0.131369816716317));
#43825=CARTESIAN_POINT('Ctrl Pts',(-1.1679637027389,53.2799935590884,-0.153081687179469));
#43826=CARTESIAN_POINT('Ctrl Pts',(-1.16318664187066,53.2778800540219,-0.184929044750261));
#43827=CARTESIAN_POINT('Ctrl Pts',(-1.16151878914946,53.2771976563521,-0.195130742575383));
#43828=CARTESIAN_POINT('Ctrl Pts',(-1.15791318200115,53.2758237458455,-0.215497533749276));
#43829=CARTESIAN_POINT('Ctrl Pts',(-1.15597531406087,53.2751322861124,-0.225661662040095));
#43830=CARTESIAN_POINT('Ctrl Pts',(-1.15178709897825,53.2737255845958,-0.246157101937808));
#43831=CARTESIAN_POINT('Ctrl Pts',(-1.14953104667879,53.2730102186906,-0.25648625732619));
#43832=CARTESIAN_POINT('Ctrl Pts',(-1.14350288650903,53.2711981769024,-0.282406620401633));
#43833=CARTESIAN_POINT('Ctrl Pts',(-1.13955084495826,53.2700958358667,-0.297953315096262));
#43834=CARTESIAN_POINT('Ctrl Pts',(-1.12014624288904,53.2650386230242,-0.368242845669103));
#43835=CARTESIAN_POINT('Ctrl Pts',(-1.10105997143721,53.2609692160256,-0.421895301867576));
#43836=CARTESIAN_POINT('Ctrl Pts',(-1.05122151251319,53.2519467010786,-0.535270825702235));
#43837=CARTESIAN_POINT('Ctrl Pts',(-1.01908590543671,53.2469792789337,-0.5941761177014));
#43838=CARTESIAN_POINT('Ctrl Pts',(-0.965430522304102,53.2399318930273,
-0.675243022136471));
#43839=CARTESIAN_POINT('Ctrl Pts',(-0.947776629563363,53.237766860554,-0.699806418748032));
#43840=CARTESIAN_POINT('Ctrl Pts',(-0.923592901813035,53.2350162446476,
-0.730858637897702));
#43841=CARTESIAN_POINT('Ctrl Pts',(-0.917906923567276,53.2343838347964,
-0.737987187947478));
#43842=CARTESIAN_POINT('Ctrl Pts',(-0.908397208115924,53.2333503610177,
-0.749629609715714));
#43843=CARTESIAN_POINT('Ctrl Pts',(-0.904621315083805,53.2329461087124,
-0.754181888744853));
#43844=CARTESIAN_POINT('Ctrl Pts',(-0.896835625858463,53.2321252310991,
-0.763425835864132));
#43845=CARTESIAN_POINT('Ctrl Pts',(-0.892822966764624,53.2317088204095,
-0.76811477077353));
#43846=CARTESIAN_POINT('Ctrl Pts',(-0.881991063398176,53.2306017174844,
-0.780572659862728));
#43847=CARTESIAN_POINT('Ctrl Pts',(-0.875105914172077,53.2299156378716,
-0.78828394022504));
#43848=CARTESIAN_POINT('Ctrl Pts',(-0.835482877495063,53.2260590857437,
-0.831502153501267));
#43849=CARTESIAN_POINT('Ctrl Pts',(-0.800683154047731,53.2230189597548,
-0.865063612500677));
#43850=CARTESIAN_POINT('Ctrl Pts',(-0.711260232793834,53.2157138714024,
-0.941270608347812));
#43851=CARTESIAN_POINT('Ctrl Pts',(-0.654753547313782,53.2114958125317,
-0.981416918827469));
#43852=CARTESIAN_POINT('Ctrl Pts',(-0.562110701056196,53.2047365256981,
-1.03565608545356));
#43853=CARTESIAN_POINT('Ctrl Pts',(-0.528256256625591,53.202297334268,-1.05332656653601));
#43854=CARTESIAN_POINT('Ctrl Pts',(-0.480650104918661,53.1988685050152,
-1.0753018943789));
#43855=CARTESIAN_POINT('Ctrl Pts',(-0.46758698415141,53.1979278791769,-1.08104628508205));
#43856=CARTESIAN_POINT('Ctrl Pts',(-0.444972459158287,53.196298099099,-1.09050424646045));
#43857=CARTESIAN_POINT('Ctrl Pts',(-0.435470844720434,53.1956129286696,
-1.09433319103701));
#43858=CARTESIAN_POINT('Ctrl Pts',(-0.417111462799178,53.1942876460043,
-1.10145466080406));
#43859=CARTESIAN_POINT('Ctrl Pts',(-0.408261611474434,53.1936482116722,
-1.10476549082157));
#43860=CARTESIAN_POINT('Ctrl Pts',(-0.384646999409304,53.1919398817379,
-1.11327749566626));
#43861=CARTESIAN_POINT('Ctrl Pts',(-0.369817191693778,53.1908648946645,
-1.11829124107762));
#43862=CARTESIAN_POINT('Ctrl Pts',(-0.308777666326095,53.1864292751039,
-1.13758092825293));
#43863=CARTESIAN_POINT('Ctrl Pts',(-0.261814987612224,53.1829884726797,
-1.14929798181298));
#43864=CARTESIAN_POINT('Ctrl Pts',(-0.14091030334436,53.1740806924452,-1.17166773033841));
#43865=CARTESIAN_POINT('Ctrl Pts',(-0.0664311877587063,53.1685395185662,
-1.17823896993833));
#43866=CARTESIAN_POINT('Ctrl Pts',(0.0297017437705045,53.1615610568858,
-1.1775723544185));
#43867=CARTESIAN_POINT('Ctrl Pts',(0.0512299188434735,53.1600106316708,
-1.17683237720296));
#43868=CARTESIAN_POINT('Ctrl Pts',(0.0878515010458165,53.1574061502739,
-1.17456664668707));
#43869=CARTESIAN_POINT('Ctrl Pts',(0.102957599117281,53.1563414324886,-1.17333903019491));
#43870=CARTESIAN_POINT('Ctrl Pts',(0.125131928046243,53.1547965974966,-1.17110542523557));
#43871=CARTESIAN_POINT('Ctrl Pts',(0.132220811276758,53.1543054591375,-1.17032627077795));
#43872=CARTESIAN_POINT('Ctrl Pts',(0.144367128060274,53.1534691061801,-1.16887946777974));
#43873=CARTESIAN_POINT('Ctrl Pts',(0.149427832740566,53.1531222193662,-1.16824329807423));
#43874=CARTESIAN_POINT('Ctrl Pts',(0.161392314151985,53.1523058263058,-1.16666024865569));
#43875=CARTESIAN_POINT('Ctrl Pts',(0.168292033439669,53.1518378957449,-1.16568495419912));
#43876=CARTESIAN_POINT('Ctrl Pts',(0.189293012154789,53.1504212694848,-1.16252605034281));
#43877=CARTESIAN_POINT('Ctrl Pts',(0.203364156772529,53.1494826115159,-1.16014728645598));
#43878=CARTESIAN_POINT('Ctrl Pts',(0.291410655436076,53.143655627514,-1.1436115184159));
#43879=CARTESIAN_POINT('Ctrl Pts',(0.363936869121167,53.1390543099286,-1.12263982019768));
#43880=CARTESIAN_POINT('Ctrl Pts',(0.476750192251949,53.1315526342403,-1.07792485768823));
#43881=CARTESIAN_POINT('Ctrl Pts',(0.518497810757143,53.1286955641166,-1.05847643193722));
#43882=CARTESIAN_POINT('Ctrl Pts',(0.585712065282108,53.1238437760148,-1.02223165794898));
#43883=CARTESIAN_POINT('Ctrl Pts',(0.611856906900606,53.1218889494526,-1.00680041283312));
#43884=CARTESIAN_POINT('Ctrl Pts',(0.648481910469745,53.1190320043405,-0.983229743739168));
#43885=CARTESIAN_POINT('Ctrl Pts',(0.659467292674132,53.1181591236908,-0.975895682785428));
#43886=CARTESIAN_POINT('Ctrl Pts',(0.678619516190133,53.1166074435277,-0.962638218147491));
#43887=CARTESIAN_POINT('Ctrl Pts',(0.686838067156415,53.1159316011766,-0.956791641590141));
#43888=CARTESIAN_POINT('Ctrl Pts',(0.703980063034734,53.1145001403933,-0.944262357361838));
#43889=CARTESIAN_POINT('Ctrl Pts',(0.71288569648386,53.1137436892311,-0.937557090245571));
#43890=CARTESIAN_POINT('Ctrl Pts',(0.736619521453132,53.1116921727298,-0.919153649580152));
#43891=CARTESIAN_POINT('Ctrl Pts',(0.751263156528585,53.1103880622523,-0.907223979191796));
#43892=CARTESIAN_POINT('Ctrl Pts',(0.828598280208299,53.1032864833245,-0.841065082488195));
#43893=CARTESIAN_POINT('Ctrl Pts',(0.885709253569833,53.0972361118865,-0.780692154252102));
#43894=CARTESIAN_POINT('Ctrl Pts',(0.973902033390121,53.0865578640274,-0.665213463795146));
#43895=CARTESIAN_POINT('Ctrl Pts',(1.00779882087184,53.0819706078462,-0.612647676529148));
#43896=CARTESIAN_POINT('Ctrl Pts',(1.04247410570068,53.0768258807859,-0.548141430908158));
#43897=CARTESIAN_POINT('Ctrl Pts',(1.04744819706604,53.076074875009,-0.538575514287927));
#43898=CARTESIAN_POINT('Ctrl Pts',(1.05510452984942,53.0748993309761,-0.523343820823535));
#43899=CARTESIAN_POINT('Ctrl Pts',(1.05787397426443,53.0744698218832,-0.517722882322851));
#43900=CARTESIAN_POINT('Ctrl Pts',(1.06311409926472,53.0736491281615,-0.506869755202702));
#43901=CARTESIAN_POINT('Ctrl Pts',(1.06559128397986,53.0732575856574,-0.501641060866144));
#43902=CARTESIAN_POINT('Ctrl Pts',(1.07171797719502,53.0722796003028,-0.4884590152888));
#43903=CARTESIAN_POINT('Ctrl Pts',(1.07531766192179,53.071696099644,-0.480482642433942));
#43904=CARTESIAN_POINT('Ctrl Pts',(1.08865981614971,53.0694959533515,-0.450017223286487));
#43905=CARTESIAN_POINT('Ctrl Pts',(1.09778906223907,53.0679113171205,-0.427264627363491));
#43906=CARTESIAN_POINT('Ctrl Pts',(1.13727080674822,53.0605835154434,-0.319223409920281));
#43907=CARTESIAN_POINT('Ctrl Pts',(1.15843641609231,53.0551368375165,-0.230902366762911));
#43908=CARTESIAN_POINT('Ctrl Pts',(1.17438664714476,53.046785609058,-0.0986529972555718));
#43909=CARTESIAN_POINT('Ctrl Pts',(1.17718957778006,53.044069675923,-0.0560404025092714));
#43910=CARTESIAN_POINT('Ctrl Pts',(1.17784178715581,53.0403183970712,0.00139670291630801));
#43911=CARTESIAN_POINT('Ctrl Pts',(1.17773163731984,53.0393458375014,0.0161673935100462));
#43912=CARTESIAN_POINT('Ctrl Pts',(1.17707241148053,53.0376782933447,0.041259400569131));
#43913=CARTESIAN_POINT('Ctrl Pts',(1.17666519944823,53.0369877952924,0.0515829117962025));
#43914=CARTESIAN_POINT('Ctrl Pts',(1.17556546999635,53.0355805719014,0.072478350259879));
#43915=CARTESIAN_POINT('Ctrl Pts',(1.17486601220825,53.0348636918126,0.0830489376975468));
#43916=CARTESIAN_POINT('Ctrl Pts',(1.17274072100554,53.0330427092746,0.109704068902194));
#43917=CARTESIAN_POINT('Ctrl Pts',(1.17112655396628,53.0319328252079,0.125770945256003));
#43918=CARTESIAN_POINT('Ctrl Pts',(1.16238712106749,53.026897320322,0.197830703730188));
#43919=CARTESIAN_POINT('Ctrl Pts',(1.15157353640139,53.0228593505094,0.253293394710134));
#43920=CARTESIAN_POINT('Ctrl Pts',(1.11928052088419,53.0138572407522,0.372579690749307));
#43921=CARTESIAN_POINT('Ctrl Pts',(1.0962217995729,53.0088769090276,0.435777560097039));
#43922=CARTESIAN_POINT('Ctrl Pts',(1.05513475364238,53.0018136740027,0.52412074150068));
#43923=CARTESIAN_POINT('Ctrl Pts',(1.04131049376399,52.9996454164127,0.551075936517293));
#43924=CARTESIAN_POINT('Ctrl Pts',(1.02199122941377,52.9968917990483,0.585416181385997));
#43925=CARTESIAN_POINT('Ctrl Pts',(1.01742882674944,52.9962594612066,0.593310015051768));
#43926=CARTESIAN_POINT('Ctrl Pts',(1.0097564379765,52.9952260730573,0.606235905446079));
#43927=CARTESIAN_POINT('Ctrl Pts',(1.0066994570074,52.9948218353864,0.61129881881871));
#43928=CARTESIAN_POINT('Ctrl Pts',(1.000374666013,52.9940009535977,0.62159768162832));
#43929=CARTESIAN_POINT('Ctrl Pts',(0.997103612170494,52.9935845244912,0.626831349880083));
#43930=CARTESIAN_POINT('Ctrl Pts',(0.988243481445447,52.9924773151794,0.640762641157766));
#43931=CARTESIAN_POINT('Ctrl Pts',(0.982580631230541,52.9917911491458,0.649413013617887));
#43932=CARTESIAN_POINT('Ctrl Pts',(0.949785162033687,52.9879300941138,0.698098939005781));
#43933=CARTESIAN_POINT('Ctrl Pts',(0.920317624316057,52.98488592719,0.736512426138912));
#43934=CARTESIAN_POINT('Ctrl Pts',(0.843193583304655,52.9775801738212,0.825165955665399));
#43935=CARTESIAN_POINT('Ctrl Pts',(0.79331644543358,52.9733651438873,0.873225736831357));
#43936=CARTESIAN_POINT('Ctrl Pts',(0.709816123139314,52.9666099155097,0.940591292442827));
#43937=CARTESIAN_POINT('Ctrl Pts',(0.678975900981495,52.9641715790578,0.963089920640685));
#43938=CARTESIAN_POINT('Ctrl Pts',(0.635178970055762,52.9607437503787,0.991890274192237));
#43939=CARTESIAN_POINT('Ctrl Pts',(0.623116489623485,52.9598032304498,0.999512106595802));
#43940=CARTESIAN_POINT('Ctrl Pts',(0.602161159445122,52.9581735748295,1.012226226339));
#43941=CARTESIAN_POINT('Ctrl Pts',(0.593334671854942,52.9574884213037,1.01742515747232));
#43942=CARTESIAN_POINT('Ctrl Pts',(0.576238083428325,52.9561631298216,1.02719716718026));
#43943=CARTESIAN_POINT('Ctrl Pts',(0.567978524389655,52.9555236692693,1.03178715624679));
#43944=CARTESIAN_POINT('Ctrl Pts',(0.545889771404482,52.9538151683903,1.04371668524398));
#43945=CARTESIAN_POINT('Ctrl Pts',(0.531968352329282,52.952740034318,1.05088048431595));
#43946=CARTESIAN_POINT('Ctrl Pts',(0.475855384023323,52.9484108869342,1.07835484750512));
#43947=CARTESIAN_POINT('Ctrl Pts',(0.432616738387698,52.945082408327,1.09641657199658));
#43948=CARTESIAN_POINT('Ctrl Pts',(0.323517113591594,52.9367187336731,1.13453012528846));
#43949=CARTESIAN_POINT('Ctrl Pts',(0.256767693375939,52.9316259251028,1.15147199457756));
#43950=CARTESIAN_POINT('Ctrl Pts',(0.188938438127302,52.9266130464139,1.16249616304658));
#43951=CARTESIAN_POINT('Origin',(0.,56.5393671147362,0.));
#43952=CARTESIAN_POINT('',(0.188938462485257,52.327342596858,1.16249615908772));
#43953=CARTESIAN_POINT('',(0.188938431190144,52.4266410775339,1.16249616417406));
#43954=CARTESIAN_POINT('',(0.188938462403162,56.5393671147362,1.16249615910107));
#43955=CARTESIAN_POINT('Ctrl Pts',(0.188938462485257,52.327342596858,1.16249615908772));
#43956=CARTESIAN_POINT('Ctrl Pts',(0.196171651122745,52.3278387177455,1.16132056162071));
#43957=CARTESIAN_POINT('Ctrl Pts',(0.203393645764959,52.3283369745778,1.16007749164273));
#43958=CARTESIAN_POINT('Ctrl Pts',(0.228868425715194,52.3301050656455,1.1554475034012));
#43959=CARTESIAN_POINT('Ctrl Pts',(0.247051330677571,52.3313863019024,1.15169668786707));
#43960=CARTESIAN_POINT('Ctrl Pts',(0.3491060353982,52.3386904527072,1.12811667111043));
#43961=CARTESIAN_POINT('Ctrl Pts',(0.430678164409059,52.3449905913468,1.09956063034604));
#43962=CARTESIAN_POINT('Ctrl Pts',(0.560634907475863,52.3555772552927,1.03737076530023));
#43963=CARTESIAN_POINT('Ctrl Pts',(0.610968992825355,52.3598250712863,1.00854734780391));
#43964=CARTESIAN_POINT('Ctrl Pts',(0.668774236404321,52.364738285421,0.969523432267412));
#43965=CARTESIAN_POINT('Ctrl Pts',(0.678467391372795,52.3655632611532,0.962765127460925));
#43966=CARTESIAN_POINT('Ctrl Pts',(0.693320079048421,52.3668270924489,0.952073722462365));
#43967=CARTESIAN_POINT('Ctrl Pts',(0.698551296394552,52.3672721687913,0.948242161252259));
#43968=CARTESIAN_POINT('Ctrl Pts',(0.708370144731885,52.3681070512215,0.94092507111451));
#43969=CARTESIAN_POINT('Ctrl Pts',(0.712964035420163,52.3684973974311,0.937448951655603));
#43970=CARTESIAN_POINT('Ctrl Pts',(0.723051080066843,52.3693542625305,0.929699214297603));
#43971=CARTESIAN_POINT('Ctrl Pts',(0.728532135178738,52.3698197255308,0.92541041023103));
#43972=CARTESIAN_POINT('Ctrl Pts',(0.747346858309635,52.3714183059802,0.910417532805911));
#43973=CARTESIAN_POINT('Ctrl Pts',(0.760485903516109,52.3725360578737,0.899471329851401));
#43974=CARTESIAN_POINT('Ctrl Pts',(0.834631596224866,52.3788829986527,0.834913493652379));
#43975=CARTESIAN_POINT('Ctrl Pts',(0.890206588434308,52.3838095042527,0.775387303015026));
#43976=CARTESIAN_POINT('Ctrl Pts',(0.967823979591012,52.3917876779878,0.672799921650939));
#43977=CARTESIAN_POINT('Ctrl Pts',(0.994119215925472,52.3947557683597,0.633300387030666));
#43978=CARTESIAN_POINT('Ctrl Pts',(1.0291944075396,52.3992398862333,0.573020779696434));
#43979=CARTESIAN_POINT('Ctrl Pts',(1.03987558456847,52.4006923591232,0.553400946470502));
#43980=CARTESIAN_POINT('Ctrl Pts',(1.05535124954253,52.4029440772238,0.522942426461188));
#43981=CARTESIAN_POINT('Ctrl Pts',(1.06055109112651,52.4037291572135,0.51231475416677));
#43982=CARTESIAN_POINT('Ctrl Pts',(1.06985050906475,52.4051883993447,0.492559670103494));
#43983=CARTESIAN_POINT('Ctrl Pts',(1.07399561434788,52.4058609078884,0.483454806609093));
#43984=CARTESIAN_POINT('Ctrl Pts',(1.08293351437436,52.407361897769,0.463140021270697));
#43985=CARTESIAN_POINT('Ctrl Pts',(1.08766919054945,52.4081922407333,0.451906393173391));
#43986=CARTESIAN_POINT('Ctrl Pts',(1.10101235331791,52.4106390897167,0.418829358223343));
#43987=CARTESIAN_POINT('Ctrl Pts',(1.10914166328743,52.4122711928743,0.396800790904513));
#43988=CARTESIAN_POINT('Ctrl Pts',(1.14453211356754,52.4201043493812,0.291293618111428));
#43989=CARTESIAN_POINT('Ctrl Pts',(1.16305550722178,52.4265728159333,0.205190366441568));
#43990=CARTESIAN_POINT('Ctrl Pts',(1.175252874049,52.4355145986921,0.0839022907124738));
#43991=CARTESIAN_POINT('Ctrl Pts',(1.17719019495639,52.4380047301848,0.0498239371205162));
#43992=CARTESIAN_POINT('Ctrl Pts',(1.1779220454132,52.4419377297626,-0.00504432905393951));
#43993=CARTESIAN_POINT('Ctrl Pts',(1.17765028208433,52.4434079698568,-0.0258017071985731));
#43994=CARTESIAN_POINT('Ctrl Pts',(1.17651273787595,52.4454114526971,-0.0545645959089164));
#43995=CARTESIAN_POINT('Ctrl Pts',(1.17611344113166,52.4459663595309,-0.0625835461111537));
#43996=CARTESIAN_POINT('Ctrl Pts',(1.17528887092577,52.4469095800765,-0.0763146766143366));
#43997=CARTESIAN_POINT('Ctrl Pts',(1.17490388281053,52.4473000085032,-0.0820288478219724));
#43998=CARTESIAN_POINT('Ctrl Pts',(1.17398555018848,52.4481352398934,-0.0943214911849874));
#43999=CARTESIAN_POINT('Ctrl Pts',(1.1734385775851,52.4485793051564,-0.100898590910782));
#44000=CARTESIAN_POINT('Ctrl Pts',(1.17173841001515,52.4498249320783,-0.119452613416765));
#44001=CARTESIAN_POINT('Ctrl Pts',(1.17045689428382,52.4506198415272,-0.131417329850327));
#44002=CARTESIAN_POINT('Ctrl Pts',(1.16017889629268,52.4561425502463,-0.215226109403612));
#44003=CARTESIAN_POINT('Ctrl Pts',(1.14475617797452,52.4605871775781,-0.286135244885433));
#44004=CARTESIAN_POINT('Ctrl Pts',(1.10334909461352,52.4690676938359,-0.417043149141915));
#44005=CARTESIAN_POINT('Ctrl Pts',(1.07870747384763,52.4730843344662,-0.477172188258911));
#44006=CARTESIAN_POINT('Ctrl Pts',(1.03920859046764,52.4786778104778,-0.554642684940989));
#44007=CARTESIAN_POINT('Ctrl Pts',(1.02862395967766,52.4801147490685,-0.574034538726406));
#44008=CARTESIAN_POINT('Ctrl Pts',(1.01156639609088,52.4823475467567,-0.603297068882315));
#44009=CARTESIAN_POINT('Ctrl Pts',(1.00547964633855,52.4831296231111,-0.61338779816486));
#44010=CARTESIAN_POINT('Ctrl Pts',(0.993946682882943,52.4845860254056,-0.631874328570208));
#44011=CARTESIAN_POINT('Ctrl Pts',(0.988542856639564,52.4852587434929,-0.640295389185344));
#44012=CARTESIAN_POINT('Ctrl Pts',(0.976288643407263,52.4867637231263,-0.658866818977799));
#44013=CARTESIAN_POINT('Ctrl Pts',(0.969386004522352,52.4875978972066,-0.668981131851096));
#44014=CARTESIAN_POINT('Ctrl Pts',(0.948168023238092,52.490123254163,-0.699053400857583));
#44015=CARTESIAN_POINT('Ctrl Pts',(0.933385642879342,52.491832004635,-0.718671930163635));
#44016=CARTESIAN_POINT('Ctrl Pts',(0.863560842143729,52.4996874354691,-0.805549366790932));
#44017=CARTESIAN_POINT('Ctrl Pts',(0.801796519832233,52.5060910787434,-0.867043910169488));
#44018=CARTESIAN_POINT('Ctrl Pts',(0.707340262809247,52.5149487474114,-0.942291441033023));
#44019=CARTESIAN_POINT('Ctrl Pts',(0.679934832277706,52.5174217608351,-0.962253758450003));
#44020=CARTESIAN_POINT('Ctrl Pts',(0.634492614857426,52.5213314889796,-0.99244204340386));
#44021=CARTESIAN_POINT('Ctrl Pts',(0.616980787317879,52.5227952258801,-1.0034226024663));
#44022=CARTESIAN_POINT('Ctrl Pts',(0.592286973951487,52.5247915053365,-1.01801544976755));
#44023=CARTESIAN_POINT('Ctrl Pts',(0.58534439071844,52.5253455169918,-1.02202312539194));
#44024=CARTESIAN_POINT('Ctrl Pts',(0.573373841981408,52.5262877256026,-1.02877124668342));
#44025=CARTESIAN_POINT('Ctrl Pts',(0.56836594126289,52.52667802499,-1.03154641349479));
#44026=CARTESIAN_POINT('Ctrl Pts',(0.55753616427182,52.5275135722115,-1.03744500119894));
#44027=CARTESIAN_POINT('Ctrl Pts',(0.55170798364647,52.5279580747668,-1.04055610662811));
#44028=CARTESIAN_POINT('Ctrl Pts',(0.535164285505931,52.5292062029695,-1.04920911849396));
#44029=CARTESIAN_POINT('Ctrl Pts',(0.524389030219952,52.5300031343864,-1.05463584217562));
#44030=CARTESIAN_POINT('Ctrl Pts',(0.448812932927772,52.5354954558795,-1.09125331918974));
#44031=CARTESIAN_POINT('Ctrl Pts',(0.381349316825964,52.5399118333018,-1.11662090376679));
#44032=CARTESIAN_POINT('Ctrl Pts',(0.263441740643995,52.5474641277285,-1.14901166935567));
#44033=CARTESIAN_POINT('Ctrl Pts',(0.214095313704058,52.5505774124116,-1.15922048032076));
#44034=CARTESIAN_POINT('Ctrl Pts',(0.132483319142417,52.5558023539137,-1.17071446300197));
#44035=CARTESIAN_POINT('Ctrl Pts',(0.10054981340637,52.5578648138136,-1.17388825711982));
#44036=CARTESIAN_POINT('Ctrl Pts',(0.055083368844715,52.5608499163235,-1.17653825810153));
#44037=CARTESIAN_POINT('Ctrl Pts',(0.0416261873327244,52.5617393886215,
-1.17709119701653));
#44038=CARTESIAN_POINT('Ctrl Pts',(0.0180435346432932,52.5633100204654,
-1.17765527810999));
#44039=CARTESIAN_POINT('Ctrl Pts',(0.00792172329658865,52.5639879773732,
-1.17776685235916));
#44040=CARTESIAN_POINT('Ctrl Pts',(-0.0132305930733779,52.5654133613249,
-1.17772734036032));
#44041=CARTESIAN_POINT('Ctrl Pts',(-0.024260006717177,52.566161488916,-1.17755177143525));
#44042=CARTESIAN_POINT('Ctrl Pts',(-0.0535777682185026,52.5681638703773,
-1.17667302636727));
#44043=CARTESIAN_POINT('Ctrl Pts',(-0.0718543076942338,52.5694264254686,
-1.17569846514909));
#44044=CARTESIAN_POINT('Ctrl Pts',(-0.178276029554224,52.5768654550174,
-1.16753309495685));
#44045=CARTESIAN_POINT('Ctrl Pts',(-0.265395278060826,52.583336703185,-1.15085874104335));
#44046=CARTESIAN_POINT('Ctrl Pts',(-0.388022558047356,52.5927722468262,
-1.11271513719296));
#44047=CARTESIAN_POINT('Ctrl Pts',(-0.425605811203037,52.5957062176172,
-1.09888876059694));
#44048=CARTESIAN_POINT('Ctrl Pts',(-0.483506222500621,52.6002324317384,
-1.07417073193855));
#44049=CARTESIAN_POINT('Ctrl Pts',(-0.50433272120519,52.6018615488285,-1.06455140660277));
#44050=CARTESIAN_POINT('Ctrl Pts',(-0.532314880737407,52.604039659617,-1.05062131969466));
#44051=CARTESIAN_POINT('Ctrl Pts',(-0.539724026125907,52.6046153205837,
-1.04683440685455));
#44052=CARTESIAN_POINT('Ctrl Pts',(-0.552202372741598,52.6055822602989,
-1.04028885171864));
#44053=CARTESIAN_POINT('Ctrl Pts',(-0.557292465125318,52.6059759386204,
-1.03757094688395));
#44054=CARTESIAN_POINT('Ctrl Pts',(-0.568036310353754,52.6068050611806,
-1.03173228578991));
#44055=CARTESIAN_POINT('Ctrl Pts',(-0.573684666523248,52.6072399311722,
-1.02860228843668));
#44056=CARTESIAN_POINT('Ctrl Pts',(-0.589482160810121,52.6084541221585,
-1.01967760498855));
#44057=CARTESIAN_POINT('Ctrl Pts',(-0.59957151791268,52.609227168136,-1.01377791281077));
#44058=CARTESIAN_POINT('Ctrl Pts',(-0.6756449725309,52.6150505490144,-0.967761326719216));
#44059=CARTESIAN_POINT('Ctrl Pts',(-0.737636419225367,52.6197734007477,
-0.921386932537127));
#44060=CARTESIAN_POINT('Ctrl Pts',(-0.829699530287199,52.6274810253954,
-0.837227105559554));
#44061=CARTESIAN_POINT('Ctrl Pts',(-0.862780206981749,52.6304255373881,
-0.803094284217346));
#44062=CARTESIAN_POINT('Ctrl Pts',(-0.913869488520139,52.6354055286484,
-0.743569677874498));
#44063=CARTESIAN_POINT('Ctrl Pts',(-0.933095162374441,52.6373980600136,
-0.719295817203522));
#44064=CARTESIAN_POINT('Ctrl Pts',(-0.959183015201604,52.6403000565938,
-0.683549523304943));
#44065=CARTESIAN_POINT('Ctrl Pts',(-0.966841827787528,52.6411789369416,
-0.67267292470351));
#44066=CARTESIAN_POINT('Ctrl Pts',(-0.979988850585412,52.6427375424247,
-0.653313804693735));
#44067=CARTESIAN_POINT('Ctrl Pts',(-0.985555296836889,52.6434142230881,
-0.64488589737217));
#44068=CARTESIAN_POINT('Ctrl Pts',(-0.997013933526051,52.6448436619321,
-0.627041974460064));
#44069=CARTESIAN_POINT('Ctrl Pts',(-1.00288266274385,52.6455972053521,-0.617612152854169));
#44070=CARTESIAN_POINT('Ctrl Pts',(-1.01825954509646,52.6476311130092,-0.592107534069492));
#44071=CARTESIAN_POINT('Ctrl Pts',(-1.02751982289569,52.6489202504077,-0.575887816198061));
#44072=CARTESIAN_POINT('Ctrl Pts',(-1.07683240714013,52.6561610300914,-0.484536371018312));
#44073=CARTESIAN_POINT('Ctrl Pts',(-1.10902523012598,52.6623820201597,-0.40546485929945));
#44074=CARTESIAN_POINT('Ctrl Pts',(-1.14891734725186,52.6730502323373,-0.265879183905796));
#44075=CARTESIAN_POINT('Ctrl Pts',(-1.16098181726994,52.6774576454823,-0.206943067781209));
#44076=CARTESIAN_POINT('Ctrl Pts',(-1.16988231714256,52.6824596230565,-0.136356027284769));
#44077=CARTESIAN_POINT('Ctrl Pts',(-1.1711123190639,52.6832312701991,-0.125353742089219));
#44078=CARTESIAN_POINT('Ctrl Pts',(-1.17280139608191,52.6844315634296,-0.108036999848024));
#44079=CARTESIAN_POINT('Ctrl Pts',(-1.17336497576778,52.6848655176651,-0.101733703162982));
#44080=CARTESIAN_POINT('Ctrl Pts',(-1.17434421353911,52.6856888119471,-0.0896876613545392));
#44081=CARTESIAN_POINT('Ctrl Pts',(-1.17476860849671,52.6860785819563,-0.0839459731359289));
#44082=CARTESIAN_POINT('Ctrl Pts',(-1.17562870439996,52.6869504316642,-0.0710210924314333));
#44083=CARTESIAN_POINT('Ctrl Pts',(-1.17604071466418,52.6874312374448,-0.0638364323985576));
#44084=CARTESIAN_POINT('Ctrl Pts',(-1.17728569655548,52.6891490811008,-0.0379824828622398));
#44085=CARTESIAN_POINT('Ctrl Pts',(-1.17774021203685,52.690367539285,-0.0192967495721671));
#44086=CARTESIAN_POINT('Ctrl Pts',(-1.177765383676,52.6935106954921,0.0295479765876257));
#44087=CARTESIAN_POINT('Ctrl Pts',(-1.17662279298064,52.6954090192095,0.0596943640464959));
#44088=CARTESIAN_POINT('Ctrl Pts',(-1.16665160274001,52.7035653177381,0.190138925176396));
#44089=CARTESIAN_POINT('Ctrl Pts',(-1.14614359440823,52.7096447395677,0.289107353461203));
#44090=CARTESIAN_POINT('Ctrl Pts',(-1.1069223761335,52.7174095186163,0.402740667361204));
#44091=CARTESIAN_POINT('Ctrl Pts',(-1.10008570165631,52.7186852023949,0.421056492495837));
#44092=CARTESIAN_POINT('Ctrl Pts',(-1.08854936552971,52.720727897612,0.449761124136841));
#44093=CARTESIAN_POINT('Ctrl Pts',(-1.08414906377245,52.7214849071075,0.460266859746315));
#44094=CARTESIAN_POINT('Ctrl Pts',(-1.07598536042091,52.7228518873122,0.478990853052281));
#44095=CARTESIAN_POINT('Ctrl Pts',(-1.0722783664773,52.7234598907621,0.487232829396527));
#44096=CARTESIAN_POINT('Ctrl Pts',(-1.06331458279389,52.724901311142,0.506564671582463));
#44097=CARTESIAN_POINT('Ctrl Pts',(-1.05797866462153,52.7257374110049,0.517616454231129));
#44098=CARTESIAN_POINT('Ctrl Pts',(-1.04138067273157,52.7282752519403,0.550665049211453));
#44099=CARTESIAN_POINT('Ctrl Pts',(-1.0295986908514,52.7299948211154,0.572391543384777));
#44100=CARTESIAN_POINT('Ctrl Pts',(-1.00009407038046,52.7341206444383,0.622937094852221));
#44101=CARTESIAN_POINT('Ctrl Pts',(-0.981796545910135,52.7365447117542,
0.651393873575988));
#44102=CARTESIAN_POINT('Ctrl Pts',(-0.9357858472675,52.742332496937,0.716599655269995));
#44103=CARTESIAN_POINT('Ctrl Pts',(-0.907092886474679,52.745716412,0.752590439792059));
#44104=CARTESIAN_POINT('Ctrl Pts',(-0.841681774006431,52.7529082628366,
0.82544716812205));
#44105=CARTESIAN_POINT('Ctrl Pts',(-0.804472417794417,52.7567072643138,
0.861751898845221));
#44106=CARTESIAN_POINT('Ctrl Pts',(-0.75525251976073,52.761280319611,0.90379895186724));
#44107=CARTESIAN_POINT('Ctrl Pts',(-0.745384484517787,52.7621762430078,
0.911954449290143));
#44108=CARTESIAN_POINT('Ctrl Pts',(-0.730102805533488,52.763529651934,0.924170268881754));
#44109=CARTESIAN_POINT('Ctrl Pts',(-0.724784220297454,52.7639945563068,
0.928347258420498));
#44110=CARTESIAN_POINT('Ctrl Pts',(-0.714964456120256,52.7648412920009,
0.935923446115648));
#44111=CARTESIAN_POINT('Ctrl Pts',(-0.710474597256807,52.7652240139641,
0.939336318406548));
#44112=CARTESIAN_POINT('Ctrl Pts',(-0.6997845538992,52.7661250549968,0.947341630503309));
#44113=CARTESIAN_POINT('Ctrl Pts',(-0.693563506578452,52.7666414525874,
0.951905592581376));
#44114=CARTESIAN_POINT('Ctrl Pts',(-0.672167972268608,52.7683921727246,
0.9672809354685));
#44115=CARTESIAN_POINT('Ctrl Pts',(-0.656781211079435,52.7696083594457,
0.97779380433841));
#44116=CARTESIAN_POINT('Ctrl Pts',(-0.616856105134819,52.7726742557191,
1.00370434311688));
#44117=CARTESIAN_POINT('Ctrl Pts',(-0.591986822373387,52.7745004791876,
1.01857040900352));
#44118=CARTESIAN_POINT('Ctrl Pts',(-0.486247786169047,52.7820300819112,
1.07659531867141));
#44119=CARTESIAN_POINT('Ctrl Pts',(-0.401034484189394,52.78757098048,1.11115510814235));
#44120=CARTESIAN_POINT('Ctrl Pts',(-0.287138849598926,52.795116869945,1.14251823880059));
#44121=CARTESIAN_POINT('Ctrl Pts',(-0.261373673642282,52.7968303492206,
1.14868632871186));
#44122=CARTESIAN_POINT('Ctrl Pts',(-0.223093649708061,52.7993982344904,
1.15649584918497));
#44123=CARTESIAN_POINT('Ctrl Pts',(-0.21072427367824,52.8002313096336,1.1588134819001));
#44124=CARTESIAN_POINT('Ctrl Pts',(-0.188438782848915,52.8017393902313,
1.16262048236914));
#44125=CARTESIAN_POINT('Ctrl Pts',(-0.178536166173565,52.8024120280386,
1.16418228278888));
#44126=CARTESIAN_POINT('Ctrl Pts',(-0.157212049413898,52.8038664527557,
1.16726697203663));
#44127=CARTESIAN_POINT('Ctrl Pts',(-0.145785800531673,52.804649457314,1.16874903051094));
#44128=CARTESIAN_POINT('Ctrl Pts',(-0.113731958332498,52.80685710428,1.17242927023569));
#44129=CARTESIAN_POINT('Ctrl Pts',(-0.0930662321954791,52.808293312736,
1.17425037081808));
#44130=CARTESIAN_POINT('Ctrl Pts',(-0.0458985163730122,52.8116024769584,
1.17715397474442));
#44131=CARTESIAN_POINT('Ctrl Pts',(-0.0193870819109981,52.8134848556146,
1.17788883912925));
#44132=CARTESIAN_POINT('Ctrl Pts',(0.0680534839491707,52.8197631486888,
1.1773598461867));
#44133=CARTESIAN_POINT('Ctrl Pts',(0.128840879173521,52.8242451618814,1.17226371691588));
#44134=CARTESIAN_POINT('Ctrl Pts',(0.188938518720853,52.8287166258961,1.16249614994785));
#44135=CARTESIAN_POINT('Ctrl Pts',(0.188938438127302,52.9266130464139,1.16249616304658));
#44136=CARTESIAN_POINT('Ctrl Pts',(0.181906598859068,52.9260933627305,1.16363903540241));
#44137=CARTESIAN_POINT('Ctrl Pts',(0.17486314581592,52.9255746504092,1.1647183075498));
#44138=CARTESIAN_POINT('Ctrl Pts',(0.13621166039432,52.9227394587882,1.17028224020324));
#44139=CARTESIAN_POINT('Ctrl Pts',(0.10443945363839,52.9204498064909,1.1735445955169));
#44140=CARTESIAN_POINT('Ctrl Pts',(0.0633266670875664,52.917569703251,1.17608272809651));
#44141=CARTESIAN_POINT('Ctrl Pts',(0.0540753257050632,52.9169270140479,
1.17654439901917));
#44142=CARTESIAN_POINT('Ctrl Pts',(0.0388801636704436,52.9158812967143,
1.17712306832208));
#44143=CARTESIAN_POINT('Ctrl Pts',(0.0329393436406825,52.9154749349046,
1.17730428947039));
#44144=CARTESIAN_POINT('Ctrl Pts',(0.0216221551707913,52.9147058577791,
1.17756377788745));
#44145=CARTESIAN_POINT('Ctrl Pts',(0.0162462129984789,52.9143426743784,
1.17765021635223));
#44146=CARTESIAN_POINT('Ctrl Pts',(0.00149830396955103,52.9133517724962,
1.17778633407267));
#44147=CARTESIAN_POINT('Ctrl Pts',(-0.00787419318824625,52.9127280487827,
1.17776097090682));
#44148=CARTESIAN_POINT('Ctrl Pts',(-0.0478188541366931,52.9100915902299,
1.17717599981353));
#44149=CARTESIAN_POINT('Ctrl Pts',(-0.0783657939029402,52.9081297142182,
1.17553780081192));
#44150=CARTESIAN_POINT('Ctrl Pts',(-0.19289970007592,52.9008637378609,1.16491010448066));
#44151=CARTESIAN_POINT('Ctrl Pts',(-0.275901630913065,52.8957642627541,
1.14808774296736));
#44152=CARTESIAN_POINT('Ctrl Pts',(-0.396061866709044,52.8878529163917,
1.10993793189134));
#44153=CARTESIAN_POINT('Ctrl Pts',(-0.435030549143859,52.8852017812498,
1.09525115356684));
#44154=CARTESIAN_POINT('Ctrl Pts',(-0.486562206428158,52.8815257603364,
1.07264494802227));
#44155=CARTESIAN_POINT('Ctrl Pts',(-0.499875174370029,52.8805602674396,
1.06650585735951));
#44156=CARTESIAN_POINT('Ctrl Pts',(-0.522351270285795,52.8789011177469,
1.05562803140338));
#44157=CARTESIAN_POINT('Ctrl Pts',(-0.531573265884883,52.8782118350317,
1.05101438700445));
#44158=CARTESIAN_POINT('Ctrl Pts',(-0.549058018298693,52.8768879806953,
1.04197800704493));
#44159=CARTESIAN_POINT('Ctrl Pts',(-0.557330925851231,52.8762542006003,
1.0375765537301));
#44160=CARTESIAN_POINT('Ctrl Pts',(-0.578883214502724,52.8745830974489,
1.02577791508226));
#44161=CARTESIAN_POINT('Ctrl Pts',(-0.592073072739325,52.8735401724103,
1.01822175665989));
#44162=CARTESIAN_POINT('Ctrl Pts',(-0.642883879259474,52.86944096029,0.987792357298786));
#44163=CARTESIAN_POINT('Ctrl Pts',(-0.6793526504809,52.8663192799724,0.963074540591081));
#44164=CARTESIAN_POINT('Ctrl Pts',(-0.777206008517299,52.8574358252869,
0.88842353066654));
#44165=CARTESIAN_POINT('Ctrl Pts',(-0.835069758050751,52.8515600969101,
0.834267775943299));
#44166=CARTESIAN_POINT('Ctrl Pts',(-0.908417975346589,52.843460625658,0.750283320685518));
#44167=CARTESIAN_POINT('Ctrl Pts',(-0.928748479518946,52.8411317482933,
0.724965472104622));
#44168=CARTESIAN_POINT('Ctrl Pts',(-0.953531150504212,52.8382109928372,
0.691346529663212));
#44169=CARTESIAN_POINT('Ctrl Pts',(-0.958964730488236,52.8375651241213,
0.683789688826118));
#44170=CARTESIAN_POINT('Ctrl Pts',(-0.967725769423283,52.8365156122482,
0.671295262164273));
#44171=CARTESIAN_POINT('Ctrl Pts',(-0.971106294035118,52.8361085902616,
0.666395576711511));
#44172=CARTESIAN_POINT('Ctrl Pts',(-0.977887037183352,52.8352882912651,
0.656406476846597));
#44173=CARTESIAN_POINT('Ctrl Pts',(-0.98128499976818,52.8348751575827,0.65131580194277));
#44174=CARTESIAN_POINT('Ctrl Pts',(-0.990184077780535,52.833786982268,0.637755860543223));
#44175=CARTESIAN_POINT('Ctrl Pts',(-0.995616347847002,52.8331162808337,
0.629241726607294));
#44176=CARTESIAN_POINT('Ctrl Pts',(-1.02300423154385,52.8296951949845,0.585073162091319));
#44177=CARTESIAN_POINT('Ctrl Pts',(-1.04315893103414,52.8270421033696,0.54833244859142));
#44178=CARTESIAN_POINT('Ctrl Pts',(-1.09356505759076,52.8197806544029,0.443558471921142));
#44179=CARTESIAN_POINT('Ctrl Pts',(-1.11939110898145,52.8152606228773,0.373620702405441));
#44180=CARTESIAN_POINT('Ctrl Pts',(-1.14530267813639,52.8089004472211,0.275849202589395));
#44181=CARTESIAN_POINT('Ctrl Pts',(-1.15127349530915,52.807200868551,0.249760295454077));
#44182=CARTESIAN_POINT('Ctrl Pts',(-1.16031292406317,52.8041302438282,0.202990156727357));
#44183=CARTESIAN_POINT('Ctrl Pts',(-1.16372922625291,52.8027696076362,0.182387739896717));
#44184=CARTESIAN_POINT('Ctrl Pts',(-1.16818135313701,52.8006300127655,0.150268824493119));
#44185=CARTESIAN_POINT('Ctrl Pts',(-1.169598416476,52.7998630300252,0.138808939472798));
#44186=CARTESIAN_POINT('Ctrl Pts',(-1.17192991205189,52.7984205694787,0.117370038574803));
#44187=CARTESIAN_POINT('Ctrl Pts',(-1.17288593598726,52.7977464684418,0.10739653220063));
#44188=CARTESIAN_POINT('Ctrl Pts',(-1.17475178551673,52.7962195123387,0.0849150313132307));
#44189=CARTESIAN_POINT('Ctrl Pts',(-1.17558929322518,52.7953644665255,0.0724024339286911));
#44190=CARTESIAN_POINT('Ctrl Pts',(-1.17725342309204,52.7931162398901,0.0397134172702676));
#44191=CARTESIAN_POINT('Ctrl Pts',(-1.17776119790702,52.7917134245488,0.0195256588717659));
#44192=CARTESIAN_POINT('Ctrl Pts',(-1.17772228042435,52.7868666274024,-0.0494890055778496));
#44193=CARTESIAN_POINT('Ctrl Pts',(-1.1746586924823,52.7833516387715,-0.098259350422583));
#44194=CARTESIAN_POINT('Ctrl Pts',(-1.15759350849066,52.7733518789253,-0.234202272227691));
#44195=CARTESIAN_POINT('Ctrl Pts',(-1.13681386911742,52.7667721350037,-0.320201156339612));
#44196=CARTESIAN_POINT('Ctrl Pts',(-1.10255237704474,52.7597157197357,-0.414264533395263));
#44197=CARTESIAN_POINT('Ctrl Pts',(-1.09830753023619,52.7588838258475,-0.425390930887397));
#44198=CARTESIAN_POINT('Ctrl Pts',(-1.09145915320445,52.7576068648468,-0.44255526823521));
#44199=CARTESIAN_POINT('Ctrl Pts',(-1.08897272250366,52.7571555419762,-0.448638678052654));
#44200=CARTESIAN_POINT('Ctrl Pts',(-1.08422234434106,52.7563162664717,-0.459988944599663));
#44201=CARTESIAN_POINT('Ctrl Pts',(-1.08197077739439,52.7559276738912,-0.465260313648089));
#44202=CARTESIAN_POINT('Ctrl Pts',(-1.07645466363868,52.7549971134014,-0.477918011817304));
#44203=CARTESIAN_POINT('Ctrl Pts',(-1.07315249237172,52.7544573812662,-0.485287549991492));
#44204=CARTESIAN_POINT('Ctrl Pts',(-1.06094994788232,52.7525220392577,-0.511786471750085));
#44205=CARTESIAN_POINT('Ctrl Pts',(-1.05161123212238,52.7511501130849,-0.530710966313526));
#44206=CARTESIAN_POINT('Ctrl Pts',(-1.02544017024571,52.7475529811635,-0.580338550912572));
#44207=CARTESIAN_POINT('Ctrl Pts',(-1.00773850964026,52.7453627920869,-0.610560229967278));
#44208=CARTESIAN_POINT('Ctrl Pts',(-0.939049798397481,52.7375157395071,
-0.716683504310696));
#44209=CARTESIAN_POINT('Ctrl Pts',(-0.880624762888923,52.7319590957658,
-0.787368210049975));
#44210=CARTESIAN_POINT('Ctrl Pts',(-0.79978879547614,52.7247427456121,-0.864785772890295));
#44211=CARTESIAN_POINT('Ctrl Pts',(-0.784593666891378,52.7234049457621,
-0.878595041350704));
#44212=CARTESIAN_POINT('Ctrl Pts',(-0.760265293487885,52.7212858331393,
-0.899569986643057));
#44213=CARTESIAN_POINT('Ctrl Pts',(-0.751373440706584,52.7205158724955,
-0.90701015090022));
#44214=CARTESIAN_POINT('Ctrl Pts',(-0.734598769735623,52.7190707807433,
-0.920630221515992));
#44215=CARTESIAN_POINT('Ctrl Pts',(-0.726744094783247,52.7183970730516,
-0.926843226888218));
#44216=CARTESIAN_POINT('Ctrl Pts',(-0.708928539050146,52.7168749934932,
-0.940569528396011));
#44217=CARTESIAN_POINT('Ctrl Pts',(-0.698925713276865,52.7160244908762,
-0.948026127034976));
#44218=CARTESIAN_POINT('Ctrl Pts',(-0.667820044868065,52.7133910495522,
-0.970453944445982));
#44219=CARTESIAN_POINT('Ctrl Pts',(-0.646342065953354,52.7115882187465,
-0.984888939333304));
#44220=CARTESIAN_POINT('Ctrl Pts',(-0.593767799108988,52.7072093180907,
-1.01776259932172));
#44221=CARTESIAN_POINT('Ctrl Pts',(-0.562265037543508,52.7046122034898,
-1.03549917241062));
#44222=CARTESIAN_POINT('Ctrl Pts',(-0.491542845406176,52.6988542375696,
-1.07113730572529));
#44223=CARTESIAN_POINT('Ctrl Pts',(-0.452053674883491,52.6956845642826,
-1.08839180976296));
#44224=CARTESIAN_POINT('Ctrl Pts',(-0.364074766241985,52.6887883924813,
-1.12121792668024));
#44225=CARTESIAN_POINT('Ctrl Pts',(-0.315334080498396,52.6850712455849,
-1.13588970763363));
#44226=CARTESIAN_POINT('Ctrl Pts',(-0.253380478849017,52.6805793668379,
-1.15024160693782));
#44227=CARTESIAN_POINT('Ctrl Pts',(-0.240920698487838,52.67968763602,-1.1529157260412));
#44228=CARTESIAN_POINT('Ctrl Pts',(-0.221798439052521,52.6783392869666,
-1.15669618521147));
#44229=CARTESIAN_POINT('Ctrl Pts',(-0.215166182252834,52.6778753276757,
-1.15794824241359));
#44230=CARTESIAN_POINT('Ctrl Pts',(-0.202972377554019,52.6770295320652,
-1.16014183902186));
#44231=CARTESIAN_POINT('Ctrl Pts',(-0.197414530335856,52.676646817697,-1.16110050288303));
#44232=CARTESIAN_POINT('Ctrl Pts',(-0.184222789972167,52.6757448044647,
-1.16327846220754));
#44233=CARTESIAN_POINT('Ctrl Pts',(-0.176583463842287,52.6752274427226,
-1.16446258222668));
#44234=CARTESIAN_POINT('Ctrl Pts',(-0.150390429735297,52.6734689071876,
-1.16825888486413));
#44235=CARTESIAN_POINT('Ctrl Pts',(-0.131785346967884,52.672246091833,-1.17050366044697));
#44236=CARTESIAN_POINT('Ctrl Pts',(-0.0840621937397945,52.6691583607835,
-1.17510919383224));
#44237=CARTESIAN_POINT('Ctrl Pts',(-0.0548947492583419,52.6673173603891,
-1.17683255119244));
#44238=CARTESIAN_POINT('Ctrl Pts',(0.0677091935300681,52.6596638094872,
-1.17950769661));
#44239=CARTESIAN_POINT('Ctrl Pts',(0.161016125991956,52.6540171461394,-1.17042582142129));
#44240=CARTESIAN_POINT('Ctrl Pts',(0.276759310421148,52.6464321961513,-1.14504493454523));
#44241=CARTESIAN_POINT('Ctrl Pts',(0.301069189325804,52.6448075706934,-1.13889455992838));
#44242=CARTESIAN_POINT('Ctrl Pts',(0.337018175520609,52.6423470641,-1.1285680988567));
#44243=CARTESIAN_POINT('Ctrl Pts',(0.348818717861868,52.6415299179226,-1.1249767496357));
#44244=CARTESIAN_POINT('Ctrl Pts',(0.370086596117126,52.6400388299362,-1.1181373390153));
#44245=CARTESIAN_POINT('Ctrl Pts',(0.379573181725984,52.6393670230533,-1.11495263871227));
#44246=CARTESIAN_POINT('Ctrl Pts',(0.400064109053508,52.6379007505945,-1.10778189885467));
#44247=CARTESIAN_POINT('Ctrl Pts',(0.41105183340377,52.6371048860821,-1.10375196475852));
#44248=CARTESIAN_POINT('Ctrl Pts',(0.442218638734939,52.634818956425,-1.09179109261006));
#44249=CARTESIAN_POINT('Ctrl Pts',(0.462240326416332,52.6333159521476,-1.08346614468807));
#44250=CARTESIAN_POINT('Ctrl Pts',(0.50771928533553,52.6298197399259,-1.06306610536183));
#44251=CARTESIAN_POINT('Ctrl Pts',(0.532995152792648,52.6278154460824,-1.05062094735149));
#44252=CARTESIAN_POINT('Ctrl Pts',(0.632455545667665,52.6196863061562,-0.997136088127851));
#44253=CARTESIAN_POINT('Ctrl Pts',(0.702552210371302,52.6133769405874,-0.949051606142162));
#44254=CARTESIAN_POINT('Ctrl Pts',(0.789835286476483,52.6050368306206,-0.87416830964758));
#44255=CARTESIAN_POINT('Ctrl Pts',(0.812027254455015,52.602869659613,-0.853593626583031));
#44256=CARTESIAN_POINT('Ctrl Pts',(0.840006537915129,52.6001002051549,-0.825573370914851));
#44257=CARTESIAN_POINT('Ctrl Pts',(0.84653031502051,52.5994516805885,-0.818882662053815));
#44258=CARTESIAN_POINT('Ctrl Pts',(0.856677758948102,52.5984394976818,-0.808224678025534));
#44259=CARTESIAN_POINT('Ctrl Pts',(0.860354932776254,52.5980719799747,-0.804309210084399));
#44260=CARTESIAN_POINT('Ctrl Pts',(0.868048115189813,52.5973017948987,-0.796004348983089));
#44261=CARTESIAN_POINT('Ctrl Pts',(0.872057897725546,52.5968996309935,-0.791609423695176));
#44262=CARTESIAN_POINT('Ctrl Pts',(0.882243505568154,52.5958755838328,-0.780274158625251));
#44263=CARTESIAN_POINT('Ctrl Pts',(0.888370990041231,52.5952571566659,-0.773290607286997));
#44264=CARTESIAN_POINT('Ctrl Pts',(0.915398026528667,52.5925147233279,-0.741742324743234));
#44265=CARTESIAN_POINT('Ctrl Pts',(0.935367755335194,52.5904481448974,-0.716395687755391));
#44266=CARTESIAN_POINT('Ctrl Pts',(0.999881325762435,52.5835056864066,-0.627206563362836));
#44267=CARTESIAN_POINT('Ctrl Pts',(1.03912921748367,52.5787907983908,-0.55978768652984));
#44268=CARTESIAN_POINT('Ctrl Pts',(1.09023205448077,52.5710944043338,-0.447814112016011));
#44269=CARTESIAN_POINT('Ctrl Pts',(1.1066321696032,52.5682226168149,-0.405595841143059));
#44270=CARTESIAN_POINT('Ctrl Pts',(1.12527327894334,52.5642731892322,-0.347978999651666));
#44271=CARTESIAN_POINT('Ctrl Pts',(1.12970034055336,52.5632664814413,-0.33332632872761));
#44272=CARTESIAN_POINT('Ctrl Pts',(1.13638019880628,52.5616272775998,-0.309553316830945));
#44273=CARTESIAN_POINT('Ctrl Pts',(1.13881171790684,52.5610006195028,-0.300484732831128));
#44274=CARTESIAN_POINT('Ctrl Pts',(1.14368147155595,52.5596794277044,-0.281413807457504));
#44275=CARTESIAN_POINT('Ctrl Pts',(1.14609748590941,52.5589842382201,-0.271406669912734));
#44276=CARTESIAN_POINT('Ctrl Pts',(1.15161387722742,52.5572952549841,-0.247169235243929));
#44277=CARTESIAN_POINT('Ctrl Pts',(1.15458201295071,52.5562973360079,-0.232910916611048));
#44278=CARTESIAN_POINT('Ctrl Pts',(1.16484487403713,52.552476589013,-0.178578995901162));
#44279=CARTESIAN_POINT('Ctrl Pts',(1.17032276321948,52.5495981822774,-0.138195512783588));
#44280=CARTESIAN_POINT('Ctrl Pts',(1.18032627252935,52.5409179343216,-0.0179137724509621));
#44281=CARTESIAN_POINT('Ctrl Pts',(1.17881891960564,52.5349795580874,0.0622509924898277));
#44282=CARTESIAN_POINT('Ctrl Pts',(1.16494913882073,52.5265799410599,0.176747227426));
#44283=CARTESIAN_POINT('Ctrl Pts',(1.15911560859603,52.5240336215335,0.211654354553783));
#44284=CARTESIAN_POINT('Ctrl Pts',(1.1496771754735,52.5208720834665,0.255798387554034));
#44285=CARTESIAN_POINT('Ctrl Pts',(1.14751663792708,52.5201935471815,0.265322453529812));
#44286=CARTESIAN_POINT('Ctrl Pts',(1.14382632806066,52.5191048925738,0.280700878711885));
#44287=CARTESIAN_POINT('Ctrl Pts',(1.14236952194913,52.518690924289,0.286572035587541));
#44288=CARTESIAN_POINT('Ctrl Pts',(1.13937402648438,52.5178705985368,0.298258393139576));
#44289=CARTESIAN_POINT('Ctrl Pts',(1.13783589650262,52.5174642283304,0.304073540059658));
#44290=CARTESIAN_POINT('Ctrl Pts',(1.13372592377178,52.5164152220568,0.319143948115073));
#44291=CARTESIAN_POINT('Ctrl Pts',(1.1310852253008,52.5157763811104,0.328380203120146));
#44292=CARTESIAN_POINT('Ctrl Pts',(1.11790393628216,52.5127440364702,0.372437057665053));
#44293=CARTESIAN_POINT('Ctrl Pts',(1.10586573671166,52.5104240431187,0.406792434895543));
#44294=CARTESIAN_POINT('Ctrl Pts',(1.05329926740777,52.5016009234835,0.53712380592191));
#44295=CARTESIAN_POINT('Ctrl Pts',(1.00170711262517,52.4953503630184,0.628112222109145));
#44296=CARTESIAN_POINT('Ctrl Pts',(0.925094626857716,52.4872015735636,0.729254279172741));
#44297=CARTESIAN_POINT('Ctrl Pts',(0.910847009357528,52.4857247634979,0.746973553409694));
#44298=CARTESIAN_POINT('Ctrl Pts',(0.888281837209385,52.4834347985403,0.773430963462203));
#44299=CARTESIAN_POINT('Ctrl Pts',(0.880327556883455,52.4826362885093,0.782472652677561));
#44300=CARTESIAN_POINT('Ctrl Pts',(0.865517796643294,52.4811641730241,0.798795327606991));
#44301=CARTESIAN_POINT('Ctrl Pts',(0.858705483207773,52.480492425786,0.806114082598959));
#44302=CARTESIAN_POINT('Ctrl Pts',(0.843539836985375,52.4790081181306,0.821996779447248));
#44303=CARTESIAN_POINT('Ctrl Pts',(0.835147626903749,52.4781939095742,0.830521874948095));
#44304=CARTESIAN_POINT('Ctrl Pts',(0.810216809466123,52.4757948151914,0.855087456784489));
#44305=CARTESIAN_POINT('Ctrl Pts',(0.793336485999797,52.4741948854623,0.870771455473966));
#44306=CARTESIAN_POINT('Ctrl Pts',(0.695115777203812,52.4650151243897,0.956803523791352));
#44307=CARTESIAN_POINT('Ctrl Pts',(0.604907023323138,52.4570043680273,1.01623754623564));
#44308=CARTESIAN_POINT('Ctrl Pts',(0.478168302727825,52.4467924540513,1.07681817625857));
#44309=CARTESIAN_POINT('Ctrl Pts',(0.447831796083334,52.444423703512,1.08978410638973));
#44310=CARTESIAN_POINT('Ctrl Pts',(0.408004685847074,52.4414427077446,1.10486176258627));
#44311=CARTESIAN_POINT('Ctrl Pts',(0.398979255703781,52.4407755216141,1.10815292568126));
#44312=CARTESIAN_POINT('Ctrl Pts',(0.384799070346671,52.4397413779465,1.11312808039989));
#44313=CARTESIAN_POINT('Ctrl Pts',(0.379671473402264,52.4393702858129,1.11488744867132));
#44314=CARTESIAN_POINT('Ctrl Pts',(0.368938736097225,52.4385997608268,1.11848740407647));
#44315=CARTESIAN_POINT('Ctrl Pts',(0.363331602395777,52.4382007615289,1.1203213882282));
#44316=CARTESIAN_POINT('Ctrl Pts',(0.349095760541582,52.4371961712028,1.12485953530908));
#44317=CARTESIAN_POINT('Ctrl Pts',(0.340449022952916,52.4365937761482,1.1275066738277));
#44318=CARTESIAN_POINT('Ctrl Pts',(0.303485243734229,52.4340482303545,1.13835886172159));
#44319=CARTESIAN_POINT('Ctrl Pts',(0.2748936922188,52.4321528036768,1.14559939002129));
#44320=CARTESIAN_POINT('Ctrl Pts',(0.227104160080551,52.4290600039825,1.15580898541881));
#44321=CARTESIAN_POINT('Ctrl Pts',(0.208058427749336,52.4278469008698,1.15938862518547));
#44322=CARTESIAN_POINT('Ctrl Pts',(0.188938431190144,52.4266410775339,1.16249616417406));
#44323=CARTESIAN_POINT('Origin',(0.,56.5393671147362,0.));
#44324=CARTESIAN_POINT('',(0.188969603130339,51.8285263152314,1.16268601701705));
#44325=CARTESIAN_POINT('',(0.188938462126305,51.9282531127635,1.16249615914606));
#44326=CARTESIAN_POINT('',(0.188938462403162,56.5393671147362,1.16249615910107));
#44327=CARTESIAN_POINT('',(-1.17791180984087,52.190632781682,0.00106564231497296));
#44328=CARTESIAN_POINT('Ctrl Pts',(-1.17791180984087,52.190632781682,0.00106564231497296));
#44329=CARTESIAN_POINT('Ctrl Pts',(-1.17509560602191,52.1700025203108,-0.30407589982206));
#44330=CARTESIAN_POINT('Ctrl Pts',(-0.898229779831263,52.1229140282017,
-1.00509144888255));
#44331=CARTESIAN_POINT('Ctrl Pts',(0.282546404343134,52.0493673053545,-1.36302106179178));
#44332=CARTESIAN_POINT('Ctrl Pts',(1.29832817159957,51.9699926131404,-0.501998847764824));
#44333=CARTESIAN_POINT('Ctrl Pts',(1.13850416835778,51.8963789497659,0.722572407938825));
#44334=CARTESIAN_POINT('Ctrl Pts',(0.49061617699014,51.8492235171297,1.11051665842283));
#44335=CARTESIAN_POINT('Ctrl Pts',(0.188969603130438,51.8285263152314,1.16268601701703));
#44336=CARTESIAN_POINT('Ctrl Pts',(-1.17774952282607,52.1907260775544,0.00106018062369387));
#44337=CARTESIAN_POINT('Ctrl Pts',(-1.17769032918845,52.1955572321385,0.0668181061152723));
#44338=CARTESIAN_POINT('Ctrl Pts',(-1.17212401445883,52.2004044666048,0.132462828800205));
#44339=CARTESIAN_POINT('Ctrl Pts',(-1.15963262707197,52.2056613724927,0.205972093646308));
#44340=CARTESIAN_POINT('Ctrl Pts',(-1.15806296705408,52.2062770878784,0.214621779343263));
#44341=CARTESIAN_POINT('Ctrl Pts',(-1.15493407317965,52.2074243986727,0.230828665966669));
#44342=CARTESIAN_POINT('Ctrl Pts',(-1.15339713908044,52.2079570419198,0.238389668752796));
#44343=CARTESIAN_POINT('Ctrl Pts',(-1.15060829706119,52.2088719746045,0.251450621687845));
#44344=CARTESIAN_POINT('Ctrl Pts',(-1.14939101848722,52.2092561139653,0.256957506328754));
#44345=CARTESIAN_POINT('Ctrl Pts',(-1.14662717537469,52.2100958285269,0.269048161890698));
#44346=CARTESIAN_POINT('Ctrl Pts',(-1.14506340845786,52.2105504427024,0.275627627351889));
#44347=CARTESIAN_POINT('Ctrl Pts',(-1.1403759545603,52.2118570065992,0.294621109323544));
#44348=CARTESIAN_POINT('Ctrl Pts',(-1.13710634302001,52.2127012458732,0.306998555720624));
#44349=CARTESIAN_POINT('Ctrl Pts',(-1.11855251730717,52.2171675021267,0.372867334790528));
#44350=CARTESIAN_POINT('Ctrl Pts',(-1.09969290062369,52.2206295643553,0.425284273843428));
#44351=CARTESIAN_POINT('Ctrl Pts',(-1.05271337054164,52.2278181382191,0.531560338401379));
#44352=CARTESIAN_POINT('Ctrl Pts',(-1.02399714289803,52.2315324211238,0.58497119338871));
#44353=CARTESIAN_POINT('Ctrl Pts',(-0.972067975520965,52.2376039740117,
0.665918785559562));
#44354=CARTESIAN_POINT('Ctrl Pts',(-0.951484922760657,52.2398858524232,
0.695010829204178));
#44355=CARTESIAN_POINT('Ctrl Pts',(-0.921037639220623,52.2431313858768,
0.734152550303415));
#44356=CARTESIAN_POINT('Ctrl Pts',(-0.912263281477002,52.2440530670737,
0.745027501352338));
#44357=CARTESIAN_POINT('Ctrl Pts',(-0.896754242571542,52.2456608338553,
0.763564588169125));
#44358=CARTESIAN_POINT('Ctrl Pts',(-0.890109537705958,52.2463432294325,
0.771300234377256));
#44359=CARTESIAN_POINT('Ctrl Pts',(-0.876200791494203,52.2477591689183,
0.787073429130178));
#44360=CARTESIAN_POINT('Ctrl Pts',(-0.868924647305794,52.2484931807043,
0.795098958274607));
#44361=CARTESIAN_POINT('Ctrl Pts',(-0.849724605774908,52.250413584928,0.815698107404455));
#44362=CARTESIAN_POINT('Ctrl Pts',(-0.837632464274675,52.2516070989924,
0.82811056444853));
#44363=CARTESIAN_POINT('Ctrl Pts',(-0.757202645107037,52.2594483670187,
0.907106504759963));
#44364=CARTESIAN_POINT('Ctrl Pts',(-0.681273277581618,52.2664498296871,
0.965431528704813));
#44365=CARTESIAN_POINT('Ctrl Pts',(-0.567686819930333,52.276136274248,1.03255192367435));
#44366=CARTESIAN_POINT('Ctrl Pts',(-0.535359389987347,52.2788101948645,
1.0496772939016));
#44367=CARTESIAN_POINT('Ctrl Pts',(-0.48266911596462,52.2829911610762,1.07452127169366));
#44368=CARTESIAN_POINT('Ctrl Pts',(-0.46279896966515,52.2845294175151,1.08322790429643));
#44369=CARTESIAN_POINT('Ctrl Pts',(-0.435139478996361,52.2866079736698,
1.09444745546263));
#44370=CARTESIAN_POINT('Ctrl Pts',(-0.427548748799424,52.2871720232298,
1.09743504404926));
#44371=CARTESIAN_POINT('Ctrl Pts',(-0.414559908927411,52.2881256347495,
1.10239201258553));
#44372=CARTESIAN_POINT('Ctrl Pts',(-0.409177425888736,52.2885174368609,
1.10440115335904));
#44373=CARTESIAN_POINT('Ctrl Pts',(-0.397642524409573,52.2893497030525,
1.10861092045666));
#44374=CARTESIAN_POINT('Ctrl Pts',(-0.391486202744324,52.2897895042055,
1.11079985071822));
#44375=CARTESIAN_POINT('Ctrl Pts',(-0.374230612917388,52.2910108418874,
1.11677393495456));
#44376=CARTESIAN_POINT('Ctrl Pts',(-0.363092226138677,52.2917861280334,
1.120444837762));
#44377=CARTESIAN_POINT('Ctrl Pts',(-0.279689054895377,52.2975074559658,
1.14655777292831));
#44378=CARTESIAN_POINT('Ctrl Pts',(-0.205456961507612,52.3021407684921,
1.16215799588203));
#44379=CARTESIAN_POINT('Ctrl Pts',(-0.0822393927391659,52.30980038585,1.17586718374556));
#44380=CARTESIAN_POINT('Ctrl Pts',(-0.0339651744219333,52.3127921893129,
1.17824992676322));
#44381=CARTESIAN_POINT('Ctrl Pts',(0.0455902504196925,52.3178411260906,
1.17728279789795));
#44382=CARTESIAN_POINT('Ctrl Pts',(0.0768341325579911,52.3198536061909,
1.17565705583618));
#44383=CARTESIAN_POINT('Ctrl Pts',(0.121268123307562,52.3227793350942,1.17156618523389));
#44384=CARTESIAN_POINT('Ctrl Pts',(0.134539625419161,52.3236612725303,1.17011638275284));
#44385=CARTESIAN_POINT('Ctrl Pts',(0.157809661834293,52.3252233382632,1.16717321406119));
#44386=CARTESIAN_POINT('Ctrl Pts',(0.167819125526565,52.3259003765286,1.16577610678777));
#44387=CARTESIAN_POINT('Ctrl Pts',(0.18152174898344,52.3268346504193,1.16368338578293));
#44388=CARTESIAN_POINT('Ctrl Pts',(0.185231575714379,52.3270883432989,1.16309863289516));
#44389=CARTESIAN_POINT('Ctrl Pts',(0.188938462485257,52.327342596858,1.16249615908772));
#44390=CARTESIAN_POINT('',(-1.17774983784145,52.2885366798091,-0.000618032721413477));
#44391=CARTESIAN_POINT('Ctrl Pts',(0.188938431190144,52.4266410775339,1.16249616417406));
#44392=CARTESIAN_POINT('Ctrl Pts',(0.151776937535318,52.4242974476015,1.1685359555542));
#44393=CARTESIAN_POINT('Ctrl Pts',(0.114334940736222,52.4219807809433,1.17279236171814));
#44394=CARTESIAN_POINT('Ctrl Pts',(0.0103317987625297,52.415535040879,1.17958352216524));
#44395=CARTESIAN_POINT('Ctrl Pts',(-0.056317377535304,52.4113854067649,
1.17828301993316));
#44396=CARTESIAN_POINT('Ctrl Pts',(-0.139007659187246,52.4059797257572,
1.16963565313208));
#44397=CARTESIAN_POINT('Ctrl Pts',(-0.155480588527765,52.404890484846,1.16756003360845));
#44398=CARTESIAN_POINT('Ctrl Pts',(-0.182473313775796,52.403082364707,1.16357754584739));
#44399=CARTESIAN_POINT('Ctrl Pts',(-0.193021112465399,52.4023699407749,
1.16187437049363));
#44400=CARTESIAN_POINT('Ctrl Pts',(-0.213660572531504,52.4009636371381,
1.15825287326899));
#44401=CARTESIAN_POINT('Ctrl Pts',(-0.22375320930376,52.4002701660734,1.15634555750961));
#44402=CARTESIAN_POINT('Ctrl Pts',(-0.247961293708739,52.3985922456276,
1.15144190489947));
#44403=CARTESIAN_POINT('Ctrl Pts',(-0.262048831482203,52.3976038045563,
1.14831774391731));
#44404=CARTESIAN_POINT('Ctrl Pts',(-0.314506945949762,52.3938763675163,
1.13566867702898));
#44405=CARTESIAN_POINT('Ctrl Pts',(-0.352443815663349,52.3910853182319,
1.12447352369067));
#44406=CARTESIAN_POINT('Ctrl Pts',(-0.460148504921617,52.3828868676463,
1.08670372802051));
#44407=CARTESIAN_POINT('Ctrl Pts',(-0.528045283947793,52.377363069702,1.05538056774806));
#44408=CARTESIAN_POINT('Ctrl Pts',(-0.628442439534823,52.3688701594635,
0.996936954408797));
#44409=CARTESIAN_POINT('Ctrl Pts',(-0.663240633826223,52.3658618403467,
0.974133335401085));
#44410=CARTESIAN_POINT('Ctrl Pts',(-0.704913086445368,52.3622379520388,
0.943554340942552));
#44411=CARTESIAN_POINT('Ctrl Pts',(-0.712986233733124,52.3615349063379,
0.9374688803604));
#44412=CARTESIAN_POINT('Ctrl Pts',(-0.725821580860414,52.3604168322989,
0.9275319833291));
#44413=CARTESIAN_POINT('Ctrl Pts',(-0.730633644072275,52.3599975863512,
0.923746193396292));
#44414=CARTESIAN_POINT('Ctrl Pts',(-0.740064153585596,52.3591761831589,
0.916207139592121));
#44415=CARTESIAN_POINT('Ctrl Pts',(-0.744684063678281,52.3587739111755,
0.912456093285352));
#44416=CARTESIAN_POINT('Ctrl Pts',(-0.756449312333146,52.3577492113737,
0.902754649692739));
#44417=CARTESIAN_POINT('Ctrl Pts',(-0.763553161930051,52.3571302484279,
0.896754203860163));
#44418=CARTESIAN_POINT('Ctrl Pts',(-0.795050379857613,52.3543808245062,
0.86950359687441));
#44419=CARTESIAN_POINT('Ctrl Pts',(-0.818635198461108,52.3523081537633,
0.847336074031021));
#44420=CARTESIAN_POINT('Ctrl Pts',(-0.896159246305273,52.3453223769718,
0.768207804278992));
#44421=CARTESIAN_POINT('Ctrl Pts',(-0.945308991245935,52.3405724328453,
0.70684976184605));
#44422=CARTESIAN_POINT('Ctrl Pts',(-1.01230515582932,52.3328722911216,0.603595695889756));
#44423=CARTESIAN_POINT('Ctrl Pts',(-1.03446057187771,52.330037095084,0.564783297154932));
#44424=CARTESIAN_POINT('Ctrl Pts',(-1.06115463939068,52.3261296745812,0.511154150840396));
#44425=CARTESIAN_POINT('Ctrl Pts',(-1.06768549417148,52.3251263076712,0.497368459867585));
#44426=CARTESIAN_POINT('Ctrl Pts',(-1.07779693388072,52.3234910526919,0.474907163525413));
#44427=CARTESIAN_POINT('Ctrl Pts',(-1.08154491185726,52.3228649462714,0.466308524065008));
#44428=CARTESIAN_POINT('Ctrl Pts',(-1.08919331255543,52.3215437085533,0.448173112589151));
#44429=CARTESIAN_POINT('Ctrl Pts',(-1.09307207574571,52.3208479079449,0.438628130004939));
#44430=CARTESIAN_POINT('Ctrl Pts',(-1.10214738196751,52.3191550241177,0.415427104644542));
#44431=CARTESIAN_POINT('Ctrl Pts',(-1.10721587552223,52.3181537684348,0.40172316606238));
#44432=CARTESIAN_POINT('Ctrl Pts',(-1.12558645437666,52.3142993566739,0.349062508197249));
#44433=CARTESIAN_POINT('Ctrl Pts',(-1.13709649825678,52.3113893178904,0.309516341717001));
#44434=CARTESIAN_POINT('Ctrl Pts',(-1.16731769116475,52.3018853919439,0.180926186713959));
#44435=CARTESIAN_POINT('Ctrl Pts',(-1.17779754836018,52.2950991319486,0.0903011917011576));
#44436=CARTESIAN_POINT('Ctrl Pts',(-1.17774983784145,52.2885366798091,-0.000618032721413477));
#44437=CARTESIAN_POINT('Ctrl Pts',(-1.17774983694482,52.288536556651,-0.000619739009734618));
#44438=CARTESIAN_POINT('Ctrl Pts',(-1.1777403719914,52.2872382631056,-0.0186069032548436));
#44439=CARTESIAN_POINT('Ctrl Pts',(-1.17731884383651,52.2859508669133,-0.0365926453733845));
#44440=CARTESIAN_POINT('Ctrl Pts',(-1.17593148901231,52.2838345935358,-0.0665068767745185));
#44441=CARTESIAN_POINT('Ctrl Pts',(-1.17519566071235,52.2829968513179,-0.0784424466870239));
#44442=CARTESIAN_POINT('Ctrl Pts',(-1.17383721644222,52.2817696162845,-0.0960951484339259));
#44443=CARTESIAN_POINT('Ctrl Pts',(-1.17335433743197,52.2813733305676,-0.10182185667435));
#44444=CARTESIAN_POINT('Ctrl Pts',(-1.17232804037805,52.2806027288331,-0.113014121334299));
#44445=CARTESIAN_POINT('Ctrl Pts',(-1.17178827100923,52.280228242115,-0.118479867256508));
#44446=CARTESIAN_POINT('Ctrl Pts',(-1.17052468247312,52.279414335236,-0.130420358555844));
#44447=CARTESIAN_POINT('Ctrl Pts',(-1.16978535268175,52.2789757671257,-0.1368931551809));
#44448=CARTESIAN_POINT('Ctrl Pts',(-1.16757498741823,52.2777610765878,-0.154917052144064));
#44449=CARTESIAN_POINT('Ctrl Pts',(-1.16598626240294,52.276991098589,-0.166453312947383));
#44450=CARTESIAN_POINT('Ctrl Pts',(-1.15616375299055,52.272734574301,-0.230711172826921));
#44451=CARTESIAN_POINT('Ctrl Pts',(-1.14452457587011,52.2694007019304,-0.282855252500812));
#44452=CARTESIAN_POINT('Ctrl Pts',(-1.11280521327593,52.2624721833434,-0.39009973665874));
#44453=CARTESIAN_POINT('Ctrl Pts',(-1.09207212252354,52.2588908043713,-0.444849997557872));
#44454=CARTESIAN_POINT('Ctrl Pts',(-1.05021288775303,52.2526703424289,-0.534596550502616));
#44455=CARTESIAN_POINT('Ctrl Pts',(-1.0311798510326,52.2500838596863,-0.570445600843968));
#44456=CARTESIAN_POINT('Ctrl Pts',(-1.00286230924222,52.2464830706194,-0.61771661188198));
#44457=CARTESIAN_POINT('Ctrl Pts',(-0.995157422317599,52.2455248748821,
-0.63005420234133));
#44458=CARTESIAN_POINT('Ctrl Pts',(-0.981614285113403,52.2438743723243,
-0.650872006609772));
#44459=CARTESIAN_POINT('Ctrl Pts',(-0.975889598715612,52.2431863241964,
-0.659424334816853));
#44460=CARTESIAN_POINT('Ctrl Pts',(-0.964013022111139,52.24177743545,-0.676673791131825));
#44461=CARTESIAN_POINT('Ctrl Pts',(-0.957853753611336,52.2410563578078,
-0.685364647520231));
#44462=CARTESIAN_POINT('Ctrl Pts',(-0.941890225642806,52.2392107009956,
-0.70725395770583));
#44463=CARTESIAN_POINT('Ctrl Pts',(-0.93192620100281,52.2380800151868,-0.720332468988305));
#44464=CARTESIAN_POINT('Ctrl Pts',(-0.881534318612431,52.2324609281526,
-0.78367937871711));
#44465=CARTESIAN_POINT('Ctrl Pts',(-0.837303464381893,52.2278221486448,
-0.830768708239352));
#44466=CARTESIAN_POINT('Ctrl Pts',(-0.753148904395042,52.2195277127737,
-0.906782453666861));
#44467=CARTESIAN_POINT('Ctrl Pts',(-0.714843039290224,52.2159155122293,
-0.937276422915876));
#44468=CARTESIAN_POINT('Ctrl Pts',(-0.643152045014247,52.209533125377,-0.987388980286748));
#44469=CARTESIAN_POINT('Ctrl Pts',(-0.610482887388668,52.2067510612345,
-1.00791507205607));
#44470=CARTESIAN_POINT('Ctrl Pts',(-0.568363204924382,52.2033677017779,
-1.03157809639927));
#44471=CARTESIAN_POINT('Ctrl Pts',(-0.559804545166975,52.2026903388203,
-1.03624755179716));
#44472=CARTESIAN_POINT('Ctrl Pts',(-0.545846045107572,52.2016030930085,
-1.04363964305366));
#44473=CARTESIAN_POINT('Ctrl Pts',(-0.540481687608634,52.2011893775031,
-1.04642780880987));
#44474=CARTESIAN_POINT('Ctrl Pts',(-0.53037694355811,52.2004181039419,-1.05158139093778));
#44475=CARTESIAN_POINT('Ctrl Pts',(-0.525641644892445,52.2000599462283,
-1.05395635005732));
#44476=CARTESIAN_POINT('Ctrl Pts',(-0.512875211630375,52.1991026904452,
-1.06025183084785));
#44477=CARTESIAN_POINT('Ctrl Pts',(-0.504815018707006,52.1985071249533,
-1.06411312206855));
#44478=CARTESIAN_POINT('Ctrl Pts',(-0.473087804209049,52.196194057678,-1.07887061504756));
#44479=CARTESIAN_POINT('Ctrl Pts',(-0.449104151052207,52.1945129462332,
-1.08907279828412));
#44480=CARTESIAN_POINT('Ctrl Pts',(-0.341887070871989,52.1872071361727,
-1.13053568256093));
#44481=CARTESIAN_POINT('Ctrl Pts',(-0.255607036281239,52.1818528927625,
-1.1531109208811));
#44482=CARTESIAN_POINT('Ctrl Pts',(-0.125624171152407,52.1736181012188,
-1.17179875744618));
#44483=CARTESIAN_POINT('Ctrl Pts',(-0.0833533954457211,52.1709184605159,
-1.1755617374923));
#44484=CARTESIAN_POINT('Ctrl Pts',(-0.0262408219167813,52.1671860909148,
-1.17754992843183));
#44485=CARTESIAN_POINT('Ctrl Pts',(-0.0114991196386139,52.1662152851507,
-1.17778612358545));
#44486=CARTESIAN_POINT('Ctrl Pts',(0.0135690026387033,52.1645498261323,
-1.17771710521445));
#44487=CARTESIAN_POINT('Ctrl Pts',(0.0238942854261437,52.1638596314378,
-1.17755286474316));
#44488=CARTESIAN_POINT('Ctrl Pts',(0.0448117046894879,52.1624522289535,
-1.17694491870802));
#44489=CARTESIAN_POINT('Ctrl Pts',(0.0554026549048939,52.1617348565697,
-1.17649392839258));
#44490=CARTESIAN_POINT('Ctrl Pts',(0.082141738014007,52.1599109721799,-1.17499346137691));
#44491=CARTESIAN_POINT('Ctrl Pts',(0.0982765511894411,52.1587986406084,
-1.17375405142512));
#44492=CARTESIAN_POINT('Ctrl Pts',(0.171621875077245,52.1536860080998,-1.16659711205167));
#44493=CARTESIAN_POINT('Ctrl Pts',(0.228369254966916,52.1495686203159,-1.15682696709697));
#44494=CARTESIAN_POINT('Ctrl Pts',(0.366723419396678,52.1391772254808,-1.122428396953));
#44495=CARTESIAN_POINT('Ctrl Pts',(0.446810743289781,52.1328341812726,-1.09301977991834));
#44496=CARTESIAN_POINT('Ctrl Pts',(0.537109170645427,52.125672451709,-1.04826315385924));
#44497=CARTESIAN_POINT('Ctrl Pts',(0.55104582959916,52.1245675457531,-1.0410045405235));
#44498=CARTESIAN_POINT('Ctrl Pts',(0.571178889405893,52.1229763535234,-1.03000098249192));
#44499=CARTESIAN_POINT('Ctrl Pts',(0.57749205349628,52.1224781311048,-1.02647468678925));
#44500=CARTESIAN_POINT('Ctrl Pts',(0.58868930128599,52.1215963123575,-1.02008431877586));
#44501=CARTESIAN_POINT('Ctrl Pts',(0.593585698103853,52.1212113858194,-1.01724290781309));
#44502=CARTESIAN_POINT('Ctrl Pts',(0.604638617511671,52.1203439702858,-1.01072184053095));
#44503=CARTESIAN_POINT('Ctrl Pts',(0.610782258868511,52.119862824206,-1.00702111972516));
#44504=CARTESIAN_POINT('Ctrl Pts',(0.629992400998763,52.1183602494314,-0.995209097555777));
#44505=CARTESIAN_POINT('Ctrl Pts',(0.64293462123777,52.1173507115199,-0.986897512649443));
#44506=CARTESIAN_POINT('Ctrl Pts',(0.717365879306775,52.1115382076419,-0.937011296165858));
#44507=CARTESIAN_POINT('Ctrl Pts',(0.774983511676959,52.107004151812,-0.889947778610385));
#44508=CARTESIAN_POINT('Ctrl Pts',(0.860255345979937,52.099592756026,-0.805691381819712));
#44509=CARTESIAN_POINT('Ctrl Pts',(0.890825245205523,52.0967582923776,-0.771756335652682));
#44510=CARTESIAN_POINT('Ctrl Pts',(0.938218338109724,52.0919397654832,-0.712567844610764));
#44511=CARTESIAN_POINT('Ctrl Pts',(0.956174460348708,52.0899948220292,-0.688285367962155));
#44512=CARTESIAN_POINT('Ctrl Pts',(0.980602373277928,52.0871496603094,-0.652447592520935));
#44513=CARTESIAN_POINT('Ctrl Pts',(0.987844159318308,52.0862783314602,-0.641430252712317));
#44514=CARTESIAN_POINT('Ctrl Pts',(1.00029525960691,52.0847283950172,-0.621776583646575));
#44515=CARTESIAN_POINT('Ctrl Pts',(1.00558152725818,52.0840527215541,-0.613190433330888));
#44516=CARTESIAN_POINT('Ctrl Pts',(1.01648502048386,52.082620574544,-0.594960338404486));
#44517=CARTESIAN_POINT('Ctrl Pts',(1.02207668217603,52.0818632550563,-0.585302350828057));
#44518=CARTESIAN_POINT('Ctrl Pts',(1.03678923532306,52.0798066669288,-0.559036772026138));
#44519=CARTESIAN_POINT('Ctrl Pts',(1.04564765340926,52.0784982753005,-0.542286771969206));
#44520=CARTESIAN_POINT('Ctrl Pts',(1.0907425530647,52.0714428712162,-0.45180207873871));
#44521=CARTESIAN_POINT('Ctrl Pts',(1.11958731859395,52.0654481658967,-0.374652266226838));
#44522=CARTESIAN_POINT('Ctrl Pts',(1.15569911571883,52.054858333392,-0.235149441131119));
#44523=CARTESIAN_POINT('Ctrl Pts',(1.16647140392589,52.0503038645972,-0.17401610427116));
#44524=CARTESIAN_POINT('Ctrl Pts',(1.17346852803646,52.0451408053934,-0.100977138017322));
#44525=CARTESIAN_POINT('Ctrl Pts',(1.17439015863073,52.0443463432203,-0.0896244845025087));
#44526=CARTESIAN_POINT('Ctrl Pts',(1.17557188497231,52.0431189023227,-0.0718796988791239));
#44527=CARTESIAN_POINT('Ctrl Pts',(1.17594481629151,52.042680231108,-0.0654961201234137));
#44528=CARTESIAN_POINT('Ctrl Pts',(1.17655315600599,52.0418542150555,-0.0533903239583587));
#44529=CARTESIAN_POINT('Ctrl Pts',(1.17679884593558,52.0414663620027,-0.047668995519125));
#44530=CARTESIAN_POINT('Ctrl Pts',(1.17730229496443,52.0405145247213,-0.0335422347585907));
#44531=CARTESIAN_POINT('Ctrl Pts',(1.17751178621274,52.0399531384632,-0.0251352110354523));
#44532=CARTESIAN_POINT('Ctrl Pts',(1.17794292822382,52.0379421085983,0.00521964359023661));
#44533=CARTESIAN_POINT('Ctrl Pts',(1.17764112803403,52.0365178209452,0.0271717178510554));
#44534=CARTESIAN_POINT('Ctrl Pts',(1.1738852236081,52.0307547079956,0.11717788314597));
#44535=CARTESIAN_POINT('Ctrl Pts',(1.16514259118797,52.0265936629039,0.184882192837355));
#44536=CARTESIAN_POINT('Ctrl Pts',(1.14132434971256,52.0196905084355,0.293868329754557));
#44537=CARTESIAN_POINT('Ctrl Pts',(1.12971762054493,52.0169882983758,0.335734398410216));
#44538=CARTESIAN_POINT('Ctrl Pts',(1.10646969669675,52.0123655056645,0.404567721056985));
#44539=CARTESIAN_POINT('Ctrl Pts',(1.09608433504862,52.0104796886056,0.431913352261917));
#44540=CARTESIAN_POINT('Ctrl Pts',(1.07961409093504,52.0077051256446,0.470848611551983));
#44541=CARTESIAN_POINT('Ctrl Pts',(1.07433654751678,52.0068432289193,0.482769055017956));
#44542=CARTESIAN_POINT('Ctrl Pts',(1.06463539382427,52.0053038335937,0.503733911713669));
#44543=CARTESIAN_POINT('Ctrl Pts',(1.06029157369158,52.0046291294446,0.512813946309728));
#44544=CARTESIAN_POINT('Ctrl Pts',(1.05085301851314,52.0031925222142,0.531910962571707));
#44545=CARTESIAN_POINT('Ctrl Pts',(1.04573025006512,52.0024296903396,0.541912878046723));
#44546=CARTESIAN_POINT('Ctrl Pts',(1.03140812917354,52.0003408345125,0.56891650022364));
#44547=CARTESIAN_POINT('Ctrl Pts',(1.02193241607423,51.9990051858091,0.585766824654158));
#44548=CARTESIAN_POINT('Ctrl Pts',(0.977902374343339,51.9929929596424,0.659741385520175));
#44549=CARTESIAN_POINT('Ctrl Pts',(0.938947417248091,51.9881620763671,0.714091748749712));
#44550=CARTESIAN_POINT('Ctrl Pts',(0.860344746519498,51.9792857709142,0.806132834848466));
#44551=CARTESIAN_POINT('Ctrl Pts',(0.822269868392659,51.9752749732389,0.844935380225857));
#44552=CARTESIAN_POINT('Ctrl Pts',(0.767739788395041,51.9700062307639,0.893317771083572));
#44553=CARTESIAN_POINT('Ctrl Pts',(0.753535473665955,51.968673152623,0.905331644784492));
#44554=CARTESIAN_POINT('Ctrl Pts',(0.728445017333622,51.9663931783941,0.925553077666798));
#44555=CARTESIAN_POINT('Ctrl Pts',(0.717690117892988,51.965438591955,0.933917328932445));
#44556=CARTESIAN_POINT('Ctrl Pts',(0.701316746098178,51.964021911007,0.946201212835682));
#44557=CARTESIAN_POINT('Ctrl Pts',(0.695805661787833,51.9635511410837,0.950261227464638));
#44558=CARTESIAN_POINT('Ctrl Pts',(0.685656593472072,51.9626956851575,0.957602405910396));
#44559=CARTESIAN_POINT('Ctrl Pts',(0.681029992262129,51.9623100650167,0.960898269246158));
#44560=CARTESIAN_POINT('Ctrl Pts',(0.670245717798173,51.9614210488624,0.968463668681551));
#44561=CARTESIAN_POINT('Ctrl Pts',(0.664070900610058,51.9609193070479,0.972708099163669));
#44562=CARTESIAN_POINT('Ctrl Pts',(0.643737550666441,51.9592892858567,0.986400904725979));
#44563=CARTESIAN_POINT('Ctrl Pts',(0.629413979444286,51.9581758021688,0.99560177430357));
#44564=CARTESIAN_POINT('Ctrl Pts',(0.530237200948051,51.9506637114619,1.05631253364499));
#44565=CARTESIAN_POINT('Ctrl Pts',(0.439359774789711,51.9447212659783,1.09723064688237));
#44566=CARTESIAN_POINT('Ctrl Pts',(0.302413612722851,51.935752898069,1.13910946384714));
#44567=CARTESIAN_POINT('Ctrl Pts',(0.259728364594098,51.9329607543732,1.14959336961719));
#44568=CARTESIAN_POINT('Ctrl Pts',(0.207372205591597,51.9294833560839,1.15938742853693));
#44569=CARTESIAN_POINT('Ctrl Pts',(0.19816421891786,51.928869914521,1.16099671307355));
#44570=CARTESIAN_POINT('Ctrl Pts',(0.188938462126305,51.9282531127635,1.16249615914606));
#44571=CARTESIAN_POINT('Origin',(0.,56.5393671147362,0.));
#44572=CARTESIAN_POINT('',(0.188938476720627,51.3293408135491,1.16249615677407));
#44573=CARTESIAN_POINT('',(0.18893837638019,51.427308721746,1.16249617308222));
#44574=CARTESIAN_POINT('',(0.188938462403162,56.5393671147362,1.16249615910107));
#44575=CARTESIAN_POINT('',(-1.1759637632873,51.6905636633131,-0.000120924575849058));
#44576=CARTESIAN_POINT('Ctrl Pts',(0.188938476720627,51.3293408135491,1.16249615677407));
#44577=CARTESIAN_POINT('Ctrl Pts',(0.204295852302049,51.330455194193,1.1600001492545));
#44578=CARTESIAN_POINT('Ctrl Pts',(0.219605556065176,51.3315599139334,1.15719952874471));
#44579=CARTESIAN_POINT('Ctrl Pts',(0.244849227074782,51.3333665079355,1.15206244040771));
#44580=CARTESIAN_POINT('Ctrl Pts',(0.254813562702692,51.3340757249261,1.14989959416533));
#44581=CARTESIAN_POINT('Ctrl Pts',(0.270733855217703,51.3352012759797,1.14622683936605));
#44582=CARTESIAN_POINT('Ctrl Pts',(0.276708021107776,51.3356219212953,1.14479931125938));
#44583=CARTESIAN_POINT('Ctrl Pts',(0.288436004635372,51.33644393593,1.14189973358364));
#44584=CARTESIAN_POINT('Ctrl Pts',(0.294190329613003,51.3368454438984,1.14043078830291));
#44585=CARTESIAN_POINT('Ctrl Pts',(0.308862464739228,51.3378651232474,1.13656689101226));
#44586=CARTESIAN_POINT('Ctrl Pts',(0.317763905949887,51.3384798991231,1.13411041492814));
#44587=CARTESIAN_POINT('Ctrl Pts',(0.356968644934529,51.3411742672938,1.12279347700888));
#44588=CARTESIAN_POINT('Ctrl Pts',(0.386940005314877,51.3431988982505,1.11282056608089));
#44589=CARTESIAN_POINT('Ctrl Pts',(0.485569861913291,51.3498545785977,1.07553385702165));
#44590=CARTESIAN_POINT('Ctrl Pts',(0.552054677732486,51.3543387212165,1.04297066901577));
#44591=CARTESIAN_POINT('Ctrl Pts',(0.656921200479987,51.3620050616451,0.978754222567422));
#44592=CARTESIAN_POINT('Ctrl Pts',(0.697140598540821,51.3651094298262,0.950525892203683));
#44593=CARTESIAN_POINT('Ctrl Pts',(0.747760118634869,51.3693319094633,0.910053361990254));
#44594=CARTESIAN_POINT('Ctrl Pts',(0.759843090062958,51.3703652733622,0.899989309212623));
#44595=CARTESIAN_POINT('Ctrl Pts',(0.778868986899859,51.3720361994635,0.883486113322305));
#44596=CARTESIAN_POINT('Ctrl Pts',(0.785942290698183,51.3726674692766,0.877199702457655));
#44597=CARTESIAN_POINT('Ctrl Pts',(0.80050894637034,51.3739891992263,0.863935939547535));
#44598=CARTESIAN_POINT('Ctrl Pts',(0.807988572685473,51.3746802130497,0.856944768198668));
#44599=CARTESIAN_POINT('Ctrl Pts',(0.825638188645483,51.3763412224887,0.840011250165949));
#44600=CARTESIAN_POINT('Ctrl Pts',(0.835720877618183,51.3773150033367,0.829980663980266));
#44601=CARTESIAN_POINT('Ctrl Pts',(0.871896093397634,51.3809030047322,0.792664782158837));
#44602=CARTESIAN_POINT('Ctrl Pts',(0.89685187925694,51.3835642420602,0.76431434781571));
#44603=CARTESIAN_POINT('Ctrl Pts',(0.962601441431847,51.3911198173678,0.681959202705431));
#44604=CARTESIAN_POINT('Ctrl Pts',(1.00016672617909,51.3961070886962,0.625567686225429));
#44605=CARTESIAN_POINT('Ctrl Pts',(1.05688066439141,51.4047603351659,0.522141111607394));
#44606=CARTESIAN_POINT('Ctrl Pts',(1.07822830368233,51.4084263908152,0.476500644738953));
#44607=CARTESIAN_POINT('Ctrl Pts',(1.10037299088285,51.4126857675529,0.419978327210269));
#44608=CARTESIAN_POINT('Ctrl Pts',(1.10402693406528,51.4134071443497,0.410276811301175));
#44609=CARTESIAN_POINT('Ctrl Pts',(1.10965364885438,51.4145472772309,0.394717641142936));
#44610=CARTESIAN_POINT('Ctrl Pts',(1.11170914159685,51.4149705327324,0.388890763026007));
#44611=CARTESIAN_POINT('Ctrl Pts',(1.11564160126565,51.4157934254934,0.377457062311811));
#44612=CARTESIAN_POINT('Ctrl Pts',(1.11752236302791,51.4161932493194,0.37185183444179));
#44613=CARTESIAN_POINT('Ctrl Pts',(1.12219110335492,51.4172025713412,0.357582199403794));
#44614=CARTESIAN_POINT('Ctrl Pts',(1.12492107481153,51.4178088125408,0.348898968193457));
#44615=CARTESIAN_POINT('Ctrl Pts',(1.13624379531362,51.4203984749306,0.311369536243215));
#44616=CARTESIAN_POINT('Ctrl Pts',(1.14383042014825,51.422332089449,0.282229075538648));
#44617=CARTESIAN_POINT('Ctrl Pts',(1.16451806006148,51.4284263090572,0.188106208900379));
#44618=CARTESIAN_POINT('Ctrl Pts',(1.17325643263249,51.4324659609223,0.12229687924145));
#44619=CARTESIAN_POINT('Ctrl Pts',(1.17915037553542,51.4401439341728,-0.00130084894931952));
#44620=CARTESIAN_POINT('Ctrl Pts',(1.1776827453898,51.443753398478,-0.0588175708633005));
#44621=CARTESIAN_POINT('Ctrl Pts',(1.17043043245947,51.4485457682019,-0.132096630816075));
#44622=CARTESIAN_POINT('Ctrl Pts',(1.16850507651486,51.449608273164,-0.148164643254995));
#44623=CARTESIAN_POINT('Ctrl Pts',(1.16477129821978,51.451384082156,-0.174686288475214));
#44624=CARTESIAN_POINT('Ctrl Pts',(1.16315155881476,51.4520914034204,-0.185164562659755));
#44625=CARTESIAN_POINT('Ctrl Pts',(1.15967484926206,51.4534967901287,-0.205805771127432));
#44626=CARTESIAN_POINT('Ctrl Pts',(1.15782518557047,51.4541945645206,-0.215968977508947));
#44627=CARTESIAN_POINT('Ctrl Pts',(1.15301025289662,51.4558991858753,-0.240582634548673));
#44628=CARTESIAN_POINT('Ctrl Pts',(1.14990678490847,51.456910344481,-0.255003918966528));
#44629=CARTESIAN_POINT('Ctrl Pts',(1.13682137261875,51.4608657882517,-0.310701572335646));
#44630=CARTESIAN_POINT('Ctrl Pts',(1.12488185392698,51.4638709623346,-0.351480245584576));
#44631=CARTESIAN_POINT('Ctrl Pts',(1.08111048217538,51.4733563049897,-0.475662099123581));
#44632=CARTESIAN_POINT('Ctrl Pts',(1.0419918374638,51.4800115924331,-0.556152383576708));
#44633=CARTESIAN_POINT('Ctrl Pts',(0.980357125459869,51.4883098255161,-0.653190793392505));
#44634=CARTESIAN_POINT('Ctrl Pts',(0.965838846964708,51.4901464650663,-0.674473012972362));
#44635=CARTESIAN_POINT('Ctrl Pts',(0.945377246506615,51.4925669777587,-0.702450137281952));
#44636=CARTESIAN_POINT('Ctrl Pts',(0.940039738079159,51.4931841249534,-0.709577082925663));
#44637=CARTESIAN_POINT('Ctrl Pts',(0.931401305635918,51.4941596674658,-0.720843034940442));
#44638=CARTESIAN_POINT('Ctrl Pts',(0.928152530112668,51.494521472602,-0.725021349416883));
#44639=CARTESIAN_POINT('Ctrl Pts',(0.921125536867816,51.4952929883284,-0.733934258207485));
#44640=CARTESIAN_POINT('Ctrl Pts',(0.917338720852213,51.4957020655959,-0.738661915521769));
#44641=CARTESIAN_POINT('Ctrl Pts',(0.907331277077833,51.4967664282709,-0.750960063750599));
#44642=CARTESIAN_POINT('Ctrl Pts',(0.901052212367415,51.4974177092726,-0.75848268931107));
#44643=CARTESIAN_POINT('Ctrl Pts',(0.869101728046392,51.5006551247009,-0.795804097540143));
#44644=CARTESIAN_POINT('Ctrl Pts',(0.842040284767702,51.5031550654204,-0.824385099925427));
#44645=CARTESIAN_POINT('Ctrl Pts',(0.778713982090678,51.508638232213,-0.884888182816776));
#44646=CARTESIAN_POINT('Ctrl Pts',(0.741815777710828,51.511598435189,-0.916041581488608));
#44647=CARTESIAN_POINT('Ctrl Pts',(0.65149993152245,51.518565560712,-0.983250473717295));
#44648=CARTESIAN_POINT('Ctrl Pts',(0.596836259757017,51.5225846863174,-1.01735868992179));
#44649=CARTESIAN_POINT('Ctrl Pts',(0.525065267729918,51.5278368025096,-1.05435826021732));
#44650=CARTESIAN_POINT('Ctrl Pts',(0.510309934395917,51.5289148440322,-1.06157835488417));
#44651=CARTESIAN_POINT('Ctrl Pts',(0.485746073276829,51.5307094963588,-1.07296750179758));
#44652=CARTESIAN_POINT('Ctrl Pts',(0.476023085479921,51.5314198522669,-1.0773163495677));
#44653=CARTESIAN_POINT('Ctrl Pts',(0.456787141156655,51.5328259077799,-1.08560885861115));
#44654=CARTESIAN_POINT('Ctrl Pts',(0.447278786255941,51.5335212479292,-1.08956081145188));
#44655=CARTESIAN_POINT('Ctrl Pts',(0.424199350082499,51.5352104241697,-1.09880029256941));
#44656=CARTESIAN_POINT('Ctrl Pts',(0.410579927974366,51.5362083843319,-1.10396162113239));
#44657=CARTESIAN_POINT('Ctrl Pts',(0.358535261909155,51.5400280796431,-1.12258862523402));
#44658=CARTESIAN_POINT('Ctrl Pts',(0.319520388980909,51.5429053432363,-1.13430983810323));
#44659=CARTESIAN_POINT('Ctrl Pts',(0.202378051358836,51.5515784693802,-1.16297940102476));
#44660=CARTESIAN_POINT('Ctrl Pts',(0.123046724142034,51.5575105349847,-1.17402541992342));
#44661=CARTESIAN_POINT('Ctrl Pts',(0.00778553855762457,51.5659110916455,
-1.17825788493766));
#44662=CARTESIAN_POINT('Ctrl Pts',(-0.0276918000622706,51.5684638894598,
-1.17795836367394));
#44663=CARTESIAN_POINT('Ctrl Pts',(-0.0728625043434388,51.5716320644978,
-1.17553460520429));
#44664=CARTESIAN_POINT('Ctrl Pts',(-0.0826138847234062,51.5723110723936,
-1.1748895754239));
#44665=CARTESIAN_POINT('Ctrl Pts',(-0.0983893040399858,51.5734003671119,
-1.17364868135226));
#44666=CARTESIAN_POINT('Ctrl Pts',(-0.104418532923595,51.5738145100978,
-1.17312763864856));
#44667=CARTESIAN_POINT('Ctrl Pts',(-0.116433102210884,51.5746350842565,
-1.17199598422113));
#44668=CARTESIAN_POINT('Ctrl Pts',(-0.122418303422446,51.5750415292047,
-1.17138593859082));
#44669=CARTESIAN_POINT('Ctrl Pts',(-0.137947007450418,51.5760906075994,
-1.16968284246732));
#44670=CARTESIAN_POINT('Ctrl Pts',(-0.147482506597035,51.5767294468237,
-1.16851882908204));
#44671=CARTESIAN_POINT('Ctrl Pts',(-0.193034680027101,51.5797602145142,
-1.16239168969202));
#44672=CARTESIAN_POINT('Ctrl Pts',(-0.22882635345683,51.5820787354112,-1.15587882887217));
#44673=CARTESIAN_POINT('Ctrl Pts',(-0.368084827267104,51.5910508119624,
-1.12381453878418));
#44674=CARTESIAN_POINT('Ctrl Pts',(-0.468179281988897,51.5974399658047,
-1.0859348471274));
#44675=CARTESIAN_POINT('Ctrl Pts',(-0.578917713397505,51.6055517601538,
-1.02583033448127));
#44676=CARTESIAN_POINT('Ctrl Pts',(-0.595783840754068,51.6068169062925,
-1.01612752182739));
#44677=CARTESIAN_POINT('Ctrl Pts',(-0.622939262400979,51.6089082562277,
-0.999596889057083));
#44678=CARTESIAN_POINT('Ctrl Pts',(-0.633375541021732,51.6097255652479,
-0.993016953551476));
#44679=CARTESIAN_POINT('Ctrl Pts',(-0.652088417036367,51.6112170046168,
-0.980803726309379));
#44680=CARTESIAN_POINT('Ctrl Pts',(-0.660400308096165,51.6118889997723,
-0.975226473986516));
#44681=CARTESIAN_POINT('Ctrl Pts',(-0.678277662071779,51.6133557549078,
-0.962897471208792));
#44682=CARTESIAN_POINT('Ctrl Pts',(-0.68781547785157,51.6141519155345,-0.956107723012773));
#44683=CARTESIAN_POINT('Ctrl Pts',(-0.71473260948134,51.6164389597027,-0.936334832596564));
#44684=CARTESIAN_POINT('Ctrl Pts',(-0.731855797574318,51.6179427980301,
-0.923012786952734));
#44685=CARTESIAN_POINT('Ctrl Pts',(-0.792300115840083,51.6234347148537,
-0.873246689953653));
#44686=CARTESIAN_POINT('Ctrl Pts',(-0.833343471649848,51.627522479204,-0.834168095435839));
#44687=CARTESIAN_POINT('Ctrl Pts',(-0.919007786596022,51.636842769047,-0.73994933985058));
#44688=CARTESIAN_POINT('Ctrl Pts',(-0.961788964807032,51.6420905156268,
-0.683420062062222));
#44689=CARTESIAN_POINT('Ctrl Pts',(-1.00917447221783,51.6484918496028,-0.607465471933665));
#44690=CARTESIAN_POINT('Ctrl Pts',(-1.01872864366801,51.649819238263,-0.591303187670937));
#44691=CARTESIAN_POINT('Ctrl Pts',(-1.03140932686091,51.6516269598634,-0.56863147377479));
#44692=CARTESIAN_POINT('Ctrl Pts',(-1.03486805929307,51.6521251204273,-0.562312243270667));
#44693=CARTESIAN_POINT('Ctrl Pts',(-1.04098717468099,51.6530152438195,-0.550884678177245));
#44694=CARTESIAN_POINT('Ctrl Pts',(-1.04366847687343,51.6534084488008,-0.545787818424753));
#44695=CARTESIAN_POINT('Ctrl Pts',(-1.04921575990447,51.654228407645,-0.5350526604289));
#44696=CARTESIAN_POINT('Ctrl Pts',(-1.05207388197608,51.6546546920453,-0.52941062684451));
#44697=CARTESIAN_POINT('Ctrl Pts',(-1.05980128202895,51.6558186354366,-0.513846718024227));
#44698=CARTESIAN_POINT('Ctrl Pts',(-1.06457670599092,51.6565508269861,-0.503878622269322));
#44699=CARTESIAN_POINT('Ctrl Pts',(-1.094184166711,51.6611845478249,-0.439776172494579));
#44700=CARTESIAN_POINT('Ctrl Pts',(-1.11502314715813,51.6648894378283,-0.383884423776815));
#44701=CARTESIAN_POINT('Ctrl Pts',(-1.1557425500198,51.6739706031755,-0.242828535582492));
#44702=CARTESIAN_POINT('Ctrl Pts',(-1.17054904363917,51.6793129584535,-0.156587701061906));
#44703=CARTESIAN_POINT('Ctrl Pts',(-1.17652583295087,51.6858798452696,-0.0554901756800495));
#44704=CARTESIAN_POINT('Ctrl Pts',(-1.17710371235242,51.6867971695693,-0.0414610539006681));
#44705=CARTESIAN_POINT('Ctrl Pts',(-1.17764313659771,51.6883232936628,-0.0183024361316305));
#44706=CARTESIAN_POINT('Ctrl Pts',(-1.1777495911096,51.6889276389105,-0.0091775618924337));
#44707=CARTESIAN_POINT('Ctrl Pts',(-1.17774999882436,51.6895352714817,-5.26234844835546E-5));
#44708=CARTESIAN_POINT('Ctrl Pts',(0.188969603130438,51.8285263152314,1.16268601701703));
#44709=CARTESIAN_POINT('Ctrl Pts',(0.105006823041406,51.8227652863916,1.17720726394182));
#44710=CARTESIAN_POINT('Ctrl Pts',(-0.372052432586408,51.7905460268137,
1.20724379575199));
#44711=CARTESIAN_POINT('Ctrl Pts',(-1.02786962445986,51.7445815501578,0.80164220951439));
#44712=CARTESIAN_POINT('Ctrl Pts',(-1.1756492492359,51.7043781023418,0.204084402645715));
#44713=CARTESIAN_POINT('Ctrl Pts',(-1.17584353021606,51.6906328852638,-0.000125521981853664));
#44714=CARTESIAN_POINT('Ctrl Pts',(0.188938462126305,51.9282531127635,1.16249615914606));
#44715=CARTESIAN_POINT('Ctrl Pts',(0.183462612124699,51.9278870166283,1.16338613944406));
#44716=CARTESIAN_POINT('Ctrl Pts',(0.17798050184252,51.9275197376481,1.16423742484463));
#44717=CARTESIAN_POINT('Ctrl Pts',(0.162250033160122,51.9264635056015,1.16656641379994));
#44718=CARTESIAN_POINT('Ctrl Pts',(0.151988266015469,51.9257716097238,1.16794769847221));
#44719=CARTESIAN_POINT('Ctrl Pts',(0.131223367283335,51.9243651229521,1.17046446894594));
#44720=CARTESIAN_POINT('Ctrl Pts',(0.120720525653028,51.9236504215511,1.17159429290802));
#44721=CARTESIAN_POINT('Ctrl Pts',(0.0942810529495212,51.9218423112242,
1.1740791846088));
#44722=CARTESIAN_POINT('Ctrl Pts',(0.0783298015161907,51.9207432881422,
1.17525114200211));
#44723=CARTESIAN_POINT('Ctrl Pts',(0.00946654721373525,51.9159611631068,
1.17890248171694));
#44724=CARTESIAN_POINT('Ctrl Pts',(-0.0435488067908089,51.9121803216698,
1.17813530308287));
#44725=CARTESIAN_POINT('Ctrl Pts',(-0.166315877857828,51.9032265274241,
1.16806062033052));
#44726=CARTESIAN_POINT('Ctrl Pts',(-0.235648561579883,51.8980148348431,
1.15606916970954));
#44727=CARTESIAN_POINT('Ctrl Pts',(-0.333346518993407,51.8906804285494,
1.13001301620693));
#44728=CARTESIAN_POINT('Ctrl Pts',(-0.362872370326534,51.8884670225882,
1.12088059606519));
#44729=CARTESIAN_POINT('Ctrl Pts',(-0.40065656146647,51.885666242194,1.10754390916431));
#44730=CARTESIAN_POINT('Ctrl Pts',(-0.409270125513075,51.8850299622536,
1.10438995313784));
#44731=CARTESIAN_POINT('Ctrl Pts',(-0.423385896769344,51.8839918834375,
1.09903346215587));
#44732=CARTESIAN_POINT('Ctrl Pts',(-0.428909762859666,51.8835868415959,
1.09688950641639));
#44733=CARTESIAN_POINT('Ctrl Pts',(-0.440139428377085,51.8827661709178,
1.09243317568849));
#44734=CARTESIAN_POINT('Ctrl Pts',(-0.445843696046905,51.8823507357693,
1.09011759127742));
#44735=CARTESIAN_POINT('Ctrl Pts',(-0.461011226969873,51.8812492676327,
1.08382152625517));
#44736=CARTESIAN_POINT('Ctrl Pts',(-0.470441283409505,51.8805677655078,
1.07976176487336));
#44737=CARTESIAN_POINT('Ctrl Pts',(-0.521620420814071,51.876880835444,1.05693067405765));
#44738=CARTESIAN_POINT('Ctrl Pts',(-0.562305680730351,51.8739921567228,
1.03585886770141));
#44739=CARTESIAN_POINT('Ctrl Pts',(-0.662850879550758,51.8667085882616,
0.976109397727067));
#44740=CARTESIAN_POINT('Ctrl Pts',(-0.720613813347096,51.8623748738761,
0.934278645186085));
#44741=CARTESIAN_POINT('Ctrl Pts',(-0.794027332826886,51.8562439551879,
0.870232556631485));
#44742=CARTESIAN_POINT('Ctrl Pts',(-0.813224159390333,51.8545753195536,
0.852320620385603));
#44743=CARTESIAN_POINT('Ctrl Pts',(-0.846381450553554,51.8515546387805,
0.819241967689644));
#44744=CARTESIAN_POINT('Ctrl Pts',(-0.860572636633313,51.8502124877072,
0.804321836139874));
#44745=CARTESIAN_POINT('Ctrl Pts',(-0.882062040004818,51.8480954694883,
0.780508565272471));
#44746=CARTESIAN_POINT('Ctrl Pts',(-0.889633772913021,51.8473321575135,
0.771867085235054));
#44747=CARTESIAN_POINT('Ctrl Pts',(-0.903573510775216,51.8458928802471,
0.755480297802631));
#44748=CARTESIAN_POINT('Ctrl Pts',(-0.909971419759694,51.8452182337526,
0.747761709495764));
#44749=CARTESIAN_POINT('Ctrl Pts',(-0.924200677327786,51.8436849647098,
0.730142116491861));
#44750=CARTESIAN_POINT('Ctrl Pts',(-0.931972831109019,51.8428240742604,
0.720195128117739));
#44751=CARTESIAN_POINT('Ctrl Pts',(-0.955698205260662,51.8401205614458,
0.68880353968434));
#44752=CARTESIAN_POINT('Ctrl Pts',(-0.971081380142646,51.8382564653814,
0.666940873993194));
#44753=CARTESIAN_POINT('Ctrl Pts',(-1.03571043092111,51.8299063779116,0.568107926069416));
#44754=CARTESIAN_POINT('Ctrl Pts',(-1.07664094282409,51.8231425871902,0.486088939257362));
#44755=CARTESIAN_POINT('Ctrl Pts',(-1.1175044777919,51.8143471076261,0.37298161413268));
#44756=CARTESIAN_POINT('Ctrl Pts',(-1.12632705418038,51.8122462181066,0.345425980429661));
#44757=CARTESIAN_POINT('Ctrl Pts',(-1.13914544761635,51.8088503706586,0.29964838659876));
#44758=CARTESIAN_POINT('Ctrl Pts',(-1.14373906035697,51.8075356226127,0.281607104561715));
#44759=CARTESIAN_POINT('Ctrl Pts',(-1.14962833587913,51.8057057362517,0.255947675947434));
#44760=CARTESIAN_POINT('Ctrl Pts',(-1.15127951918364,51.8051733804073,0.248414976116174));
#44761=CARTESIAN_POINT('Ctrl Pts',(-1.15400967826238,51.8042588570661,0.235347637755888));
#44762=CARTESIAN_POINT('Ctrl Pts',(-1.15512307649148,51.8038748424923,0.229820650276862));
#44763=CARTESIAN_POINT('Ctrl Pts',(-1.15748442910733,51.8030353196771,0.217647825057052));
#44764=CARTESIAN_POINT('Ctrl Pts',(-1.15871490075926,51.8025807729735,0.210998966248973));
#44765=CARTESIAN_POINT('Ctrl Pts',(-1.16210906460721,51.8012742409649,0.191732760728299));
#44766=CARTESIAN_POINT('Ctrl Pts',(-1.1641244742733,51.8004299677878,0.179089839836327));
#44767=CARTESIAN_POINT('Ctrl Pts',(-1.17375072987791,51.795983665926,0.111646945734306));
#44768=CARTESIAN_POINT('Ctrl Pts',(-1.17770009804705,51.7925397376763,0.0563886714383546));
#44769=CARTESIAN_POINT('Ctrl Pts',(-1.17782728655719,51.7837305019052,-0.085992224174415));
#44770=CARTESIAN_POINT('Ctrl Pts',(-1.16825572491506,51.7784043491381,-0.1727676935835));
#44771=CARTESIAN_POINT('Ctrl Pts',(-1.14517246557387,51.7715723035668,-0.275709991094904));
#44772=CARTESIAN_POINT('Ctrl Pts',(-1.14070963547905,51.7703647650872,-0.293628067370979));
#44773=CARTESIAN_POINT('Ctrl Pts',(-1.13290261332065,51.7684123258271,-0.322101060345485));
#44774=CARTESIAN_POINT('Ctrl Pts',(-1.12982749286203,51.7676761163491,-0.332726985111607));
#44775=CARTESIAN_POINT('Ctrl Pts',(-1.12365651968738,51.7662577041675,-0.352977733859893));
#44776=CARTESIAN_POINT('Ctrl Pts',(-1.12058549830709,51.7655763690396,-0.362609134945579));
#44777=CARTESIAN_POINT('Ctrl Pts',(-1.11316011443999,51.7639831317681,-0.384901092743328));
#44778=CARTESIAN_POINT('Ctrl Pts',(-1.10871316944721,51.7630682451989,-0.3975290851225));
#44779=CARTESIAN_POINT('Ctrl Pts',(-1.09306830405138,51.7599736353379,-0.439649712538828));
#44780=CARTESIAN_POINT('Ctrl Pts',(-1.08090184709768,51.7577624482988,-0.468765465494556));
#44781=CARTESIAN_POINT('Ctrl Pts',(-1.04690129990442,51.7520316309258,-0.541748231518111));
#44782=CARTESIAN_POINT('Ctrl Pts',(-1.02347318337572,51.7484680593363,-0.584803647398971));
#44783=CARTESIAN_POINT('Ctrl Pts',(-0.957882792449539,51.7394194147271,
-0.689266508583233));
#44784=CARTESIAN_POINT('Ctrl Pts',(-0.912448615953605,51.733910250578,-0.748376147206907));
#44785=CARTESIAN_POINT('Ctrl Pts',(-0.853654142501249,51.7278311656367,
-0.811486507626759));
#44786=CARTESIAN_POINT('Ctrl Pts',(-0.845438074450274,51.7270025886761,
-0.820042825921475));
#44787=CARTESIAN_POINT('Ctrl Pts',(-0.832478070147195,51.7257295984871,
-0.833137671720877));
#44788=CARTESIAN_POINT('Ctrl Pts',(-0.827823345229624,51.7252789876061,
-0.837762873152522));
#44789=CARTESIAN_POINT('Ctrl Pts',(-0.819028307480639,51.724440249119,-0.846357243693378));
#44790=CARTESIAN_POINT('Ctrl Pts',(-0.814897490186356,51.7240514926395,
-0.850335248209219));
#44791=CARTESIAN_POINT('Ctrl Pts',(-0.804866175146836,51.7231194887353,
-0.859855233922112));
#44792=CARTESIAN_POINT('Ctrl Pts',(-0.798937329851195,51.7225784962274,
-0.865366821297075));
#44793=CARTESIAN_POINT('Ctrl Pts',(-0.777248142279038,51.7206326835768,
-0.885116645071476));
#44794=CARTESIAN_POINT('Ctrl Pts',(-0.761159269944817,51.7192518850147,
-0.898989903656797));
#44795=CARTESIAN_POINT('Ctrl Pts',(-0.717299275868071,51.7156230491057,
-0.934787686266086));
#44796=CARTESIAN_POINT('Ctrl Pts',(-0.688900132699164,51.713410793343,-0.955909622099035));
#44797=CARTESIAN_POINT('Ctrl Pts',(-0.582598474065916,51.7054480087722,
-1.02776989880228));
#44798=CARTESIAN_POINT('Ctrl Pts',(-0.499722913953653,51.6997973497193,
-1.07051749683297));
#44799=CARTESIAN_POINT('Ctrl Pts',(-0.394552599406553,51.6925416584963,
-1.10986403371338));
#44800=CARTESIAN_POINT('Ctrl Pts',(-0.376255074585946,51.6912777969649,
-1.11619979246553));
#44801=CARTESIAN_POINT('Ctrl Pts',(-0.346998564878577,51.6892498088831,
-1.12552913933316));
#44802=CARTESIAN_POINT('Ctrl Pts',(-0.336137682807531,51.6884954377621,
-1.12882030923926));
#44803=CARTESIAN_POINT('Ctrl Pts',(-0.315576913408956,51.6870636050458,
-1.13472779765957));
#44804=CARTESIAN_POINT('Ctrl Pts',(-0.305887754359871,51.686387318489,-1.13737796441804));
#44805=CARTESIAN_POINT('Ctrl Pts',(-0.283736406909279,51.6848371172491,
-1.143133256206));
#44806=CARTESIAN_POINT('Ctrl Pts',(-0.271255138818756,51.683960730004,-1.14615907133421));
#44807=CARTESIAN_POINT('Ctrl Pts',(-0.231371702469412,51.6811498389345,
-1.15514002261123));
#44808=CARTESIAN_POINT('Ctrl Pts',(-0.203807017784058,51.6791913168755,
-1.16032056202564));
#44809=CARTESIAN_POINT('Ctrl Pts',(-0.135830482380693,51.6743208240502,
-1.17059927931991));
#44810=CARTESIAN_POINT('Ctrl Pts',(-0.095290299645714,51.6713806242783,
-1.17459432007002));
#44811=CARTESIAN_POINT('Ctrl Pts',(0.0325751078803395,51.6620355047494,
-1.1805315265436));
#44812=CARTESIAN_POINT('Ctrl Pts',(0.11995951507089,51.6555252719099,-1.17487304545372));
#44813=CARTESIAN_POINT('Ctrl Pts',(0.217803460915769,51.6485176827157,-1.15749834899699));
#44814=CARTESIAN_POINT('Ctrl Pts',(0.229656129652328,51.6476740536699,-1.15520511857476));
#44815=CARTESIAN_POINT('Ctrl Pts',(0.247938486595406,51.6463830553016,-1.15137536002117));
#44816=CARTESIAN_POINT('Ctrl Pts',(0.254393654611757,51.6459292229118,-1.14996634151417));
#44817=CARTESIAN_POINT('Ctrl Pts',(0.266417862057183,51.645088018983,-1.14723552068467));
#44818=CARTESIAN_POINT('Ctrl Pts',(0.271989372330439,51.644699968661,-1.14592739735966));
#44819=CARTESIAN_POINT('Ctrl Pts',(0.285334353671719,51.6437743353231,-1.14269134246325));
#44820=CARTESIAN_POINT('Ctrl Pts',(0.29309805058174,51.6432389225362,-1.14072465531099));
#44821=CARTESIAN_POINT('Ctrl Pts',(0.320778976967498,51.6413390276787,-1.13341129629457));
#44822=CARTESIAN_POINT('Ctrl Pts',(0.340576255218611,51.639997104275,-1.12762061618568));
#44823=CARTESIAN_POINT('Ctrl Pts',(0.392374374305499,51.6365059516286,-1.11098088946537));
#44824=CARTESIAN_POINT('Ctrl Pts',(0.424078938116739,51.6343892450726,-1.09926954799639));
#44825=CARTESIAN_POINT('Ctrl Pts',(0.534981711703971,51.6269177301872,-1.05278946823765));
#44826=CARTESIAN_POINT('Ctrl Pts',(0.610797641052369,51.6216631618294,-1.01069117959426));
#44827=CARTESIAN_POINT('Ctrl Pts',(0.701666518293402,51.614530729542,-0.946245868475442));
#44828=CARTESIAN_POINT('Ctrl Pts',(0.721546312291629,51.6129142313404,-0.93117556083893));
#44829=CARTESIAN_POINT('Ctrl Pts',(0.750501620864091,51.6104635545818,-0.907741126122959));
#44830=CARTESIAN_POINT('Ctrl Pts',(0.759949204460988,51.6096478816022,-0.899846554963675));
#44831=CARTESIAN_POINT('Ctrl Pts',(0.776847411884057,51.6081583233203,-0.885270170394331));
#44832=CARTESIAN_POINT('Ctrl Pts',(0.784340018322728,51.6074865511765,-0.878638663462971));
#44833=CARTESIAN_POINT('Ctrl Pts',(0.80042504274422,51.6060190012996,-0.864032532926315));
#44834=CARTESIAN_POINT('Ctrl Pts',(0.808984642098776,51.6052218063553,-0.856023538485632));
#44835=CARTESIAN_POINT('Ctrl Pts',(0.833101276107259,51.6029277711956,-0.832773435800495));
#44836=CARTESIAN_POINT('Ctrl Pts',(0.848356316405623,51.601417846077,-0.817227497283205));
#44837=CARTESIAN_POINT('Ctrl Pts',(0.903912679649658,51.5956890811113,-0.757379104189814));
#44838=CARTESIAN_POINT('Ctrl Pts',(0.941242425216576,51.5913564108608,-0.710452101871946));
#44839=CARTESIAN_POINT('Ctrl Pts',(1.01794877935151,51.5813396166399,-0.597308395673047));
#44840=CARTESIAN_POINT('Ctrl Pts',(1.05473596631605,51.5756392022864,-0.52965128678864));
#44841=CARTESIAN_POINT('Ctrl Pts',(1.08961458620735,51.5693172267289,-0.447209100276167));
#44842=CARTESIAN_POINT('Ctrl Pts',(1.09436761780922,51.568429716205,-0.435448591040879));
#44843=CARTESIAN_POINT('Ctrl Pts',(1.10135303589467,51.5670863866018,-0.417327133572524));
#44844=CARTESIAN_POINT('Ctrl Pts',(1.10372220198934,51.5666233053141,-0.411020379716992));
#44845=CARTESIAN_POINT('Ctrl Pts',(1.10779773877904,51.5658136540792,-0.399881837057961));
#44846=CARTESIAN_POINT('Ctrl Pts',(1.10952681527662,51.5654658073397,-0.395058934143007));
#44847=CARTESIAN_POINT('Ctrl Pts',(1.11368239724219,51.5646188140736,-0.383225276549293));
#44848=CARTESIAN_POINT('Ctrl Pts',(1.1160742213194,51.5641216738024,-0.376202650540096));
#44849=CARTESIAN_POINT('Ctrl Pts',(1.12366524190434,51.5625100933248,-0.353204903809116));
#44850=CARTESIAN_POINT('Ctrl Pts',(1.12858927690882,51.5614101221376,-0.337140317030607));
#44851=CARTESIAN_POINT('Ctrl Pts',(1.13995684128539,51.5587130084674,-0.297008325596261));
#44852=CARTESIAN_POINT('Ctrl Pts',(1.14598385459334,51.5571327784842,-0.272830902088554));
#44853=CARTESIAN_POINT('Ctrl Pts',(1.17139188461725,51.5495744396951,-0.155111820177261));
#44854=CARTESIAN_POINT('Ctrl Pts',(1.18011108972063,51.543823702531,-0.0596419259651858));
#44855=CARTESIAN_POINT('Ctrl Pts',(1.17634134878957,51.5359310763864,0.0641968616380028));
#44856=CARTESIAN_POINT('Ctrl Pts',(1.17445337618798,51.5340994748725,0.0925163385151291));
#44857=CARTESIAN_POINT('Ctrl Pts',(1.17022269009456,51.5313898052987,0.133567398215436));
#44858=CARTESIAN_POINT('Ctrl Pts',(1.16868995149018,51.5305367823428,0.146373391406597));
#44859=CARTESIAN_POINT('Ctrl Pts',(1.16558914833725,51.529007206507,0.169109464053154));
#44860=CARTESIAN_POINT('Ctrl Pts',(1.16410364264697,51.5283333170692,0.179049635434051));
#44861=CARTESIAN_POINT('Ctrl Pts',(1.16067551606526,51.5268920245428,0.200138597461469));
#44862=CARTESIAN_POINT('Ctrl Pts',(1.15869906833716,51.5261236103602,0.211280773301466));
#44863=CARTESIAN_POINT('Ctrl Pts',(1.15283865298841,51.5240019332518,0.241758145710643));
#44864=CARTESIAN_POINT('Ctrl Pts',(1.1486292690451,51.5226385236471,0.261026207841442));
#44865=CARTESIAN_POINT('Ctrl Pts',(1.13804664754031,51.5195294032643,0.304233895214888));
#44866=CARTESIAN_POINT('Ctrl Pts',(1.131397983325,51.5177758801429,0.32809585595942));
#44867=CARTESIAN_POINT('Ctrl Pts',(1.10523289699926,51.5115038488961,0.411710262156313));
#44868=CARTESIAN_POINT('Ctrl Pts',(1.08169359692449,51.5068836273392,0.470088012251854));
#44869=CARTESIAN_POINT('Ctrl Pts',(1.03021264018664,51.4984211413603,0.573148305380368));
#44870=CARTESIAN_POINT('Ctrl Pts',(1.00371227751021,51.4945888481177,0.618384760168006));
#44871=CARTESIAN_POINT('Ctrl Pts',(0.967079967850452,51.4899825960001,0.672321295255519));
#44872=CARTESIAN_POINT('Ctrl Pts',(0.959700108053729,51.4890847839051,0.682814267865826));
#44873=CARTESIAN_POINT('Ctrl Pts',(0.948167212845705,51.4877292062156,0.698655700986576));
#44874=CARTESIAN_POINT('Ctrl Pts',(0.944137299855534,51.4872639853379,0.704092051328692));
#44875=CARTESIAN_POINT('Ctrl Pts',(0.936664693908591,51.4864171068407,0.713993061478256));
#44876=CARTESIAN_POINT('Ctrl Pts',(0.933236619348428,51.4860345522981,0.718467991562704));
#44877=CARTESIAN_POINT('Ctrl Pts',(0.92504817000169,51.4851344890235,0.728999506546271));
#44878=CARTESIAN_POINT('Ctrl Pts',(0.920260315408643,51.4846188908422,0.735034255868959));
#44879=CARTESIAN_POINT('Ctrl Pts',(0.903735624037448,51.4828736218386,0.755447858438214));
#44880=CARTESIAN_POINT('Ctrl Pts',(0.891717651800982,51.4816619385389,0.769596820065839));
#44881=CARTESIAN_POINT('Ctrl Pts',(0.860211078138958,51.478610606278,0.804960509550186));
#44882=CARTESIAN_POINT('Ctrl Pts',(0.840269095950351,51.4767941649389,0.825755761557385));
#44883=CARTESIAN_POINT('Ctrl Pts',(0.754604125610371,51.4693460483427,0.908765443530676));
#44884=CARTESIAN_POINT('Ctrl Pts',(0.682588246703392,51.4638745660641,0.964030756287453));
#44885=CARTESIAN_POINT('Ctrl Pts',(0.581408599316212,51.4563524772678,1.02460345972236));
#44886=CARTESIAN_POINT('Ctrl Pts',(0.55737820462134,51.4545791247731,1.03787165066499));
#44887=CARTESIAN_POINT('Ctrl Pts',(0.52154317498901,51.4519393480716,1.05605406232302));
#44888=CARTESIAN_POINT('Ctrl Pts',(0.510086156307196,51.4510961011832,1.06163532248707));
#44889=CARTESIAN_POINT('Ctrl Pts',(0.489449043406567,51.449577221007,1.07127746621177));
#44890=CARTESIAN_POINT('Ctrl Pts',(0.480303222166705,51.4489041071393,1.0754090290398));
#44891=CARTESIAN_POINT('Ctrl Pts',(0.460648970576079,51.4474570419454,1.083986976827));
#44892=CARTESIAN_POINT('Ctrl Pts',(0.450126551769554,51.446681983352,1.08839850760892));
#44893=CARTESIAN_POINT('Ctrl Pts',(0.420812261144959,51.4445210165315,1.10019074457432));
#44894=CARTESIAN_POINT('Ctrl Pts',(0.401892955986705,51.4431243212654,1.1072418876155));
#44895=CARTESIAN_POINT('Ctrl Pts',(0.358629277967955,51.439924123658,1.12211117413984));
#44896=CARTESIAN_POINT('Ctrl Pts',(0.334193327887872,51.4381120951896,1.12962963170276));
#44897=CARTESIAN_POINT('Ctrl Pts',(0.269803577984737,51.433328066067,1.14716898750013));
#44898=CARTESIAN_POINT('Ctrl Pts',(0.229549396662269,51.4303272326354,1.15589573824819));
#44899=CARTESIAN_POINT('Ctrl Pts',(0.18893837638019,51.427308721746,1.16249617308222));
#44900=CARTESIAN_POINT('Origin',(0.,56.5393671147362,0.));
#44901=CARTESIAN_POINT('',(0.188938575466302,50.827546579051,1.16249614072511));
#44902=CARTESIAN_POINT('',(0.18893846240316,50.927164359664,1.16249615910107));
#44903=CARTESIAN_POINT('',(0.188938462403162,56.5393671147362,1.16249615910107));
#44904=CARTESIAN_POINT('Ctrl Pts',(0.188938575466302,50.827546579051,1.16249614072511));
#44905=CARTESIAN_POINT('Ctrl Pts',(0.259627942104656,50.8326143480709,1.15100711485622));
#44906=CARTESIAN_POINT('Ctrl Pts',(0.32914111607513,50.837863869476,1.13309119767087));
#44907=CARTESIAN_POINT('Ctrl Pts',(0.452718762653112,50.8475082684021,1.08889462587203));
#44908=CARTESIAN_POINT('Ctrl Pts',(0.507228187990633,50.8518793517914,1.0645969831142));
#44909=CARTESIAN_POINT('Ctrl Pts',(0.569393707715353,50.856846433725,1.03102281040476));
#44910=CARTESIAN_POINT('Ctrl Pts',(0.579044964963574,50.8576168822874,1.02563355093232));
#44911=CARTESIAN_POINT('Ctrl Pts',(0.594097261400788,50.8588157330355,1.01694813287376));
#44912=CARTESIAN_POINT('Ctrl Pts',(0.599549787651772,50.8592494239745,1.01374312220045));
#44913=CARTESIAN_POINT('Ctrl Pts',(0.609916913798747,50.8600725205075,1.00753639064356));
#44914=CARTESIAN_POINT('Ctrl Pts',(0.614835696914428,50.8604623522168,1.00454232736016));
#44915=CARTESIAN_POINT('Ctrl Pts',(0.62585658071665,50.8613346410909,0.99772264156154));
#44916=CARTESIAN_POINT('Ctrl Pts',(0.631946051661149,50.8618158193953,0.993876814996615));
#44917=CARTESIAN_POINT('Ctrl Pts',(0.653766830888981,50.8635386381763,0.979814182397296));
#44918=CARTESIAN_POINT('Ctrl Pts',(0.66928966843692,50.8647615419271,0.969277222256888));
#44919=CARTESIAN_POINT('Ctrl Pts',(0.742130557723507,50.8705210693014,0.917247801076728));
#44920=CARTESIAN_POINT('Ctrl Pts',(0.795888293366376,50.8748422967611,0.871013788436937));
#44921=CARTESIAN_POINT('Ctrl Pts',(0.876079641583324,50.8819643785318,0.788383684409174));
#44922=CARTESIAN_POINT('Ctrl Pts',(0.90515919190761,50.8847238538695,0.754818401878749));
#44923=CARTESIAN_POINT('Ctrl Pts',(0.95039813429856,50.8894316965573,0.696217001721589));
#44924=CARTESIAN_POINT('Ctrl Pts',(0.967627507292236,50.8913434449042,0.672065107411906));
#44925=CARTESIAN_POINT('Ctrl Pts',(0.991127301414742,50.8941490834824,0.636343788099257));
#44926=CARTESIAN_POINT('Ctrl Pts',(0.998145128453671,50.8950152376651,0.625278357165891));
#44927=CARTESIAN_POINT('Ctrl Pts',(1.01022974858605,50.8965594807933,0.605501788651564));
#44928=CARTESIAN_POINT('Ctrl Pts',(1.01537216888101,50.8972347132135,0.596838260167771));
#44929=CARTESIAN_POINT('Ctrl Pts',(1.02599781341864,50.8986695741594,0.578402193477325));
#44930=CARTESIAN_POINT('Ctrl Pts',(1.03145394912399,50.8994300952994,0.568615288398058));
#44931=CARTESIAN_POINT('Ctrl Pts',(1.04586092233997,50.9015050008596,0.541883032636944));
#44932=CARTESIAN_POINT('Ctrl Pts',(1.05453881475556,50.902828790241,0.524795296084028));
#44933=CARTESIAN_POINT('Ctrl Pts',(1.1046338387831,50.9109452721693,0.419888267125618));
#44934=CARTESIAN_POINT('Ctrl Pts',(1.1354705666607,50.9180975454135,0.327447643440453));
#44935=CARTESIAN_POINT('Ctrl Pts',(1.16115521099394,50.9276458069994,0.199783591125745));
#44936=CARTESIAN_POINT('Ctrl Pts',(1.16632057583926,50.9300645488661,0.1670074158695));
#44937=CARTESIAN_POINT('Ctrl Pts',(1.17241532842624,50.9339002675268,0.113809600453559));
#44938=CARTESIAN_POINT('Ctrl Pts',(1.17420915078907,50.9353431706389,0.0935057026633607));
#44939=CARTESIAN_POINT('Ctrl Pts',(1.17597065304988,50.9373163060155,0.0652049068412056));
#44940=CARTESIAN_POINT('Ctrl Pts',(1.17638521719627,50.9378673907132,0.0572406013884337));
#44941=CARTESIAN_POINT('Ctrl Pts',(1.17695814868201,50.9388062778386,0.0435579114685473));
#44942=CARTESIAN_POINT('Ctrl Pts',(1.17715580704249,50.9391961428226,0.0378416039196781));
#44943=CARTESIAN_POINT('Ctrl Pts',(1.17749261392439,50.9400327092992,0.0254978676405069));
#44944=CARTESIAN_POINT('Ctrl Pts',(1.17761747192257,50.9404786405492,0.0188704066778337));
#44945=CARTESIAN_POINT('Ctrl Pts',(1.17781283300023,50.9417349319346,7.66448210947528E-5));
#44946=CARTESIAN_POINT('Ctrl Pts',(1.17775078941898,50.942538460152,-0.0120905723682189));
#44947=CARTESIAN_POINT('Ctrl Pts',(1.17606276703339,50.9478974164786,-0.0940377489813075));
#44948=CARTESIAN_POINT('Ctrl Pts',(1.16842464807765,50.9521912191395,-0.163563645674606));
#44949=CARTESIAN_POINT('Ctrl Pts',(1.14450302802036,50.9596909249419,-0.282616780253624));
#44950=CARTESIAN_POINT('Ctrl Pts',(1.13101918996311,50.9628796035003,-0.332497474951011));
#44951=CARTESIAN_POINT('Ctrl Pts',(1.10707150503448,50.9675658029512,-0.402476418010754));
#44952=CARTESIAN_POINT('Ctrl Pts',(1.09923495366496,50.9689956724105,-0.423411160555576));
#44953=CARTESIAN_POINT('Ctrl Pts',(1.08392122243635,50.9716267128675,-0.461024279203603));
#44954=CARTESIAN_POINT('Ctrl Pts',(1.07664234484914,50.9728215155987,-0.477775894025711));
#44955=CARTESIAN_POINT('Ctrl Pts',(1.06435032769334,50.9747585415348,-0.504355979945449));
#44956=CARTESIAN_POINT('Ctrl Pts',(1.05958330952193,50.9754923288003,-0.514295411989171));
#44957=CARTESIAN_POINT('Ctrl Pts',(1.05017128423351,50.9769094867815,-0.533233398757788));
#44958=CARTESIAN_POINT('Ctrl Pts',(1.04554834160172,50.9775920368745,-0.542241863030465));
#44959=CARTESIAN_POINT('Ctrl Pts',(1.03460739559543,50.9791775539514,-0.562901632950017));
#44960=CARTESIAN_POINT('Ctrl Pts',(1.02820782095753,50.9800833504959,-0.574507931313546));
#44961=CARTESIAN_POINT('Ctrl Pts',(1.00708304617504,50.9830075197304,-0.611335988201504));
#44962=CARTESIAN_POINT('Ctrl Pts',(0.99161610508143,50.9850519746332,-0.636117281242357));
#44963=CARTESIAN_POINT('Ctrl Pts',(0.926139175970483,50.9933468432241,-0.732825468286185));
#44964=CARTESIAN_POINT('Ctrl Pts',(0.869099090636311,50.9998344007438,-0.799643706673251));
#44965=CARTESIAN_POINT('Ctrl Pts',(0.784475563347867,51.0083114337444,-0.87891922143992));
#44966=CARTESIAN_POINT('Ctrl Pts',(0.763062496210773,51.0103723366655,-0.897572685369569));
#44967=CARTESIAN_POINT('Ctrl Pts',(0.726708103191955,51.013712103079,-0.926999595952955));
#44968=CARTESIAN_POINT('Ctrl Pts',(0.712151388596709,51.0150100208736,-0.938228867528149));
#44969=CARTESIAN_POINT('Ctrl Pts',(0.691150571368268,51.0168210719332,-0.953658680536643));
#44970=CARTESIAN_POINT('Ctrl Pts',(0.684919799690257,51.0173509653471,-0.958143448199318));
#44971=CARTESIAN_POINT('Ctrl Pts',(0.673997653827916,51.018266365179,-0.965843964875581));
#44972=CARTESIAN_POINT('Ctrl Pts',(0.669326176891426,51.0186536420821,-0.969087135296385));
#44973=CARTESIAN_POINT('Ctrl Pts',(0.659006794931623,51.0194997633285,-0.976141137366368));
#44974=CARTESIAN_POINT('Ctrl Pts',(0.653349087719074,51.0199576375446,-0.97993696284044));
#44975=CARTESIAN_POINT('Ctrl Pts',(0.636423676373294,51.0213106196566,-0.991080676156905));
#44976=CARTESIAN_POINT('Ctrl Pts',(0.625062275531782,51.0221969647458,-0.998285125558602));
#44977=CARTESIAN_POINT('Ctrl Pts',(0.548574125885574,51.0280376486168,-1.04496954137573));
#44978=CARTESIAN_POINT('Ctrl Pts',(0.479865521743824,51.032690768697,-1.07825178185986));
#44979=CARTESIAN_POINT('Ctrl Pts',(0.364989823088811,51.040261270085,-1.12072349738529));
#44980=CARTESIAN_POINT('Ctrl Pts',(0.320656273835647,51.0431350511907,-1.13420362893105));
#44981=CARTESIAN_POINT('Ctrl Pts',(0.24602512001743,51.0480114631145,-1.15216969030049));
#44982=CARTESIAN_POINT('Ctrl Pts',(0.21614008615792,51.0499736311142,-1.15814790741264));
#44983=CARTESIAN_POINT('Ctrl Pts',(0.172996545306663,51.0528394671767,-1.16505031886907));
#44984=CARTESIAN_POINT('Ctrl Pts',(0.159900546748441,51.0537136395047,-1.16691980951486));
#44985=CARTESIAN_POINT('Ctrl Pts',(0.136764199236654,51.0552669344928,-1.16982581574905));
#44986=CARTESIAN_POINT('Ctrl Pts',(0.126736663711469,51.055943082723,-1.17095460738734));
#44987=CARTESIAN_POINT('Ctrl Pts',(0.10560838297638,51.0573745012184,-1.17305843369908));
#44988=CARTESIAN_POINT('Ctrl Pts',(0.0945058797306597,51.0581305959129,
-1.17400504393459));
#44989=CARTESIAN_POINT('Ctrl Pts',(0.0645870968504152,51.0601793831649,
-1.17612880819369));
#44990=CARTESIAN_POINT('Ctrl Pts',(0.0457539253395615,51.06148107527,-1.17701188315866));
#44991=CARTESIAN_POINT('Ctrl Pts',(-0.0563745238890062,51.0686088410396,
-1.17934586725071));
#44992=CARTESIAN_POINT('Ctrl Pts',(-0.139611160143111,51.0746908021634,
-1.17240733556285));
#44993=CARTESIAN_POINT('Ctrl Pts',(-0.282147149173311,51.0853557581067,
-1.1451257299012));
#44994=CARTESIAN_POINT('Ctrl Pts',(-0.341886065992276,51.0898981781938,
-1.12873174380644));
#44995=CARTESIAN_POINT('Ctrl Pts',(-0.410334145193804,51.0950125571576,
-1.10401093693003));
#44996=CARTESIAN_POINT('Ctrl Pts',(-0.420551110570461,51.0957733414174,
-1.10015955411338));
#44997=CARTESIAN_POINT('Ctrl Pts',(-0.436573322274917,51.0969606512547,
-1.09386399330535));
#44998=CARTESIAN_POINT('Ctrl Pts',(-0.442414770692499,51.0973923061009,
-1.09151448772327));
#44999=CARTESIAN_POINT('Ctrl Pts',(-0.453575493683122,51.0982143007377,
-1.08692118274831));
#45000=CARTESIAN_POINT('Ctrl Pts',(-0.458897525140794,51.0986050325418,
-1.08468495376965));
#45001=CARTESIAN_POINT('Ctrl Pts',(-0.472172864730658,51.0995770408817,
-1.07899168191695));
#45002=CARTESIAN_POINT('Ctrl Pts',(-0.480105039530118,51.1001554559465,
-1.07548566983944));
#45003=CARTESIAN_POINT('Ctrl Pts',(-0.509733511398159,51.1023096872442,
-1.06199677958033));
#45004=CARTESIAN_POINT('Ctrl Pts',(-0.531164678955256,51.1038551905542,
-1.05144171215719));
#45005=CARTESIAN_POINT('Ctrl Pts',(-0.611049015760629,51.1096225734624,
-1.00903131307519));
#45006=CARTESIAN_POINT('Ctrl Pts',(-0.667089120057695,51.1136876364292,
-0.972891821773245));
#45007=CARTESIAN_POINT('Ctrl Pts',(-0.770541370313129,51.121777531743,-0.893014058272752));
#45008=CARTESIAN_POINT('Ctrl Pts',(-0.818011571922139,51.1257859992835,
-0.84974334255876));
#45009=CARTESIAN_POINT('Ctrl Pts',(-0.872811216364997,51.1310168703948,
-0.790923722052533));
#45010=CARTESIAN_POINT('Ctrl Pts',(-0.883653081669486,51.1320849386948,
-0.77879197632036));
#45011=CARTESIAN_POINT('Ctrl Pts',(-0.901150760090802,51.1338674846273,
-0.758376654340316));
#45012=CARTESIAN_POINT('Ctrl Pts',(-0.907952178926406,51.134575882362,-0.7502204146024));
#45013=CARTESIAN_POINT('Ctrl Pts',(-0.921067773759815,51.1359735321554,
-0.734052619190414));
#45014=CARTESIAN_POINT('Ctrl Pts',(-0.927390011419804,51.1366623729528,
-0.726048790998807));
#45015=CARTESIAN_POINT('Ctrl Pts',(-0.941100457753503,51.1381906167781,
-0.708220359674336));
#45016=CARTESIAN_POINT('Ctrl Pts',(-0.948440327817344,51.1390318176979,
-0.698360275165104));
#45017=CARTESIAN_POINT('Ctrl Pts',(-0.973557659205522,51.1419937492174,
-0.663492218655802));
#45018=CARTESIAN_POINT('Ctrl Pts',(-0.990509802363704,51.1441449215001,
-0.637907889233139));
#45019=CARTESIAN_POINT('Ctrl Pts',(-1.05377161414093,51.1528131596257,-0.533820715178569));
#45020=CARTESIAN_POINT('Ctrl Pts',(-1.09189912605093,51.1595830022785,-0.450723545126745));
#45021=CARTESIAN_POINT('Ctrl Pts',(-1.12777674903422,51.1680416497381,-0.340348828181685));
#45022=CARTESIAN_POINT('Ctrl Pts',(-1.13473488269983,51.1698462128101,-0.316377326596745));
#45023=CARTESIAN_POINT('Ctrl Pts',(-1.1450997369968,51.1728211756122,-0.27590684676094));
#45024=CARTESIAN_POINT('Ctrl Pts',(-1.14892366495532,51.1740061863463,-0.259523560887414));
#45025=CARTESIAN_POINT('Ctrl Pts',(-1.15392749480546,51.1756892291304,-0.235799706364306));
#45026=CARTESIAN_POINT('Ctrl Pts',(-1.15539081485754,51.1762011132553,-0.228521852527856));
#45027=CARTESIAN_POINT('Ctrl Pts',(-1.15774799219058,51.1770599898401,-0.216196476381845));
#45028=CARTESIAN_POINT('Ctrl Pts',(-1.15867785046393,51.1774089288977,-0.211156274547567));
#45029=CARTESIAN_POINT('Ctrl Pts',(-1.16075383077045,51.1782121752737,-0.199476801350127));
#45030=CARTESIAN_POINT('Ctrl Pts',(-1.16187593012931,51.1786651446625,-0.192833551224834));
#45031=CARTESIAN_POINT('Ctrl Pts',(-1.16494535584697,51.179962116542,-0.1736610032469));
#45032=CARTESIAN_POINT('Ctrl Pts',(-1.1667475089576,51.1807985800248,-0.161108995408212));
#45033=CARTESIAN_POINT('Ctrl Pts',(-1.17456551124465,51.184845870989,-0.0996119622266914));
#45034=CARTESIAN_POINT('Ctrl Pts',(-1.17770665723725,51.1879323382119,-0.0503463966565076));
#45035=CARTESIAN_POINT('Ctrl Pts',(-1.17783255203574,51.1969082215981,0.0944037241186597));
#45036=CARTESIAN_POINT('Ctrl Pts',(-1.1663181155478,51.2027161345442,0.189478315892197));
#45037=CARTESIAN_POINT('Ctrl Pts',(-1.13930656857895,51.2100358070486,0.298958885154033));
#45038=CARTESIAN_POINT('Ctrl Pts',(-1.13478072718027,51.2111722248204,0.315703219194191));
#45039=CARTESIAN_POINT('Ctrl Pts',(-1.12682925057453,51.2130379320123,0.342736520701312));
#45040=CARTESIAN_POINT('Ctrl Pts',(-1.12362826754823,51.2137599065956,0.353089203523291));
#45041=CARTESIAN_POINT('Ctrl Pts',(-1.11713896443712,51.2151703743131,0.373094568546962));
#45042=CARTESIAN_POINT('Ctrl Pts',(-1.11386722459418,51.2158582672985,0.382751639497525));
#45043=CARTESIAN_POINT('Ctrl Pts',(-1.10581870568822,51.217498169777,0.405530555001746));
#45044=CARTESIAN_POINT('Ctrl Pts',(-1.10093321982709,51.2184537126734,0.418612060193123));
#45045=CARTESIAN_POINT('Ctrl Pts',(-1.08273700904316,51.2218791786702,0.464811232996171));
#45046=CARTESIAN_POINT('Ctrl Pts',(-1.06815608491228,51.2243906140529,0.497404294368731));
#45047=CARTESIAN_POINT('Ctrl Pts',(-1.02485615446862,51.2312829180026,0.583476859005111));
#45048=CARTESIAN_POINT('Ctrl Pts',(-0.993448591200546,51.2357361501649,
0.63547937547028));
#45049=CARTESIAN_POINT('Ctrl Pts',(-0.925922546140864,51.2442693530678,
0.729958843424596));
#45050=CARTESIAN_POINT('Ctrl Pts',(-0.890514443913304,51.2483367991947,
0.772759722888525));
#45051=CARTESIAN_POINT('Ctrl Pts',(-0.843382058520212,51.2531607508105,
0.822171301195518));
#45052=CARTESIAN_POINT('Ctrl Pts',(-0.834395174539325,51.2540567611435,
0.831290365152012));
#45053=CARTESIAN_POINT('Ctrl Pts',(-0.820436125759192,51.2554102760242,
0.845000213032642));
#45054=CARTESIAN_POINT('Ctrl Pts',(-0.815570432673642,51.2558752009452,
0.849697399961489));
#45055=CARTESIAN_POINT('Ctrl Pts',(-0.806573191788908,51.2567219567454,
0.858234558088236));
#45056=CARTESIAN_POINT('Ctrl Pts',(-0.80245430146567,51.2571046785391,0.862086983076733));
#45057=CARTESIAN_POINT('Ctrl Pts',(-0.792635459192559,51.2580056985756,
0.871139260230269));
#45058=CARTESIAN_POINT('Ctrl Pts',(-0.786911856515027,51.2585220756768,
0.87631291217442));
#45059=CARTESIAN_POINT('Ctrl Pts',(-0.767195435336329,51.2602726387528,
0.893785923625735));
#45060=CARTESIAN_POINT('Ctrl Pts',(-0.752961102993835,51.2614886933439,
0.905810014620946));
#45061=CARTESIAN_POINT('Ctrl Pts',(-0.715888275090469,51.2645541573368,
0.935648203641285));
#45062=CARTESIAN_POINT('Ctrl Pts',(-0.692666570512478,51.2663800891113,
0.952967375375869));
#45063=CARTESIAN_POINT('Ctrl Pts',(-0.593421352118865,51.2739072608547,
1.02143972436333));
#45064=CARTESIAN_POINT('Ctrl Pts',(-0.512204988751643,51.2794460883624,
1.06448767250117));
#45065=CARTESIAN_POINT('Ctrl Pts',(-0.402106936592523,51.2869912385975,
1.10729767693632));
#45066=CARTESIAN_POINT('Ctrl Pts',(-0.377078088286573,51.288706478194,1.11606903135868));
#45067=CARTESIAN_POINT('Ctrl Pts',(-0.339761589612949,51.2912764836053,
1.12774802547282));
#45068=CARTESIAN_POINT('Ctrl Pts',(-0.327688093268305,51.2921098654283,
1.13131518149038));
#45069=CARTESIAN_POINT('Ctrl Pts',(-0.305901419416378,51.2936182739578,
1.1373741203664));
#45070=CARTESIAN_POINT('Ctrl Pts',(-0.296209088502571,51.2942909284969,
1.13993672335503));
#45071=CARTESIAN_POINT('Ctrl Pts',(-0.275313088074717,51.295745134872,1.14517703369123));
#45072=CARTESIAN_POINT('Ctrl Pts',(-0.264100560390666,51.2965279010022,
1.14781471172112));
#45073=CARTESIAN_POINT('Ctrl Pts',(-0.232608376654076,51.2987341222224,
1.15473719504402));
#45074=CARTESIAN_POINT('Ctrl Pts',(-0.212252528496873,51.3001691190988,
1.15865155062833));
#45075=CARTESIAN_POINT('Ctrl Pts',(-0.165672349411034,51.3034749217905,
1.16634011382907));
#45076=CARTESIAN_POINT('Ctrl Pts',(-0.139403331971461,51.3053551220269,
1.16977054257879));
#45077=CARTESIAN_POINT('Ctrl Pts',(-0.0407383696870978,51.3124717240502,
1.17928451237274));
#45078=CARTESIAN_POINT('Ctrl Pts',(0.0320517482618634,51.3178436886102,
1.1795518796349));
#45079=CARTESIAN_POINT('Ctrl Pts',(0.132697673873903,51.3252393043525,1.17059549570839));
#45080=CARTESIAN_POINT('Ctrl Pts',(0.160897548225851,51.3273060734476,1.16705360006949));
#45081=CARTESIAN_POINT('Ctrl Pts',(0.188938476720627,51.3293408135491,1.16249615677407));
#45082=CARTESIAN_POINT('',(-1.17774999976701,51.2893671147362,2.34267279165755E-5));
#45083=CARTESIAN_POINT('Ctrl Pts',(0.18893837638019,51.427308721746,1.16249617308222));
#45084=CARTESIAN_POINT('Ctrl Pts',(0.167780174989307,51.4257360879916,1.16593497684819));
#45085=CARTESIAN_POINT('Ctrl Pts',(0.146525093563944,51.4241589555535,1.16879662929704));
#45086=CARTESIAN_POINT('Ctrl Pts',(0.0744055527542759,51.418832162536,1.17650673483916));
#45087=CARTESIAN_POINT('Ctrl Pts',(0.0233102087280465,51.4150970553667,
1.17862710853437));
#45088=CARTESIAN_POINT('Ctrl Pts',(-0.0405152136121301,51.4105874701334,
1.17712201115765));
#45089=CARTESIAN_POINT('Ctrl Pts',(-0.0532600023433328,51.4096949223222,
1.17661426000105));
#45090=CARTESIAN_POINT('Ctrl Pts',(-0.072735501794312,51.4083456019064,
1.17552124243315));
#45091=CARTESIAN_POINT('Ctrl Pts',(-0.0794731812488466,51.4078814729405,
1.17508496022441));
#45092=CARTESIAN_POINT('Ctrl Pts',(-0.091831473921267,51.4070355324296,
1.17417794590902));
#45093=CARTESIAN_POINT('Ctrl Pts',(-0.0974527636959587,51.4066528402923,
1.17372476714136));
#45094=CARTESIAN_POINT('Ctrl Pts',(-0.110767715544907,51.4057510925089,
1.17255501921064));
#45095=CARTESIAN_POINT('Ctrl Pts',(-0.118457900540155,51.4052339703768,
1.17180309514844));
#45096=CARTESIAN_POINT('Ctrl Pts',(-0.144744876568355,51.4034772420464,
1.16897139686902));
#45097=CARTESIAN_POINT('Ctrl Pts',(-0.163300211919216,51.4022559435375,
1.16652404168512));
#45098=CARTESIAN_POINT('Ctrl Pts',(-0.210591949586825,51.3991731845479,
1.15913582489187));
#45099=CARTESIAN_POINT('Ctrl Pts',(-0.239218277354355,51.3973355420423,
1.15356823024454));
#45100=CARTESIAN_POINT('Ctrl Pts',(-0.358192952257415,51.3897103972331,
1.1258085136181));
#45101=CARTESIAN_POINT('Ctrl Pts',(-0.445948766863184,51.3840880113415,
1.0940185434197));
#45102=CARTESIAN_POINT('Ctrl Pts',(-0.551737390743096,51.3765122948905,
1.04082932542601));
#45103=CARTESIAN_POINT('Ctrl Pts',(-0.574047382370542,51.3748674948078,
1.02869299991465));
#45104=CARTESIAN_POINT('Ctrl Pts',(-0.606634683896286,51.372382602165,1.009575640819));
#45105=CARTESIAN_POINT('Ctrl Pts',(-0.617222844451097,51.3715618199211,
1.00313735601702));
#45106=CARTESIAN_POINT('Ctrl Pts',(-0.636176652026868,51.3700669368533,
0.991198528930466));
#45107=CARTESIAN_POINT('Ctrl Pts',(-0.644577591169899,51.369395024632,0.985756042144522));
#45108=CARTESIAN_POINT('Ctrl Pts',(-0.662610458342805,51.3679318079224,
0.973744499216107));
#45109=CARTESIAN_POINT('Ctrl Pts',(-0.672216185156617,51.3671391486798,
0.967138228250668));
#45110=CARTESIAN_POINT('Ctrl Pts',(-0.699211437608676,51.3648726854243,
0.947975967038142));
#45111=CARTESIAN_POINT('Ctrl Pts',(-0.716357449216303,51.3633862892541,
0.935086610213727));
#45112=CARTESIAN_POINT('Ctrl Pts',(-0.793330562604256,51.3564904718998,
0.87386291113953));
#45113=CARTESIAN_POINT('Ctrl Pts',(-0.848677326237563,51.3508761527402,
0.820215294973942));
#45114=CARTESIAN_POINT('Ctrl Pts',(-0.937374133903037,51.3407959364567,
0.715582883139381));
#45115=CARTESIAN_POINT('Ctrl Pts',(-0.972770288346427,51.3363636073935,
0.66666958629533));
#45116=CARTESIAN_POINT('Ctrl Pts',(-1.01091726541823,51.3312059417839,0.604403318100627));
#45117=CARTESIAN_POINT('Ctrl Pts',(-1.01739081566078,51.3303151488728,0.593441698469523));
#45118=CARTESIAN_POINT('Ctrl Pts',(-1.02702163454418,51.3289679150825,0.576512911972019));
#45119=CARTESIAN_POINT('Ctrl Pts',(-1.03030723663795,51.3285041507016,0.570620345994147));
#45120=CARTESIAN_POINT('Ctrl Pts',(-1.03624659777287,51.3276585211019,0.559749824898884));
#45121=CARTESIAN_POINT('Ctrl Pts',(-1.03891538224669,51.3272757807603,0.554780774970583));
#45122=CARTESIAN_POINT('Ctrl Pts',(-1.04515906457285,51.3263734609112,0.542952495746081));
#45123=CARTESIAN_POINT('Ctrl Pts',(-1.0487022468717,51.3258558226858,0.536076942650783));
#45124=CARTESIAN_POINT('Ctrl Pts',(-1.06060816652715,51.324095201414,0.512403608216472));
#45125=CARTESIAN_POINT('Ctrl Pts',(-1.06863753754756,51.3228706354384,0.495440256450002));
#45126=CARTESIAN_POINT('Ctrl Pts',(-1.08814551674467,51.3197771614402,0.451543082856523));
#45127=CARTESIAN_POINT('Ctrl Pts',(-1.09903191498767,51.3179322813617,0.424359387068967));
#45128=CARTESIAN_POINT('Ctrl Pts',(-1.13882945481606,51.3105606260455,0.313140511963303));
#45129=CARTESIAN_POINT('Ctrl Pts',(-1.15920077778096,51.3051834696005,0.226369194553585));
#45130=CARTESIAN_POINT('Ctrl Pts',(-1.17285020539874,51.2977662631761,0.110793778666655));
#45131=CARTESIAN_POINT('Ctrl Pts',(-1.17511915485752,51.2959890681501,0.0833525912917017));
#45132=CARTESIAN_POINT('Ctrl Pts',(-1.17694443035614,51.2934631968828,0.0449109468104858));
#45133=CARTESIAN_POINT('Ctrl Pts',(-1.17731138884305,51.2927393751073,0.0339568204069161));
#45134=CARTESIAN_POINT('Ctrl Pts',(-1.17767546588511,51.2914999929461,0.0153168226509932));
#45135=CARTESIAN_POINT('Ctrl Pts',(-1.17775032938723,51.2909868759087,0.00763308451535553));
#45136=CARTESIAN_POINT('Ctrl Pts',(-1.17774999891067,51.2904714046889,-5.06548628808275E-5));
#45137=CARTESIAN_POINT('Ctrl Pts',(-1.17774999976701,51.2893671147362,2.34267279165755E-5));
#45138=CARTESIAN_POINT('Ctrl Pts',(-1.17775098584611,51.2860358491932,-0.0495504902548409));
#45139=CARTESIAN_POINT('Ctrl Pts',(-1.17461756283641,51.2827045836502,-0.0990659735613131));
#45140=CARTESIAN_POINT('Ctrl Pts',(-1.1683981279826,51.2793733181072,-0.148124532157086));
#45141=CARTESIAN_POINT('Ctrl Pts',(-1.16220075919595,51.2760538716331,-0.197009034833941));
#45142=CARTESIAN_POINT('Ctrl Pts',(-1.15293941438527,51.272734425159,-0.245439390503012));
#45143=CARTESIAN_POINT('Ctrl Pts',(-1.14071301295608,51.2694149786849,-0.293033930753193));
#45144=CARTESIAN_POINT('Ctrl Pts',(-1.12842131238035,51.2660778036074,-0.340882665410138));
#45145=CARTESIAN_POINT('Ctrl Pts',(-1.11313296878558,51.26274062853,-0.387886174007096));
#45146=CARTESIAN_POINT('Ctrl Pts',(-1.0949976714854,51.2594034534525,-0.433676333158223));
#45147=CARTESIAN_POINT('Ctrl Pts',(-1.07686237418522,51.256066278375,-0.479466492309345));
#45148=CARTESIAN_POINT('Ctrl Pts',(-1.0558803976495,51.2527291032976,-0.524042897517819));
#45149=CARTESIAN_POINT('Ctrl Pts',(-1.03224706539606,51.2493919282201,-0.567063540073974));
#45150=CARTESIAN_POINT('Ctrl Pts',(-1.00882545342797,51.2460846493779,-0.609698780240791));
#45151=CARTESIAN_POINT('Ctrl Pts',(-0.982702983883552,51.2427773705356,
-0.650980507097607));
#45152=CARTESIAN_POINT('Ctrl Pts',(-0.954064531220093,51.2394700916934,
-0.690547560105591));
#45153=CARTESIAN_POINT('Ctrl Pts',(-0.926613588631255,51.2362999510894,
-0.728473942277681));
#45154=CARTESIAN_POINT('Ctrl Pts',(-0.896851585769304,51.2331298104854,
-0.764824550574183));
#45155=CARTESIAN_POINT('Ctrl Pts',(-0.864987948315027,51.2299596698814,
-0.79930651928391));
#45156=CARTESIAN_POINT('Ctrl Pts',(-0.83315629824842,51.22679271173,-0.833753872105784));
#45157=CARTESIAN_POINT('Ctrl Pts',(-0.799227566282257,51.2236257535786,
-0.866335889631641));
#45158=CARTESIAN_POINT('Ctrl Pts',(-0.763451669643917,51.2204587954272,
-0.896792401070568));
#45159=CARTESIAN_POINT('Ctrl Pts',(-0.727695879834679,51.2172936171749,
-0.927231795290136));
#45160=CARTESIAN_POINT('Ctrl Pts',(-0.690095406083873,51.2141284389227,
-0.955547688190852));
#45161=CARTESIAN_POINT('Ctrl Pts',(-0.650935286476295,51.2109632606704,
-0.981518372380275));
#45162=CARTESIAN_POINT('Ctrl Pts',(-0.611779873486442,51.2077984628379,
-1.00748593517774));
#45163=CARTESIAN_POINT('Ctrl Pts',(-0.571065652962939,51.2046336650054,
-1.03110854201715));
#45164=CARTESIAN_POINT('Ctrl Pts',(-0.529106582671327,51.2014688671729,
-1.05220781534537));
#45165=CARTESIAN_POINT('Ctrl Pts',(-0.487104733704155,51.1983008427232,
-1.07332860008845));
#45166=CARTESIAN_POINT('Ctrl Pts',(-0.443856002868032,51.1951328182734,
-1.09192066801306));
#45167=CARTESIAN_POINT('Ctrl Pts',(-0.399697098116125,51.1919647938237,
-1.10785255889832));
#45168=CARTESIAN_POINT('Ctrl Pts',(-0.355511452057059,51.1887948509134,
-1.12379409765845));
#45169=CARTESIAN_POINT('Ctrl Pts',(-0.310415071177013,51.1856249080032,
-1.13707209616858));
#45170=CARTESIAN_POINT('Ctrl Pts',(-0.264759183772611,51.1824549650929,
-1.14760517474786));
#45171=CARTESIAN_POINT('Ctrl Pts',(-0.219019813394498,51.1792792258599,
-1.15815751333438));
#45172=CARTESIAN_POINT('Ctrl Pts',(-0.172719446179654,51.1761034866269,
-1.16595482962459));
#45173=CARTESIAN_POINT('Ctrl Pts',(-0.126216922168788,51.1729277473938,
-1.17096727155725));
#45174=CARTESIAN_POINT('Ctrl Pts',(-0.112010662799723,51.1719575769312,
-1.17249854435765));
#45175=CARTESIAN_POINT('Ctrl Pts',(-0.0977855444772725,51.1709874064686,
-1.1737702818834));
#45176=CARTESIAN_POINT('Ctrl Pts',(-0.083551780083155,51.1700172360059,
-1.17478260224815));
#45177=CARTESIAN_POINT('Ctrl Pts',(-0.0350293506342434,51.1667099571637,
-1.17823356870497));
#45178=CARTESIAN_POINT('Ctrl Pts',(0.0138210693818673,51.1634026783214,
-1.17868136187856));
#45179=CARTESIAN_POINT('Ctrl Pts',(0.0625957882037462,51.1600953994792,
-1.17608538371972));
#45180=CARTESIAN_POINT('Ctrl Pts',(0.109348059870649,51.1569252571873,-1.17359704797827));
#45181=CARTESIAN_POINT('Ctrl Pts',(0.156030159644109,51.1537551148954,-1.16831243738101));
#45182=CARTESIAN_POINT('Ctrl Pts',(0.202282451386361,51.1505849726035,-1.16024862523561));
#45183=CARTESIAN_POINT('Ctrl Pts',(0.248488310997001,51.1474180127802,-1.15219290825637));
#45184=CARTESIAN_POINT('Ctrl Pts',(0.294264668904109,51.1442510529569,-1.1413636068324));
#45185=CARTESIAN_POINT('Ctrl Pts',(0.339257391268508,51.1410840931336,-1.12782954606168));
#45186=CARTESIAN_POINT('Ctrl Pts',(0.384224826492013,51.1379189132283,-1.11430309180338));
#45187=CARTESIAN_POINT('Ctrl Pts',(0.428408964712441,51.1347537333231,-1.09807504974805));
#45188=CARTESIAN_POINT('Ctrl Pts',(0.471468933732513,51.1315885534178,-1.07926461399655));
#45189=CARTESIAN_POINT('Ctrl Pts',(0.514523727118959,51.1284237539544,-1.06045643918314));
#45190=CARTESIAN_POINT('Ctrl Pts',(0.556454108913126,51.1252589544909,-1.03906671208195));
#45191=CARTESIAN_POINT('Ctrl Pts',(0.596939920603469,51.1220941550275,-1.01526242602094));
#45192=CARTESIAN_POINT('Ctrl Pts',(0.637467008344609,51.1189261289911,-0.991433871040036));
#45193=CARTESIAN_POINT('Ctrl Pts',(0.676546105853428,51.1157581029547,-0.96518612986692));
#45194=CARTESIAN_POINT('Ctrl Pts',(0.713884128734477,51.1125900769183,-0.936730758137586));
#45195=CARTESIAN_POINT('Ctrl Pts',(0.751244762108054,51.1094201324454,-0.908258154912843));
#45196=CARTESIAN_POINT('Ctrl Pts',(0.786861799734846,51.1062501879724,-0.877575625595539));
#45197=CARTESIAN_POINT('Ctrl Pts',(0.820476352944512,51.1030802434994,-0.844934090186254));
#45198=CARTESIAN_POINT('Ctrl Pts',(0.854152370666398,51.0999045027546,-0.81223286943653));
#45199=CARTESIAN_POINT('Ctrl Pts',(0.885818225532972,51.0967287620097,-0.777565910679258));
#45200=CARTESIAN_POINT('Ctrl Pts',(0.915254187814639,51.0935530212648,-0.741218479389016));
#45201=CARTESIAN_POINT('Ctrl Pts',(0.924246599559352,51.0925828621071,-0.730114678368451));
#45202=CARTESIAN_POINT('Ctrl Pts',(0.933031212701967,51.0916127029495,-0.718854254181465));
#45203=CARTESIAN_POINT('Ctrl Pts',(0.941602586729074,51.0906425437918,-0.707445850341294));
#45204=CARTESIAN_POINT('Ctrl Pts',(0.970822456216233,51.0873352649495,-0.6685545278751));
#45205=CARTESIAN_POINT('Ctrl Pts',(0.997697300846977,51.0840279861073,-0.627758608695592));
#45206=CARTESIAN_POINT('Ctrl Pts',(1.021974034713,51.080720707265,-0.585375208624723));
#45207=CARTESIAN_POINT('Ctrl Pts',(1.04524415178131,51.0775505622916,-0.544749204861402));
#45208=CARTESIAN_POINT('Ctrl Pts',(1.06612707311976,51.0743804173181,-0.502665325701072));
#45209=CARTESIAN_POINT('Ctrl Pts',(1.08444205916883,51.0712102723447,-0.45943496036508));
#45210=CARTESIAN_POINT('Ctrl Pts',(1.1027386591622,51.0680433098177,-0.416247993145983));
#45211=CARTESIAN_POINT('Ctrl Pts',(1.11847220888306,51.0648763472907,-0.3719173293596));
#45212=CARTESIAN_POINT('Ctrl Pts',(1.13150842972917,51.0617093847637,-0.326777808230353));
#45213=CARTESIAN_POINT('Ctrl Pts',(1.14453732393725,51.0585442021381,-0.281663656488119));
#45214=CARTESIAN_POINT('Ctrl Pts',(1.15487173727667,51.0553790195126,-0.235742083379568));
#45215=CARTESIAN_POINT('Ctrl Pts',(1.1624268994366,51.052213836887,-0.189364109498653));
#45216=CARTESIAN_POINT('Ctrl Pts',(1.16998115352415,51.049049034692,-0.142991709893506));
#45217=CARTESIAN_POINT('Ctrl Pts',(1.17475673178944,51.045884232497,-0.0961635695605844));
#45218=CARTESIAN_POINT('Ctrl Pts',(1.1767202556796,51.0427194303021,-0.049239236116421));
#45219=CARTESIAN_POINT('Ctrl Pts',(1.17868578141524,51.0395514015383,-0.00226706252884466));
#45220=CARTESIAN_POINT('Ctrl Pts',(1.17783351024976,51.0363833727745,0.0448009409663622));
#45221=CARTESIAN_POINT('Ctrl Pts',(1.17418218625771,51.0332153440107,0.0916037989117204));
#45222=CARTESIAN_POINT('Ctrl Pts',(1.17052865116323,51.0300453968096,0.138434998881334));
#45223=CARTESIAN_POINT('Ctrl Pts',(1.16407276720998,51.0268754496086,0.185000180531924));
#45224=CARTESIAN_POINT('Ctrl Pts',(1.1548848974311,51.0237055024075,0.230945742947455));
#45225=CARTESIAN_POINT('Ctrl Pts',(1.14568022764256,51.0205297589615,0.276975316772712));
#45226=CARTESIAN_POINT('Ctrl Pts',(1.13373375151382,51.0173540155155,0.322382472471943));
#45227=CARTESIAN_POINT('Ctrl Pts',(1.11916592698197,51.0141782720695,0.366827875689118));
#45228=CARTESIAN_POINT('Ctrl Pts',(1.11471568346571,51.0132081319055,0.380405254182543));
#45229=CARTESIAN_POINT('Ctrl Pts',(1.11002115248972,51.0122379917416,0.393893025709404));
#45230=CARTESIAN_POINT('Ctrl Pts',(1.10508664395222,51.0112678515776,0.407281931662105));
#45231=CARTESIAN_POINT('Ctrl Pts',(1.08826454309579,51.0079605727353,0.452925692247782));
#45232=CARTESIAN_POINT('Ctrl Pts',(1.06857035799753,51.0046532938931,0.4976325612908));
#45233=CARTESIAN_POINT('Ctrl Pts',(1.04613320897857,51.0013460150508,0.54101790319009));
#45234=CARTESIAN_POINT('Ctrl Pts',(1.02462648268996,50.9981758823053,0.582604143597785));
#45235=CARTESIAN_POINT('Ctrl Pts',(1.00060010244264,50.9950057495598,0.622975750099127));
#45236=CARTESIAN_POINT('Ctrl Pts',(0.974217620543403,50.9918356168143,0.661811975052393));
#45237=CARTESIAN_POINT('Ctrl Pts',(0.947861623483634,50.9886686665009,0.70060921310567));
#45238=CARTESIAN_POINT('Ctrl Pts',(0.919154518118493,50.9855017161875,0.73787366022939));
#45239=CARTESIAN_POINT('Ctrl Pts',(0.888304759476732,50.9823347658741,0.773310879783147));
#45240=CARTESIAN_POINT('Ctrl Pts',(0.857472338765933,50.9791695954244,0.808728183198395));
#45241=CARTESIAN_POINT('Ctrl Pts',(0.824500015962497,50.9760044249747,0.842319872634824));
#45242=CARTESIAN_POINT('Ctrl Pts',(0.789636695488352,50.972839254525,0.873824325387109));
#45243=CARTESIAN_POINT('Ctrl Pts',(0.754777564660626,50.9696744644448,0.905324992139786));
#45244=CARTESIAN_POINT('Ctrl Pts',(0.718028302689345,50.9665096743647,0.93473854743771));
#45245=CARTESIAN_POINT('Ctrl Pts',(0.679672854675254,50.9633448842845,0.961841916906095));
#45246=CARTESIAN_POINT('Ctrl Pts',(0.641278300311027,50.9601768674557,0.98897292035899));
#45247=CARTESIAN_POINT('Ctrl Pts',(0.601274749852972,50.9570088506269,1.01378871647048));
#45248=CARTESIAN_POINT('Ctrl Pts',(0.559975621549293,50.9538408337982,1.03610924412944));
#45249=CARTESIAN_POINT('Ctrl Pts',(0.518651482791735,50.9506708984413,1.05844328893878));
#45250=CARTESIAN_POINT('Ctrl Pts',(0.476030711412737,50.9475009630844,1.07827882276602));
#45251=CARTESIAN_POINT('Ctrl Pts',(0.4324485306959,50.9443310277275,1.09548314948198));
#45252=CARTESIAN_POINT('Ctrl Pts',(0.388786656222819,50.9411552958718,1.11271893578526));
#45253=CARTESIAN_POINT('Ctrl Pts',(0.344160396506679,50.9379795640162,1.12731374621947));
#45254=CARTESIAN_POINT('Ctrl Pts',(0.298920163199764,50.9348038321606,1.13918470782074));
#45255=CARTESIAN_POINT('Ctrl Pts',(0.28509872797285,50.9338336078948,1.14281142932193));
#45256=CARTESIAN_POINT('Ctrl Pts',(0.271220048283304,50.9328633836291,1.14618427629002));
#45257=CARTESIAN_POINT('Ctrl Pts',(0.257294242770588,50.9318931593634,1.14930184683446));
#45258=CARTESIAN_POINT('Ctrl Pts',(0.23466980178663,50.930316892797,1.15436678119188));
#45259=CARTESIAN_POINT('Ctrl Pts',(0.211870534327436,50.9287406262305,1.1587690496606));
#45260=CARTESIAN_POINT('Ctrl Pts',(0.18893846240316,50.927164359664,1.16249615910107));
#45261=CARTESIAN_POINT('Origin',(0.,56.5393671147362,0.));
#45262=CARTESIAN_POINT('',(0.188938462403167,50.3284861847587,1.16249615910106));
#45263=CARTESIAN_POINT('',(0.188738354032613,50.4271343927849,1.1611983583706));
#45264=CARTESIAN_POINT('',(0.188938462403162,56.5393671147362,1.16249615910107));
#45265=CARTESIAN_POINT('',(-1.17774975332751,50.6906328852214,0.000762257828655969));
#45266=CARTESIAN_POINT('Ctrl Pts',(-1.17774975332751,50.6906328852214,0.000762257828655968));
#45267=CARTESIAN_POINT('Ctrl Pts',(-1.17777960133562,50.6875036592274,-0.0453553192892874));
#45268=CARTESIAN_POINT('Ctrl Pts',(-1.17509643829781,50.6843744332334,-0.0915797958995521));
#45269=CARTESIAN_POINT('Ctrl Pts',(-1.16968895932775,50.6812452072394,-0.137560172022192));
#45270=CARTESIAN_POINT('Ctrl Pts',(-1.16428831115918,50.6781199341265,-0.183482465104016));
#45271=CARTESIAN_POINT('Ctrl Pts',(-1.15617021436046,50.6749946610137,-0.229160700083915));
#45272=CARTESIAN_POINT('Ctrl Pts',(-1.1453753572639,50.6718693879008,-0.274245060981234));
#45273=CARTESIAN_POINT('Ctrl Pts',(-1.13458905489139,50.6687465915089,-0.319293693358658));
#45274=CARTESIAN_POINT('Ctrl Pts',(-1.12113032074461,50.665623795117,-0.363748824722831));
#45275=CARTESIAN_POINT('Ctrl Pts',(-1.1050910789745,50.6625009987251,-0.40726989782081));
#45276=CARTESIAN_POINT('Ctrl Pts',(-1.08905700047954,50.6593792076088,-0.450776960825402));
#45277=CARTESIAN_POINT('Ctrl Pts',(-1.07044425940943,50.6562574164924,-0.493350022218267));
#45278=CARTESIAN_POINT('Ctrl Pts',(-1.04939397700165,50.653135625376,-0.534665637134698));
#45279=CARTESIAN_POINT('Ctrl Pts',(-1.02832572433874,50.6500111692416,-0.576016522463505));
#45280=CARTESIAN_POINT('Ctrl Pts',(-1.00481603678679,50.6468867131071,-0.616107304310351));
#45281=CARTESIAN_POINT('Ctrl Pts',(-0.979052376769155,50.6437622569727,
-0.65463845444846));
#45282=CARTESIAN_POINT('Ctrl Pts',(-0.953276437597511,50.640636311699,-0.693187968822341));
#45283=CARTESIAN_POINT('Ctrl Pts',(-0.925244736251638,50.6375103664252,
-0.730175913647999));
#45284=CARTESIAN_POINT('Ctrl Pts',(-0.895186268754897,50.6343844211515,
-0.765334310437397));
#45285=CARTESIAN_POINT('Ctrl Pts',(-0.865072275691823,50.6312527014689,
-0.800557653648075));
#45286=CARTESIAN_POINT('Ctrl Pts',(-0.832924448549775,50.6281209817863,
-0.833944294490212));
#45287=CARTESIAN_POINT('Ctrl Pts',(-0.799008557989088,50.6249892621037,
-0.865263189301497));
#45288=CARTESIAN_POINT('Ctrl Pts',(-0.783246088514481,50.6235337899022,
-0.879818700458073));
#45289=CARTESIAN_POINT('Ctrl Pts',(-0.767102188339089,50.6220783177007,
-0.893928168453297));
#45290=CARTESIAN_POINT('Ctrl Pts',(-0.750605721389883,50.6206228454992,
-0.907571547326586));
#45291=CARTESIAN_POINT('Ctrl Pts',(-0.713120693467588,50.617315566657,-0.938573484868386));
#45292=CARTESIAN_POINT('Ctrl Pts',(-0.673623973074418,50.6140082878147,
-0.96732176496925));
#45293=CARTESIAN_POINT('Ctrl Pts',(-0.632420466200204,50.6107010089725,
-0.993548899869109));
#45294=CARTESIAN_POINT('Ctrl Pts',(-0.592917355023133,50.607530215666,-1.01869368739819));
#45295=CARTESIAN_POINT('Ctrl Pts',(-0.551846104246025,50.6043594223596,
-1.04152101376355));
#45296=CARTESIAN_POINT('Ctrl Pts',(-0.509509439020997,50.6011886290531,
-1.06183576604318));
#45297=CARTESIAN_POINT('Ctrl Pts',(-0.467215333017838,50.5980210232083,
-1.08213009677934));
#45298=CARTESIAN_POINT('Ctrl Pts',(-0.423658831060098,50.5948534173635,
-1.09991661186439));
#45299=CARTESIAN_POINT('Ctrl Pts',(-0.379168248237177,50.5916858115186,
-1.11504551567582));
#45300=CARTESIAN_POINT('Ctrl Pts',(-0.334702752040581,50.5885199917719,
-1.13016588884699));
#45301=CARTESIAN_POINT('Ctrl Pts',(-0.289304745753612,50.5853541720251,
-1.14263143956209));
#45302=CARTESIAN_POINT('Ctrl Pts',(-0.243321018792249,50.5821883522784,
-1.15234107117377));
#45303=CARTESIAN_POINT('Ctrl Pts',(-0.197342924872337,50.5790229203469,
-1.1620495133482));
#45304=CARTESIAN_POINT('Ctrl Pts',(-0.150779798929501,50.5758574884155,
-1.16900259328095));
#45305=CARTESIAN_POINT('Ctrl Pts',(-0.103989349852103,50.5726920564841,
-1.17315015135205));
#45306=CARTESIAN_POINT('Ctrl Pts',(-0.0571514356966482,50.5695234134812,
-1.17730191678109));
#45307=CARTESIAN_POINT('Ctrl Pts',(-0.0100862952838123,50.5663547704783,
-1.17864243359444));
#45308=CARTESIAN_POINT('Ctrl Pts',(0.0368444992566834,50.5631861274755,
-1.17717354089128));
#45309=CARTESIAN_POINT('Ctrl Pts',(0.0838035848038834,50.5600155743388,
-1.17570376270443));
#45310=CARTESIAN_POINT('Ctrl Pts',(0.130627607303061,50.556845021202,-1.17142125577396));
#45311=CARTESIAN_POINT('Ctrl Pts',(0.17695994161919,50.5536744680653,-1.1643797668983));
#45312=CARTESIAN_POINT('Ctrl Pts',(0.223376710912688,50.5504981369857,-1.15732544577572));
#45313=CARTESIAN_POINT('Ctrl Pts',(0.269299459827032,50.547321805906,-1.14750223200047));
#45314=CARTESIAN_POINT('Ctrl Pts',(0.314383465650027,50.5441454748264,-1.13501458097501));
#45315=CARTESIAN_POINT('Ctrl Pts',(0.328091404984733,50.5431797009793,-1.13121766986285));
#45316=CARTESIAN_POINT('Ctrl Pts',(0.34172193121587,50.5422139271322,-1.12717477801867));
#45317=CARTESIAN_POINT('Ctrl Pts',(0.355265722240397,50.5412481532851,-1.12288972259123));
#45318=CARTESIAN_POINT('Ctrl Pts',(0.401646242518149,50.5379408744428,-1.10821561105307));
#45319=CARTESIAN_POINT('Ctrl Pts',(0.447224421856732,50.5346335956006,-1.09062878989607));
#45320=CARTESIAN_POINT('Ctrl Pts',(0.491610142778868,50.5313263167583,-1.07024040757997));
#45321=CARTESIAN_POINT('Ctrl Pts',(0.534163917951637,50.5281555402707,-1.0506935213474));
#45322=CARTESIAN_POINT('Ctrl Pts',(0.575621176024836,50.524984763783,-1.02857207485304));
#45323=CARTESIAN_POINT('Ctrl Pts',(0.615653809146321,50.5218139872954,-1.00402462608425));
#45324=CARTESIAN_POINT('Ctrl Pts',(0.655646363744687,50.5186463852189,-0.979501752903342));
#45325=CARTESIAN_POINT('Ctrl Pts',(0.694216642462461,50.5154787831425,-0.952557974732043));
#45326=CARTESIAN_POINT('Ctrl Pts',(0.731060739788494,50.512311181066,-0.923387923486061));
#45327=CARTESIAN_POINT('Ctrl Pts',(0.767884212040613,50.5091453521916,-0.894234201435437));
#45328=CARTESIAN_POINT('Ctrl Pts',(0.802982980064314,50.5059795233171,-0.862857020689699));
#45329=CARTESIAN_POINT('Ctrl Pts',(0.836084039999323,50.5028136944427,-0.829492941837608));
#45330=CARTESIAN_POINT('Ctrl Pts',(0.869181178452938,50.4996482406239,-0.796132815626755));
#45331=CARTESIAN_POINT('Ctrl Pts',(0.900280687193004,50.496482786805,-0.760786656012133));
#45332=CARTESIAN_POINT('Ctrl Pts',(0.929146440585488,50.4933173329862,-0.723727817931104));
#45333=CARTESIAN_POINT('Ctrl Pts',(0.958041644055425,50.4901486496359,-0.68663117083685));
#45334=CARTESIAN_POINT('Ctrl Pts',(0.984698202406906,50.4869799662856,-0.647818800622675));
#45335=CARTESIAN_POINT('Ctrl Pts',(1.00892158498275,50.4838112829352,-0.607595505131413));
#45336=CARTESIAN_POINT('Ctrl Pts',(1.03315965209366,50.4806406786871,-0.567347825746148));
#45337=CARTESIAN_POINT('Ctrl Pts',(1.05496134947865,50.477470074439,-0.525688013787875));
#45338=CARTESIAN_POINT('Ctrl Pts',(1.07417844350484,50.4742994701909,-0.482944856075216));
#45339=CARTESIAN_POINT('Ctrl Pts',(1.09343064942889,50.4711230728748,-0.440123601570934));
#45340=CARTESIAN_POINT('Ctrl Pts',(1.11008863631632,50.4679466755587,-0.396215574995143));
#45341=CARTESIAN_POINT('Ctrl Pts',(1.12405323063788,50.4647702782426,-0.351567059310943));
#45342=CARTESIAN_POINT('Ctrl Pts',(1.12829838351607,50.4638046725187,-0.337994178459621));
#45343=CARTESIAN_POINT('Ctrl Pts',(1.13229499011369,50.4628390667948,-0.324352945767847));
#45344=CARTESIAN_POINT('Ctrl Pts',(1.13604120344335,50.4618734610709,-0.310653257795543));
#45345=CARTESIAN_POINT('Ctrl Pts',(1.14887229151292,50.4585661822287,-0.263730702289515));
#45346=CARTESIAN_POINT('Ctrl Pts',(1.1588219373472,50.4552589033864,-0.215900020683312));
#45347=CARTESIAN_POINT('Ctrl Pts',(1.16577105125511,50.4519516245441,-0.167549749494168));
#45348=CARTESIAN_POINT('Ctrl Pts',(1.17242391791113,50.4487853381048,-0.12126069577215));
#45349=CARTESIAN_POINT('Ctrl Pts',(1.17632682284683,50.4456190516655,-0.0744960820848609));
#45350=CARTESIAN_POINT('Ctrl Pts',(1.17742629591009,50.4424527652262,-0.027611233211309));
#45351=CARTESIAN_POINT('Ctrl Pts',(1.17852466466893,50.4392896589868,0.0192265247898934));
#45352=CARTESIAN_POINT('Ctrl Pts',(1.176825160427,50.4361265527474,0.0661837218374673));
#45353=CARTESIAN_POINT('Ctrl Pts',(1.1723261417246,50.4329634465079,0.112900309694455));
#45354=CARTESIAN_POINT('Ctrl Pts',(1.16782964112703,50.4298021106619,0.159590750235196));
#45355=CARTESIAN_POINT('Ctrl Pts',(1.16053678287553,50.4266407748159,0.206040291937972));
#45356=CARTESIAN_POINT('Ctrl Pts',(1.1504979143807,50.4234794389699,0.251892063204993));
#45357=CARTESIAN_POINT('Ctrl Pts',(1.14046020069847,50.4203184667854,0.297738559952893));
#45358=CARTESIAN_POINT('Ctrl Pts',(1.12767722550168,50.4171574946009,0.342986876561605));
#45359=CARTESIAN_POINT('Ctrl Pts',(1.11225025469533,50.4139965224165,0.387291148143334));
#45360=CARTESIAN_POINT('Ctrl Pts',(1.09680727846605,50.4108322707355,0.431641385236569));
#45361=CARTESIAN_POINT('Ctrl Pts',(1.07871501910745,50.4076680190546,0.475045093878604));
#45362=CARTESIAN_POINT('Ctrl Pts',(1.05812372171996,50.4045037673736,0.517174295603998));
#45363=CARTESIAN_POINT('Ctrl Pts',(1.0375197691433,50.4013375709777,0.559329389482157));
#45364=CARTESIAN_POINT('Ctrl Pts',(1.01441399866896,50.3981713745818,0.600207930638587));
#45365=CARTESIAN_POINT('Ctrl Pts',(0.989001906318251,50.3950051781859,0.639507851240988));
#45366=CARTESIAN_POINT('Ctrl Pts',(0.963542676605009,50.3918331087534,0.678880669996738));
#45367=CARTESIAN_POINT('Ctrl Pts',(0.935768925027702,50.388661039321,0.716668578269015));
#45368=CARTESIAN_POINT('Ctrl Pts',(0.905917433478278,50.3854889698885,0.752601266422087));
#45369=CARTESIAN_POINT('Ctrl Pts',(0.896537441149297,50.3844922362113,0.763892103889202));
#45370=CARTESIAN_POINT('Ctrl Pts',(0.886952577258788,50.383495502534,0.77500003826868));
#45371=CARTESIAN_POINT('Ctrl Pts',(0.877170910770406,50.3824987688568,0.785917461186744));
#45372=CARTESIAN_POINT('Ctrl Pts',(0.845949491876466,50.3793173641646,0.820764021798068));
#45373=CARTESIAN_POINT('Ctrl Pts',(0.812579211245098,50.3761359594725,0.853824453538088));
#45374=CARTESIAN_POINT('Ctrl Pts',(0.77729203235371,50.3729545547803,0.884823235985267));
#45375=CARTESIAN_POINT('Ctrl Pts',(0.742060225007989,50.3697781422497,0.91577337610535));
#45376=CARTESIAN_POINT('Ctrl Pts',(0.704917888945249,50.366601729719,0.944667907808254));
#45377=CARTESIAN_POINT('Ctrl Pts',(0.666134917544255,50.3634253171883,0.971266870704601));
#45378=CARTESIAN_POINT('Ctrl Pts',(0.627393529067787,50.3602523103927,0.997837314314606));
#45379=CARTESIAN_POINT('Ctrl Pts',(0.587015445270432,50.357079303597,1.02211674971657));
#45380=CARTESIAN_POINT('Ctrl Pts',(0.545302794957308,50.3539062968013,1.04390608979532));
#45381=CARTESIAN_POINT('Ctrl Pts',(0.50361723764742,50.350735350922,1.06568127736501));
#45382=CARTESIAN_POINT('Ctrl Pts',(0.460599324617646,50.3475644050427,1.08496931928487));
#45383=CARTESIAN_POINT('Ctrl Pts',(0.41657690880579,50.3443934591633,1.10161642214966));
#45384=CARTESIAN_POINT('Ctrl Pts',(0.37254562580824,50.3412218745784,1.11826687814602));
#45385=CARTESIAN_POINT('Ctrl Pts',(0.327509953016673,50.3380502899934,1.13227512669869));
#45386=CARTESIAN_POINT('Ctrl Pts',(0.281816798700614,50.3348787054084,1.14353589994811));
#45387=CARTESIAN_POINT('Ctrl Pts',(0.251117692865634,50.3327478651918,1.15110148991322));
#45388=CARTESIAN_POINT('Ctrl Pts',(0.220122192528981,50.3306170249752,1.15742792212166));
#45389=CARTESIAN_POINT('Ctrl Pts',(0.188938462403167,50.3284861847587,1.16249615910106));
#45390=CARTESIAN_POINT('Ctrl Pts',(-1.17774978721175,50.691380992042,0.000707970817746733));
#45391=CARTESIAN_POINT('Ctrl Pts',(-1.17773238358118,50.6934819144442,0.0296599017206249));
#45392=CARTESIAN_POINT('Ctrl Pts',(-1.17664741682129,50.6955591604751,0.0586042188794689));
#45393=CARTESIAN_POINT('Ctrl Pts',(-1.1739257268983,50.698130269672,0.0951446063022735));
#45394=CARTESIAN_POINT('Ctrl Pts',(-1.17327996126533,50.6986661946033,0.102801986002212));
#45395=CARTESIAN_POINT('Ctrl Pts',(-1.17202848744619,50.6995904147902,0.116087553336253));
#45396=CARTESIAN_POINT('Ctrl Pts',(-1.17145707416217,50.6999803896171,0.12171861854001));
#45397=CARTESIAN_POINT('Ctrl Pts',(-1.17023866037199,50.7007524192947,0.132921008251392));
#45398=CARTESIAN_POINT('Ctrl Pts',(-1.16959242134995,50.7011344733746,0.138492200352297));
#45399=CARTESIAN_POINT('Ctrl Pts',(-1.16808315669741,50.7019700059919,0.150738501743828));
#45400=CARTESIAN_POINT('Ctrl Pts',(-1.16720268496718,50.702422528339,0.157411100701953));
#45401=CARTESIAN_POINT('Ctrl Pts',(-1.16450344391011,50.7037167966332,0.176597518482482));
#45402=CARTESIAN_POINT('Ctrl Pts',(-1.16254022414858,50.7045510528989,0.189090489738766));
#45403=CARTESIAN_POINT('Ctrl Pts',(-1.14950230027356,50.7095255542255,0.264153218678005));
#45404=CARTESIAN_POINT('Ctrl Pts',(-1.133578717653,50.7134535287098,0.325781684112863));
#45405=CARTESIAN_POINT('Ctrl Pts',(-1.09503857902437,50.7207210221512,0.436933749774168));
#45406=CARTESIAN_POINT('Ctrl Pts',(-1.0738205461786,50.724052439107,0.486754164192088));
#45407=CARTESIAN_POINT('Ctrl Pts',(-1.03345953983596,50.7296679961069,0.565920369249477));
#45408=CARTESIAN_POINT('Ctrl Pts',(-1.01630061051121,50.7318977295043,0.596185549189738));
#45409=CARTESIAN_POINT('Ctrl Pts',(-0.990473830412874,50.7350808551219,
0.63737615676897));
#45410=CARTESIAN_POINT('Ctrl Pts',(-0.982912528188526,50.7359944587146,
0.648975892553797));
#45411=CARTESIAN_POINT('Ctrl Pts',(-0.969440003326239,50.7375930205735,
0.668868283703132));
#45412=CARTESIAN_POINT('Ctrl Pts',(-0.963622373339021,50.7382744151777,
0.67722271922699));
#45413=CARTESIAN_POINT('Ctrl Pts',(-0.951362601468362,50.739692920204,0.694350571444581));
#45414=CARTESIAN_POINT('Ctrl Pts',(-0.944905698764399,50.7404305561586,
0.703112168914322));
#45415=CARTESIAN_POINT('Ctrl Pts',(-0.927711725110049,50.7423712660027,
0.725778628177384));
#45416=CARTESIAN_POINT('Ctrl Pts',(-0.916783690469505,50.7435817405991,
0.739534494595114));
#45417=CARTESIAN_POINT('Ctrl Pts',(-0.845546143506708,50.7513350208662,
0.825199703958517));
#45418=CARTESIAN_POINT('Ctrl Pts',(-0.777139465905238,50.7582175682842,
0.889916106344646));
#45419=CARTESIAN_POINT('Ctrl Pts',(-0.671889906922505,50.7678408159439,
0.968011391517464));
#45420=CARTESIAN_POINT('Ctrl Pts',(-0.640943566762677,50.7705658364262,
0.988773861796829));
#45421=CARTESIAN_POINT('Ctrl Pts',(-0.590284600738896,50.7748152149674,
1.01938243874763));
#45422=CARTESIAN_POINT('Ctrl Pts',(-0.571190515499763,50.776371848158,1.03020289540381));
#45423=CARTESIAN_POINT('Ctrl Pts',(-0.544565636007778,50.7784707791179,
1.04432296651246));
#45424=CARTESIAN_POINT('Ctrl Pts',(-0.537287262139458,50.7790373879785,
1.04808615958777));
#45425=CARTESIAN_POINT('Ctrl Pts',(-0.524833065677163,50.7799940463966,
1.05436160922498));
#45426=CARTESIAN_POINT('Ctrl Pts',(-0.519677133943699,50.7803863690419,
1.05691240518364));
#45427=CARTESIAN_POINT('Ctrl Pts',(-0.508637859378323,50.7812182307483,
1.0622735499892));
#45428=CARTESIAN_POINT('Ctrl Pts',(-0.502749585441482,50.7816571254264,
1.0650729676542));
#45429=CARTESIAN_POINT('Ctrl Pts',(-0.486267054232453,50.7828731539292,
1.07274197997591));
#45430=CARTESIAN_POINT('Ctrl Pts',(-0.475622965746376,50.7836441257516,
1.07750351432911));
#45431=CARTESIAN_POINT('Ctrl Pts',(-0.39482868279484,50.789401960397,1.11221546494007));
#45432=CARTESIAN_POINT('Ctrl Pts',(-0.321978978616777,50.7940703672457,
1.13544951884604));
#45433=CARTESIAN_POINT('Ctrl Pts',(-0.200486535163913,50.8017483197142,
1.16155122599014));
#45434=CARTESIAN_POINT('Ctrl Pts',(-0.153018001884107,50.8047211660809,
1.16875196966845));
#45435=CARTESIAN_POINT('Ctrl Pts',(-0.0742224313004178,50.809742454362,
1.17582152210263));
#45436=CARTESIAN_POINT('Ctrl Pts',(-0.0431037979658147,50.8117469367186,
1.17737293426376));
#45437=CARTESIAN_POINT('Ctrl Pts',(0.00136815300788591,50.8146631670213,
1.17782465011632));
#45438=CARTESIAN_POINT('Ctrl Pts',(0.0146993375790103,50.8155438987066,
1.17773370662409));
#45439=CARTESIAN_POINT('Ctrl Pts',(0.0381269527773765,50.8171046190051,
1.17717606656907));
#45440=CARTESIAN_POINT('Ctrl Pts',(0.0482244427663947,50.8177815359742,
1.17680565448047));
#45441=CARTESIAN_POINT('Ctrl Pts',(0.0693956119694622,50.8192102927326,
1.17575608812076));
#45442=CARTESIAN_POINT('Ctrl Pts',(0.0804669115761797,50.8199629029164,
1.17505029301462));
#45443=CARTESIAN_POINT('Ctrl Pts',(0.110079462898091,50.8219912839454,1.17274203767767));
#45444=CARTESIAN_POINT('Ctrl Pts',(0.128594790068155,50.8232757438431,1.17085638999268));
#45445=CARTESIAN_POINT('Ctrl Pts',(0.161058491999941,50.8255576316109,1.16677091894303));
#45446=CARTESIAN_POINT('Ctrl Pts',(0.175021311207389,50.826548840862,1.16475809067173));
#45447=CARTESIAN_POINT('Ctrl Pts',(0.188938575466302,50.827546579051,1.16249614072511));
#45448=CARTESIAN_POINT('',(-1.17774953461646,50.7893671294558,-0.00104700082271912));
#45449=CARTESIAN_POINT('Ctrl Pts',(0.18893846240316,50.927164359664,1.16249615910107));
#45450=CARTESIAN_POINT('Ctrl Pts',(0.142784164703441,50.9239918824189,1.16999753617867));
#45451=CARTESIAN_POINT('Ctrl Pts',(0.0960912008263255,50.9208194051738,
1.17476079817481));
#45452=CARTESIAN_POINT('Ctrl Pts',(0.0492132149086467,50.9176469279288,
1.17672134423506));
#45453=CARTESIAN_POINT('Ctrl Pts',(0.0023935893101753,50.9144784002301,
1.17867944953144));
#45454=CARTESIAN_POINT('Ctrl Pts',(-0.0446100484742123,50.9113098725315,
1.17784171922707));
#45455=CARTESIAN_POINT('Ctrl Pts',(-0.0914375188926661,50.9081413448329,
1.17419514674468));
#45456=CARTESIAN_POINT('Ctrl Pts',(-0.138227383916993,50.9049753616607,
1.17055150268857));
#45457=CARTESIAN_POINT('Ctrl Pts',(-0.184840806630934,50.9018093784884,
1.16410352514596));
#45458=CARTESIAN_POINT('Ctrl Pts',(-0.230918938622777,50.8986433953162,
1.15489025724756));
#45459=CARTESIAN_POINT('Ctrl Pts',(-0.276980426257284,50.8954785557614,
1.14568031736868));
#45460=CARTESIAN_POINT('Ctrl Pts',(-0.322506459461986,50.8923137162066,
1.13370717669309));
#45461=CARTESIAN_POINT('Ctrl Pts',(-0.367147365638656,50.8891488766518,
1.11906115758014));
#45462=CARTESIAN_POINT('Ctrl Pts',(-0.411826012401549,50.8859813614591,
1.10440275634068));
#45463=CARTESIAN_POINT('Ctrl Pts',(-0.455617503926761,50.8828138462664,
1.08706713215073));
#45464=CARTESIAN_POINT('Ctrl Pts',(-0.498188217486216,50.8796463310737,
1.06719424776275));
#45465=CARTESIAN_POINT('Ctrl Pts',(-0.540775509334069,50.8764775823574,
1.04731362428889));
#45466=CARTESIAN_POINT('Ctrl Pts',(-0.5821405815923,50.8733088336411,1.02489403398469));
#45467=CARTESIAN_POINT('Ctrl Pts',(-0.621974046690846,50.8701400849247,
1.00012166647014));
#45468=CARTESIAN_POINT('Ctrl Pts',(-0.661887316002142,50.8669649877902,
0.975299668844766));
#45469=CARTESIAN_POINT('Ctrl Pts',(-0.700262388733832,50.8637898906556,
0.948115798200907));
#45470=CARTESIAN_POINT('Ctrl Pts',(-0.736819797934553,50.8606147935211,
0.91879902474463));
#45471=CARTESIAN_POINT('Ctrl Pts',(-0.767892938235702,50.8579160180638,
0.893880294596601));
#45472=CARTESIAN_POINT('Ctrl Pts',(-0.797653289032728,50.8552172426065,
0.867421451720827));
#45473=CARTESIAN_POINT('Ctrl Pts',(-0.825950597196265,50.8525184671493,
0.839583631028579));
#45474=CARTESIAN_POINT('Ctrl Pts',(-0.858767565167755,50.8493886419648,
0.807299540090532));
#45475=CARTESIAN_POINT('Ctrl Pts',(-0.88977284264808,50.8462588167803,0.77300549370469));
#45476=CARTESIAN_POINT('Ctrl Pts',(-0.918705936922051,50.8431289915958,
0.736935861499613));
#45477=CARTESIAN_POINT('Ctrl Pts',(-0.94759557596985,50.840003867162,0.700920403037952));
#45478=CARTESIAN_POINT('Ctrl Pts',(-0.974418826007374,50.8368787427281,
0.663135074061715));
#45479=CARTESIAN_POINT('Ctrl Pts',(-0.998951946545905,50.8337536182943,
0.623851000634083));
#45480=CARTESIAN_POINT('Ctrl Pts',(-1.0234597983108,50.8306317126952,0.584607389256827));
#45481=CARTESIAN_POINT('Ctrl Pts',(-1.04568188243562,50.8275098070962,0.543868572739639));
#45482=CARTESIAN_POINT('Ctrl Pts',(-1.06543653331898,50.8243879014971,0.501936306685644));
#45483=CARTESIAN_POINT('Ctrl Pts',(-1.08518858364019,50.8212664068752,0.460009560722331));
#45484=CARTESIAN_POINT('Ctrl Pts',(-1.10247357640349,50.8181449122533,0.416890186179884));
#45485=CARTESIAN_POINT('Ctrl Pts',(-1.11715603410307,50.8150234176313,0.372904086820056));
#45486=CARTESIAN_POINT('Ctrl Pts',(-1.13183652688546,50.8119023407513,0.328923874011706));
#45487=CARTESIAN_POINT('Ctrl Pts',(-1.14391500222188,50.8087812638714,0.284077716200727));
#45488=CARTESIAN_POINT('Ctrl Pts',(-1.15330554738567,50.8056601869914,0.238707722684957));
#45489=CARTESIAN_POINT('Ctrl Pts',(-1.16270689885228,50.802535518488,0.193285519006744));
#45490=CARTESIAN_POINT('Ctrl Pts',(-1.16941404099522,50.7994108499846,0.147338843973864));
#45491=CARTESIAN_POINT('Ctrl Pts',(-1.17339242612076,50.7962861814812,0.101218954857428));
#45492=CARTESIAN_POINT('Ctrl Pts',(-1.17632891401069,50.7939798308061,0.0671773797958268));
#45493=CARTESIAN_POINT('Ctrl Pts',(-1.17777983888489,50.7916734801309,0.0330416429229676));
#45494=CARTESIAN_POINT('Ctrl Pts',(-1.17774953461646,50.7893671294558,-0.00104700082271912));
#45495=CARTESIAN_POINT('Ctrl Pts',(-1.17810120469558,50.7893671147362,-0.00104753107751893));
#45496=CARTESIAN_POINT('Ctrl Pts',(-1.1788378426409,50.7839593348025,-0.0810009332839553));
#45497=CARTESIAN_POINT('Ctrl Pts',(-1.13496814489393,50.7520933241307,-0.551332790626785));
#45498=CARTESIAN_POINT('Ctrl Pts',(-0.502684486253736,50.6937690827209,
-1.29806349587743));
#45499=CARTESIAN_POINT('Ctrl Pts',(0.817803162580305,50.6143943905067,-1.12642683757311));
#45500=CARTESIAN_POINT('Ctrl Pts',(1.38993487805217,50.5350196982925,0.0760013926731982));
#45501=CARTESIAN_POINT('Ctrl Pts',(0.839567365761362,50.4725996990519,0.966914061782009));
#45502=CARTESIAN_POINT('Ctrl Pts',(0.328078249322183,50.4366379305494,1.13955181241402));
#45503=CARTESIAN_POINT('Ctrl Pts',(0.18873835403253,50.4271343927849,1.16119835837062));
#45504=CARTESIAN_POINT('Origin',(0.,55.715,0.));
#45505=CARTESIAN_POINT('',(-1.46349970539298,55.454344954121,0.000928608990242965));
#45506=CARTESIAN_POINT('',(-1.46357455043502,55.5256550458429,0.0014857082342598));
#45507=CARTESIAN_POINT('',(-1.4635,55.715,-1.79227059055215E-16));
#45508=CARTESIAN_POINT('',(0.634286466388226,55.6149831334283,1.31890595895111));
#45509=CARTESIAN_POINT('Ctrl Pts',(-1.46349970539256,55.4543449541571,0.000928609651264057));
#45510=CARTESIAN_POINT('Ctrl Pts',(-1.4634682143009,55.4570563262928,0.0505589395830078));
#45511=CARTESIAN_POINT('Ctrl Pts',(-1.46091230617661,55.4597676984285,0.10011308468285));
#45512=CARTESIAN_POINT('Ctrl Pts',(-1.45585397646145,55.4624790705642,0.149403645274732));
#45513=CARTESIAN_POINT('Ctrl Pts',(-1.45023131890728,55.4654929344045,0.204193261307642));
#45514=CARTESIAN_POINT('Ctrl Pts',(-1.44149964314002,55.4685067982449,0.258779993253343));
#45515=CARTESIAN_POINT('Ctrl Pts',(-1.42968466713854,55.4715206620852,0.312784274778906));
#45516=CARTESIAN_POINT('Ctrl Pts',(-1.41789104075309,55.4745290798852,0.366690970776174));
#45517=CARTESIAN_POINT('Ctrl Pts',(-1.40302528350236,55.4775374976852,0.420016794785235));
#45518=CARTESIAN_POINT('Ctrl Pts',(-1.38516471160696,55.4805459154852,0.472388581274784));
#45519=CARTESIAN_POINT('Ctrl Pts',(-1.36732216386837,55.4835512973133,0.524707516304846));
#45520=CARTESIAN_POINT('Ctrl Pts',(-1.34649095805777,55.4865566791415,0.576073825096052));
#45521=CARTESIAN_POINT('Ctrl Pts',(-1.32279872936154,55.4895620609696,0.626127600094015));
#45522=CARTESIAN_POINT('Ctrl Pts',(-1.29912110990318,55.492565589602,0.676150510646314));
#45523=CARTESIAN_POINT('Ctrl Pts',(-1.27258618939207,55.4955691182343,0.724862016522588));
#45524=CARTESIAN_POINT('Ctrl Pts',(-1.24336956297523,55.4985726468667,0.771922521932601));
#45525=CARTESIAN_POINT('Ctrl Pts',(-1.21415948458859,55.5015755023482,0.818972480142311));
#45526=CARTESIAN_POINT('Ctrl Pts',(-1.1822691713679,55.5045783578297,0.864371725312425));
#45527=CARTESIAN_POINT('Ctrl Pts',(-1.14791881148039,55.5075812133113,0.907807607508025));
#45528=CARTESIAN_POINT('Ctrl Pts',(-1.11353807289256,55.5105867244519,0.951281903439411));
#45529=CARTESIAN_POINT('Ctrl Pts',(-1.07669326758234,55.5135922355926,0.992788952558395));
#45530=CARTESIAN_POINT('Ctrl Pts',(-1.03764544852851,55.5165977467332,1.03204853236079));
#45531=CARTESIAN_POINT('Ctrl Pts',(-0.998580863004207,55.5196045483894,
1.07132496956014));
#45532=CARTESIAN_POINT('Ctrl Pts',(-0.957311769947083,55.5226113500455,
1.10835166023693));
#45533=CARTESIAN_POINT('Ctrl Pts',(-0.914134350043771,55.5256181517016,
1.14288697606984));
#45534=CARTESIAN_POINT('Ctrl Pts',(-0.870876293319733,55.528630568768,1.17748678899584));
#45535=CARTESIAN_POINT('Ctrl Pts',(-0.825703219598404,55.5316429858343,
1.20958562469138));
#45536=CARTESIAN_POINT('Ctrl Pts',(-0.778941555092246,55.5346554029007,
1.23898438398168));
#45537=CARTESIAN_POINT('Ctrl Pts',(-0.74169490982564,55.5370548561933,1.26240111155391));
#45538=CARTESIAN_POINT('Ctrl Pts',(-0.703441039287024,55.5394543094858,
1.28410560897184));
#45539=CARTESIAN_POINT('Ctrl Pts',(-0.664354874088175,55.5418537627784,
1.30401873118268));
#45540=CARTESIAN_POINT('Ctrl Pts',(-0.614719493413587,55.5449008198888,
1.32930633349225));
#45541=CARTESIAN_POINT('Ctrl Pts',(-0.563520193639003,55.5479478769992,
1.35181588548473));
#45542=CARTESIAN_POINT('Ctrl Pts',(-0.511105263984488,55.5509949341097,
1.37135103424592));
#45543=CARTESIAN_POINT('Ctrl Pts',(-0.459990530233786,55.5539664064354,
1.39040159740206));
#45544=CARTESIAN_POINT('Ctrl Pts',(-0.407720314823116,55.5569378787611,
1.40662340207885));
#45545=CARTESIAN_POINT('Ctrl Pts',(-0.354642567370892,55.5599093510868,
1.4198805933629));
#45546=CARTESIAN_POINT('Ctrl Pts',(-0.301615480101468,55.5628779872836,
1.43312513128907));
#45547=CARTESIAN_POINT('Ctrl Pts',(-0.24778290885404,55.5658466234804,1.44341052655117));
#45548=CARTESIAN_POINT('Ctrl Pts',(-0.193509041103219,55.5688152596773,
1.45065037173377));
#45549=CARTESIAN_POINT('Ctrl Pts',(-0.139264365231086,55.571782299156,1.45788632287506));
#45550=CARTESIAN_POINT('Ctrl Pts',(-0.0845793984116932,55.5747493386348,
1.46207989783114));
#45551=CARTESIAN_POINT('Ctrl Pts',(-0.0298271696790935,55.5777163781135,
1.46319601897659));
#45552=CARTESIAN_POINT('Ctrl Pts',(0.0274813001988054,55.5808219410564,
1.46436424895598));
#45553=CARTESIAN_POINT('Ctrl Pts',(0.0848628353463616,55.5839275039993,
1.46216048954602));
#45554=CARTESIAN_POINT('Ctrl Pts',(0.141888195121509,55.5870330669422,1.45660563986453));
#45555=CARTESIAN_POINT('Ctrl Pts',(0.196413795785491,55.5900024946763,1.4512942921295));
#45556=CARTESIAN_POINT('Ctrl Pts',(0.25061324320126,55.5929719224103,1.44291969991955));
#45557=CARTESIAN_POINT('Ctrl Pts',(0.30411845769905,55.5959413501444,1.43155307749547));
#45558=CARTESIAN_POINT('Ctrl Pts',(0.357654942063916,55.5989125132908,1.42017981211564));
#45559=CARTESIAN_POINT('Ctrl Pts',(0.410495865403998,55.6018836764372,1.40581118259737));
#45560=CARTESIAN_POINT('Ctrl Pts',(0.462287531165772,55.6048548395837,1.38856850336188));
#45561=CARTESIAN_POINT('Ctrl Pts',(0.514162411669356,55.6078307765594,1.37129811995663));
#45562=CARTESIAN_POINT('Ctrl Pts',(0.56498417446405,55.6108067135352,1.35114468492091));
#45563=CARTESIAN_POINT('Ctrl Pts',(0.61442003466674,55.613782650511,1.3282771815401));
#45564=CARTESIAN_POINT('Ctrl Pts',(0.621067454303904,55.6141828114834,1.32520229034972));
#45565=CARTESIAN_POINT('Ctrl Pts',(0.627689855127081,55.6145829724558,1.32207839229904));
#45566=CARTESIAN_POINT('Ctrl Pts',(0.634286466388226,55.6149831334283,1.31890595895111));
#45567=CARTESIAN_POINT('',(-0.634007094575041,55.615,1.31904027763693));
#45568=CARTESIAN_POINT('Origin',(0.,55.615,0.));
#45569=CARTESIAN_POINT('Ctrl Pts',(-0.63400709457504,55.615,1.31904027763693));
#45570=CARTESIAN_POINT('Ctrl Pts',(-1.07256679420512,55.588541769262,1.10824310512125));
#45571=CARTESIAN_POINT('Ctrl Pts',(-1.43427071524654,55.5587601178763,0.607354686391449));
#45572=CARTESIAN_POINT('Ctrl Pts',(-1.46522723293725,55.5289784664906,0.062380321776885));
#45573=CARTESIAN_POINT('Ctrl Pts',(-1.46474336208885,55.5256550458429,0.0014868947218889));
#45574=CARTESIAN_POINT('Origin',(0.,55.715,0.));
#45575=CARTESIAN_POINT('',(-1.4634496027614,54.9543449877359,0.000746977488451873));
#45576=CARTESIAN_POINT('',(-1.4634998802993,55.0256550458709,0.000591915479193347));
#45577=CARTESIAN_POINT('',(-1.4635,55.715,-1.79227059055215E-16));
#45578=CARTESIAN_POINT('Ctrl Pts',(-1.46349980934833,54.954344988597,0.000747019002576732));
#45579=CARTESIAN_POINT('Ctrl Pts',(-1.4634685843509,54.9576560770049,0.0619205335156351));
#45580=CARTESIAN_POINT('Ctrl Pts',(-1.45959766985196,54.9609671654128,0.122961773930032));
#45581=CARTESIAN_POINT('Ctrl Pts',(-1.45196136132378,54.9642782538206,0.183413345269103));
#45582=CARTESIAN_POINT('Ctrl Pts',(-1.44429538136574,54.9676022077024,0.244099805566855));
#45583=CARTESIAN_POINT('Ctrl Pts',(-1.43283483841439,54.9709261615841,0.304191696763971));
#45584=CARTESIAN_POINT('Ctrl Pts',(-1.41770468045198,54.9742501154658,0.36324329178188));
#45585=CARTESIAN_POINT('Ctrl Pts',(-1.40250127100869,54.9775901620112,0.422580780495997));
#45586=CARTESIAN_POINT('Ctrl Pts',(-1.38359278817325,54.9809302085567,0.480867578854932));
#45587=CARTESIAN_POINT('Ctrl Pts',(-1.36115385057846,54.9842702551021,0.537673176804868));
#45588=CARTESIAN_POINT('Ctrl Pts',(-1.3567631756147,54.9849238091611,0.548788449783657));
#45589=CARTESIAN_POINT('Ctrl Pts',(-1.35223746983837,54.9855773632201,0.559847085362521));
#45590=CARTESIAN_POINT('Ctrl Pts',(-1.34757824592688,54.9862309172791,0.570845969684141));
#45591=CARTESIAN_POINT('Ctrl Pts',(-1.32613120233688,54.9892393158146,0.621475335425864));
#45592=CARTESIAN_POINT('Ctrl Pts',(-1.30178119111294,54.9922477143501,0.671002303954884));
#45593=CARTESIAN_POINT('Ctrl Pts',(-1.274663492119,54.9952561128856,0.71907248025425));
#45594=CARTESIAN_POINT('Ctrl Pts',(-1.24759452264009,54.9982591054388,0.767056276201849));
#45595=CARTESIAN_POINT('Ctrl Pts',(-1.2177679924346,55.001262097992,0.813588017926406));
#45596=CARTESIAN_POINT('Ctrl Pts',(-1.18536665257206,55.0042650905452,0.858334520434843));
#45597=CARTESIAN_POINT('Ctrl Pts',(-1.15299776236589,55.0072650756278,0.903036209715288));
#45598=CARTESIAN_POINT('Ctrl Pts',(-1.11805947891956,55.0102650607104,0.945955775088201));
#45599=CARTESIAN_POINT('Ctrl Pts',(-1.08077877794127,55.013265045793,0.986787455915294));
#45600=CARTESIAN_POINT('Ctrl Pts',(-1.04352063769655,55.0162632154091,1.02759442710312));
#45601=CARTESIAN_POINT('Ctrl Pts',(-1.00392324518647,55.0192613850252,1.06631562812772));
#45602=CARTESIAN_POINT('Ctrl Pts',(-0.962253460080595,55.0222595546413,
1.10267879664158));
#45603=CARTESIAN_POINT('Ctrl Pts',(-0.920592377607056,55.025257098097,1.13903437079696));
#45604=CARTESIAN_POINT('Ctrl Pts',(-0.876860160158432,55.0282546415527,
1.17303254274021));
#45605=CARTESIAN_POINT('Ctrl Pts',(-0.831358363940373,55.0312521850084,
1.20443991992394));
#45606=CARTESIAN_POINT('Ctrl Pts',(-0.785814511376617,55.0342524990301,
1.23587632628063));
#45607=CARTESIAN_POINT('Ctrl Pts',(-0.738498248211412,55.0372528130516,
1.26471685212984));
#45608=CARTESIAN_POINT('Ctrl Pts',(-0.689740646933369,55.0402531270732,
1.29077112222421));
#45609=CARTESIAN_POINT('Ctrl Pts',(-0.640961171813114,55.0432547871085,
1.3168370808959));
#45610=CARTESIAN_POINT('Ctrl Pts',(-0.590739550243402,55.0462564471437,
1.34011406912444));
#45611=CARTESIAN_POINT('Ctrl Pts',(-0.539429025217443,55.0492581071789,
1.36045895812882));
#45612=CARTESIAN_POINT('Ctrl Pts',(-0.488019840116207,55.0522655388176,
1.38084296636419));
#45613=CARTESIAN_POINT('Ctrl Pts',(-0.435518071857954,55.0552729704563,
1.39828344465212));
#45614=CARTESIAN_POINT('Ctrl Pts',(-0.382293312057844,55.058280402095,1.41268682784113));
#45615=CARTESIAN_POINT('Ctrl Pts',(-0.33908009326065,55.0607221378945,1.42438094447978));
#45616=CARTESIAN_POINT('Ctrl Pts',(-0.295390679312955,55.0631638736939,
1.43407400534725));
#45617=CARTESIAN_POINT('Ctrl Pts',(-0.251426222477321,55.0656056094934,
1.44174099776998));
#45618=CARTESIAN_POINT('Ctrl Pts',(-0.197257943091071,55.0686140539618,
1.45118744195465));
#45619=CARTESIAN_POINT('Ctrl Pts',(-0.142441105338817,55.0716224984301,
1.45759699901049));
#45620=CARTESIAN_POINT('Ctrl Pts',(-0.0873468318633905,55.0746309428985,
1.4608910914108));
#45621=CARTESIAN_POINT('Ctrl Pts',(-0.0323515139282667,55.0776339838607,
1.46417926724895));
#45622=CARTESIAN_POINT('Ctrl Pts',(0.022919727367197,55.0806370248228,1.46436305137819));
#45623=CARTESIAN_POINT('Ctrl Pts',(0.0780878397517109,55.083640065785,1.46141525217267));
#45624=CARTESIAN_POINT('Ctrl Pts',(0.133200729689996,55.0866401007486,1.45847040366958));
#45625=CARTESIAN_POINT('Ctrl Pts',(0.188210169783137,55.0896401357122,1.45240020909698));
#45626=CARTESIAN_POINT('Ctrl Pts',(0.242736159893193,55.0926401706758,1.44322950589305));
#45627=CARTESIAN_POINT('Ctrl Pts',(0.297229178550358,55.0956383915409,1.43406434814384));
#45628=CARTESIAN_POINT('Ctrl Pts',(0.351238806173742,55.0986366124061,1.42180248507628));
#45629=CARTESIAN_POINT('Ctrl Pts',(0.404391551688584,55.1016348332713,1.40652043103643));
#45630=CARTESIAN_POINT('Ctrl Pts',(0.457533219018479,55.1046324292422,1.39124156210808));
#45631=CARTESIAN_POINT('Ctrl Pts',(0.509817850889621,55.1076300252131,1.37294389811306));
#45632=CARTESIAN_POINT('Ctrl Pts',(0.560885791387536,55.1106276211841,1.35175418587093));
#45633=CARTESIAN_POINT('Ctrl Pts',(0.612000957901915,55.113627989237,1.33054487805299));
#45634=CARTESIAN_POINT('Ctrl Pts',(0.661896695340679,55.1166283572898,1.30643838128853));
#45635=CARTESIAN_POINT('Ctrl Pts',(0.710233476738354,55.1196287253427,1.2796095726901));
#45636=CARTESIAN_POINT('Ctrl Pts',(0.7585919576928,55.1226304403338,1.252768719987));
#45637=CARTESIAN_POINT('Ctrl Pts',(0.805389639508389,55.1256321553249,1.22320340211702));
#45638=CARTESIAN_POINT('Ctrl Pts',(0.850314661533951,55.128633870316,1.1911327492687));
#45639=CARTESIAN_POINT('Ctrl Pts',(0.895326075978649,55.131641357712,1.15900042341148));
#45640=CARTESIAN_POINT('Ctrl Pts',(0.938457222594922,55.134648845108,1.12435346937979));
#45641=CARTESIAN_POINT('Ctrl Pts',(0.979429011371886,55.1376563325041,1.08745163648003));
#45642=CARTESIAN_POINT('Ctrl Pts',(1.01268779516711,55.1400976555719,1.05749663283736));
#45643=CARTESIAN_POINT('Ctrl Pts',(1.04452428496812,55.1425389786397,1.02605664842551));
#45644=CARTESIAN_POINT('Ctrl Pts',(1.07480842371899,55.1449803017075,0.993287019095031));
#45645=CARTESIAN_POINT('Ctrl Pts',(1.11212006042545,55.147988138917,0.952913128503586));
#45646=CARTESIAN_POINT('Ctrl Pts',(1.14723335600289,55.1509959761264,0.910347695448135));
#45647=CARTESIAN_POINT('Ctrl Pts',(1.17988101179648,55.1540038133358,0.865859716121563));
#45648=CARTESIAN_POINT('Ctrl Pts',(1.21246999821183,55.1570062453198,0.82145168379342));
#45649=CARTESIAN_POINT('Ctrl Pts',(1.24260182698818,55.1600086773038,0.775128384058019));
#45650=CARTESIAN_POINT('Ctrl Pts',(1.27004805762475,55.1630111092878,0.727193358965556));
#45651=CARTESIAN_POINT('Ctrl Pts',(1.29746680377979,55.1660105346554,0.679306335703612));
#45652=CARTESIAN_POINT('Ctrl Pts',(1.32220501722386,55.169009960023,0.629811240817045));
#45653=CARTESIAN_POINT('Ctrl Pts',(1.34407744651238,55.1720093853906,0.579040644321941));
#45654=CARTESIAN_POINT('Ctrl Pts',(1.36593665021578,55.175006997098,0.528300747244649));
#45655=CARTESIAN_POINT('Ctrl Pts',(1.38493329515023,55.1780046088054,0.476287361988805));
#45656=CARTESIAN_POINT('Ctrl Pts',(1.40092907082036,55.1810022205128,0.423355628910736));
#45657=CARTESIAN_POINT('Ctrl Pts',(1.41692151991189,55.1839992088186,0.370434903837164));
#45658=CARTESIAN_POINT('Ctrl Pts',(1.42991418591346,55.1869961971245,0.316596716318655));
#45659=CARTESIAN_POINT('Ctrl Pts',(1.43981846179572,55.1899931854303,0.262211836254961));
#45660=CARTESIAN_POINT('Ctrl Pts',(1.44973192234837,55.1929929529752,0.207776522701447));
#45661=CARTESIAN_POINT('Ctrl Pts',(1.45655117529059,55.19599272052,0.152794025308403));
#45662=CARTESIAN_POINT('Ctrl Pts',(1.46023896601188,55.1989924880649,0.0976443144302231));
#45663=CARTESIAN_POINT('Ctrl Pts',(1.46392841627738,55.2019936055363,0.0424697856080811));
#45664=CARTESIAN_POINT('Ctrl Pts',(1.46448358984535,55.2049947230078,-0.0128715766705545));
#45665=CARTESIAN_POINT('Ctrl Pts',(1.46191941648469,55.2079958404792,-0.0679990419421796));
#45666=CARTESIAN_POINT('Ctrl Pts',(1.45935030043546,55.2110027428907,-0.123232770658072));
#45667=CARTESIAN_POINT('Ctrl Pts',(1.45364987951497,55.2140096453022,-0.178251250939895));
#45668=CARTESIAN_POINT('Ctrl Pts',(1.4448849835864,55.2170165477137,-0.232679251774885));
#45669=CARTESIAN_POINT('Ctrl Pts',(1.43775464273627,55.2194626964497,-0.276957039087768));
#45670=CARTESIAN_POINT('Ctrl Pts',(1.4285972490309,55.2219088451857,-0.320844079201327));
#45671=CARTESIAN_POINT('Ctrl Pts',(1.41747316725082,55.2243549939217,-0.364145671571044));
#45672=CARTESIAN_POINT('Ctrl Pts',(1.4037896749191,55.2273639485602,-0.417410023528928));
#45673=CARTESIAN_POINT('Ctrl Pts',(1.38707060222972,55.2303729031987,-0.47001542865737));
#45674=CARTESIAN_POINT('Ctrl Pts',(1.36739710706093,55.2333818578372,-0.521591220786352));
#45675=CARTESIAN_POINT('Ctrl Pts',(1.34775899147727,55.2363854013596,-0.573074262231615));
#45676=CARTESIAN_POINT('Ctrl Pts',(1.32517718370166,55.239388944882,-0.623530875210123));
#45677=CARTESIAN_POINT('Ctrl Pts',(1.29978293645842,55.2423924884044,-0.672604317627782));
#45678=CARTESIAN_POINT('Ctrl Pts',(1.27441414639096,55.2453930209403,-0.721628564995936));
#45679=CARTESIAN_POINT('Ctrl Pts',(1.24623874338507,55.2483935534762,-0.769271921294565));
#45680=CARTESIAN_POINT('Ctrl Pts',(1.21543578882913,55.2513940860121,-0.815198192609205));
#45681=CARTESIAN_POINT('Ctrl Pts',(1.18465151691794,55.2543927986614,-0.86109660866696));
#45682=CARTESIAN_POINT('Ctrl Pts',(1.15124314584916,55.2573915113108,-0.905279565680527));
#45683=CARTESIAN_POINT('Ctrl Pts',(1.11543415722865,55.2603902239601,-0.947438067045866));
#45684=CARTESIAN_POINT('Ctrl Pts',(1.07963270949874,55.2633883051209,-0.98958769039876));
#45685=CARTESIAN_POINT('Ctrl Pts',(1.04143199003147,55.2663863862818,-1.02971330190103));
#45686=CARTESIAN_POINT('Ctrl Pts',(1.00109557116825,55.2693844674426,-1.06753918306886));
#45687=CARTESIAN_POINT('Ctrl Pts',(0.960722044703797,55.2723853066966,-1.10539986226174));
#45688=CARTESIAN_POINT('Ctrl Pts',(0.918209279542544,55.2753861459506,-1.14095622140911));
#45689=CARTESIAN_POINT('Ctrl Pts',(0.87385643315756,55.2783869852046,-1.17397069138422));
#45690=CARTESIAN_POINT('Ctrl Pts',(0.829483781968685,55.2813891644184,-1.20699990325657));
#45691=CARTESIAN_POINT('Ctrl Pts',(0.783269853607096,55.2843913436322,-1.2374846714938));
#45692=CARTESIAN_POINT('Ctrl Pts',(0.735542760091726,55.287393522846,-1.26523084774149));
#45693=CARTESIAN_POINT('Ctrl Pts',(0.687724175251795,55.2904014571422,-1.29303021252905));
#45694=CARTESIAN_POINT('Ctrl Pts',(0.638387102763967,55.2934093914384,-1.31808025697743));
#45695=CARTESIAN_POINT('Ctrl Pts',(0.587883196447786,55.2964173257345,-1.34023341151246));
#45696=CARTESIAN_POINT('Ctrl Pts',(0.546957794017624,55.2988547792016,-1.35818502814124));
#45697=CARTESIAN_POINT('Ctrl Pts',(0.505266710682442,55.3012922326688,-1.37423527324438));
#45698=CARTESIAN_POINT('Ctrl Pts',(0.463004067676604,55.3037296861359,-1.38832974588709));
#45699=CARTESIAN_POINT('Ctrl Pts',(0.410832891124243,55.3067386038497,-1.40572868661481));
#45700=CARTESIAN_POINT('Ctrl Pts',(0.357568794285465,55.3097475215634,-1.42021973131096));
#45701=CARTESIAN_POINT('Ctrl Pts',(0.303567241783893,55.3127564392772,-1.43167006664096));
#45702=CARTESIAN_POINT('Ctrl Pts',(0.24966245862682,55.3157599650906,-1.44309988327486));
#45703=CARTESIAN_POINT('Ctrl Pts',(0.195023355111327,55.3187634909039,-1.45149969473198));
#45704=CARTESIAN_POINT('Ctrl Pts',(0.140020861134086,55.3217670167173,-1.45678632902951));
#45705=CARTESIAN_POINT('Ctrl Pts',(0.0850732919769199,55.3247675432463,
-1.46206768415846));
#45706=CARTESIAN_POINT('Ctrl Pts',(0.0297635747249087,55.3277680697754,
-1.46424196981431));
#45707=CARTESIAN_POINT('Ctrl Pts',(-0.0255287033080896,55.3307685963045,
-1.46327732686166));
#45708=CARTESIAN_POINT('Ctrl Pts',(-0.0807876585500475,55.3337673145174,
-1.46231326526678));
#45709=CARTESIAN_POINT('Ctrl Pts',(-0.136028667932132,55.3367660327303,
-1.45821403354496));
#45710=CARTESIAN_POINT('Ctrl Pts',(-0.190870910656135,55.3397647509433,
-1.45099984337191));
#45711=CARTESIAN_POINT('Ctrl Pts',(-0.245701813826826,55.3427628491209,
-1.44378714485364));
#45712=CARTESIAN_POINT('Ctrl Pts',(-0.300133590235123,55.3457609472986,
-1.43346083566842));
#45713=CARTESIAN_POINT('Ctrl Pts',(-0.35379164221338,55.3487590454763,-1.42009285749206));
#45714=CARTESIAN_POINT('Ctrl Pts',(-0.407499367981711,55.3517599191348,
-1.40671250394766));
#45715=CARTESIAN_POINT('Ctrl Pts',(-0.460431424062973,55.3547607927934,
-1.39028498329125));
#45716=CARTESIAN_POINT('Ctrl Pts',(-0.512225969490007,55.357761666452,-1.37093282336518));
#45717=CARTESIAN_POINT('Ctrl Pts',(-0.564043809213344,55.3607638897361,
-1.35157195991746));
#45718=CARTESIAN_POINT('Ctrl Pts',(-0.614722633606314,55.3637661130202,
-1.32928404823263));
#45719=CARTESIAN_POINT('Ctrl Pts',(-0.663921385527143,55.3667683363043,
-1.30423948868286));
#45720=CARTESIAN_POINT('Ctrl Pts',(-0.713214697242056,55.3697763298489,
-1.27914679359506));
#45721=CARTESIAN_POINT('Ctrl Pts',(-0.761021795231998,55.3727843233935,
-1.25128713242896));
#45722=CARTESIAN_POINT('Ctrl Pts',(-0.807027992491674,55.3757923169381,
-1.22087594346635));
#45723=CARTESIAN_POINT('Ctrl Pts',(-0.844306456768326,55.3782296707421,
-1.1962339932753));
#45724=CARTESIAN_POINT('Ctrl Pts',(-0.88040295285426,55.3806670245461,-1.16991769516912));
#45725=CARTESIAN_POINT('Ctrl Pts',(-0.915166532093658,55.3831043783501,
-1.14206062384432));
#45726=CARTESIAN_POINT('Ctrl Pts',(-0.957503727813097,55.3860727356739,
-1.10813459244442));
#45727=CARTESIAN_POINT('Ctrl Pts',(-0.998054495391826,55.3890410929977,
-1.07176862385729));
#45728=CARTESIAN_POINT('Ctrl Pts',(-1.03651833694835,55.3920094503214,-1.03318052012696));
#45729=CARTESIAN_POINT('Ctrl Pts',(-1.07489554527512,55.3949711219276,-0.994679329505699));
#45730=CARTESIAN_POINT('Ctrl Pts',(-1.11119478090176,55.3979327935338,-0.953966326324882));
#45731=CARTESIAN_POINT('Ctrl Pts',(-1.14514877261919,55.40089446514,-0.91129936824776));
#45732=CARTESIAN_POINT('Ctrl Pts',(-1.17906926620127,55.4038532148372,-0.868674504294599));
#45733=CARTESIAN_POINT('Ctrl Pts',(-1.21064875745915,55.4068119645343,-0.824099924521325));
#45734=CARTESIAN_POINT('Ctrl Pts',(-1.23965810540703,55.4097707142314,-0.777868903928321));
#45735=CARTESIAN_POINT('Ctrl Pts',(-1.26865107833675,55.4127277937918,-0.731663979537253));
#45736=CARTESIAN_POINT('Ctrl Pts',(-1.29507649266034,55.4156848733521,-0.683804926928464));
#45737=CARTESIAN_POINT('Ctrl Pts',(-1.31874816875926,55.4186419529124,-0.634614463587228));
#45738=CARTESIAN_POINT('Ctrl Pts',(-1.34256530159622,55.4216172030131,-0.585121736717594));
#45739=CARTESIAN_POINT('Ctrl Pts',(-1.36359445535666,55.4245924531138,-0.534281661715596));
#45740=CARTESIAN_POINT('Ctrl Pts',(-1.38169379472098,55.4275677032145,-0.482446377983639));
#45741=CARTESIAN_POINT('Ctrl Pts',(-1.39969521979474,55.4305268577276,-0.430891514157128));
#45742=CARTESIAN_POINT('Ctrl Pts',(-1.41479833346101,55.4334860122407,-0.378352722285895));
#45743=CARTESIAN_POINT('Ctrl Pts',(-1.42691362714353,55.4364451667538,-0.325191867475339));
#45744=CARTESIAN_POINT('Ctrl Pts',(-1.4391277680324,55.4394284646483,-0.271597279721673));
#45745=CARTESIAN_POINT('Ctrl Pts',(-1.44830499876274,55.4424117625429,-0.217370983158963));
#45746=CARTESIAN_POINT('Ctrl Pts',(-1.45440663779413,55.4453950604374,-0.16289131941386));
#45747=CARTESIAN_POINT('Ctrl Pts',(-1.46050827682551,55.4483783583319,-0.108411655668757));
#45748=CARTESIAN_POINT('Ctrl Pts',(-1.46353435472766,55.4513616562265,-0.0536791878676936));
#45749=CARTESIAN_POINT('Ctrl Pts',(-1.46349970539298,55.454344954121,0.000928608990243761));
#45750=CARTESIAN_POINT('Ctrl Pts',(-1.46349924595067,55.5256550458429,0.00148563179094337));
#45751=CARTESIAN_POINT('Ctrl Pts',(-1.46355384318984,55.5227171263939,-0.0522982323151164));
#45752=CARTESIAN_POINT('Ctrl Pts',(-1.46063941780497,55.5197792069449,-0.10621577743416));
#45753=CARTESIAN_POINT('Ctrl Pts',(-1.45473831007084,55.5168412874958,-0.159902155120703));
#45754=CARTESIAN_POINT('Ctrl Pts',(-1.44884470734304,55.5139071044816,-0.21352025467661));
#45755=CARTESIAN_POINT('Ctrl Pts',(-1.43997199045938,55.5109729214673,-0.266907222341851));
#45756=CARTESIAN_POINT('Ctrl Pts',(-1.42815449504172,55.5080387384531,-0.319698276961466));
#45757=CARTESIAN_POINT('Ctrl Pts',(-1.41634689186904,55.5051070115986,-0.372445140995297));
#45758=CARTESIAN_POINT('Ctrl Pts',(-1.4015995059739,55.5021752847442,-0.42459654015682));
#45759=CARTESIAN_POINT('Ctrl Pts',(-1.38399813666318,55.4992435578897,-0.475795552430716));
#45760=CARTESIAN_POINT('Ctrl Pts',(-1.3664038572382,55.4963130119439,-0.526973941584838));
#45761=CARTESIAN_POINT('Ctrl Pts',(-1.34595805090473,55.493382465998,-0.577200180277564));
#45762=CARTESIAN_POINT('Ctrl Pts',(-1.32279625441777,55.4904519200522,-0.626132828797794));
#45763=CARTESIAN_POINT('Ctrl Pts',(-1.29961665952346,55.4875191221631,-0.675103079030449));
#45764=CARTESIAN_POINT('Ctrl Pts',(-1.27371713703299,55.484586324274,-0.722777248762854));
#45765=CARTESIAN_POINT('Ctrl Pts',(-1.24528050137009,55.4816535263849,-0.768835953183423));
#45766=CARTESIAN_POINT('Ctrl Pts',(-1.21683417100642,55.4787197286379,-0.814910360071822));
#45767=CARTESIAN_POINT('Ctrl Pts',(-1.18584932148862,55.4757859308908,-0.859367748945078));
#45768=CARTESIAN_POINT('Ctrl Pts',(-1.15255169799166,55.4728521331437,-0.901918418404091));
#45769=CARTESIAN_POINT('Ctrl Pts',(-1.11918966051721,55.4699126599891,-0.944551401781544));
#45770=CARTESIAN_POINT('Ctrl Pts',(-1.0835062805902,55.4669731868346,-0.985269882275895));
#45771=CARTESIAN_POINT('Ctrl Pts',(-1.04576617187633,55.46403371368,-1.02381900927807));
#45772=CARTESIAN_POINT('Ctrl Pts',(-1.01245691844994,55.4614393476439,-1.057842298676));
#45773=CARTESIAN_POINT('Ctrl Pts',(-0.977546272076871,55.4588449816078,
-1.09017610936883));
#45774=CARTESIAN_POINT('Ctrl Pts',(-0.941236463326947,55.4562506155717,
-1.12067219565035));
#45775=CARTESIAN_POINT('Ctrl Pts',(-0.89908941689693,55.4532391740482,-1.15607089392754));
#45776=CARTESIAN_POINT('Ctrl Pts',(-0.85485358911812,55.4502277325247,-1.18916344235199));
#45777=CARTESIAN_POINT('Ctrl Pts',(-0.808811171130817,55.4472162910012,
-1.21969534698383));
#45778=CARTESIAN_POINT('Ctrl Pts',(-0.762851855995484,55.4442102848868,
-1.25017214398965));
#45779=CARTESIAN_POINT('Ctrl Pts',(-0.715092857972174,55.4412042787724,
-1.27809718026094));
#45780=CARTESIAN_POINT('Ctrl Pts',(-0.66584898706299,55.4381982726581,-1.30325645075219));
#45781=CARTESIAN_POINT('Ctrl Pts',(-0.61665471834428,55.4351952944228,-1.32839037890328));
#45782=CARTESIAN_POINT('Ctrl Pts',(-0.565979007125824,55.4321923161875,
-1.35076382126136));
#45783=CARTESIAN_POINT('Ctrl Pts',(-0.514163582315877,55.4291893379523,
-1.37020730570965));
#45784=CARTESIAN_POINT('Ctrl Pts',(-0.46237993191135,55.4261882012121,-1.38963886696789));
#45785=CARTESIAN_POINT('Ctrl Pts',(-0.409458446126396,55.4231870644718,
-1.40614384656038));
#45786=CARTESIAN_POINT('Ctrl Pts',(-0.355761160543727,55.4201859277316,
-1.41960073494225));
#45787=CARTESIAN_POINT('Ctrl Pts',(-0.302075645105117,55.4171854488238,
-1.43305467364961));
#45788=CARTESIAN_POINT('Ctrl Pts',(-0.247615178994482,55.4141849699159,
-1.4434617195614));
#45789=CARTESIAN_POINT('Ctrl Pts',(-0.192755059142475,55.411184491008,-1.45075074950006));
#45790=CARTESIAN_POINT('Ctrl Pts',(-0.137845635759255,55.4081813155292,
-1.45804633018844));
#45791=CARTESIAN_POINT('Ctrl Pts',(-0.0825363650716257,55.4051781400504,
-1.46221822581618));
#45792=CARTESIAN_POINT('Ctrl Pts',(-0.0272093101413858,55.4021749645716,
-1.46324704115253));
#45793=CARTESIAN_POINT('Ctrl Pts',(0.0281418707602797,55.399170479525,-1.46427630511513));
#45794=CARTESIAN_POINT('Ctrl Pts',(0.0835103231341836,55.3961659944785,
-1.46215977587118));
#45795=CARTESIAN_POINT('Ctrl Pts',(0.138515650026584,55.3931615094319,-1.45693021957049));
#45796=CARTESIAN_POINT('Ctrl Pts',(0.193624860538797,55.3901513500844,-1.45169078667658));
#45797=CARTESIAN_POINT('Ctrl Pts',(0.248369052342751,55.3871411907368,-1.44332666007825));
#45798=CARTESIAN_POINT('Ctrl Pts',(0.302375736754545,55.3841310313892,-1.43192219195812));
#45799=CARTESIAN_POINT('Ctrl Pts',(0.345764838415967,55.3817126620453,-1.42275981452192));
#45800=CARTESIAN_POINT('Ctrl Pts',(0.38867800768965,55.3792942927014,-1.41163606378852));
#45801=CARTESIAN_POINT('Ctrl Pts',(0.430930136872908,55.3768759233575,-1.39861769870637));
#45802=CARTESIAN_POINT('Ctrl Pts',(0.483576999531882,55.3738625945343,-1.38239659714835));
#45803=CARTESIAN_POINT('Ctrl Pts',(0.535414735736252,55.3708492657111,-1.36316547803516));
#45804=CARTESIAN_POINT('Ctrl Pts',(0.586076255091749,55.3678359368879,-1.34102456100462));
#45805=CARTESIAN_POINT('Ctrl Pts',(0.636649562556188,55.3648278548761,-1.31892219576221));
#45806=CARTESIAN_POINT('Ctrl Pts',(0.686050238750951,55.3618197728643,-1.29392029700104));
#45807=CARTESIAN_POINT('Ctrl Pts',(0.733927662556537,55.3588116908524,-1.26616840749337));
#45808=CARTESIAN_POINT('Ctrl Pts',(0.781758704685495,55.3558065229466,-1.23844340287345));
#45809=CARTESIAN_POINT('Ctrl Pts',(0.828068964271635,55.3528013550407,-1.2079739483108));
#45810=CARTESIAN_POINT('Ctrl Pts',(0.872530785051554,55.3497961871349,-1.17495628818153));
#45811=CARTESIAN_POINT('Ctrl Pts',(0.916966985596722,55.3467927508969,-1.14195765381838));
#45812=CARTESIAN_POINT('Ctrl Pts',(0.959556436513209,55.3437893146589,-1.10641403797563));
#45813=CARTESIAN_POINT('Ctrl Pts',(1.00000089248573,55.340785878421,-1.06856467517308));
#45814=CARTESIAN_POINT('Ctrl Pts',(1.04043791773393,55.3377829939943,-1.03072226630707));
#45815=CARTESIAN_POINT('Ctrl Pts',(1.07873034637521,55.3347801095676,-0.990575311700769));
#45816=CARTESIAN_POINT('Ctrl Pts',(1.11461517874458,55.3317772251409,-0.948401419923113));
#45817=CARTESIAN_POINT('Ctrl Pts',(1.15053398718889,55.3287714975568,-0.906187597533764));
#45818=CARTESIAN_POINT('Ctrl Pts',(1.18404030302639,55.3257657699727,-0.861943405947744));
#45819=CARTESIAN_POINT('Ctrl Pts',(1.21491099080409,55.3227600423887,-0.815980106634614));
#45820=CARTESIAN_POINT('Ctrl Pts',(1.24579600263332,55.3197529201419,-0.769995480272567));
#45821=CARTESIAN_POINT('Ctrl Pts',(1.27404267968776,55.3167457978951,-0.722290610220477));
#45822=CARTESIAN_POINT('Ctrl Pts',(1.29947267887532,55.3137386756483,-0.673203540436759));
#45823=CARTESIAN_POINT('Ctrl Pts',(1.32495157941273,55.3107257707691,-0.624022077257494));
#45824=CARTESIAN_POINT('Ctrl Pts',(1.34760276506019,55.3077128658899,-0.573453586299472));
#45825=CARTESIAN_POINT('Ctrl Pts',(1.36729556336216,55.3046999610108,-0.521857348717217));
#45826=CARTESIAN_POINT('Ctrl Pts',(1.38297955616363,55.3023003843883,-0.48076440669777));
#45827=CARTESIAN_POINT('Ctrl Pts',(1.39678796259989,55.2999008077658,-0.439020032257649));
#45828=CARTESIAN_POINT('Ctrl Pts',(1.40867778461437,55.2975012311433,-0.396811226068455));
#45829=CARTESIAN_POINT('Ctrl Pts',(1.42356683378495,55.2944963573717,-0.343955179105175));
#45830=CARTESIAN_POINT('Ctrl Pts',(1.43550931560213,55.2914914836001,-0.290144737559877));
#45831=CARTESIAN_POINT('Ctrl Pts',(1.44438875528196,55.2884866098284,-0.235740055177355));
#45832=CARTESIAN_POINT('Ctrl Pts',(1.45325200784476,55.2854872139073,-0.181434551908938));
#45833=CARTESIAN_POINT('Ctrl Pts',(1.45906321348545,55.2824878179862,-0.126537476220011));
#45834=CARTESIAN_POINT('Ctrl Pts',(1.46175617560072,55.2794884220651,-0.0714222170836544));
#45835=CARTESIAN_POINT('Ctrl Pts',(1.46444640034116,55.2764920750065,-0.0163629821753025));
#45836=CARTESIAN_POINT('Ctrl Pts',(1.4640246336337,55.2734957279477,0.0389134700365081));
#45837=CARTESIAN_POINT('Ctrl Pts',(1.46047632558275,55.270499380889,0.0940274024543575));
#45838=CARTESIAN_POINT('Ctrl Pts',(1.45693020887449,55.2675048842963,0.149107297942038));
#45839=CARTESIAN_POINT('Ctrl Pts',(1.45026141118792,55.2645103877036,0.204024344470546));
#45840=CARTESIAN_POINT('Ctrl Pts',(1.44050745448951,55.2615158911108,0.258399929489455));
#45841=CARTESIAN_POINT('Ctrl Pts',(1.43075563074694,55.2585220493425,0.312763623875092));
#45842=CARTESIAN_POINT('Ctrl Pts',(1.41792008089446,55.2555282075742,0.366585570154613));
#45843=CARTESIAN_POINT('Ctrl Pts',(1.40208971802482,55.2525343658058,0.419495736103585));
#45844=CARTESIAN_POINT('Ctrl Pts',(1.386244785755,55.2495377686693,0.472454597675473));
#45845=CARTESIAN_POINT('Ctrl Pts',(1.36739968532074,55.2465411715327,0.524499492965711));
#45846=CARTESIAN_POINT('Ctrl Pts',(1.34569327485495,55.2435445743962,0.575275464460424));
#45847=CARTESIAN_POINT('Ctrl Pts',(1.32397721920763,55.2405466457302,0.626073998113151));
#45848=CARTESIAN_POINT('Ctrl Pts',(1.29939755524102,55.2375487170643,0.675602008087615));
#45849=CARTESIAN_POINT('Ctrl Pts',(1.27213999548243,55.2345507883984,0.723527526700929));
#45850=CARTESIAN_POINT('Ctrl Pts',(1.2448297464843,55.2315470646949,0.771545686003748));
#45851=CARTESIAN_POINT('Ctrl Pts',(1.21483154885192,55.2285433409915,0.817954718840988));
#45852=CARTESIAN_POINT('Ctrl Pts',(1.18237487347815,55.225539617288,0.862451105030028));
#45853=CARTESIAN_POINT('Ctrl Pts',(1.15567425100956,55.2230685911684,0.899056246966732));
#45854=CARTESIAN_POINT('Ctrl Pts',(1.12731071301053,55.2205975650487,0.934367454944674));
#45855=CARTESIAN_POINT('Ctrl Pts',(1.09743113615349,55.218126538929,0.968234037514105));
#45856=CARTESIAN_POINT('Ctrl Pts',(1.06104696853818,55.2151175863943,1.0094731562158));
#45857=CARTESIAN_POINT('Ctrl Pts',(1.02225765640098,55.2121086338597,1.0487462821852));
#45858=CARTESIAN_POINT('Ctrl Pts',(0.981303895793412,55.209099681325,1.0857600628595));
#45859=CARTESIAN_POINT('Ctrl Pts',(0.940423693769962,55.2060961332827,1.12270736169529));
#45860=CARTESIAN_POINT('Ctrl Pts',(0.897387147029046,55.2030925852404,1.15740301676308));
#45861=CARTESIAN_POINT('Ctrl Pts',(0.852473253623644,55.2000890371981,1.18958883731158));
#45862=CARTESIAN_POINT('Ctrl Pts',(0.807604325458639,55.1970884961376,1.22174243524368));
#45863=CARTESIAN_POINT('Ctrl Pts',(0.76086220113353,55.1940879550772,1.25139086956008));
#45864=CARTESIAN_POINT('Ctrl Pts',(0.712559134285563,55.1910874140167,1.2783159742983));
#45865=CARTESIAN_POINT('Ctrl Pts',(0.664285301521891,55.18808868895,1.30522478336768));
#45866=CARTESIAN_POINT('Ctrl Pts',(0.614452859391236,55.1850899638833,1.32941327266492));
#45867=CARTESIAN_POINT('Ctrl Pts',(0.563401278014001,55.1820912388166,1.35070768485716));
#45868=CARTESIAN_POINT('Ctrl Pts',(0.512360382915796,55.1790931414526,1.37199763963546));
#45869=CARTESIAN_POINT('Ctrl Pts',(0.460101342890859,55.1760950440886,1.39039451677633));
#45870=CARTESIAN_POINT('Ctrl Pts',(0.406984225354113,55.1730969467245,1.40577241768108));
#45871=CARTESIAN_POINT('Ctrl Pts',(0.353818145098614,55.1700960857505,1.42116449374955));
#45872=CARTESIAN_POINT('Ctrl Pts',(0.2997929158096,55.1670952247765,1.43353188582999));
#45873=CARTESIAN_POINT('Ctrl Pts',(0.24528297634443,55.1640943638024,1.44279884651867));
#45874=CARTESIAN_POINT('Ctrl Pts',(0.190748640841548,55.1610921597867,1.45206995465505));
#45875=CARTESIAN_POINT('Ctrl Pts',(0.135729689007291,55.1580899557711,1.4582378060625));
#45876=CARTESIAN_POINT('Ctrl Pts',(0.0806066288835818,55.1550877517554,
1.46127848864617));
#45877=CARTESIAN_POINT('Ctrl Pts',(0.0253778166797984,55.1520797880936,
1.46432500469604));
#45878=CARTESIAN_POINT('Ctrl Pts',(-0.02995497274921,55.1490718244318,1.46423236689615));
#45879=CARTESIAN_POINT('Ctrl Pts',(-0.0850114179338464,55.14606386077,1.46102885283655));
#45880=CARTESIAN_POINT('Ctrl Pts',(-0.12962338207046,55.1436265227517,1.4584330613019));
#45881=CARTESIAN_POINT('Ctrl Pts',(-0.174053837648228,55.1411891847333,
1.45379575896721));
#45882=CARTESIAN_POINT('Ctrl Pts',(-0.218105165681863,55.138751846715,1.44715665589558));
#45883=CARTESIAN_POINT('Ctrl Pts',(-0.27248642703196,55.1357429586362,1.43896069869328));
#45884=CARTESIAN_POINT('Ctrl Pts',(-0.326520527592842,55.1327340705574,
1.42767776515773));
#45885=CARTESIAN_POINT('Ctrl Pts',(-0.379830470494731,55.1297251824786,
1.41335100512355));
#45886=CARTESIAN_POINT('Ctrl Pts',(-0.433044981610845,55.1267216807039,
1.39904989186781));
#45887=CARTESIAN_POINT('Ctrl Pts',(-0.485537401230335,55.1237181789292,
1.38171590105493));
#45888=CARTESIAN_POINT('Ctrl Pts',(-0.536939504491591,55.1207146771545,
1.3614434319928));
#45889=CARTESIAN_POINT('Ctrl Pts',(-0.588290337110829,55.1177141712001,
1.34119118355274));
#45890=CARTESIAN_POINT('Ctrl Pts',(-0.638552518272102,55.1147136652457,
1.31800645561976));
#45891=CARTESIAN_POINT('Ctrl Pts',(-0.687373420401407,55.1117131592913,
1.29203329327292));
#45892=CARTESIAN_POINT('Ctrl Pts',(-0.736164957429819,55.1087144580999,
1.26607575342586));
#45893=CARTESIAN_POINT('Ctrl Pts',(-0.783516467821157,55.1057157569085,
1.23733335106368));
#45894=CARTESIAN_POINT('Ctrl Pts',(-0.829097879551163,55.1027170557172,
1.20599707964977));
#45895=CARTESIAN_POINT('Ctrl Pts',(-0.874669921934138,55.0997189709146,
1.17466724946683));
#45896=CARTESIAN_POINT('Ctrl Pts',(-0.91847215273347,55.096720886112,1.14074490824729));
#45897=CARTESIAN_POINT('Ctrl Pts',(-0.960203543664407,55.0937228013095,
1.10446430668189));
#45898=CARTESIAN_POINT('Ctrl Pts',(-1.00197365063869,55.090721935052,1.06815004600973));
#45899=CARTESIAN_POINT('Ctrl Pts',(-1.0416686792142,55.0877210687946,1.02947350114224));
#45900=CARTESIAN_POINT('Ctrl Pts',(-1.07902194531063,55.0847202025371,0.988708193319984));
#45901=CARTESIAN_POINT('Ctrl Pts',(-1.11639205187186,55.0817179833596,0.947924506737228));
#45902=CARTESIAN_POINT('Ctrl Pts',(-1.15141795619799,55.0787157641822,0.905050590072751));
#45903=CARTESIAN_POINT('Ctrl Pts',(-1.18387323762103,55.0757135450047,0.860393170152288));
#45904=CARTESIAN_POINT('Ctrl Pts',(-1.21639095955814,55.0727055498764,0.815649834099376));
#45905=CARTESIAN_POINT('Ctrl Pts',(-1.24632789125963,55.0696975547481,0.76911658548395));
#45906=CARTESIAN_POINT('Ctrl Pts',(-1.27350156397274,55.0666895596198,0.721128294105139));
#45907=CARTESIAN_POINT('Ctrl Pts',(-1.29552120329789,55.0642520912468,0.682241947046049));
#45908=CARTESIAN_POINT('Ctrl Pts',(-1.31572721393398,55.0618146228737,0.64240077918245));
#45909=CARTESIAN_POINT('Ctrl Pts',(-1.33404579483354,55.0593771545007,0.601792378887404));
#45910=CARTESIAN_POINT('Ctrl Pts',(-1.35874262868613,55.0560909964867,0.547044747473952));
#45911=CARTESIAN_POINT('Ctrl Pts',(-1.38009909771906,55.0528048384726,0.490700317698954));
#45912=CARTESIAN_POINT('Ctrl Pts',(-1.39792695643952,55.0495186804585,0.43316564321254));
#45913=CARTESIAN_POINT('Ctrl Pts',(-1.41570101042178,55.0462424401174,0.375804609214719));
#45914=CARTESIAN_POINT('Ctrl Pts',(-1.42996753253458,55.0429661997763,0.317260822737725));
#45915=CARTESIAN_POINT('Ctrl Pts',(-1.44058626795848,55.0396899594351,0.257960180201249));
#45916=CARTESIAN_POINT('Ctrl Pts',(-1.45115547624072,55.0364289998984,0.19893612345452));
#45917=CARTESIAN_POINT('Ctrl Pts',(-1.45811070118538,55.0331680403617,0.139162595522109));
#45918=CARTESIAN_POINT('Ctrl Pts',(-1.46136203782201,55.0299070808251,0.0790774583095327));
#45919=CARTESIAN_POINT('Ctrl Pts',(-1.46277520030494,55.0284897358403,0.0529620260488936));
#45920=CARTESIAN_POINT('Ctrl Pts',(-1.4634892852701,55.0270723908556,0.0267879257304701));
#45921=CARTESIAN_POINT('Ctrl Pts',(-1.4634998802993,55.0256550458709,0.000591915479186377));
#45922=CARTESIAN_POINT('Origin',(0.,55.715,0.));
#45923=CARTESIAN_POINT('',(-1.46349946245349,54.4543449264189,-0.00125435176163375));
#45924=CARTESIAN_POINT('',(-1.46349941614739,54.5256550458061,-0.00130726288314624));
#45925=CARTESIAN_POINT('',(-1.4635,55.715,-1.79227059055215E-16));
#45926=CARTESIAN_POINT('Ctrl Pts',(-1.46258057639989,54.4543449541571,-0.00125305338302531));
#45927=CARTESIAN_POINT('Ctrl Pts',(-1.45979356777586,54.4728908907694,0.340279369314991));
#45928=CARTESIAN_POINT('Ctrl Pts',(-1.17029252859884,54.51789505812,1.17331067980076));
#45929=CARTESIAN_POINT('Ctrl Pts',(0.217062202804517,54.5893574562082,1.71605622949271));
#45930=CARTESIAN_POINT('Ctrl Pts',(1.55938868398063,54.6687321484225,0.748514022091191));
#45931=CARTESIAN_POINT('Ctrl Pts',(1.47470200890391,54.7481068406366,-0.904002308136149));
#45932=CARTESIAN_POINT('Ctrl Pts',(0.0405007560907972,54.8274815328507,
-1.72925446836193));
#45933=CARTESIAN_POINT('Ctrl Pts',(-1.23375485783567,54.896227570691,-1.07344525015692));
#45934=CARTESIAN_POINT('Ctrl Pts',(-1.46014652428568,54.9385153777931,-0.291311080189099));
#45935=CARTESIAN_POINT('Ctrl Pts',(-1.46149175089378,54.9543449541571,0.000745358607108643));
#45936=CARTESIAN_POINT('Ctrl Pts',(-1.46349988029951,55.0256550458429,0.000591914962299759));
#45937=CARTESIAN_POINT('Ctrl Pts',(-1.46352273945175,55.0225970709691,-0.0559269580044757));
#45938=CARTESIAN_POINT('Ctrl Pts',(-1.46026720689571,55.0195390960954,-0.112428152305842));
#45939=CARTESIAN_POINT('Ctrl Pts',(-1.45376562565274,55.0164811212216,-0.168516336509234));
#45940=CARTESIAN_POINT('Ctrl Pts',(-1.4472533939806,55.0134181369904,-0.224696400397169));
#45941=CARTESIAN_POINT('Ctrl Pts',(-1.43748455285694,55.0103551527591,-0.280461606436067));
#45942=CARTESIAN_POINT('Ctrl Pts',(-1.42454317052395,55.0072921685278,-0.335423620685192));
#45943=CARTESIAN_POINT('Ctrl Pts',(-1.41159150289028,55.0042267499574,-0.390429316577325));
#45944=CARTESIAN_POINT('Ctrl Pts',(-1.39546241426794,55.001161331387,-0.44463007058759));
#45945=CARTESIAN_POINT('Ctrl Pts',(-1.37628990407881,54.9980959128166,-0.497652840774301));
#45946=CARTESIAN_POINT('Ctrl Pts',(-1.35707046383798,54.9950229907815,-0.550805398939841));
#45947=CARTESIAN_POINT('Ctrl Pts',(-1.33479290857018,54.9919500687465,-0.602773749554788));
#45948=CARTESIAN_POINT('Ctrl Pts',(-1.30963927072332,54.9888771467114,-0.653205351003256));
#45949=CARTESIAN_POINT('Ctrl Pts',(-1.28542446849519,54.9859189185698,-0.701754640873667));
#45950=CARTESIAN_POINT('Ctrl Pts',(-1.25854478280758,54.9829606904283,-0.748879575681883));
#45951=CARTESIAN_POINT('Ctrl Pts',(-1.22920027887007,54.9800024622867,-0.794291460627482));
#45952=CARTESIAN_POINT('Ctrl Pts',(-1.19935762844891,54.9769940158504,-0.84047424873267));
#45953=CARTESIAN_POINT('Ctrl Pts',(-1.16684502167947,54.9739855694142,-0.885071281384762));
#45954=CARTESIAN_POINT('Ctrl Pts',(-1.1318567431638,54.9709771229779,-0.927756736949206));
#45955=CARTESIAN_POINT('Ctrl Pts',(-1.09693131524253,54.9679740807128,-0.970365515227181));
#45956=CARTESIAN_POINT('Ctrl Pts',(-1.05953937299723,54.9649710384477,-1.01106912495695));
#45957=CARTESIAN_POINT('Ctrl Pts',(-1.01991831143784,54.9619679961826,-1.04957081132898));
#45958=CARTESIAN_POINT('Ctrl Pts',(-0.980336915308954,54.9589679603227,
-1.08803395289921));
#45959=CARTESIAN_POINT('Ctrl Pts',(-0.938531197625199,54.9559679244628,
-1.12429917090959));
#45960=CARTESIAN_POINT('Ctrl Pts',(-0.894777395778928,54.9529678886028,
-1.15810433986022));
#45961=CARTESIAN_POINT('Ctrl Pts',(-0.851050057434734,54.9499696672471,
-1.19188906251542));
#45962=CARTESIAN_POINT('Ctrl Pts',(-0.805377387735205,54.9469714458913,
-1.22321636233412));
#45963=CARTESIAN_POINT('Ctrl Pts',(-0.758069145018266,54.9439732245355,
-1.25186397878175));
#45964=CARTESIAN_POINT('Ctrl Pts',(-0.71077076876065,54.9409756284794,-1.28050562057198));
#45965=CARTESIAN_POINT('Ctrl Pts',(-0.661837948886245,54.9379780324233,
-1.30646841488371));
#45966=CARTESIAN_POINT('Ctrl Pts',(-0.611607930138179,54.9349804363673,
-1.32957436414519));
#45967=CARTESIAN_POINT('Ctrl Pts',(-0.561331470795344,54.931980068858,-1.3527016762103));
#45968=CARTESIAN_POINT('Ctrl Pts',(-0.509755897711565,54.9289797013488,
-1.37296664414412));
#45969=CARTESIAN_POINT('Ctrl Pts',(-0.457240125395904,54.9259793338395,
-1.39023872688396));
#45970=CARTESIAN_POINT('Ctrl Pts',(-0.404700783568403,54.9229776197406,
-1.40751856147702));
#45971=CARTESIAN_POINT('Ctrl Pts',(-0.351220913178297,54.9199759056417,
-1.42180269638156));
#45972=CARTESIAN_POINT('Ctrl Pts',(-0.297173134507942,54.9169741915427,
-1.43301094836248));
#45973=CARTESIAN_POINT('Ctrl Pts',(-0.243021430149966,54.9139667056025,
-1.44424075211338));
#45974=CARTESIAN_POINT('Ctrl Pts',(-0.188300160387169,54.9109592196622,
-1.45238277874376));
#45975=CARTESIAN_POINT('Ctrl Pts',(-0.133389517620246,54.907951733722,-1.45740848309218));
#45976=CARTESIAN_POINT('Ctrl Pts',(-0.088815903689603,54.9055104125054,
-1.46148808941379));
#45977=CARTESIAN_POINT('Ctrl Pts',(-0.044117724991045,54.9030690912889,
-1.46351523952389));
#45978=CARTESIAN_POINT('Ctrl Pts',(0.000502671042219297,54.9006277700723,
-1.46349991367332));
#45979=CARTESIAN_POINT('Ctrl Pts',(0.0554874744758696,54.8976193797588,
-1.46348102794044));
#45980=CARTESIAN_POINT('Ctrl Pts',(0.110588412878166,54.8946109894453,-1.46035905738128));
#45981=CARTESIAN_POINT('Ctrl Pts',(0.165426389183475,54.8916025991318,-1.45412047635735));
#45982=CARTESIAN_POINT('Ctrl Pts',(0.220165879294719,54.8885996117331,-1.4478930995051));
#45983=CARTESIAN_POINT('Ctrl Pts',(0.274642823368808,54.8855966243344,-1.43856027877067));
#45984=CARTESIAN_POINT('Ctrl Pts',(0.328479157627615,54.8825936369356,-1.4261604723888));
#45985=CARTESIAN_POINT('Ctrl Pts',(0.382261608791315,54.8795936551326,-1.41377307658347));
#45986=CARTESIAN_POINT('Ctrl Pts',(0.435404207407102,54.8765936733296,-1.39832489362432));
#45987=CARTESIAN_POINT('Ctrl Pts',(0.487536911658011,54.8735936915266,-1.37990579742639));
#45988=CARTESIAN_POINT('Ctrl Pts',(0.539638099813497,54.8705955233206,-1.36149783623483));
#45989=CARTESIAN_POINT('Ctrl Pts',(0.590730105965462,54.8675973551145,-1.34012269716246));
#45990=CARTESIAN_POINT('Ctrl Pts',(0.640458195559618,54.8645991869084,-1.3159200392655));
#45991=CARTESIAN_POINT('Ctrl Pts',(0.690175930519373,54.8616016429961,-1.29172242096841));
#45992=CARTESIAN_POINT('Ctrl Pts',(0.738529837567229,54.8586040990838,-1.26469868417835));
#45993=CARTESIAN_POINT('Ctrl Pts',(0.785187457789192,54.8556065551715,-1.23503558901375));
#45994=CARTESIAN_POINT('Ctrl Pts',(0.831888247611472,54.852606237805,-1.20534504830101));
#45995=CARTESIAN_POINT('Ctrl Pts',(0.876889167374615,54.8496059204385,-1.17301055417713));
#45996=CARTESIAN_POINT('Ctrl Pts',(0.919885871830842,54.846605603072,-1.13826281359184));
#45997=CARTESIAN_POINT('Ctrl Pts',(0.962901888589307,54.8436039380897,-1.10349946579021));
#45998=CARTESIAN_POINT('Ctrl Pts',(1.0039115029153,54.8406022731075,-1.06632106656798));
#45999=CARTESIAN_POINT('Ctrl Pts',(1.04264524109831,54.8376006081252,-1.02699715248634));
#46000=CARTESIAN_POINT('Ctrl Pts',(1.08145348983831,54.834593168959,-0.987597592549722));
#46001=CARTESIAN_POINT('Ctrl Pts',(1.11797676575785,54.8315857297928,-0.946044670508383));
#46002=CARTESIAN_POINT('Ctrl Pts',(1.1519848691766,54.8285782906266,-0.90264229414989));
#46003=CARTESIAN_POINT('Ctrl Pts',(1.17959602267748,54.8261365530371,-0.86740393753878));
#46004=CARTESIAN_POINT('Ctrl Pts',(1.20554994260307,54.8236948154477,-0.830947182786983));
#46005=CARTESIAN_POINT('Ctrl Pts',(1.22974520446427,54.8212530778583,-0.79344752951731));
#46006=CARTESIAN_POINT('Ctrl Pts',(1.25955426048327,54.8182448073545,-0.747247191971024));
#46007=CARTESIAN_POINT('Ctrl Pts',(1.28681973469681,54.8152365368508,-0.699266104732976));
#46008=CARTESIAN_POINT('Ctrl Pts',(1.31132461368342,54.8122282663471,-0.649815364198196));
#46009=CARTESIAN_POINT('Ctrl Pts',(1.33578545153028,54.8092254024263,-0.600453498494248));
#46010=CARTESIAN_POINT('Ctrl Pts',(1.35749530680087,54.8062225385056,-0.549627690924813));
#46011=CARTESIAN_POINT('Ctrl Pts',(1.37628139507752,54.8032196745848,-0.497676372317858));
#46012=CARTESIAN_POINT('Ctrl Pts',(1.39504866671308,54.8002198184117,-0.445777089520705));
#46013=CARTESIAN_POINT('Ctrl Pts',(1.41089779322862,54.7972199622386,-0.392755023596504));
#46014=CARTESIAN_POINT('Ctrl Pts',(1.42370353352889,54.7942201060654,-0.338969760623804));
#46015=CARTESIAN_POINT('Ctrl Pts',(1.43650152374846,54.7912220654162,-0.285217048688247));
#46016=CARTESIAN_POINT('Ctrl Pts',(1.44625965588852,54.788224024767,-0.230702568584233));
#46017=CARTESIAN_POINT('Ctrl Pts',(1.45290281510818,54.7852259841177,-0.175800056458286));
#46018=CARTESIAN_POINT('Ctrl Pts',(1.45954458721925,54.782228569467,-0.120909008116791));
#46019=CARTESIAN_POINT('Ctrl Pts',(1.46307261434322,54.7792311548163,-0.0656306134065736));
#46020=CARTESIAN_POINT('Ctrl Pts',(1.46346343367585,54.7762337401656,-0.0103454479689026));
#46021=CARTESIAN_POINT('Ctrl Pts',(1.46385461441479,54.7732335536855,0.0449908418770366));
#46022=CARTESIAN_POINT('Ctrl Pts',(1.46110278696083,54.7702333672053,0.100333384890216));
#46023=CARTESIAN_POINT('Ctrl Pts',(1.45523665797459,54.7672331807251,0.155301382115353));
#46024=CARTESIAN_POINT('Ctrl Pts',(1.44936789622432,54.7642316477381,0.210294049402625));
#46025=CARTESIAN_POINT('Ctrl Pts',(1.44038213257665,54.761230114751,0.264911312928163));
#46026=CARTESIAN_POINT('Ctrl Pts',(1.42835961035724,54.7582285817639,0.318780604021195));
#46027=CARTESIAN_POINT('Ctrl Pts',(1.41631396052695,54.7552212747566,0.372753522953688));
#46028=CARTESIAN_POINT('Ctrl Pts',(1.40122002588493,54.7522139677493,0.425975084581314));
#46029=CARTESIAN_POINT('Ctrl Pts',(1.38320822925877,54.749206660742,0.478087067918401));
#46030=CARTESIAN_POINT('Ctrl Pts',(1.36857770873395,54.746763902376,0.520416295681001));
#46031=CARTESIAN_POINT('Ctrl Pts',(1.35202301228425,54.74432114401,0.5620136445533));
#46032=CARTESIAN_POINT('Ctrl Pts',(1.33363668231757,54.741878385644,0.602698473182883));
#46033=CARTESIAN_POINT('Ctrl Pts',(1.31099320721888,54.7388700344215,0.652803410146271));
#46034=CARTESIAN_POINT('Ctrl Pts',(1.28547384292371,54.735861683199,0.701737332544859));
#46035=CARTESIAN_POINT('Ctrl Pts',(1.25722224614297,54.7328533319765,0.749149166590487));
#46036=CARTESIAN_POINT('Ctrl Pts',(1.22902140692497,54.7298503856371,0.796475819286555));
#46037=CARTESIAN_POINT('Ctrl Pts',(1.19809834478068,54.7268474392976,0.842285359687871));
#46038=CARTESIAN_POINT('Ctrl Pts',(1.16464367048006,54.7238444929581,0.886249045590872));
#46039=CARTESIAN_POINT('Ctrl Pts',(1.13122249344159,54.7208445533878,0.93016871184213));
#46040=CARTESIAN_POINT('Ctrl Pts',(1.09527504391662,54.7178446138174,0.972245765785033));
#46041=CARTESIAN_POINT('Ctrl Pts',(1.05703549326846,54.714844674247,1.01217993260621));
#46042=CARTESIAN_POINT('Ctrl Pts',(1.01881907412523,54.7118465493716,1.05208994283137));
#46043=CARTESIAN_POINT('Ctrl Pts',(0.978313666816864,54.7088484244961,1.08985925377929));
#46044=CARTESIAN_POINT('Ctrl Pts',(0.935792519379252,54.7058502996206,1.12522202727899));
#46045=CARTESIAN_POINT('Ctrl Pts',(0.893280240561043,54.7028528000629,1.16057742517859));
#46046=CARTESIAN_POINT('Ctrl Pts',(0.848753462785047,54.6998553005051,1.19352694426159));
#46047=CARTESIAN_POINT('Ctrl Pts',(0.802519196972512,54.6968578009474,1.22384442985642));
#46048=CARTESIAN_POINT('Ctrl Pts',(0.756242171850833,54.6938575291815,1.25418995428168));
#46049=CARTESIAN_POINT('Ctrl Pts',(0.708254946661054,54.6908572574156,1.28189829080232));
#46050=CARTESIAN_POINT('Ctrl Pts',(0.658893017884118,54.6878569856497,1.30678699143493));
#46051=CARTESIAN_POINT('Ctrl Pts',(0.609508930020067,54.6848553670303,1.33168686486608));
#46052=CARTESIAN_POINT('Ctrl Pts',(0.558749394219457,54.681853748411,1.35376436774521));
#46053=CARTESIAN_POINT('Ctrl Pts',(0.506970947798101,54.6788521297916,1.37288481238911));
#46054=CARTESIAN_POINT('Ctrl Pts',(0.455092907428903,54.6758447376686,1.39204203450895));
#46055=CARTESIAN_POINT('Ctrl Pts',(0.402192548117434,54.6728373455457,1.40823067989922));
#46056=CARTESIAN_POINT('Ctrl Pts',(0.348641572802339,54.6698299534227,1.42136599921129));
#46057=CARTESIAN_POINT('Ctrl Pts',(0.305156680467599,54.6673878667584,1.43203224651504));
#46058=CARTESIAN_POINT('Ctrl Pts',(0.261243144667189,54.6649457800941,1.44068611617323));
#46059=CARTESIAN_POINT('Ctrl Pts',(0.217102745319451,54.6625036934298,1.44730737853946));
#46060=CARTESIAN_POINT('Ctrl Pts',(0.16272743217266,54.6594953557377,1.45546392492125));
#46061=CARTESIAN_POINT('Ctrl Pts',(0.107775865216766,54.6564870180457,1.4605692797054));
#46062=CARTESIAN_POINT('Ctrl Pts',(0.0526209011115321,54.6534786803536,
1.4625536881654));
#46063=CARTESIAN_POINT('Ctrl Pts',(-0.00243496989973289,54.6504757475329,
1.46453453137651));
#46064=CARTESIAN_POINT('Ctrl Pts',(-0.0576929887456028,54.6474728147122,
1.46340553636841));
#46065=CARTESIAN_POINT('Ctrl Pts',(-0.112773589062501,54.6444698818916,
1.45914850772975));
#46066=CARTESIAN_POINT('Ctrl Pts',(-0.167799038727877,54.6414699558228,
1.4548957415338));
#46067=CARTESIAN_POINT('Ctrl Pts',(-0.222646897102024,54.6384700297541,
1.44752118616505));
#46068=CARTESIAN_POINT('Ctrl Pts',(-0.276937883601701,54.6354701036854,
1.43705868308368));
#46069=CARTESIAN_POINT('Ctrl Pts',(-0.331196029517262,54.6324719922701,
1.42660250876395));
#46070=CARTESIAN_POINT('Ctrl Pts',(-0.384897452908743,54.6294738808548,
1.41306218858695));
#46071=CARTESIAN_POINT('Ctrl Pts',(-0.437670606045531,54.6264757694394,
1.3965230719912));
#46072=CARTESIAN_POINT('Ctrl Pts',(-0.49043275341438,54.6234782832761,1.3799874046053));
#46073=CARTESIAN_POINT('Ctrl Pts',(-0.54226651052236,54.6204807971128,1.36045434063509));
#46074=CARTESIAN_POINT('Ctrl Pts',(-0.592815352842416,54.6174833109495,
1.33805911955874));
#46075=CARTESIAN_POINT('Ctrl Pts',(-0.643410948547461,54.6144830523661,
1.31564318480539));
#46076=CARTESIAN_POINT('Ctrl Pts',(-0.692718770243103,54.6114827937827,
1.29036001821938));
#46077=CARTESIAN_POINT('Ctrl Pts',(-0.740403559142361,54.6084825351993,
1.26239249823869));
#46078=CARTESIAN_POINT('Ctrl Pts',(-0.788109755862552,54.6054809296665,
1.23441242239536));
#46079=CARTESIAN_POINT('Ctrl Pts',(-0.834191026089493,54.6024793241337,
1.20374588427166));
#46080=CARTESIAN_POINT('Ctrl Pts',(-0.878340820641819,54.5994777186008,
1.17061934581411));
#46081=CARTESIAN_POINT('Ctrl Pts',(-0.922575540900822,54.5964703392366,
1.13742908577605));
#46082=CARTESIAN_POINT('Ctrl Pts',(-0.964870957345358,54.5934629598724,
1.10176971345234));
#46083=CARTESIAN_POINT('Ctrl Pts',(-1.00495424712117,54.5904555805082,1.06390752003786));
#46084=CARTESIAN_POINT('Ctrl Pts',(-1.03750455812629,54.5880133874106,1.03316088776615));
#46085=CARTESIAN_POINT('Ctrl Pts',(-1.06859667897818,54.5855711943131,1.00096242404768));
#46086=CARTESIAN_POINT('Ctrl Pts',(-1.09810414428273,54.5831290012156,0.96747069118867));
#46087=CARTESIAN_POINT('Ctrl Pts',(-1.1341172943334,54.5801483634155,0.926594838638836));
#46088=CARTESIAN_POINT('Ctrl Pts',(-1.16792915694634,54.5771677256153,0.883609641676309));
#46089=CARTESIAN_POINT('Ctrl Pts',(-1.19928058434743,54.5741870878152,0.838783839858214));
#46090=CARTESIAN_POINT('Ctrl Pts',(-1.23058534817692,54.5712108864065,0.79402475691661));
#46091=CARTESIAN_POINT('Ctrl Pts',(-1.25943662076532,54.5682346849978,0.747430930264581));
#46092=CARTESIAN_POINT('Ctrl Pts',(-1.28561436600705,54.5652584835892,0.699305335255124));
#46093=CARTESIAN_POINT('Ctrl Pts',(-1.31176399018126,54.5622854793222,0.651231438476151));
#46094=CARTESIAN_POINT('Ctrl Pts',(-1.33524551999412,54.5593124750552,0.601629504235346));
#46095=CARTESIAN_POINT('Ctrl Pts',(-1.3558826571817,54.5563394707882,0.550830708978623));
#46096=CARTESIAN_POINT('Ctrl Pts',(-1.3765107506202,54.5533677693718,0.500054175121516));
#46097=CARTESIAN_POINT('Ctrl Pts',(-1.39429670909912,54.5503960679553,0.448082314244971));
#46098=CARTESIAN_POINT('Ctrl Pts',(-1.40911156259441,54.5474243665388,0.395268078856282));
#46099=CARTESIAN_POINT('Ctrl Pts',(-1.4239225907283,54.544453432449,0.342467480695771));
#46100=CARTESIAN_POINT('Ctrl Pts',(-1.43576389637017,54.5414824983592,0.288825460409155));
#46101=CARTESIAN_POINT('Ctrl Pts',(-1.44455659671544,54.5385115642694,0.234709371107956));
#46102=CARTESIAN_POINT('Ctrl Pts',(-1.45335457797144,54.5355388458315,0.180560779591822));
#46103=CARTESIAN_POINT('Ctrl Pts',(-1.45910022057736,54.5325661273937,0.125938084675089));
#46104=CARTESIAN_POINT('Ctrl Pts',(-1.46176623275603,54.5295934089558,0.0712160850809124));
#46105=CARTESIAN_POINT('Ctrl Pts',(-1.46294357534021,54.5282806212515,0.0470502013204441));
#46106=CARTESIAN_POINT('Ctrl Pts',(-1.46352100787057,54.5269678335472,0.022864991273397));
#46107=CARTESIAN_POINT('Ctrl Pts',(-1.463499416148,54.5256550458429,-0.00130726220482866));
#46108=CARTESIAN_POINT('Origin',(0.,55.715,0.));
#46109=CARTESIAN_POINT('',(-1.46349999999901,53.9543449541294,1.70220316479836E-6));
#46110=CARTESIAN_POINT('',(-1.46349998499324,54.0256550457892,0.000209582428622512));
#46111=CARTESIAN_POINT('',(-1.4635,55.715,-1.79227059055215E-16));
#46112=CARTESIAN_POINT('Ctrl Pts',(-1.46349999999901,53.9543449541572,1.70271267885967E-6));
#46113=CARTESIAN_POINT('Ctrl Pts',(-1.46349993602608,53.9573533892216,0.0549871306756696));
#46114=CARTESIAN_POINT('Ctrl Pts',(-1.4603967571549,53.9603618242859,0.110089773684055));
#46115=CARTESIAN_POINT('Ctrl Pts',(-1.45417680140553,53.9633702593503,0.16493053160035));
#46116=CARTESIAN_POINT('Ctrl Pts',(-1.44796802121601,53.9663732890793,0.219672755669014));
#46117=CARTESIAN_POINT('Ctrl Pts',(-1.43865363596765,53.9693763188084,0.274153507271366));
#46118=CARTESIAN_POINT('Ctrl Pts',(-1.42627196782833,53.9723793485375,0.327994700852163));
#46119=CARTESIAN_POINT('Ctrl Pts',(-1.4139026984683,53.9753793710868,0.381781978832245));
#46120=CARTESIAN_POINT('Ctrl Pts',(-1.39847234824465,53.978379393636,0.434930454602946));
#46121=CARTESIAN_POINT('Ctrl Pts',(-1.38007065789482,53.9813794161852,0.487070045494232));
#46122=CARTESIAN_POINT('Ctrl Pts',(-1.36168010205213,53.9843776234788,0.539178087726878));
#46123=CARTESIAN_POINT('Ctrl Pts',(-1.3403219449858,53.9873758307724,0.590277957279319));
#46124=CARTESIAN_POINT('Ctrl Pts',(-1.31613571827124,53.990374038066,0.640014860054559));
#46125=CARTESIAN_POINT('Ctrl Pts',(-1.29195454166697,53.9933716193307,0.689741377710707));
#46126=CARTESIAN_POINT('Ctrl Pts',(-1.26494669903289,53.9963692005953,0.738105018336184));
#46127=CARTESIAN_POINT('Ctrl Pts',(-1.23529883145681,53.99936678186,0.784773245594821));
#46128=CARTESIAN_POINT('Ctrl Pts',(-1.20562354636837,54.0023671352034,0.831484630314773));
#46129=CARTESIAN_POINT('Ctrl Pts',(-1.17330364236257,54.0053674885467,0.876497021543102));
#46130=CARTESIAN_POINT('Ctrl Pts',(-1.13856971830611,54.00836784189,0.91950597961968));
#46131=CARTESIAN_POINT('Ctrl Pts',(-1.10382021305539,54.0113695411535,0.962534230964986));
#46132=CARTESIAN_POINT('Ctrl Pts',(-1.06665488468436,54.014371240417,1.00355686488468));
#46133=CARTESIAN_POINT('Ctrl Pts',(-1.02734317536112,54.0173729396805,1.04230429819652));
#46134=CARTESIAN_POINT('Ctrl Pts',(-0.987955827932152,54.0203804143949,
1.08112628391292));
#46135=CARTESIAN_POINT('Ctrl Pts',(-0.946414247093647,54.0233878891092,
1.11766397294946));
#46136=CARTESIAN_POINT('Ctrl Pts',(-0.903022262819839,54.0263953638236,
1.15168704206123));
#46137=CARTESIAN_POINT('Ctrl Pts',(-0.867725264986005,54.0288417794521,
1.1793629415813));
#46138=CARTESIAN_POINT('Ctrl Pts',(-0.831204594011595,54.0312881950806,
1.20537564955582));
#46139=CARTESIAN_POINT('Ctrl Pts',(-0.793636730561745,54.033734610709,1.2296231088847));
#46140=CARTESIAN_POINT('Ctrl Pts',(-0.747439914276172,54.0367429429103,
1.25943996087319));
#46141=CARTESIAN_POINT('Ctrl Pts',(-0.69946191794101,54.0397512751115,1.28671336006666));
#46142=CARTESIAN_POINT('Ctrl Pts',(-0.650013825152869,54.0427596073127,
1.31122624939792));
#46143=CARTESIAN_POINT('Ctrl Pts',(-0.600654576570762,54.0457625343937,
1.33569509601555));
#46144=CARTESIAN_POINT('Ctrl Pts',(-0.549830942972984,54.0487654614747,
1.35741304220325));
#46145=CARTESIAN_POINT('Ctrl Pts',(-0.497881347329851,54.0517683885557,
1.37620725691337));
#46146=CARTESIAN_POINT('Ctrl Pts',(-0.445983770009828,54.0547683087368,
1.39498265254469));
#46147=CARTESIAN_POINT('Ctrl Pts',(-0.392962958728821,54.057768228918,1.41083993669034));
#46148=CARTESIAN_POINT('Ctrl Pts',(-0.339178497152869,54.0607681490992,
1.42365381925141));
#46149=CARTESIAN_POINT('Ctrl Pts',(-0.285426572291352,54.0637662544895,
1.43645995010082));
#46150=CARTESIAN_POINT('Ctrl Pts',(-0.230912426129334,54.0667643598799,
1.44622620590558));
#46151=CARTESIAN_POINT('Ctrl Pts',(-0.176009798460427,54.0697624652702,
1.4528774211357));
#46152=CARTESIAN_POINT('Ctrl Pts',(-0.121118623008082,54.0727599452815,
1.45952724897945));
#46153=CARTESIAN_POINT('Ctrl Pts',(-0.0658396516920146,54.0757574252928,
1.46306326283564));
#46154=CARTESIAN_POINT('Ctrl Pts',(-0.0105534703801381,54.0787549053042,
1.46346194834814));
#46155=CARTESIAN_POINT('Ctrl Pts',(0.0447838433034418,54.0817551575862,
1.46386100259177));
#46156=CARTESIAN_POINT('Ctrl Pts',(0.100127850262098,54.0847554098682,1.46111692700126));
#46157=CARTESIAN_POINT('Ctrl Pts',(0.155097734339402,54.0877556621503,1.45525837664752));
#46158=CARTESIAN_POINT('Ctrl Pts',(0.210092295193867,54.090757261289,1.44939719630567));
#46159=CARTESIAN_POINT('Ctrl Pts',(0.264711875505141,54.0937588604278,1.44041883993959));
#46160=CARTESIAN_POINT('Ctrl Pts',(0.318583882175109,54.0967604595665,1.42840350042214));
#46161=CARTESIAN_POINT('Ctrl Pts',(0.372559514923604,54.0997678324636,1.41636504866899));
#46162=CARTESIAN_POINT('Ctrl Pts',(0.425784190889171,54.1027752053607,1.40127808736956));
#46163=CARTESIAN_POINT('Ctrl Pts',(0.477899657451986,54.1057825782578,1.38327299091946));
#46164=CARTESIAN_POINT('Ctrl Pts',(0.520221831142743,54.1082248198129,1.36865132734169));
#46165=CARTESIAN_POINT('Ctrl Pts',(0.561812711243729,54.110667061368,1.35210620685036));
#46166=CARTESIAN_POINT('Ctrl Pts',(0.602491761139594,54.1131093029232,1.33373008054813));
#46167=CARTESIAN_POINT('Ctrl Pts',(0.652599867060699,54.1161176351935,1.31109452525543));
#46168=CARTESIAN_POINT('Ctrl Pts',(0.701537431757105,54.1191259674638,1.28558293299416));
#46169=CARTESIAN_POINT('Ctrl Pts',(0.748953361756599,54.1221342997342,1.25733890097837));
#46170=CARTESIAN_POINT('Ctrl Pts',(0.796284098780793,54.1251372268848,1.22914561547586));
#46171=CARTESIAN_POINT('Ctrl Pts',(0.842098175770399,54.1281401540355,1.19822990093416));
#46172=CARTESIAN_POINT('Ctrl Pts',(0.886066823055248,54.1311430811861,1.16478231231453));
#46173=CARTESIAN_POINT('Ctrl Pts',(0.929991443528835,54.1341430014372,1.1313682155297));
#46174=CARTESIAN_POINT('Ctrl Pts',(0.972073875769551,54.1371429216883,1.09542758504222));
#46175=CARTESIAN_POINT('Ctrl Pts',(1.01201381034426,54.1401428419394,1.05719454107203));
#46176=CARTESIAN_POINT('Ctrl Pts',(1.05192958340331,54.1431409473998,1.01898462604034));
#46177=CARTESIAN_POINT('Ctrl Pts',(1.08970504626173,54.1461390528602,0.978485410964945));
#46178=CARTESIAN_POINT('Ctrl Pts',(1.12507431979167,54.1491371583206,0.935970098317945));
#46179=CARTESIAN_POINT('Ctrl Pts',(1.16043621559541,54.1521346384021,0.893463653999441));
#46180=CARTESIAN_POINT('Ctrl Pts',(1.19339258059246,54.1551321184835,0.84894235346802));
#46181=CARTESIAN_POINT('Ctrl Pts',(1.22371721374798,54.1581295985649,0.802713168433708));
#46182=CARTESIAN_POINT('Ctrl Pts',(1.25406989315387,54.1611298509165,0.756441227554957));
#46183=CARTESIAN_POINT('Ctrl Pts',(1.28178568664402,54.1641301032681,0.708458689278313));
#46184=CARTESIAN_POINT('Ctrl Pts',(1.30668209535494,54.1671303556197,0.659101017810481));
#46185=CARTESIAN_POINT('Ctrl Pts',(1.3315896804226,54.1701319548279,0.609721188972472));
#46186=CARTESIAN_POINT('Ctrl Pts',(1.35367514617084,54.173133554036,0.558965482172848));
#46187=CARTESIAN_POINT('Ctrl Pts',(1.3728037507583,54.1761351532441,0.507190409909275));
#46188=CARTESIAN_POINT('Ctrl Pts',(1.39196915037071,54.1791425262094,0.455315745170632));
#46189=CARTESIAN_POINT('Ctrl Pts',(1.40816617043101,54.1821498991748,0.402418304684393));
#46190=CARTESIAN_POINT('Ctrl Pts',(1.42131000508393,54.1851572721401,0.348869774340397));
#46191=CARTESIAN_POINT('Ctrl Pts',(1.43198390959968,54.1875995131392,0.305383842346905));
#46192=CARTESIAN_POINT('Ctrl Pts',(1.44064524891602,54.1900417541383,0.261468894889259));
#46193=CARTESIAN_POINT('Ctrl Pts',(1.44727375927812,54.1924839951374,0.217326748710252));
#46194=CARTESIAN_POINT('Ctrl Pts',(1.45543870299328,54.1954923272071,0.162952821639372));
#46195=CARTESIAN_POINT('Ctrl Pts',(1.46055255904921,54.1985006592768,0.108002164972088));
#46196=CARTESIAN_POINT('Ctrl Pts',(1.46254551339752,54.2015089913464,0.0528476228488291));
#46197=CARTESIAN_POINT('Ctrl Pts',(1.46453488697223,54.2045119182968,-0.00220782220849207));
#46198=CARTESIAN_POINT('Ctrl Pts',(1.46341446723391,54.2075148452472,-0.0574659016324648));
#46199=CARTESIAN_POINT('Ctrl Pts',(1.45916599836584,54.2105177721975,-0.112547053328953));
#46200=CARTESIAN_POINT('Ctrl Pts',(1.4549217835865,54.2135176922487,-0.167573051012567));
#46201=CARTESIAN_POINT('Ctrl Pts',(1.44755576439947,54.2165176122998,-0.222421947242493));
#46202=CARTESIAN_POINT('Ctrl Pts',(1.43710172189686,54.219517532351,-0.276714457376353));
#46203=CARTESIAN_POINT('Ctrl Pts',(1.42665400352655,54.2225156376122,-0.330974123467612));
#46204=CARTESIAN_POINT('Ctrl Pts',(1.41312206399171,54.2255137428734,-0.384677552264548));
#46205=CARTESIAN_POINT('Ctrl Pts',(1.39659119359043,54.2285118481346,-0.43745318376445));
#46206=CARTESIAN_POINT('Ctrl Pts',(1.38006377138099,54.2315093280178,-0.490217806739235));
#46207=CARTESIAN_POINT('Ctrl Pts',(1.36053881836953,54.234506807901,-0.542054512266186));
#46208=CARTESIAN_POINT('Ctrl Pts',(1.33815151727725,54.2375042877842,-0.592606755621791));
#46209=CARTESIAN_POINT('Ctrl Pts',(1.31574351088537,54.2405045399409,-0.643205753132372));
#46210=CARTESIAN_POINT('Ctrl Pts',(1.29046808152626,54.2435047920975,-0.692517430171096));
#46211=CARTESIAN_POINT('Ctrl Pts',(1.26250805423934,54.2465050442541,-0.74020650022868));
#46212=CARTESIAN_POINT('Ctrl Pts',(1.23453547527884,54.2495066432687,-0.78791697862163));
#46213=CARTESIAN_POINT('Ctrl Pts',(1.20387618937576,54.2525082422833,-0.834002956764934));
#46214=CARTESIAN_POINT('Ctrl Pts',(1.17075660960583,54.2555098412979,-0.878157850881181));
#46215=CARTESIAN_POINT('Ctrl Pts',(1.13757332226858,54.2585172140745,-0.922397679676829));
#46216=CARTESIAN_POINT('Ctrl Pts',(1.10192062801555,54.2615245868511,-0.964698597828198));
#46217=CARTESIAN_POINT('Ctrl Pts',(1.06406477447401,54.2645319596277,-1.00478774162684));
#46218=CARTESIAN_POINT('Ctrl Pts',(1.03332260046163,54.2669742022023,-1.03734353734581));
#46219=CARTESIAN_POINT('Ctrl Pts',(1.00112830682736,54.2694164447769,-1.06844130958447));
#46220=CARTESIAN_POINT('Ctrl Pts',(0.967640446453791,54.2718586873516,-1.09795456025589));
#46221=CARTESIAN_POINT('Ctrl Pts',(0.926390404078387,54.2748670195821,-1.13430871448525));
#46222=CARTESIAN_POINT('Ctrl Pts',(0.883000809343282,54.2778753518127,-1.16841251976987));
#46223=CARTESIAN_POINT('Ctrl Pts',(0.837747015186586,54.2808836840433,-1.20000507855007));
#46224=CARTESIAN_POINT('Ctrl Pts',(0.792574529298209,54.2838866111517,-1.23154087443793));
#46225=CARTESIAN_POINT('Ctrl Pts',(0.745544920711969,54.2868895382602,-1.260574077247));
#46226=CARTESIAN_POINT('Ctrl Pts',(0.696967153554221,54.2898924653686,-1.28688345892957));
#46227=CARTESIAN_POINT('Ctrl Pts',(0.648438028449004,54.292892385576,-1.31316649641394));
#46228=CARTESIAN_POINT('Ctrl Pts',(0.598364278136964,54.2958923057834,-1.33673086467611));
#46229=CARTESIAN_POINT('Ctrl Pts',(0.54708286080914,54.2988922259909,-1.3573992019332));
#46230=CARTESIAN_POINT('Ctrl Pts',(0.495832466008745,54.3018903314063,-1.37805503594656));
#46231=CARTESIAN_POINT('Ctrl Pts',(0.443376341644131,54.3048884368216,-1.39581811383031));
#46232=CARTESIAN_POINT('Ctrl Pts',(0.390072897403153,54.307886542237,-1.41055853643566));
#46233=CARTESIAN_POINT('Ctrl Pts',(0.336780571824872,54.3108840222722,-1.42529588430936));
#46234=CARTESIAN_POINT('Ctrl Pts',(0.282641786766773,54.3138815023073,-1.43701168791634));
#46235=CARTESIAN_POINT('Ctrl Pts',(0.228029401594911,54.3168789823424,-1.44562610726573));
#46236=CARTESIAN_POINT('Ctrl Pts',(0.173366507261933,54.3198792346461,-1.45424849380229));
#46237=CARTESIAN_POINT('Ctrl Pts',(0.118229661204808,54.3228794869499,-1.45976368225195));
#46238=CARTESIAN_POINT('Ctrl Pts',(0.0629997072737128,54.3258797392536,
-1.46214338793547));
#46239=CARTESIAN_POINT('Ctrl Pts',(0.00774495983722705,54.3288813384129,
-1.46452416190245));
#46240=CARTESIAN_POINT('Ctrl Pts',(-0.0476024489784899,54.3318829375723,
-1.46376665434922));
#46241=CARTESIAN_POINT('Ctrl Pts',(-0.102662144137076,54.3348845367316,
-1.45989476818063));
#46242=CARTESIAN_POINT('Ctrl Pts',(-0.157827749925949,54.3378919096471,
-1.45601543420647));
#46243=CARTESIAN_POINT('Ctrl Pts',(-0.212704010310351,54.3408992825627,
-1.44900982032604));
#46244=CARTESIAN_POINT('Ctrl Pts',(-0.266917270148343,54.3439066554783,
-1.43895358538646));
#46245=CARTESIAN_POINT('Ctrl Pts',(-0.310943025945519,54.3463488968408,
-1.43078707141899));
#46246=CARTESIAN_POINT('Ctrl Pts',(-0.354531603814856,54.3487911382033,
-1.42060974891572));
#46247=CARTESIAN_POINT('Ctrl Pts',(-0.397490727899304,54.3512333795657,
-1.40848619845353));
#46248=CARTESIAN_POINT('Ctrl Pts',(-0.450407420777729,54.3542417122277,
-1.39355250950907));
#46249=CARTESIAN_POINT('Ctrl Pts',(-0.502594203267989,54.3572500448897,
-1.37560071000914));
#46250=CARTESIAN_POINT('Ctrl Pts',(-0.553682533718253,54.3602583775517,
-1.35472059918469));
#46251=CARTESIAN_POINT('Ctrl Pts',(-0.604679072979523,54.3632613050962,
-1.33387800397647));
#46252=CARTESIAN_POINT('Ctrl Pts',(-0.654580591136171,54.3662642326406,
-1.31011773653688));
#46253=CARTESIAN_POINT('Ctrl Pts',(-0.703033640352132,54.369267160185,-1.28357935108556));
#46254=CARTESIAN_POINT('Ctrl Pts',(-0.751438172445503,54.3722670808309,
-1.25706753911354));
#46255=CARTESIAN_POINT('Ctrl Pts',(-0.798396647012399,54.3752670014768,
-1.2277833720989));
#46256=CARTESIAN_POINT('Ctrl Pts',(-0.843577282665841,54.3782669221226,
-1.19591371685842));
#46257=CARTESIAN_POINT('Ctrl Pts',(-0.888730586469374,54.3812650279782,
-1.16406334104198));
#46258=CARTESIAN_POINT('Ctrl Pts',(-0.932107751592581,54.3842631338337,
-1.12963088107265));
#46259=CARTESIAN_POINT('Ctrl Pts',(-0.973405233355805,54.3872612396893,
-1.09284697084063));
#46260=CARTESIAN_POINT('Ctrl Pts',(-1.01469410081568,54.3902587201654,-1.05607073341933));
#46261=CARTESIAN_POINT('Ctrl Pts',(-1.05390375154847,54.3932562006416,-1.01694437120819));
#46262=CARTESIAN_POINT('Ctrl Pts',(-1.09076485699683,54.3962536811178,-0.975737811474319));
#46263=CARTESIAN_POINT('Ctrl Pts',(-1.12766005401229,54.3992539338604,-0.9344931412123));
#46264=CARTESIAN_POINT('Ctrl Pts',(-1.16220201232692,54.4022541866031,-0.891164824363979));
#46265=CARTESIAN_POINT('Ctrl Pts',(-1.19416038342083,54.4052544393457,-0.846057461800444));
#46266=CARTESIAN_POINT('Ctrl Pts',(-1.22613310107108,54.4082560389435,-0.800929849915821));
#46267=CARTESIAN_POINT('Ctrl Pts',(-1.25551963809301,54.4112576385412,-0.754022049243226));
#46268=CARTESIAN_POINT('Ctrl Pts',(-1.28213374261602,54.4142592381389,-0.70566657568956));
#46269=CARTESIAN_POINT('Ctrl Pts',(-1.30879904090305,54.4172666114865,-0.657218087595426));
#46270=CARTESIAN_POINT('Ctrl Pts',(-1.3326810233957,54.4202739848341,-0.607316841650005));
#46271=CARTESIAN_POINT('Ctrl Pts',(-1.3536405631197,54.4232813581817,-0.55631778317521));
#46272=CARTESIAN_POINT('Ctrl Pts',(-1.37066145665484,54.4257235960478,-0.514902296188243));
#46273=CARTESIAN_POINT('Ctrl Pts',(-1.38575594771885,54.4281658339138,-0.472763328227954));
#46274=CARTESIAN_POINT('Ctrl Pts',(-1.39887399106228,54.4306080717799,-0.430097439110576));
#46275=CARTESIAN_POINT('Ctrl Pts',(-1.41857703393164,54.4342762649786,-0.366014113546658));
#46276=CARTESIAN_POINT('Ctrl Pts',(-1.43388913296348,54.4379444581773,-0.300521302854243));
#46277=CARTESIAN_POINT('Ctrl Pts',(-1.44464494335243,54.441612651376,-0.234164979547004));
#46278=CARTESIAN_POINT('Ctrl Pts',(-1.45524603995122,54.4452280805288,-0.168763139250205));
#46279=CARTESIAN_POINT('Ctrl Pts',(-1.46142092106582,54.4488435096816,-0.10252243931409));
#46280=CARTESIAN_POINT('Ctrl Pts',(-1.46305749085711,54.4524589388344,-0.0359865036769872));
#46281=CARTESIAN_POINT('Ctrl Pts',(-1.46334206291177,54.4530876013625,-0.0244170197394469));
#46282=CARTESIAN_POINT('Ctrl Pts',(-1.46348953364981,54.4537162638907,-0.0128386611170273));
#46283=CARTESIAN_POINT('Ctrl Pts',(-1.46349946245349,54.4543449264188,-0.00125435176163375));
#46284=CARTESIAN_POINT('Ctrl Pts',(-1.46349941614739,54.5256550458061,-0.00130726288314757));
#46285=CARTESIAN_POINT('Ctrl Pts',(-1.46343776422637,54.5219065796245,-0.0703274665285052));
#46286=CARTESIAN_POINT('Ctrl Pts',(-1.45848961851053,54.5181581134429,-0.13913082750592));
#46287=CARTESIAN_POINT('Ctrl Pts',(-1.44876956711919,54.5144096472613,-0.207120716948527));
#46288=CARTESIAN_POINT('Ctrl Pts',(-1.43955953911841,54.5108578678414,-0.271543090897566));
#46289=CARTESIAN_POINT('Ctrl Pts',(-1.42606575562852,54.5073060884214,-0.335235472021534));
#46290=CARTESIAN_POINT('Ctrl Pts',(-1.40842466851716,54.5037543090015,-0.39770869127081));
#46291=CARTESIAN_POINT('Ctrl Pts',(-1.39348277695714,54.5007459738234,-0.45062312117727));
#46292=CARTESIAN_POINT('Ctrl Pts',(-1.37552288279277,54.4977376386452,-0.502807170500935));
#46293=CARTESIAN_POINT('Ctrl Pts',(-1.35463484295704,54.4947293034671,-0.553892311055827));
#46294=CARTESIAN_POINT('Ctrl Pts',(-1.33378433265413,54.4917263733636,-0.604885666959094));
#46295=CARTESIAN_POINT('Ctrl Pts',(-1.3100163151661,54.48872344326,-0.654783546654793));
#46296=CARTESIAN_POINT('Ctrl Pts',(-1.28347040005656,54.4857205131565,-0.703232523550111));
#46297=CARTESIAN_POINT('Ctrl Pts',(-1.25695106572798,54.4827205899272,-0.751632987834817));
#46298=CARTESIAN_POINT('Ctrl Pts',(-1.22765959633201,54.4797206666979,-0.798586961608401));
#46299=CARTESIAN_POINT('Ctrl Pts',(-1.19578291064711,54.4767207434685,-0.843762692114504));
#46300=CARTESIAN_POINT('Ctrl Pts',(-1.16392550841339,54.4737226350098,-0.888911094058218));
#46301=CARTESIAN_POINT('Ctrl Pts',(-1.12948629366787,54.4707245265512,-0.932282953475559));
#46302=CARTESIAN_POINT('Ctrl Pts',(-1.09269594786137,54.4677264180925,-0.973574761139249));
#46303=CARTESIAN_POINT('Ctrl Pts',(-1.05591327601637,54.4647289349981,-1.01485795589823));
#46304=CARTESIAN_POINT('Ctrl Pts',(-1.01678079848737,54.4617314519037,-1.05406156572294));
#46305=CARTESIAN_POINT('Ctrl Pts',(-0.97556848477783,54.4587339688093,-1.090916303622));
#46306=CARTESIAN_POINT('Ctrl Pts',(-0.934318055219737,54.4557337134461,
-1.12780512719794));
#46307=CARTESIAN_POINT('Ctrl Pts',(-0.890984341139564,54.4527334580829,
-1.16234038489046));
#46308=CARTESIAN_POINT('Ctrl Pts',(-0.845871979587388,54.4497332027197,
-1.19429177513241));
#46309=CARTESIAN_POINT('Ctrl Pts',(-0.800739366405015,54.4467316004959,
-1.22625750884291));
#46310=CARTESIAN_POINT('Ctrl Pts',(-0.753826963071888,54.4437299982722,
-1.2556367815072));
#46311=CARTESIAN_POINT('Ctrl Pts',(-0.705467314835336,54.4407283960484,
-1.28224339253475));
#46312=CARTESIAN_POINT('Ctrl Pts',(-0.657014644503662,54.4377210200992,
-1.30890118265049));
#46313=CARTESIAN_POINT('Ctrl Pts',(-0.607109646006053,54.4347136441501,
-1.33277542708262));
#46314=CARTESIAN_POINT('Ctrl Pts',(-0.556107286701153,54.4317062682009,
-1.35372705361084));
#46315=CARTESIAN_POINT('Ctrl Pts',(-0.514689506526157,54.4292640510631,
-1.37074136184444));
#46316=CARTESIAN_POINT('Ctrl Pts',(-0.472548556674602,54.4268218339252,
-1.38582918825657));
#46317=CARTESIAN_POINT('Ctrl Pts',(-0.42988099944998,54.4243796167873,-1.3989405192187));
#46318=CARTESIAN_POINT('Ctrl Pts',(-0.377322935550869,54.4213712841633,
-1.41509110798764));
#46319=CARTESIAN_POINT('Ctrl Pts',(-0.323741358591926,54.4183629515393,
-1.42831011315973));
#46320=CARTESIAN_POINT('Ctrl Pts',(-0.269494607687241,54.4153546189152,
-1.43847311633812));
#46321=CARTESIAN_POINT('Ctrl Pts',(-0.215345322320914,54.4123516913846,
-1.44861785957357));
#46322=CARTESIAN_POINT('Ctrl Pts',(-0.160533750147607,54.4093487638541,
-1.45571740011836));
#46323=CARTESIAN_POINT('Ctrl Pts',(-0.105432531682753,54.4063458363235,
-1.45969730809609));
#46324=CARTESIAN_POINT('Ctrl Pts',(-0.0503864870309643,54.4033459156767,
-1.4636732309224));
#46325=CARTESIAN_POINT('Ctrl Pts',(0.0049481045831354,54.40034599503,-1.46453567080183));
#46326=CARTESIAN_POINT('Ctrl Pts',(0.0601911479564839,54.3973460743832,
-1.46226169877614));
#46327=CARTESIAN_POINT('Ctrl Pts',(0.115400772536663,54.3943479685121,-1.45998910236983));
#46328=CARTESIAN_POINT('Ctrl Pts',(0.170518431290405,54.3913498626409,-1.45458387610775));
#46329=CARTESIAN_POINT('Ctrl Pts',(0.225164017286448,54.3883517567698,-1.44607517623374));
#46330=CARTESIAN_POINT('Ctrl Pts',(0.279798204946626,54.3853542762633,-1.43756825116032));
#46331=CARTESIAN_POINT('Ctrl Pts',(0.333959993074543,54.3823567957568,-1.42595921913628));
#46332=CARTESIAN_POINT('Ctrl Pts',(0.387276712919702,54.3793593152503,-1.41132880564031));
#46333=CARTESIAN_POINT('Ctrl Pts',(0.440642743967967,54.3763590624545,-1.39668486086759));
#46334=CARTESIAN_POINT('Ctrl Pts',(0.493161633905515,54.3733588096587,-1.37901409145004));
#46335=CARTESIAN_POINT('Ctrl Pts',(0.544474660054742,54.370358556863,-1.35844749422209));
#46336=CARTESIAN_POINT('Ctrl Pts',(0.595810721550143,54.3673569571994,-1.3378716642764));
#46337=CARTESIAN_POINT('Ctrl Pts',(0.645939360235003,54.3643553575359,-1.31439763967138));
#46338=CARTESIAN_POINT('Ctrl Pts',(0.694523763630163,54.3613537578723,-1.2882037850251));
#46339=CARTESIAN_POINT('Ctrl Pts',(0.743201622252027,54.3583463844386,-1.26195954481364));
#46340=CARTESIAN_POINT('Ctrl Pts',(0.790328859340506,54.355339011005,-1.23298530008649));
#46341=CARTESIAN_POINT('Ctrl Pts',(0.835596091803423,54.3523316375713,-1.20150381662434));
#46342=CARTESIAN_POINT('Ctrl Pts',(0.872356854175208,54.3498893999052,-1.17593823044428));
#46343=CARTESIAN_POINT('Ctrl Pts',(0.907891455234829,54.3474471622392,-1.14872007734812));
#46344=CARTESIAN_POINT('Ctrl Pts',(0.942051250991144,54.3450049245731,-1.11998736176174));
#46345=CARTESIAN_POINT('Ctrl Pts',(0.984129047428765,54.341996593373,-1.08459460455182));
#46346=CARTESIAN_POINT('Ctrl Pts',(1.02429924813557,54.3389882621728,-1.04675178230511));
#46347=CARTESIAN_POINT('Ctrl Pts',(1.06226295109496,54.3359799309727,-1.00669244197571));
#46348=CARTESIAN_POINT('Ctrl Pts',(1.1001584436897,54.3329770049189,-0.966705077296702));
#46349=CARTESIAN_POINT('Ctrl Pts',(1.13585494489424,54.329974078865,-0.92450947809802));
#46350=CARTESIAN_POINT('Ctrl Pts',(1.16908778985078,54.3269711528111,-0.880378321871802));
#46351=CARTESIAN_POINT('Ctrl Pts',(1.20228735781706,54.3239712336723,-0.836291355424049));
#46352=CARTESIAN_POINT('Ctrl Pts',(1.2330278394993,54.3209713145335,-0.790273091355688));
#46353=CARTESIAN_POINT('Ctrl Pts',(1.26108379172199,54.3179713953947,-0.742630406229155));
#46354=CARTESIAN_POINT('Ctrl Pts',(1.28912277146795,54.31497329106,-0.69501654259328));
#46355=CARTESIAN_POINT('Ctrl Pts',(1.31448017255231,54.3119751867253,-0.645780660293874));
#46356=CARTESIAN_POINT('Ctrl Pts',(1.33697430174022,54.3089770823906,-0.595257899138059));
#46357=CARTESIAN_POINT('Ctrl Pts',(1.35946373875826,54.3059796034464,-0.544745676793315));
#46358=CARTESIAN_POINT('Ctrl Pts',(1.37909087479105,54.3029821245022,-0.492947591473747));
#46359=CARTESIAN_POINT('Ctrl Pts',(1.39572137425979,54.299984645558,-0.440220507739433));
#46360=CARTESIAN_POINT('Ctrl Pts',(1.41236725468445,54.2969843943524,-0.387444658605611));
#46361=CARTESIAN_POINT('Ctrl Pts',(1.42601080144522,54.2939841431469,-0.333738599817354));
#46362=CARTESIAN_POINT('Ctrl Pts',(1.43656747646328,54.2909838919413,-0.279474749428162));
#46363=CARTESIAN_POINT('Ctrl Pts',(1.44712889050309,54.2879822938859,-0.225186539326533));
#46364=CARTESIAN_POINT('Ctrl Pts',(1.45460059878481,54.2849806958305,-0.170340563466602));
#46365=CARTESIAN_POINT('Ctrl Pts',(1.45894974156856,54.2819790977751,-0.115316527770419));
#46366=CARTESIAN_POINT('Ctrl Pts',(1.46330725019915,54.2789717259591,-0.060186649916865));
#46367=CARTESIAN_POINT('Ctrl Pts',(1.46453018168205,54.275964354143,-0.00487855816238617));
#46368=CARTESIAN_POINT('Ctrl Pts',(1.46263785624305,54.272956982327,0.0502269995594));
#46369=CARTESIAN_POINT('Ctrl Pts',(1.46110112182314,54.2705147323376,0.0949775512002204));
#46370=CARTESIAN_POINT('Ctrl Pts',(1.45751093409315,54.2680724823483,0.139594440919207));
#46371=CARTESIAN_POINT('Ctrl Pts',(1.45190259880462,54.265630232359,0.183877931205435));
#46372=CARTESIAN_POINT('Ctrl Pts',(1.44499432232729,54.2626218997103,0.238425774467192));
#46373=CARTESIAN_POINT('Ctrl Pts',(1.4349929986005,54.2596135670617,0.292700086311256));
#46374=CARTESIAN_POINT('Ctrl Pts',(1.42193269097772,54.256605234413,0.346323075074201));
#46375=CARTESIAN_POINT('Ctrl Pts',(1.40889584898746,54.2536023068766,0.399849718683207));
#46376=CARTESIAN_POINT('Ctrl Pts',(1.39281105377228,54.2505993793402,0.45272685185352));
#46377=CARTESIAN_POINT('Ctrl Pts',(1.37376381367828,54.2475964518038,0.504584219162773));
#46378=CARTESIAN_POINT('Ctrl Pts',(1.35473564599147,54.2445965311627,0.55638966058566));
#46379=CARTESIAN_POINT('Ctrl Pts',(1.33275109063391,54.2415966105216,0.60717686483264));
#46380=CARTESIAN_POINT('Ctrl Pts',(1.30794566188285,54.2385966898805,0.656589975221846));
#46381=CARTESIAN_POINT('Ctrl Pts',(1.28315523905266,54.2355985840264,0.705973193395472));
#46382=CARTESIAN_POINT('Ctrl Pts',(1.25554756167424,54.2326004781724,0.753983493472151));
#46383=CARTESIAN_POINT('Ctrl Pts',(1.22530561964596,54.2296023723184,0.800286441509554));
#46384=CARTESIAN_POINT('Ctrl Pts',(1.19506998579682,54.2266048918405,0.846579731195973));
#46385=CARTESIAN_POINT('Ctrl Pts',(1.16220146737196,54.2236074113626,0.891165933422689));
#46386=CARTESIAN_POINT('Ctrl Pts',(1.12692699394499,54.2206099308847,0.933738614558757));
#46387=CARTESIAN_POINT('Ctrl Pts',(1.09161989631333,54.2176096781353,0.976350669772697));
#46388=CARTESIAN_POINT('Ctrl Pts',(1.05390273574852,54.2146094253859,1.01694507482582));
#46389=CARTESIAN_POINT('Ctrl Pts',(1.01404252055877,54.2116091726365,1.05524879364954));
#46390=CARTESIAN_POINT('Ctrl Pts',(0.974164411528354,54.2086075730293,1.09356970757968));
#46391=CARTESIAN_POINT('Ctrl Pts',(0.932141732274421,54.205605973422,1.1295975404169));
#46392=CARTESIAN_POINT('Ctrl Pts',(0.888275646213262,54.2026043738148,1.16309871736857));
#46393=CARTESIAN_POINT('Ctrl Pts',(0.844325181142252,54.1995970004532,1.19666433581466));
#46394=CARTESIAN_POINT('Ctrl Pts',(0.798524664186527,54.1965896270917,1.22769329106748));
#46395=CARTESIAN_POINT('Ctrl Pts',(0.751204438885884,54.1935822537301,1.2559952790509));
#46396=CARTESIAN_POINT('Ctrl Pts',(0.712776471366623,54.1911400158683,1.27897885252392));
#46397=CARTESIAN_POINT('Ctrl Pts',(0.67334691764437,54.1886977780066,1.30016485093418));
#46398=CARTESIAN_POINT('Ctrl Pts',(0.63310272398115,54.1862555401448,1.31947458895109));
#46399=CARTESIAN_POINT('Ctrl Pts',(0.583530196150556,54.1832472079272,1.34326019472704));
#46400=CARTESIAN_POINT('Ctrl Pts',(0.532509652540926,54.1802388757095,1.36429898322371));
#46401=CARTESIAN_POINT('Ctrl Pts',(0.480376950062696,54.1772305434919,1.38241463962462));
#46402=CARTESIAN_POINT('Ctrl Pts',(0.428337915222931,54.1742276163916,1.40049774734353));
#46403=CARTESIAN_POINT('Ctrl Pts',(0.375191182263449,54.1712246892913,1.41566797300545));
#46404=CARTESIAN_POINT('Ctrl Pts',(0.321294183042467,54.1682217621909,1.42779630828178));
#46405=CARTESIAN_POINT('Ctrl Pts',(0.26745115209298,54.1652218419887,1.43991249918457));
#46406=CARTESIAN_POINT('Ctrl Pts',(0.212859856349481,54.1622219217865,1.44899271754237));
#46407=CARTESIAN_POINT('Ctrl Pts',(0.157892756878364,54.1592220015843,1.45495777510048));
#46408=CARTESIAN_POINT('Ctrl Pts',(0.102958909522796,54.1562238961712,1.46091922412213));
#46409=CARTESIAN_POINT('Ctrl Pts',(0.0476502337176695,54.1532257907581,
1.46376919029396));
#46410=CARTESIAN_POINT('Ctrl Pts',(-0.00765305361946869,54.150227685345,
1.46347998987697));
#46411=CARTESIAN_POINT('Ctrl Pts',(-0.0629448051966588,54.1472302053093,
1.46319084978455));
#46412=CARTESIAN_POINT('Ctrl Pts',(-0.118230641962594,54.1442327252736,
1.45976384601396));
#46413=CARTESIAN_POINT('Ctrl Pts',(-0.173130034968162,54.1412352452378,
1.45322339679484));
#46414=CARTESIAN_POINT('Ctrl Pts',(-0.22808020266123,54.138234992929,1.44667689852403));
#46415=CARTESIAN_POINT('Ctrl Pts',(-0.282642686123091,54.1352347406201,
1.43701126397151));
#46416=CARTESIAN_POINT('Ctrl Pts',(-0.336443272906292,54.1322344883113,
1.42430269750362));
#46417=CARTESIAN_POINT('Ctrl Pts',(-0.390268011576567,54.1292328891443,
1.41158842597041));
#46418=CARTESIAN_POINT('Ctrl Pts',(-0.443329663792386,54.1262312899774,
1.39582865019909));
#46419=CARTESIAN_POINT('Ctrl Pts',(-0.495268640925472,54.1232296908104,
1.37714967353438));
#46420=CARTESIAN_POINT('Ctrl Pts',(-0.547307525869696,54.1202223178832,
1.35843476671132));
#46421=CARTESIAN_POINT('Ctrl Pts',(-0.598218933261884,54.117214944956,1.33678964809974));
#46422=CARTESIAN_POINT('Ctrl Pts',(-0.647663797226496,54.1142075720288,
1.31238860699191));
#46423=CARTESIAN_POINT('Ctrl Pts',(-0.687817211863172,54.1117653306628,
1.29257289626671));
#46424=CARTESIAN_POINT('Ctrl Pts',(-0.727003801605313,54.1093230892967,
1.27094067101378));
#46425=CARTESIAN_POINT('Ctrl Pts',(-0.765056054817736,54.1068808479306,
1.24760630127726));
#46426=CARTESIAN_POINT('Ctrl Pts',(-0.811928495705812,54.1038725158504,
1.21886322369838));
#46427=CARTESIAN_POINT('Ctrl Pts',(-0.857278827777476,54.1008641837701,
1.18741368394173));
#46428=CARTESIAN_POINT('Ctrl Pts',(-0.900776746638556,54.0978558516899,
1.15344419141771));
#46429=CARTESIAN_POINT('Ctrl Pts',(-0.94419651202103,54.094852924733,1.11953573248052));
#46430=CARTESIAN_POINT('Ctrl Pts',(-0.985770055459424,54.0918499977761,
1.0831166283029));
#46431=CARTESIAN_POINT('Ctrl Pts',(-1.02519511111212,54.0888470708192,1.0444171743857));
#46432=CARTESIAN_POINT('Ctrl Pts',(-1.06458068952564,54.0858471507639,1.00575647114553));
#46433=CARTESIAN_POINT('Ctrl Pts',(-1.10182166599974,54.0828472307087,0.964820309688656));
#46434=CARTESIAN_POINT('Ctrl Pts',(-1.13664947559035,54.0798473106535,0.921878636068854));
#46435=CARTESIAN_POINT('Ctrl Pts',(-1.17145621620474,54.0768492053906,0.878962939882364));
#46436=CARTESIAN_POINT('Ctrl Pts',(-1.20385235072037,54.0738511001278,0.834044545944874));
#46437=CARTESIAN_POINT('Ctrl Pts',(-1.23360837557169,54.070852994865,0.787427854294844));
#46438=CARTESIAN_POINT('Ctrl Pts',(-1.26335819355787,54.0678555149826,0.740820886508129));
#46439=CARTESIAN_POINT('Ctrl Pts',(-1.29046871093687,54.0648580351001,0.692516769945924));
#46440=CARTESIAN_POINT('Ctrl Pts',(-1.31475402529904,54.0618605552177,0.642848429227278));
#46441=CARTESIAN_POINT('Ctrl Pts',(-1.33906180034197,54.0588603030657,0.593134151909713));
#46442=CARTESIAN_POINT('Ctrl Pts',(-1.36053891866768,54.0558600509137,0.542053605584976));
#46443=CARTESIAN_POINT('Ctrl Pts',(-1.37904640930907,54.0528597987617,0.489962499556597));
#46444=CARTESIAN_POINT('Ctrl Pts',(-1.39756220822633,54.0498581997538,0.437848009089597));
#46445=CARTESIAN_POINT('Ctrl Pts',(-1.41310557308966,54.0468566007459,0.384722563097819));
#46446=CARTESIAN_POINT('Ctrl Pts',(-1.42558755326905,54.043855001738,0.33095676147248));
#46447=CARTESIAN_POINT('Ctrl Pts',(-1.43809354329804,54.0408476289715,0.277087538050962));
#46448=CARTESIAN_POINT('Ctrl Pts',(-1.44752629341353,54.0378402562049,0.222576020707));
#46449=CARTESIAN_POINT('Ctrl Pts',(-1.45384829802984,54.0348328834384,0.167801598072695));
#46450=CARTESIAN_POINT('Ctrl Pts',(-1.45898230369712,54.0323906408644,0.123320106315844));
#46451=CARTESIAN_POINT('Ctrl Pts',(-1.46206581984142,54.0299483982904,0.0786654767993697));
#46452=CARTESIAN_POINT('Ctrl Pts',(-1.46310406195348,54.0275061557164,0.0340404743685822));
#46453=CARTESIAN_POINT('Ctrl Pts',(-1.46336637553979,54.0268891190919,0.0227658937181583));
#46454=CARTESIAN_POINT('Ctrl Pts',(-1.46349836980657,54.0262720824674,0.0114882693004367));
#46455=CARTESIAN_POINT('Ctrl Pts',(-1.4634999849931,54.0256550458429,0.000209583410763473));
#46456=CARTESIAN_POINT('Origin',(0.,55.715,0.));
#46457=CARTESIAN_POINT('',(-1.46349946337466,53.4543449820144,0.00125327654337655));
#46458=CARTESIAN_POINT('',(-1.46349952908363,53.5256550458752,0.00117404088105176));
#46459=CARTESIAN_POINT('',(-1.4635,55.715,-1.79227059055215E-16));
#46460=CARTESIAN_POINT('Ctrl Pts',(-1.46349946337466,53.4543449820144,0.00125327654337655));
#46461=CARTESIAN_POINT('Ctrl Pts',(-1.46344247146976,53.457956593816,0.0678049268389159));
#46462=CARTESIAN_POINT('Ctrl Pts',(-1.45884204417911,53.4615682056176,0.134158530349188));
#46463=CARTESIAN_POINT('Ctrl Pts',(-1.44980166704424,53.4651798174191,0.199768306384531));
#46464=CARTESIAN_POINT('Ctrl Pts',(-1.44062889273595,53.4688443216152,0.266338943760728));
#46465=CARTESIAN_POINT('Ctrl Pts',(-1.42688524973019,53.4725088258113,0.332143813274635));
#46466=CARTESIAN_POINT('Ctrl Pts',(-1.40872749801776,53.4761733300074,0.396634701367167));
#46467=CARTESIAN_POINT('Ctrl Pts',(-1.40552582568331,53.4768194750748,0.408006081232914));
#46468=CARTESIAN_POINT('Ctrl Pts',(-1.40218703503298,53.4774656201422,0.419336662599626));
#46469=CARTESIAN_POINT('Ctrl Pts',(-1.39871213746661,53.4781117652096,0.430623509000147));
#46470=CARTESIAN_POINT('Ctrl Pts',(-1.3825336556066,53.4811200974129,0.4831729831241));
#46471=CARTESIAN_POINT('Ctrl Pts',(-1.36335513237752,53.4841284296161,0.534921516347173));
#46472=CARTESIAN_POINT('Ctrl Pts',(-1.34127504032735,53.4871367618194,0.585502789228946));
#46473=CARTESIAN_POINT('Ctrl Pts',(-1.31923461994155,53.4901396889028,0.635993181906195));
#46474=CARTESIAN_POINT('Ctrl Pts',(-1.2943031858894,53.4931426159861,0.685319995328997));
#46475=CARTESIAN_POINT('Ctrl Pts',(-1.2666285956018,53.4961455430694,0.733133173989421));
#46476=CARTESIAN_POINT('Ctrl Pts',(-1.23898171651536,53.4991454632531,0.780898476218864));
#46477=CARTESIAN_POINT('Ctrl Pts',(-1.20859738564374,53.5021453834368,0.827152690447797));
#46478=CARTESIAN_POINT('Ctrl Pts',(-1.17567024846075,53.5051453036205,0.871568538259749));
#46479=CARTESIAN_POINT('Ctrl Pts',(-1.14276303042778,53.5081434090135,0.915957516868622));
#46480=CARTESIAN_POINT('Ctrl Pts',(-1.107316369079,53.5111415144066,0.958509909163623));
#46481=CARTESIAN_POINT('Ctrl Pts',(-1.06956799832171,53.5141396197996,0.99892769856786));
#46482=CARTESIAN_POINT('Ctrl Pts',(-1.03182750154829,53.5171370998138,1.03933705717058));
#46483=CARTESIAN_POINT('Ctrl Pts',(-0.991786609455625,53.520134579828,1.07761231066859));
#46484=CARTESIAN_POINT('Ctrl Pts',(-0.949721530805348,53.5231320598421,
1.11349057648673));
#46485=CARTESIAN_POINT('Ctrl Pts',(-0.907617547543504,53.5261323121273,
1.14940202493617));
#46486=CARTESIAN_POINT('Ctrl Pts',(-0.863486040390983,53.5291325644124,
1.18291171218449));
#46487=CARTESIAN_POINT('Ctrl Pts',(-0.817636962037858,53.5321328166975,
1.21379654321039));
#46488=CARTESIAN_POINT('Ctrl Pts',(-0.771767301367409,53.5351344158395,
1.24469523888562));
#46489=CARTESIAN_POINT('Ctrl Pts',(-0.724178987950642,53.5381360149815,
1.27296645867143));
#46490=CARTESIAN_POINT('Ctrl Pts',(-0.675208840953914,53.5411376141234,
1.29843185077141));
#46491=CARTESIAN_POINT('Ctrl Pts',(-0.626144496900949,53.5441449870239,
1.32394622710197));
#46492=CARTESIAN_POINT('Ctrl Pts',(-0.575693492577419,53.5471523599244,
1.34664377545156));
#46493=CARTESIAN_POINT('Ctrl Pts',(-0.524213958059398,53.5501597328249,
1.36639378517897));
#46494=CARTESIAN_POINT('Ctrl Pts',(-0.482408215485274,53.5526019743579,
1.38243246599126));
#46495=CARTESIAN_POINT('Ctrl Pts',(-0.439924658865493,53.555044215891,1.39652819935841));
#46496=CARTESIAN_POINT('Ctrl Pts',(-0.396960975376122,53.557486457424,1.40863559305749));
#46497=CARTESIAN_POINT('Ctrl Pts',(-0.34403867802658,53.5604947896273,1.42354937691938));
#46498=CARTESIAN_POINT('Ctrl Pts',(-0.290161887486237,53.5635031218305,
1.43550838544453));
#46499=CARTESIAN_POINT('Ctrl Pts',(-0.235691761507292,53.5665114540337,
1.44439663650868));
#46500=CARTESIAN_POINT('Ctrl Pts',(-0.181319502899288,53.569514381117,1.453268917906));
#46501=CARTESIAN_POINT('Ctrl Pts',(-0.126356541991729,53.5725173082003,
1.45908130592402));
#46502=CARTESIAN_POINT('Ctrl Pts',(-0.0711771619183304,53.5755202352836,
1.46176812854202));
#46503=CARTESIAN_POINT('Ctrl Pts',(-0.0160530342221854,53.5785201554673,
1.46445226078299));
#46504=CARTESIAN_POINT('Ctrl Pts',(0.0392865578033683,53.5815200756509,
1.46401700136158));
#46505=CARTESIAN_POINT('Ctrl Pts',(0.0944610859346182,53.5845199958345,
1.46044833980667));
#46506=CARTESIAN_POINT('Ctrl Pts',(0.149602236438777,53.5875181012275,1.45688183710039));
#46507=CARTESIAN_POINT('Ctrl Pts',(0.20457799425863,53.5905162066205,1.4501857230921));
#46508=CARTESIAN_POINT('Ctrl Pts',(0.259009040695779,53.5935143120135,1.44039805846782));
#46509=CARTESIAN_POINT('Ctrl Pts',(0.313428733287042,53.5965117920276,1.43061243546579));
#46510=CARTESIAN_POINT('Ctrl Pts',(0.367303419860547,53.5995092720417,1.41773663582437));
#46511=CARTESIAN_POINT('Ctrl Pts',(0.42026242700844,53.6025067520558,1.40186010088203));
#46512=CARTESIAN_POINT('Ctrl Pts',(0.473270414204989,53.6055070043408,1.38596888225327));
#46513=CARTESIAN_POINT('Ctrl Pts',(0.525360522100424,53.6085072566259,1.36707153528687));
#46514=CARTESIAN_POINT('Ctrl Pts',(0.576177198252906,53.6115075089109,1.3453074318584));
#46515=CARTESIAN_POINT('Ctrl Pts',(0.627016686749469,53.6145091080528,1.32353355820775));
#46516=CARTESIAN_POINT('Ctrl Pts',(0.67658112942205,53.6175107071947,1.29889059847301));
#46517=CARTESIAN_POINT('Ctrl Pts',(0.724537988649745,53.6205123063366,1.27156476555596));
#46518=CARTESIAN_POINT('Ctrl Pts',(0.772587095812953,53.623519679237,1.2441863697373));
#46519=CARTESIAN_POINT('Ctrl Pts',(0.819021996490471,53.6265270521374,1.21411507882206));
#46520=CARTESIAN_POINT('Ctrl Pts',(0.863538615996965,53.6295344250378,1.1815808515214));
#46521=CARTESIAN_POINT('Ctrl Pts',(0.899689881798259,53.6319766665712,1.15516030315487));
#46522=CARTESIAN_POINT('Ctrl Pts',(0.934576570746223,53.6344189081046,1.12711638728839));
#46523=CARTESIAN_POINT('Ctrl Pts',(0.968053314844246,53.6368611496381,1.09759055645494));
#46524=CARTESIAN_POINT('Ctrl Pts',(1.00928968151939,53.6398694818428,1.0612208909023));
#46525=CARTESIAN_POINT('Ctrl Pts',(1.04856152653202,53.6428778140476,1.02244656129843));
#46526=CARTESIAN_POINT('Ctrl Pts',(1.08557550615083,53.6458861462524,0.981508059287019));
#46527=CARTESIAN_POINT('Ctrl Pts',(1.12252298214399,53.6488890733373,0.940643112155147));
#46528=CARTESIAN_POINT('Ctrl Pts',(1.15722029123299,53.6518920004221,0.897622097857804));
#46529=CARTESIAN_POINT('Ctrl Pts',(1.1894092349799,53.654894927507,0.852723825012847));
#46530=CARTESIAN_POINT('Ctrl Pts',(1.22156594720012,53.6578948476922,0.807870509836911));
#46531=CARTESIAN_POINT('Ctrl Pts',(1.25121896263647,53.6608947678774,0.761144087175086));
#46532=CARTESIAN_POINT('Ctrl Pts',(1.27815009566093,53.6638946880625,0.71285663563016));
#46533=CARTESIAN_POINT('Ctrl Pts',(1.3050649367959,53.6668927934571,0.664598395400761));
#46534=CARTESIAN_POINT('Ctrl Pts',(1.32926090181372,53.6698908988516,0.61478145881872));
#46535=CARTESIAN_POINT('Ctrl Pts',(1.35056420572131,53.6728890042462,0.563745134102613));
#46536=CARTESIAN_POINT('Ctrl Pts',(1.37186306594379,53.6758864842619,0.512719455122817));
#46537=CARTESIAN_POINT('Ctrl Pts',(1.3902702594988,53.6788839642775,0.460475380835802));
#46538=CARTESIAN_POINT('Ctrl Pts',(1.40565985543317,53.6818814442932,0.407372827792434));
#46539=CARTESIAN_POINT('Ctrl Pts',(1.42106368469994,53.6848816965798,0.354221161939852));
#46540=CARTESIAN_POINT('Ctrl Pts',(1.43344419239104,53.6878819488664,0.300209940002899));
#46541=CARTESIAN_POINT('Ctrl Pts',(1.44272559606006,53.690882201153,0.245713460097595));
#46542=CARTESIAN_POINT('Ctrl Pts',(1.452011166286,53.6938838002965,0.191192515930983));
#46543=CARTESIAN_POINT('Ctrl Pts',(1.45819479984448,53.6968853994399,0.13618640608039));
#46544=CARTESIAN_POINT('Ctrl Pts',(1.46125254930464,53.6998869985833,0.0810755027778488));
#46545=CARTESIAN_POINT('Ctrl Pts',(1.46431618053183,53.7028943714852,0.0258585903015235));
#46546=CARTESIAN_POINT('Ctrl Pts',(1.46424191570225,53.7059017443871,-0.0294629880018957));
#46547=CARTESIAN_POINT('Ctrl Pts',(1.46105799743672,53.708909117289,-0.0845090416831317));
#46548=CARTESIAN_POINT('Ctrl Pts',(1.45847238612692,53.7113513588101,-0.12921109967839));
#46549=CARTESIAN_POINT('Ctrl Pts',(1.45383703455088,53.7137936003313,-0.173731384701363));
#46550=CARTESIAN_POINT('Ctrl Pts',(1.4471919216604,53.7162358418524,-0.21787104415427));
#46551=CARTESIAN_POINT('Ctrl Pts',(1.43900652848005,53.719244174054,-0.272241898859626));
#46552=CARTESIAN_POINT('Ctrl Pts',(1.42773535304935,53.7222525062556,-0.326266773180041));
#46553=CARTESIAN_POINT('Ctrl Pts',(1.41342130756537,53.7252608384572,-0.379568778115642));
#46554=CARTESIAN_POINT('Ctrl Pts',(1.39913298036218,53.7282637655389,-0.432775014462888));
#46555=CARTESIAN_POINT('Ctrl Pts',(1.38181276825587,53.7312666926206,-0.48526045221439));
#46556=CARTESIAN_POINT('Ctrl Pts',(1.3615548375873,53.7342696197023,-0.536656942788047));
#46557=CARTESIAN_POINT('Ctrl Pts',(1.34131719164868,53.7372695398843,-0.588001968878557));
#46558=CARTESIAN_POINT('Ctrl Pts',(1.31814784685433,53.7402694600663,-0.638259718085283));
#46559=CARTESIAN_POINT('Ctrl Pts',(1.2921906241153,53.7432693802484,-0.687077609115968));
#46560=CARTESIAN_POINT('Ctrl Pts',(1.26624910410221,53.7462674856398,-0.735865967943945));
#46561=CARTESIAN_POINT('Ctrl Pts',(1.23752329643222,53.7492655910312,-0.783215728889403));
#46562=CARTESIAN_POINT('Ctrl Pts',(1.20620398227689,53.7522636964226,-0.828796840690991));
#46563=CARTESIAN_POINT('Ctrl Pts',(1.17489120105964,53.7552611764351,-0.874368444666847));
#46564=CARTESIAN_POINT('Ctrl Pts',(1.14098628685266,53.7582586564477,-0.918171696367938));
#46565=CARTESIAN_POINT('Ctrl Pts',(1.1047232918858,53.7612561364602,-0.959905567420563));
#46566=CARTESIAN_POINT('Ctrl Pts',(1.06842675846383,53.7642563887437,-1.00167803676223));
#46567=CARTESIAN_POINT('Ctrl Pts',(1.02976813429827,53.7672566410273,-1.04137690120061));
#46568=CARTESIAN_POINT('Ctrl Pts',(0.989020756245025,53.7702568933108,-1.07873546048905));
#46569=CARTESIAN_POINT('Ctrl Pts',(0.948255086101592,53.7732584924512,-1.11611079057768));
#46570=CARTESIAN_POINT('Ctrl Pts',(0.905399203044032,53.7762600915916,-1.15114338577598));
#46571=CARTESIAN_POINT('Ctrl Pts',(0.860759664375077,53.779261690732,-1.18360679711841));
#46572=CARTESIAN_POINT('Ctrl Pts',(0.81603425883766,53.7822690636309,-1.2161326538076));
#46573=CARTESIAN_POINT('Ctrl Pts',(0.76951878908108,53.7852764365298,-1.24607916626769));
#46574=CARTESIAN_POINT('Ctrl Pts',(0.72154796991533,53.7882838094288,-1.27326382855678));
#46575=CARTESIAN_POINT('Ctrl Pts',(0.682591601186528,53.7907260509747,-1.29534007712453));
#46576=CARTESIAN_POINT('Ctrl Pts',(0.642676067438844,53.7931682925206,-1.31559575457021));
#46577=CARTESIAN_POINT('Ctrl Pts',(0.601990109420668,53.7956105340664,-1.33395658031275));
#46578=CARTESIAN_POINT('Ctrl Pts',(0.551873495075722,53.7986188662688,-1.35657328808163));
#46579=CARTESIAN_POINT('Ctrl Pts',(0.50037366940323,53.8016271984713,-1.37640998129086));
#46580=CARTESIAN_POINT('Ctrl Pts',(0.447830531129377,53.8046355306737,-1.39329826863755));
#46581=CARTESIAN_POINT('Ctrl Pts',(0.395381797976556,53.8076384577561,-1.41015621252049));
#46582=CARTESIAN_POINT('Ctrl Pts',(0.341893971407634,53.8106413848386,-1.4240761023605));
#46583=CARTESIAN_POINT('Ctrl Pts',(0.287727409941581,53.813644311921,-1.43493734621701));
#46584=CARTESIAN_POINT('Ctrl Pts',(0.233615086694667,53.8166442321038,-1.44578771446117));
#46585=CARTESIAN_POINT('Ctrl Pts',(0.17882589070928,53.8196441522865,-1.4535853998682));
#46586=CARTESIAN_POINT('Ctrl Pts',(0.123734037419925,53.8226440724693,-1.45825996927289));
#46587=CARTESIAN_POINT('Ctrl Pts',(0.0686755117441382,53.8256421778614,
-1.46293171081404));
#46588=CARTESIAN_POINT('Ctrl Pts',(0.0133152175354595,53.8286402832535,
-1.46448403616265));
#46589=CARTESIAN_POINT('Ctrl Pts',(-0.0419660837095952,53.8316383886456,
-1.46289818436489));
#46590=CARTESIAN_POINT('Ctrl Pts',(-0.0972358537526679,53.8346358686588,
-1.46131266336211));
#46591=CARTESIAN_POINT('Ctrl Pts',(-0.152426135183783,53.837633348672,-1.45659028011005));
#46592=CARTESIAN_POINT('Ctrl Pts',(-0.207157076226368,53.8406308286852,
-1.44876436861532));
#46593=CARTESIAN_POINT('Ctrl Pts',(-0.261938636120848,53.8436310809694,
-1.44093121919178));
#46594=CARTESIAN_POINT('Ctrl Pts',(-0.31625948206119,53.8466313332535,-1.42998888134765));
#46595=CARTESIAN_POINT('Ctrl Pts',(-0.369747291296459,53.8496315855377,
-1.41602231288173));
#46596=CARTESIAN_POINT('Ctrl Pts',(-0.423259111986075,53.8526331846786,
-1.40204947462041));
#46597=CARTESIAN_POINT('Ctrl Pts',(-0.475936646207775,53.8556347838196,
-1.38504986202171));
#46598=CARTESIAN_POINT('Ctrl Pts',(-0.52742336570976,53.8586363829606,-1.3651581751956));
#46599=CARTESIAN_POINT('Ctrl Pts',(-0.579009123048124,53.86164375586,-1.34522822550008));
#46600=CARTESIAN_POINT('Ctrl Pts',(-0.629399006339953,53.8646511287595,
-1.32239530631913));
#46601=CARTESIAN_POINT('Ctrl Pts',(-0.67825812959912,53.867658501659,-1.29684160930805));
#46602=CARTESIAN_POINT('Ctrl Pts',(-0.717935876406113,53.8701007431995,
-1.2760898427524));
#46603=CARTESIAN_POINT('Ctrl Pts',(-0.756604471036526,53.8725429847401,
-1.25354473055454));
#46604=CARTESIAN_POINT('Ctrl Pts',(-0.794099129575007,53.8749852262807,
-1.22932453908975));
#46605=CARTESIAN_POINT('Ctrl Pts',(-0.840283151242524,53.8779934557358,
-1.19949133374789));
#46606=CARTESIAN_POINT('Ctrl Pts',(-0.884882167445745,53.881001685191,-1.16698825815757));
#46607=CARTESIAN_POINT('Ctrl Pts',(-0.927570350766358,53.8840099146462,
-1.13200949394392));
#46608=CARTESIAN_POINT('Ctrl Pts',(-0.970181836005141,53.8870127391998,
-1.09709357625854));
#46609=CARTESIAN_POINT('Ctrl Pts',(-1.01088889550785,53.8900155637534,-1.05971112920328));
#46610=CARTESIAN_POINT('Ctrl Pts',(-1.04939475798609,53.893018388307,-1.0200994519709));
#46611=CARTESIAN_POINT('Ctrl Pts',(-1.08786206595882,53.8960182062427,-0.980527436455715));
#46612=CARTESIAN_POINT('Ctrl Pts',(-1.12413217573949,53.8990180241783,-0.93873098934721));
#46613=CARTESIAN_POINT('Ctrl Pts',(-1.15794293658584,53.902017842114,-0.894986260012392));
#46614=CARTESIAN_POINT('Ctrl Pts',(-1.19173324829453,53.9050158457253,-0.851267987993812));
#46615=CARTESIAN_POINT('Ctrl Pts',(-1.22306683623055,53.9080138493365,-0.805604186729965));
#46616=CARTESIAN_POINT('Ctrl Pts',(-1.25172140781955,53.9110118529477,-0.758304534607467));
#46617=CARTESIAN_POINT('Ctrl Pts',(-1.28037000832997,53.9140092318309,-0.711014738850777));
#46618=CARTESIAN_POINT('Ctrl Pts',(-1.30634042704404,53.9170066107141,-0.662090221203661));
#46619=CARTESIAN_POINT('Ctrl Pts',(-1.32945462939384,53.9200039895973,-0.611868154411794));
#46620=CARTESIAN_POINT('Ctrl Pts',(-1.35259021151039,53.923004140943,-0.561599634099379));
#46621=CARTESIAN_POINT('Ctrl Pts',(-1.37286407693083,53.9260042922888,-0.510031648127808));
#46622=CARTESIAN_POINT('Ctrl Pts',(-1.3901456441654,53.9290044436346,-0.457523046422747));
#46623=CARTESIAN_POINT('Ctrl Pts',(-1.40743497500246,53.9320059427737,-0.404990855658612));
#46624=CARTESIAN_POINT('Ctrl Pts',(-1.42172919100888,53.9350074419129,-0.351517718710409));
#46625=CARTESIAN_POINT('Ctrl Pts',(-1.43294806662417,53.9380089410521,-0.297476197968935));
#46626=CARTESIAN_POINT('Ctrl Pts',(-1.44418851681402,53.9410162122552,-0.24333075212318));
#46627=CARTESIAN_POINT('Ctrl Pts',(-1.45234173314682,53.9440234834582,-0.188615263369206));
#46628=CARTESIAN_POINT('Ctrl Pts',(-1.45737912717119,53.9470307546613,-0.133709871309992));
#46629=CARTESIAN_POINT('Ctrl Pts',(-1.46146306265128,53.9494688211507,-0.089196760444808));
#46630=CARTESIAN_POINT('Ctrl Pts',(-1.46350005182781,53.95190688764,-0.0445590499666518));
#46631=CARTESIAN_POINT('Ctrl Pts',(-1.46349999999901,53.9543449541294,1.70220316559402E-6));
#46632=CARTESIAN_POINT('Ctrl Pts',(-1.46349998499324,54.0256550457892,0.000209582428625436));
#46633=CARTESIAN_POINT('Ctrl Pts',(-1.46350782863152,54.0226585901551,-0.054562015460591));
#46634=CARTESIAN_POINT('Ctrl Pts',(-1.46043663080279,54.019662134521,-0.109454800121881));
#46635=CARTESIAN_POINT('Ctrl Pts',(-1.45427163563079,54.0166656788869,-0.164092229553177));
#46636=CARTESIAN_POINT('Ctrl Pts',(-1.44811761703811,54.0136745583475,-0.218632378765915));
#46637=CARTESIAN_POINT('Ctrl Pts',(-1.43888078854372,54.010683437808,-0.272917549034307));
#46638=CARTESIAN_POINT('Ctrl Pts',(-1.42659838444462,54.0076923172686,-0.326572043353398));
#46639=CARTESIAN_POINT('Ctrl Pts',(-1.41432808282349,54.0047041440325,-0.380173669168011));
#46640=CARTESIAN_POINT('Ctrl Pts',(-1.39901826673936,54.0017159707964,-0.433145332152493));
#46641=CARTESIAN_POINT('Ctrl Pts',(-1.38075760625046,53.9987277975603,-0.485119245940098));
#46642=CARTESIAN_POINT('Ctrl Pts',(-1.36250755088441,53.9957413597458,-0.537062975182055));
#46643=CARTESIAN_POINT('Ctrl Pts',(-1.34131022339059,53.9927549219313,-0.588009601014911));
#46644=CARTESIAN_POINT('Ctrl Pts',(-1.31730409443323,53.9897684841168,-0.637606597197248));
#46645=CARTESIAN_POINT('Ctrl Pts',(-1.29330219526639,53.9867825725015,-0.687194854573563));
#46646=CARTESIAN_POINT('Ctrl Pts',(-1.2664927100556,53.9837966608862,-0.735433474673621));
#46647=CARTESIAN_POINT('Ctrl Pts',(-1.23706120277647,53.9808107492709,-0.781992219005559));
#46648=CARTESIAN_POINT('Ctrl Pts',(-1.2076019815707,53.9778220259975,-0.828594804980147));
#46649=CARTESIAN_POINT('Ctrl Pts',(-1.17551609341556,53.9748333027241,-0.873513904364883));
#46650=CARTESIAN_POINT('Ctrl Pts',(-1.14103298148957,53.9718445794507,-0.916447480848212));
#46651=CARTESIAN_POINT('Ctrl Pts',(-1.10653286838508,53.9688543826497,-0.95940222483518));
#46652=CARTESIAN_POINT('Ctrl Pts',(-1.06963353541908,53.9658641858487,-1.00036909962799));
#46653=CARTESIAN_POINT('Ctrl Pts',(-1.03060314573366,53.9628739890477,-1.03908103918987));
#46654=CARTESIAN_POINT('Ctrl Pts',(-0.991500095299347,53.9598782255603,
-1.07786504665939));
#46655=CARTESIAN_POINT('Ctrl Pts',(-0.950258467416528,53.956882462073,-1.11438538372738));
#46656=CARTESIAN_POINT('Ctrl Pts',(-0.907180510680163,53.9538866985856,
-1.14841445961033));
#46657=CARTESIAN_POINT('Ctrl Pts',(-0.879594469150748,53.9519682868911,
-1.17020582511681));
#46658=CARTESIAN_POINT('Ctrl Pts',(-0.851256028304565,53.9500498751967,
-1.19097642150542));
#46659=CARTESIAN_POINT('Ctrl Pts',(-0.822250282559253,53.9481314635023,
-1.21067614283558));
#46660=CARTESIAN_POINT('Ctrl Pts',(-0.776765301853876,53.9451231313024,
-1.24156800310599));
#46661=CARTESIAN_POINT('Ctrl Pts',(-0.729439992864939,53.9421147991026,
-1.26995887430848));
#46662=CARTESIAN_POINT('Ctrl Pts',(-0.680580264189124,53.9391064669027,
-1.29562446488026));
#46663=CARTESIAN_POINT('Ctrl Pts',(-0.631808322587715,53.9361035398226,
-1.32124394166528));
#46664=CARTESIAN_POINT('Ctrl Pts',(-0.581507896484375,53.9331006127424,
-1.34414761068936));
#46665=CARTESIAN_POINT('Ctrl Pts',(-0.530013263328142,53.9300976856623,
-1.36415475320663));
#46666=CARTESIAN_POINT('Ctrl Pts',(-0.478570192925391,53.9270977654817,
-1.38414186211469));
#46667=CARTESIAN_POINT('Ctrl Pts',(-0.425935774579324,53.9240978453011,
-1.40123799899503));
#46668=CARTESIAN_POINT('Ctrl Pts',(-0.372466555339235,53.9210979251205,
-1.41530947681195));
#46669=CARTESIAN_POINT('Ctrl Pts',(-0.3190296821035,53.9180998197304,-1.42937244214095));
#46670=CARTESIAN_POINT('Ctrl Pts',(-0.264759519264145,53.9151017143403,
-1.44041424046975));
#46671=CARTESIAN_POINT('Ctrl Pts',(-0.210027941408102,53.9121036089502,
-1.44835096362307));
#46672=CARTESIAN_POINT('Ctrl Pts',(-0.155307780083542,53.9091061289389,
-1.45628603124492));
#46673=CARTESIAN_POINT('Ctrl Pts',(-0.100126917957422,53.9061086489275,
-1.46111723386381));
#46674=CARTESIAN_POINT('Ctrl Pts',(-0.0448652849060839,53.9031111689161,
-1.46281213975353));
#46675=CARTESIAN_POINT('Ctrl Pts',(0.0104474578217938,53.9001109166336,
-1.46450861320626));
#46676=CARTESIAN_POINT('Ctrl Pts',(0.0658405909274442,53.897110664351,-1.46306297791753));
#46677=CARTESIAN_POINT('Ctrl Pts',(0.120932731060135,53.8941104120684,-1.45849495184534));
#46678=CARTESIAN_POINT('Ctrl Pts',(0.17604960285729,53.8911088129289,-1.45392487511968));
#46679=CARTESIAN_POINT('Ctrl Pts',(0.230864687593562,53.8881072137894,-1.44622968698154));
#46680=CARTESIAN_POINT('Ctrl Pts',(0.285003614276744,53.8851056146498,-1.4354808218326));
#46681=CARTESIAN_POINT('Ctrl Pts',(0.339246680482899,53.8820982417515,-1.42471128058685));
#46682=CARTESIAN_POINT('Ctrl Pts',(0.392810476690926,53.8790908688532,-1.41087645977689));
#46683=CARTESIAN_POINT('Ctrl Pts',(0.445333791806705,53.8760834959549,-1.39409829778071));
#46684=CARTESIAN_POINT('Ctrl Pts',(0.487987173063869,53.8736412543993,-1.38047300891918));
#46685=CARTESIAN_POINT('Ctrl Pts',(0.529954562293615,53.8711990128437,-1.36490764486807));
#46686=CARTESIAN_POINT('Ctrl Pts',(0.57105330475754,53.8687567712881,-1.34749039815707));
#46687=CARTESIAN_POINT('Ctrl Pts',(0.621678383013754,53.8657484390993,-1.32603598313388));
#46688=CARTESIAN_POINT('Ctrl Pts',(0.671200678228524,53.8627401069105,-1.30167887558553));
#46689=CARTESIAN_POINT('Ctrl Pts',(0.719265826454129,53.8597317747218,-1.27455440091636));
#46690=CARTESIAN_POINT('Ctrl Pts',(0.76724461523034,53.8567288476533,-1.24747866124093));
#46691=CARTESIAN_POINT('Ctrl Pts',(0.813770995584772,53.8537259205849,-1.21764567905283));
#46692=CARTESIAN_POINT('Ctrl Pts',(0.858511820184278,53.8507229935165,-1.18523824803449));
#46693=CARTESIAN_POINT('Ctrl Pts',(0.903207844767272,53.847723073348,-1.15286326732207));
#46694=CARTESIAN_POINT('Ctrl Pts',(0.946121428957106,53.8447231531795,-1.11791925269181));
#46695=CARTESIAN_POINT('Ctrl Pts',(0.986946856329365,53.841723233011,-1.08063321843333));
#46696=CARTESIAN_POINT('Ctrl Pts',(1.0277475865069,53.8387251276333,-1.04336974022651));
#46697=CARTESIAN_POINT('Ctrl Pts',(1.06646227372821,53.8357270222557,-1.00376740626566));
#46698=CARTESIAN_POINT('Ctrl Pts',(1.10281870602089,53.832728916878,-0.962093109657488));
#46699=CARTESIAN_POINT('Ctrl Pts',(1.13916755467355,53.8297314368795,-0.920427505950224));
#46700=CARTESIAN_POINT('Ctrl Pts',(1.17315877763142,53.8267339568809,-0.876691196053912));
#46701=CARTESIAN_POINT('Ctrl Pts',(1.20455903829702,53.8237364768823,-0.831185763386839));
#46702=CARTESIAN_POINT('Ctrl Pts',(1.235988340032,53.820736224613,-0.785638244240252));
#46703=CARTESIAN_POINT('Ctrl Pts',(1.26482159042764,53.8177359723437,-0.738318769322307));
#46704=CARTESIAN_POINT('Ctrl Pts',(1.29086847496074,53.8147357200743,-0.689558431427348));
#46705=CARTESIAN_POINT('Ctrl Pts',(1.31692705231761,53.8117341209483,-0.640776204310375));
#46706=CARTESIAN_POINT('Ctrl Pts',(1.34019654748639,53.8087325218223,-0.590552305532093));
#46707=CARTESIAN_POINT('Ctrl Pts',(1.36053389630347,53.8057309226962,-0.539239990179977));
#46708=CARTESIAN_POINT('Ctrl Pts',(1.38091036524808,53.8027235498117,-0.487828972468046));
#46709=CARTESIAN_POINT('Ctrl Pts',(1.39834325257721,53.7997161769272,-0.435325858756278));
#46710=CARTESIAN_POINT('Ctrl Pts',(1.41273906060424,53.7967088040426,-0.382100244233165));
#46711=CARTESIAN_POINT('Ctrl Pts',(1.42442967676295,53.7942665623864,-0.338876534384224));
#46712=CARTESIAN_POINT('Ctrl Pts',(1.43411833936465,53.7918243207301,-0.295176736857024));
#46713=CARTESIAN_POINT('Ctrl Pts',(1.4417800580858,53.7893820790739,-0.251202137940935));
#46714=CARTESIAN_POINT('Ctrl Pts',(1.45121769713886,53.7863737468613,-0.197034606192844));
#46715=CARTESIAN_POINT('Ctrl Pts',(1.45761861003363,53.7833654146488,-0.14221896263965));
#46716=CARTESIAN_POINT('Ctrl Pts',(1.46090425961526,53.7803570824363,-0.0871263119728763));
#46717=CARTESIAN_POINT('Ctrl Pts',(1.46418400581649,53.7773541553435,-0.0321326471735748));
#46718=CARTESIAN_POINT('Ctrl Pts',(1.46435956471138,53.7743512282507,0.0231365135285706));
#46719=CARTESIAN_POINT('Ctrl Pts',(1.46140378568201,53.7713483011579,0.0783021404196221));
#46720=CARTESIAN_POINT('Ctrl Pts',(1.45845096634177,53.7683483809647,0.133412528706947));
#46721=CARTESIAN_POINT('Ctrl Pts',(1.45237304800998,53.7653484607715,0.188419063081002));
#46722=CARTESIAN_POINT('Ctrl Pts',(1.44319490917644,53.7623485405783,0.242941771062965));
#46723=CARTESIAN_POINT('Ctrl Pts',(1.4340223226238,53.7593504351756,0.297431495735774));
#46724=CARTESIAN_POINT('Ctrl Pts',(1.42175332016554,53.756352329773,0.351437453626223));
#46725=CARTESIAN_POINT('Ctrl Pts',(1.40646445646018,53.7533542243703,0.404586187003662));
#46726=CARTESIAN_POINT('Ctrl Pts',(1.39117878187926,53.7503567443464,0.457723834016046));
#46727=CARTESIAN_POINT('Ctrl Pts',(1.37287464291517,53.7473592643226,0.510004103570024));
#46728=CARTESIAN_POINT('Ctrl Pts',(1.35167882500509,53.7443617842987,0.561067379227193));
#46729=CARTESIAN_POINT('Ctrl Pts',(1.33046340377805,53.7413615320039,0.612177881633607));
#46730=CARTESIAN_POINT('Ctrl Pts',(1.30635116309793,53.738361279709,0.662068651624444));
#46731=CARTESIAN_POINT('Ctrl Pts',(1.27951701607627,53.7353610274142,0.710400208031552));
#46732=CARTESIAN_POINT('Ctrl Pts',(1.25267082281594,53.7323594282625,0.758753461176909));
#46733=CARTESIAN_POINT('Ctrl Pts',(1.22310057038838,53.7293578291107,0.805545657443051));
#46734=CARTESIAN_POINT('Ctrl Pts',(1.19102542096925,53.726356229959,0.850464988465146));
#46735=CARTESIAN_POINT('Ctrl Pts',(1.15888857305027,53.7233488570489,0.895470724551247));
#46736=CARTESIAN_POINT('Ctrl Pts',(1.12423753408622,53.7203414841387,0.938595984611326));
#46737=CARTESIAN_POINT('Ctrl Pts',(1.08733208050887,53.7173341112285,0.979561737051965));
#46738=CARTESIAN_POINT('Ctrl Pts',(1.05736172718687,53.7148918697723,1.01282939686202));
#46739=CARTESIAN_POINT('Ctrl Pts',(1.0259054676592,53.712449628316,1.04467348410061));
#46740=CARTESIAN_POINT('Ctrl Pts',(0.993118844906541,53.7100073868598,1.07496381794528));
#46741=CARTESIAN_POINT('Ctrl Pts',(0.952732562551795,53.7069990546575,1.11227519290754));
#46742=CARTESIAN_POINT('Ctrl Pts',(0.910154550746728,53.7039907224552,1.14738700506166));
#46743=CARTESIAN_POINT('Ctrl Pts',(0.865653969298483,53.7009823902529,1.18003197220998));
#46744=CARTESIAN_POINT('Ctrl Pts',(0.821233342776419,53.6979794631706,1.21261828560922));
#46745=CARTESIAN_POINT('Ctrl Pts',(0.774897424288765,53.6949765360882,1.24274623911318));
#46746=CARTESIAN_POINT('Ctrl Pts',(0.726949905745565,53.6919736090058,1.27018742102751));
#46747=CARTESIAN_POINT('Ctrl Pts',(0.679050398150856,53.6889736888231,1.29760112545789));
#46748=CARTESIAN_POINT('Ctrl Pts',(0.629542943692324,53.6859737686404,1.32233312593508));
#46749=CARTESIAN_POINT('Ctrl Pts',(0.57876024920718,53.6829738484577,1.34419820857552));
#46750=CARTESIAN_POINT('Ctrl Pts',(0.528008275525374,53.6799757430656,1.36605006401503));
#46751=CARTESIAN_POINT('Ctrl Pts',(0.475983075522737,53.6769776376736,1.3850382301616));
#46752=CARTESIAN_POINT('Ctrl Pts',(0.423039914520692,53.6739795322815,1.40102443973056));
#46753=CARTESIAN_POINT('Ctrl Pts',(0.370107797004325,53.6709820522683,1.4170073147144));
#46754=CARTESIAN_POINT('Ctrl Pts',(0.316258604698278,53.6679845722551,1.42998932364978));
#46755=CARTESIAN_POINT('Ctrl Pts',(0.261863222396774,53.6649870922418,1.43988190583672));
#46756=CARTESIAN_POINT('Ctrl Pts',(0.207417531589752,53.6619868399577,1.44978363734855));
#46757=CARTESIAN_POINT('Ctrl Pts',(0.15242516295222,53.6589865876735,1.45659013812067));
#46758=CARTESIAN_POINT('Ctrl Pts',(0.0972661924160646,53.6559863353893,
1.46026420137346));
#46759=CARTESIAN_POINT('Ctrl Pts',(0.0420824602165115,53.6529847362482,
1.46393991396664));
#46760=CARTESIAN_POINT('Ctrl Pts',(-0.0132674931339486,53.6499831371072,
1.46448038058406));
#46761=CARTESIAN_POINT('Ctrl Pts',(-0.0684028367148747,53.6469815379662,
1.46190057867468));
#46762=CARTESIAN_POINT('Ctrl Pts',(-0.123644236483194,53.6439741650666,
1.45931581435939));
#46763=CARTESIAN_POINT('Ctrl Pts',(-0.178669674239935,53.640966792167,1.45359884523322));
#46764=CARTESIAN_POINT('Ctrl Pts',(-0.233103823558772,53.6379594192674,
1.44481654802341));
#46765=CARTESIAN_POINT('Ctrl Pts',(-0.277308963770685,53.6355171777268,
1.43768457876514));
#46766=CARTESIAN_POINT('Ctrl Pts',(-0.321124194878841,53.6330749361862,
1.42853210273926));
#46767=CARTESIAN_POINT('Ctrl Pts',(-0.364355779586917,53.6306326946455,
1.41741917437348));
#46768=CARTESIAN_POINT('Ctrl Pts',(-0.417608075171855,53.6276243624437,
1.40373036444101));
#46769=CARTESIAN_POINT('Ctrl Pts',(-0.470201429048979,53.624616030242,1.38700715994846));
#46770=CARTESIAN_POINT('Ctrl Pts',(-0.52176529539383,53.6216076980402,1.36733069391519));
#46771=CARTESIAN_POINT('Ctrl Pts',(-0.573236516091384,53.6186047709584,
1.34768958091227));
#46772=CARTESIAN_POINT('Ctrl Pts',(-0.623681429787296,53.6156018438765,
1.32510592298748));
#46773=CARTESIAN_POINT('Ctrl Pts',(-0.672743413675605,53.6125989167947,
1.29971094838664));
#46774=CARTESIAN_POINT('Ctrl Pts',(-0.721756270675137,53.6095989966126,
1.27434140235581));
#46775=CARTESIAN_POINT('Ctrl Pts',(-0.769388473490375,53.6065990764305,
1.24616635757713));
#46776=CARTESIAN_POINT('Ctrl Pts',(-0.815303950431102,53.6035991562484,
1.21536484991604));
#46777=CARTESIAN_POINT('Ctrl Pts',(-0.861191650973091,53.600601050857,1.18458197551362));
#46778=CARTESIAN_POINT('Ctrl Pts',(-0.905364245588497,53.5976029454656,
1.15117608123266));
#46779=CARTESIAN_POINT('Ctrl Pts',(-0.947512865291517,53.5946048400741,
1.11537062006629));
#46780=CARTESIAN_POINT('Ctrl Pts',(-0.9896526931564,53.5916073600616,1.07957262760996));
#46781=CARTESIAN_POINT('Ctrl Pts',(-1.02976898153332,53.5886098800491,1.04137640431734));
#46782=CARTESIAN_POINT('Ctrl Pts',(-1.06758614681198,53.5856124000365,1.00104548804495));
#46783=CARTESIAN_POINT('Ctrl Pts',(-1.10543828794615,53.5826121477531,0.960677271031219));
#46784=CARTESIAN_POINT('Ctrl Pts',(-1.14098669472224,53.5796118954696,0.91817080286692));
#46785=CARTESIAN_POINT('Ctrl Pts',(-1.17399393983496,53.5766116431861,0.873825199471148));
#46786=CARTESIAN_POINT('Ctrl Pts',(-1.20701600237928,53.5736100440459,0.82945968869011));
#46787=CARTESIAN_POINT('Ctrl Pts',(-1.2374943373654,53.5706084449056,0.78325383910798));
#46788=CARTESIAN_POINT('Ctrl Pts',(-1.26523494747296,53.5676068457653,0.735535707966041));
#46789=CARTESIAN_POINT('Ctrl Pts',(-1.29302891833125,53.5645994728665,0.687725788096614));
#46790=CARTESIAN_POINT('Ctrl Pts',(-1.31807440322412,53.5615920999678,0.638398247899321));
#46791=CARTESIAN_POINT('Ctrl Pts',(-1.34022399085555,53.558584727069,0.587904672829887));
#46792=CARTESIAN_POINT('Ctrl Pts',(-1.3582113322855,53.5561424855231,0.546899612604587));
#46793=CARTESIAN_POINT('Ctrl Pts',(-1.3742897590747,53.5537002439772,0.505126098320758));
#46794=CARTESIAN_POINT('Ctrl Pts',(-1.38840463064804,53.5512580024313,0.46277946323825));
#46795=CARTESIAN_POINT('Ctrl Pts',(-1.4090478451279,53.5476861870038,0.400846864987792));
#46796=CARTESIAN_POINT('Ctrl Pts',(-1.42556244976633,53.5441143715763,0.337473458473622));
#46797=CARTESIAN_POINT('Ctrl Pts',(-1.43777994548423,53.5405425561488,0.273168589635323));
#46798=CARTESIAN_POINT('Ctrl Pts',(-1.44985697291845,53.5370118069753,0.209603053534845));
#46799=CARTESIAN_POINT('Ctrl Pts',(-1.45773505299724,53.5334810578018,0.145127443764852));
#46800=CARTESIAN_POINT('Ctrl Pts',(-1.46129787737112,53.5299503086283,0.0802543680472647));
#46801=CARTESIAN_POINT('Ctrl Pts',(-1.46274263843805,53.5285185543773,0.0539476842892827));
#46802=CARTESIAN_POINT('Ctrl Pts',(-1.46347834914557,53.5270868001262,0.0275758722661284));
#46803=CARTESIAN_POINT('Ctrl Pts',(-1.46349952908363,53.5256550458752,0.00117404088105226));
#46804=CARTESIAN_POINT('Origin',(0.,55.715,0.));
#46805=CARTESIAN_POINT('',(-1.46345008434496,52.9543449205092,-0.000748272696638112));
#46806=CARTESIAN_POINT('',(-1.46349972639677,53.0256550458429,-0.000894894726806227));
#46807=CARTESIAN_POINT('',(-1.4635,55.715,-1.79227059055215E-16));
#46808=CARTESIAN_POINT('Ctrl Pts',(-1.4614949149962,52.9543449541571,-0.000746652183517826));
#46809=CARTESIAN_POINT('Ctrl Pts',(-1.46014398544565,52.9701845067463,0.291491935245273));
#46810=CARTESIAN_POINT('Ctrl Pts',(-1.23353547905525,53.0124822900733,1.07381215251494));
#46811=CARTESIAN_POINT('Ctrl Pts',(0.0411507811327844,53.081238304139,1.72924034556294));
#46812=CARTESIAN_POINT('Ctrl Pts',(1.47504206610459,53.160612996353,0.903446989440327));
#46813=CARTESIAN_POINT('Ctrl Pts',(1.55910697444425,53.2399876885673,-0.749100127985283));
#46814=CARTESIAN_POINT('Ctrl Pts',(0.216416831887046,53.3193623807813,-1.71613790657862));
#46815=CARTESIAN_POINT('Ctrl Pts',(-1.17054009011867,53.3908148026447,-1.17294623829698));
#46816=CARTESIAN_POINT('Ctrl Pts',(-1.4597932078458,53.4358089937699,-0.340099651390323));
#46817=CARTESIAN_POINT('Ctrl Pts',(-1.46257561148105,53.4543449541571,0.00125197239151345));
#46818=CARTESIAN_POINT('Ctrl Pts',(-1.46349952908411,53.5256550458429,0.00117404028541898));
#46819=CARTESIAN_POINT('Ctrl Pts',(-1.46354376834028,53.5226644905813,-0.0539723898429259));
#46820=CARTESIAN_POINT('Ctrl Pts',(-1.46046671848057,53.5196739353198,-0.109161561176566));
#46821=CARTESIAN_POINT('Ctrl Pts',(-1.45428048852627,53.5166833800582,-0.164013751532615));
#46822=CARTESIAN_POINT('Ctrl Pts',(-1.44809574892989,53.5136935452674,-0.218852727152532));
#46823=CARTESIAN_POINT('Ctrl Pts',(-1.43880337509673,53.5107037104765,-0.273354355238613));
#46824=CARTESIAN_POINT('Ctrl Pts',(-1.42646732953524,53.5077138756857,-0.327144016861991));
#46825=CARTESIAN_POINT('Ctrl Pts',(-1.41411960847097,53.504721211153,-0.380984587939385));
#46826=CARTESIAN_POINT('Ctrl Pts',(-1.39872257657072,53.5017285466204,-0.434111326458504));
#46827=CARTESIAN_POINT('Ctrl Pts',(-1.38039106058168,53.4987358820877,-0.486161259116953));
#46828=CARTESIAN_POINT('Ctrl Pts',(-1.36205174102466,53.4957419436036,-0.538233348982043));
#46829=CARTESIAN_POINT('Ctrl Pts',(-1.34077565159835,53.4927480051194,-0.589227227488573));
#46830=CARTESIAN_POINT('Ctrl Pts',(-1.31672591829994,53.4897540666353,-0.638799738632687));
#46831=CARTESIAN_POINT('Ctrl Pts',(-1.29262661862144,53.4867539576589,-0.688474418474416));
#46832=CARTESIAN_POINT('Ctrl Pts',(-1.26574251017182,53.4837538486826,-0.736721410432874));
#46833=CARTESIAN_POINT('Ctrl Pts',(-1.23628238045958,53.4807537397062,-0.783222909372043));
#46834=CARTESIAN_POINT('Ctrl Pts',(-1.20724743479485,53.4777969298765,-0.829053274282686));
#46835=CARTESIAN_POINT('Ctrl Pts',(-1.17571072582716,53.4748401200468,-0.873187873684522));
#46836=CARTESIAN_POINT('Ctrl Pts',(-1.14190992569338,53.4718833102171,-0.915354560595474));
#46837=CARTESIAN_POINT('Ctrl Pts',(-1.1075201470487,53.4688749780139,-0.958256001487645));
#46838=CARTESIAN_POINT('Ctrl Pts',(-1.07063596092685,53.4658666458107,-0.999308203109229));
#46839=CARTESIAN_POINT('Ctrl Pts',(-1.03148379480124,53.4628583136074,-1.03820683443254));
#46840=CARTESIAN_POINT('Ctrl Pts',(-0.992401974016205,53.4598553865241,
-1.07703557594542));
#46841=CARTESIAN_POINT('Ctrl Pts',(-0.951060631611375,53.4568524594408,
-1.11371805588311));
#46842=CARTESIAN_POINT('Ctrl Pts',(-0.907726122749242,53.4538495323575,
-1.14798324729877));
#46843=CARTESIAN_POINT('Ctrl Pts',(-0.864435005723443,53.4508496121739,
-1.1822141281934));
#46844=CARTESIAN_POINT('Ctrl Pts',(-0.819155088302014,53.4478496919903,
-1.21403218870371));
#46845=CARTESIAN_POINT('Ctrl Pts',(-0.772187840886459,53.4448497718067,
-1.24320480548746));
#46846=CARTESIAN_POINT('Ctrl Pts',(-0.725249006133795,53.4418516664137,
-1.27235977440441));
#46847=CARTESIAN_POINT('Ctrl Pts',(-0.676625312742512,53.4388535610207,
-1.29887219284699));
#46848=CARTESIAN_POINT('Ctrl Pts',(-0.62664751905947,53.4358554556277,-1.32255250816616));
#46849=CARTESIAN_POINT('Ctrl Pts',(-0.576680150312218,53.4328579756136,
-1.34622788397624));
#46850=CARTESIAN_POINT('Ctrl Pts',(-0.525359719776652,53.4298604955995,
-1.36707210330548));
#46851=CARTESIAN_POINT('Ctrl Pts',(-0.473039822227728,53.4268630155854,
-1.38494244522535));
#46852=CARTESIAN_POINT('Ctrl Pts',(-0.420671535721616,53.4238627633003,
-1.40282931483832));
#46853=CARTESIAN_POINT('Ctrl Pts',(-0.367302436829406,53.4208625110152,
-1.4177366400966));
#46854=CARTESIAN_POINT('Ctrl Pts',(-0.313302844803723,53.4178622587302,
-1.42957111660732));
#46855=CARTESIAN_POINT('Ctrl Pts',(-0.25927901157679,53.4148606595883,-1.44141090578645));
#46856=CARTESIAN_POINT('Ctrl Pts',(-0.204624644159727,53.4118590604464,
-1.45017501236716));
#46857=CARTESIAN_POINT('Ctrl Pts',(-0.14971856735692,53.4088574613045,-1.45582162389099));
#46858=CARTESIAN_POINT('Ctrl Pts',(-0.0947068753758562,53.4058500884041,
-1.46147909701553));
#46859=CARTESIAN_POINT('Ctrl Pts',(-0.0394430364872446,53.4028427155037,
-1.46400707041701));
#46860=CARTESIAN_POINT('Ctrl Pts',(0.0156918512274061,53.3998353426032,
-1.46341587247271));
#46861=CARTESIAN_POINT('Ctrl Pts',(0.0604660502298152,53.3973931010698,
-1.46293576966476));
#46862=CARTESIAN_POINT('Ctrl Pts',(0.105155090899535,53.3949508595364,-1.46039964528197));
#46863=CARTESIAN_POINT('Ctrl Pts',(0.149558460248952,53.392508618003,-1.45583808061472));
#46864=CARTESIAN_POINT('Ctrl Pts',(0.204254150302647,53.3895002857997,-1.45021918432701));
#46865=CARTESIAN_POINT('Ctrl Pts',(0.25874938857528,53.3864919535964,-1.44150164742992));
#46866=CARTESIAN_POINT('Ctrl Pts',(0.312665684768387,53.3834836213931,-1.42971060693006));
#46867=CARTESIAN_POINT('Ctrl Pts',(0.366485108665576,53.3804806943098,-1.41794075158654));
#46868=CARTESIAN_POINT('Ctrl Pts',(0.41972714227277,53.3774777672264,-1.40310846303509));
#46869=CARTESIAN_POINT('Ctrl Pts',(0.472019615198521,53.374474840143,-1.38529048681778));
#46870=CARTESIAN_POINT('Ctrl Pts',(0.524259726473268,53.3714749199594,-1.36749035214821));
#46871=CARTESIAN_POINT('Ctrl Pts',(0.575551662363499,53.3684749997757,-1.34671062142189));
#46872=CARTESIAN_POINT('Ctrl Pts',(0.625536466939525,53.365475079592,-1.32307837202821));
#46873=CARTESIAN_POINT('Ctrl Pts',(0.67549103339254,53.362476974199,-1.29946041887657));
#46874=CARTESIAN_POINT('Ctrl Pts',(0.724139558553897,53.3594788688059,-1.27299359265179));
#46875=CARTESIAN_POINT('Ctrl Pts',(0.77114338272203,53.3564807634129,-1.2438529387689));
#46876=CARTESIAN_POINT('Ctrl Pts',(0.818137402298552,53.3534832833987,-1.21471836337463));
#46877=CARTESIAN_POINT('Ctrl Pts',(0.863486952817407,53.3504858033846,-1.18291134626145));
#46878=CARTESIAN_POINT('Ctrl Pts',(0.906880330003941,53.3474883233704,-1.14865152115511));
#46879=CARTESIAN_POINT('Ctrl Pts',(0.950313840301762,53.3444880710853,-1.11436001026022));
#46880=CARTESIAN_POINT('Ctrl Pts',(0.99178714630534,53.3414878188002,-1.07761148713108));
#46881=CARTESIAN_POINT('Ctrl Pts',(1.03102098604369,53.3384875665151,-1.03866644132633));
#46882=CARTESIAN_POINT('Ctrl Pts',(1.07027243842259,53.3354859673732,-0.99970391252482));
#46883=CARTESIAN_POINT('Ctrl Pts',(1.10728206611334,53.3324843682312,-0.958543289348735));
#46884=CARTESIAN_POINT('Ctrl Pts',(1.14180925128689,53.3294827690893,-0.915480138329427));
#46885=CARTESIAN_POINT('Ctrl Pts',(1.17640285160107,53.3264753961889,-0.872334152720036));
#46886=CARTESIAN_POINT('Ctrl Pts',(1.20850416171198,53.3234680232884,-0.827278759840527));
#46887=CARTESIAN_POINT('Ctrl Pts',(1.23791513373388,53.320460650388,-0.780639719507421));
#46888=CARTESIAN_POINT('Ctrl Pts',(1.26179933425598,53.3180184088549,-0.742764868222509));
#46889=CARTESIAN_POINT('Ctrl Pts',(1.28391009492697,53.3155761673219,-0.703846279542525));
#46890=CARTESIAN_POINT('Ctrl Pts',(1.30416433960299,53.3131339257888,-0.664068991376574));
#46891=CARTESIAN_POINT('Ctrl Pts',(1.32911334472593,53.3101255935852,-0.615071668489279));
#46892=CARTESIAN_POINT('Ctrl Pts',(1.35135047432382,53.3071172613816,-0.56456190198843));
#46893=CARTESIAN_POINT('Ctrl Pts',(1.37069153569222,53.3041089291779,-0.512871293778182));
#46894=CARTESIAN_POINT('Ctrl Pts',(1.38999784665771,53.3011060020942,-0.46127355893344));
#46895=CARTESIAN_POINT('Ctrl Pts',(1.40641823129796,53.2981030750105,-0.40849968381212));
#46896=CARTESIAN_POINT('Ctrl Pts',(1.41981528099887,53.2951001479268,-0.354903955799443));
#46897=CARTESIAN_POINT('Ctrl Pts',(1.43319891592706,53.2921002277427,-0.301361894416825));
#46898=CARTESIAN_POINT('Ctrl Pts',(1.44356508487175,53.2891003075587,-0.247000120728342));
#46899=CARTESIAN_POINT('Ctrl Pts',(1.45082583068964,53.2861003873746,-0.192189123010937));
#46900=CARTESIAN_POINT('Ctrl Pts',(1.45808218414616,53.2831022819812,-0.137411283004198));
#46901=CARTESIAN_POINT('Ctrl Pts',(1.46223676838547,53.2801041765878,-0.0821852807834841));
#46902=CARTESIAN_POINT('Ctrl Pts',(1.46325293337584,53.2771060711944,-0.0268905739432862));
#46903=CARTESIAN_POINT('Ctrl Pts',(1.46426888640298,53.2741085911799,0.0283925988989668));
#46904=CARTESIAN_POINT('Ctrl Pts',(1.46214771030909,53.2711111111653,0.0837439194122856));
#46905=CARTESIAN_POINT('Ctrl Pts',(1.45690483515211,53.2681136311508,0.138782388329361));
#46906=CARTESIAN_POINT('Ctrl Pts',(1.45165711103186,53.2651133788653,0.193871760521138));
#46907=CARTESIAN_POINT('Ctrl Pts',(1.44328196932721,53.2621131265798,0.248647175308659));
#46908=CARTESIAN_POINT('Ctrl Pts',(1.43184676089073,53.2591128742943,0.3027327258932));
#46909=CARTESIAN_POINT('Ctrl Pts',(1.42040641902306,53.256111275152,0.356842556267067));
#46910=CARTESIAN_POINT('Ctrl Pts',(1.40590341073846,53.2531096760097,0.410261393706924));
#46911=CARTESIAN_POINT('Ctrl Pts',(1.38845551706784,53.2501080768673,0.462626768706566));
#46912=CARTESIAN_POINT('Ctrl Pts',(1.37097406131256,53.2471007039665,0.51509287168989));
#46913=CARTESIAN_POINT('Ctrl Pts',(1.35053659899753,53.2440933310657,0.566500970985331));
#46914=CARTESIAN_POINT('Ctrl Pts',(1.32730936811835,53.2410859581648,0.616507981542214));
#46915=CARTESIAN_POINT('Ctrl Pts',(1.30844688921991,53.2386437166348,0.657117909876322));
#46916=CARTESIAN_POINT('Ctrl Pts',(1.28774558225792,53.2362014751047,0.696804156453991));
#46917=CARTESIAN_POINT('Ctrl Pts',(1.26531583177733,53.2337592335746,0.73539655686823));
#46918=CARTESIAN_POINT('Ctrl Pts',(1.2376870572049,53.2307509013712,0.782934345225549));
#46919=CARTESIAN_POINT('Ctrl Pts',(1.20731664893692,53.2277425691678,0.829014327277459));
#46920=CARTESIAN_POINT('Ctrl Pts',(1.17438326852762,53.2247342369643,0.873301888582852));
#46921=CARTESIAN_POINT('Ctrl Pts',(1.14150906006434,53.2217313098808,0.917509877698758));
#46922=CARTESIAN_POINT('Ctrl Pts',(1.10608133051636,53.2187283827973,0.959931415927525));
#46923=CARTESIAN_POINT('Ctrl Pts',(1.06832317710263,53.2157254557138,1.00025888612166));
#46924=CARTESIAN_POINT('Ctrl Pts',(1.03060283179282,53.21272553553,1.04054597549612));
#46925=CARTESIAN_POINT('Ctrl Pts',(0.990557044489343,53.2097256153462,1.07874276614619));
#46926=CARTESIAN_POINT('Ctrl Pts',(0.94844934733431,53.2067256951623,1.11457439659321));
#46927=CARTESIAN_POINT('Ctrl Pts',(0.906367123075159,53.2037275897691,1.15038435082773));
#46928=CARTESIAN_POINT('Ctrl Pts',(0.862225863030327,53.2007294843759,1.18383163850145));
#46929=CARTESIAN_POINT('Ctrl Pts',(0.816324465664141,53.1977313789828,1.21467963544227));
#46930=CARTESIAN_POINT('Ctrl Pts',(0.7704326429328,53.1947338989684,1.24552119775748));
#46931=CARTESIAN_POINT('Ctrl Pts',(0.722781850590871,53.1917364189541,1.27376425105146));
#46932=CARTESIAN_POINT('Ctrl Pts',(0.673700532821939,53.1887389389398,1.29921508691803));
#46933=CARTESIAN_POINT('Ctrl Pts',(0.624573821351992,53.1857386866545,1.32468946142796));
#46934=CARTESIAN_POINT('Ctrl Pts',(0.574014411452842,53.1827384343693,1.34736621458981));
#46935=CARTESIAN_POINT('Ctrl Pts',(0.522374633333037,53.179738182084,1.36709801859639));
#46936=CARTESIAN_POINT('Ctrl Pts',(0.470711673366742,53.1767365829419,1.38683868049641));
#46937=CARTESIAN_POINT('Ctrl Pts',(0.417967883231469,53.1737349837998,1.40363159699367));
#46938=CARTESIAN_POINT('Ctrl Pts',(0.364511660168443,53.1707333846577,1.4173790952322));
#46939=CARTESIAN_POINT('Ctrl Pts',(0.31095261080908,53.1677260117571,1.43115303761973));
#46940=CARTESIAN_POINT('Ctrl Pts',(0.256678910962631,53.1647186388565,1.4418697555694));
#46941=CARTESIAN_POINT('Ctrl Pts',(0.202068958382688,53.1617112659559,1.44948279950406));
#46942=CARTESIAN_POINT('Ctrl Pts',(0.157721051206288,53.1592690244241,1.45566523603429));
#46943=CARTESIAN_POINT('Ctrl Pts',(0.113151658485708,53.1568267828922,1.45980184246395));
#46944=CARTESIAN_POINT('Ctrl Pts',(0.0685636114066627,53.1543845413604,
1.46189304711079));
#46945=CARTESIAN_POINT('Ctrl Pts',(0.0136404368681237,53.151376209157,1.46446897508563));
#46946=CARTESIAN_POINT('Ctrl Pts',(-0.0415452319520151,53.1483678769535,
1.46395090058842));
#46947=CARTESIAN_POINT('Ctrl Pts',(-0.0966153742922227,53.1453595447501,
1.46030740580549));
#46948=CARTESIAN_POINT('Ctrl Pts',(-0.151586571202367,53.1423566176665,
1.45667045734954));
#46949=CARTESIAN_POINT('Ctrl Pts',(-0.206442130184051,53.139353690583,1.44991926667887));
#46950=CARTESIAN_POINT('Ctrl Pts',(-0.260802606776823,53.1363507634995,
1.44007439054322));
#46951=CARTESIAN_POINT('Ctrl Pts',(-0.315108650979167,53.1333508433156,
1.43023937230755));
#46952=CARTESIAN_POINT('Ctrl Pts',(-0.368920076967387,53.1303509231318,
1.41731689847776));
#46953=CARTESIAN_POINT('Ctrl Pts',(-0.421863024325294,53.1273510029479,
1.40137926297884));
#46954=CARTESIAN_POINT('Ctrl Pts',(-0.47477394404273,53.1243528975547,1.38545126889365));
#46955=CARTESIAN_POINT('Ctrl Pts',(-0.526816920995354,53.1213547921615,
1.36651188028076));
#46956=CARTESIAN_POINT('Ctrl Pts',(-0.57763103332442,53.1183566867683,1.34468384363781));
#46957=CARTESIAN_POINT('Ctrl Pts',(-0.628434546268866,53.1153592067539,
1.32286036013464));
#46958=CARTESIAN_POINT('Ctrl Pts',(-0.678009217880427,53.1123617267396,
1.29814963362067));
#46959=CARTESIAN_POINT('Ctrl Pts',(-0.726014152547299,53.1093642467252,
1.27072251113334));
#46960=CARTESIAN_POINT('Ctrl Pts',(-0.774063485403634,53.1063639944399,
1.24327002220006));
#46961=CARTESIAN_POINT('Ctrl Pts',(-0.820539720261415,53.1033637421546,
1.21309638044427));
#46962=CARTESIAN_POINT('Ctrl Pts',(-0.865127968604045,53.1003634898693,
1.18041765826297));
#46963=CARTESIAN_POINT('Ctrl Pts',(-0.909736233259117,53.0973618907272,
1.14772426612854));
#46964=CARTESIAN_POINT('Ctrl Pts',(-0.952454412876865,53.0943602915851,
1.11252388867989));
#46965=CARTESIAN_POINT('Ctrl Pts',(-0.993000618162861,53.091358692443,1.07507303116029));
#46966=CARTESIAN_POINT('Ctrl Pts',(-1.03362481654068,53.0883513195423,1.03755013463855));
#46967=CARTESIAN_POINT('Ctrl Pts',(-1.07206832522004,53.0853439466417,0.997768490892899));
#46968=CARTESIAN_POINT('Ctrl Pts',(-1.10808686241959,53.0823365737411,0.956020792312128));
#46969=CARTESIAN_POINT('Ctrl Pts',(-1.1373369655372,53.0798943322095,0.922118124870501));
#46970=CARTESIAN_POINT('Ctrl Pts',(-1.16498852794603,53.0774520906778,0.886919639444868));
#46971=CARTESIAN_POINT('Ctrl Pts',(-1.19093188475308,53.0750098491462,0.850595965120026));
#46972=CARTESIAN_POINT('Ctrl Pts',(-1.22317500899146,53.0719745635543,0.805451894028509));
#46973=CARTESIAN_POINT('Ctrl Pts',(-1.25291514808135,53.0689392779623,0.758377611385144));
#46974=CARTESIAN_POINT('Ctrl Pts',(-1.27991741444354,53.0659039923703,0.709678562593066));
#46975=CARTESIAN_POINT('Ctrl Pts',(-1.30687456070399,53.0628737786635,0.661060888675478));
#46976=CARTESIAN_POINT('Ctrl Pts',(-1.33110265731129,53.0598435649568,0.610824279516039));
#46977=CARTESIAN_POINT('Ctrl Pts',(-1.35240949428086,53.05681335125,0.559303861759417));
#46978=CARTESIAN_POINT('Ctrl Pts',(-1.37368565050044,53.0537875008952,0.507857630756016));
#46979=CARTESIAN_POINT('Ctrl Pts',(-1.39204870241039,53.0507616505403,0.455131736075086));
#46980=CARTESIAN_POINT('Ctrl Pts',(-1.40735296774861,53.0477358001855,0.401484587710638));
#46981=CARTESIAN_POINT('Ctrl Pts',(-1.42264437592381,53.0447124918574,0.34788250848977));
#46982=CARTESIAN_POINT('Ctrl Pts',(-1.43488195380794,53.0416891835293,0.293361205924596));
#46983=CARTESIAN_POINT('Ctrl Pts',(-1.44396929253368,53.0386658752012,0.238295892158849));
#46984=CARTESIAN_POINT('Ctrl Pts',(-1.45305339393419,53.0356436439137,0.183250195173629));
#46985=CARTESIAN_POINT('Ctrl Pts',(-1.45898939495832,53.0326214126261,0.127661379838728));
#46986=CARTESIAN_POINT('Ctrl Pts',(-1.46173203743927,53.0295991813386,0.0719145376376866));
#46987=CARTESIAN_POINT('Ctrl Pts',(-1.46292512432683,53.0282844695067,0.047663900919573));
#46988=CARTESIAN_POINT('Ctrl Pts',(-1.46351457201552,53.0269697576748,0.0233834458729815));
#46989=CARTESIAN_POINT('Ctrl Pts',(-1.46349972639677,53.0256550458429,-0.000894894726806227));
#46990=CARTESIAN_POINT('Origin',(0.,55.715,0.));
#46991=CARTESIAN_POINT('',(-1.46349975751718,52.4543449541929,-0.000842464927107473));
#46992=CARTESIAN_POINT('',(-1.46356159323047,52.5256550654528,-0.000674754275529077));
#46993=CARTESIAN_POINT('',(-1.4635,55.715,-1.79227059055215E-16));
#46994=CARTESIAN_POINT('Ctrl Pts',(-1.46349975751718,52.4543449541929,-0.000842464927105523));
#46995=CARTESIAN_POINT('Ctrl Pts',(-1.46353104926595,52.4573145585449,0.053516435090471));
#46996=CARTESIAN_POINT('Ctrl Pts',(-1.46052950171535,52.4602841628968,0.10799664215151));
#46997=CARTESIAN_POINT('Ctrl Pts',(-1.45448095535421,52.4632537672487,0.162226386608034));
#46998=CARTESIAN_POINT('Ctrl Pts',(-1.44844398843846,52.466217686537,0.216352312671336));
#46999=CARTESIAN_POINT('Ctrl Pts',(-1.43937166570992,52.4691816058252,0.270228191471467));
#47000=CARTESIAN_POINT('Ctrl Pts',(-1.427301866151,52.4721455251134,0.323483589818531));
#47001=CARTESIAN_POINT('Ctrl Pts',(-1.41524210424932,52.4751069795052,0.376694699158753));
#47002=CARTESIAN_POINT('Ctrl Pts',(-1.40018991934944,52.478068433897,0.429285821314699));
#47003=CARTESIAN_POINT('Ctrl Pts',(-1.3822345951345,52.4810298882888,0.48089476396959));
#47004=CARTESIAN_POINT('Ctrl Pts',(-1.3642866557656,52.4839901246639,0.532482480380307));
#47005=CARTESIAN_POINT('Ctrl Pts',(-1.34343812148758,52.486950361039,0.583088304963121));
#47006=CARTESIAN_POINT('Ctrl Pts',(-1.31982794369632,52.4899105974141,0.63236575574452));
#47007=CARTESIAN_POINT('Ctrl Pts',(-1.29609678355886,52.4928860025162,0.68189571210479));
#47008=CARTESIAN_POINT('Ctrl Pts',(-1.26957580844062,52.4958614076184,0.73008312987647));
#47009=CARTESIAN_POINT('Ctrl Pts',(-1.24045377280016,52.4988368127205,0.776599438285822));
#47010=CARTESIAN_POINT('Ctrl Pts',(-1.21144935669503,52.5018002006075,0.822927874300251));
#47011=CARTESIAN_POINT('Ctrl Pts',(-1.1798651988766,52.5047635884946,0.867598248163093));
#47012=CARTESIAN_POINT('Ctrl Pts',(-1.14593065596066,52.5077269763816,0.910315979058679));
#47013=CARTESIAN_POINT('Ctrl Pts',(-1.11178969455546,52.5107083900913,0.953293555195093));
#47014=CARTESIAN_POINT('Ctrl Pts',(-1.07527002533709,52.513689803801,0.994294235726321));
#47015=CARTESIAN_POINT('Ctrl Pts',(-1.0366434733955,52.5166712175106,1.03305496420399));
#47016=CARTESIAN_POINT('Ctrl Pts',(-0.998016921453907,52.5196526312203,
1.07181569268167));
#47017=CARTESIAN_POINT('Ctrl Pts',(-0.957283944973365,52.5226340449299,
1.10833615314451));
#47018=CARTESIAN_POINT('Ctrl Pts',(-0.914748300344012,52.5256154586396,
1.14239563944272));
#47019=CARTESIAN_POINT('Ctrl Pts',(-0.871828611231862,52.528623790843,1.1767626409535));
#47020=CARTESIAN_POINT('Ctrl Pts',(-0.826877950761343,52.5316321230465,
1.20878083215128));
#47021=CARTESIAN_POINT('Ctrl Pts',(-0.780183677225224,52.53464045525,1.23820260046219));
#47022=CARTESIAN_POINT('Ctrl Pts',(-0.733573300058009,52.5376433823335,
1.26757150619829));
#47023=CARTESIAN_POINT('Ctrl Pts',(-0.685225970294237,52.540646309417,1.29435296678914));
#47024=CARTESIAN_POINT('Ctrl Pts',(-0.635460747905163,52.5436492365005,
1.31834058113668));
#47025=CARTESIAN_POINT('Ctrl Pts',(-0.585745356573187,52.5466491566844,
1.34230417613653));
#47026=CARTESIAN_POINT('Ctrl Pts',(-0.534615358916831,52.5496490768682,
1.36347923779956));
#47027=CARTESIAN_POINT('Ctrl Pts',(-0.482415707669257,52.5526489970521,
1.38170450350065));
#47028=CARTESIAN_POINT('Ctrl Pts',(-0.430247634407936,52.5556471024453,
1.39991874389455));
#47029=CARTESIAN_POINT('Ctrl Pts',(-0.377011688301272,52.5586452078385,
1.41518655098178));
#47030=CARTESIAN_POINT('Ctrl Pts',(-0.323072009847727,52.5616433132318,
1.42739508421913));
#47031=CARTESIAN_POINT('Ctrl Pts',(-0.269143582744988,52.5646407932461,
1.43960107086196));
#47032=CARTESIAN_POINT('Ctrl Pts',(-0.214512230302412,52.5676382732604,
1.44874893402928));
#47033=CARTESIAN_POINT('Ctrl Pts',(-0.159554164232267,52.5706357532748,
1.45477651846466));
#47034=CARTESIAN_POINT('Ctrl Pts',(-0.104545269249389,52.5736360055601,
1.46080967761517));
#47035=CARTESIAN_POINT('Ctrl Pts',(-0.0492095837828533,52.5766362578454,
1.46371673408402));
#47036=CARTESIAN_POINT('Ctrl Pts',(0.00607113783769222,52.5796365101307,
1.46348740728622));
#47037=CARTESIAN_POINT('Ctrl Pts',(0.0613766757771898,52.5826381092728,
1.4632579775403));
#47038=CARTESIAN_POINT('Ctrl Pts',(0.116626671796092,52.5856397084149,1.45988938996001));
#47039=CARTESIAN_POINT('Ctrl Pts',(0.171442302665545,52.588641307557,1.45342347127626));
#47040=CARTESIAN_POINT('Ctrl Pts',(0.226363374734846,52.5916486804577,1.44694511500467));
#47041=CARTESIAN_POINT('Ctrl Pts',(0.280847890085497,52.5946560533583,1.43735761659836));
#47042=CARTESIAN_POINT('Ctrl Pts',(0.334526180335395,52.5976634262589,1.4247541839455));
#47043=CARTESIAN_POINT('Ctrl Pts',(0.378117498780343,52.6001056677905,1.41451912907113));
#47044=CARTESIAN_POINT('Ctrl Pts',(0.421177233326342,52.6025479093222,1.40229613677227));
#47045=CARTESIAN_POINT('Ctrl Pts',(0.463516369951613,52.6049901508538,1.38815878947146));
#47046=CARTESIAN_POINT('Ctrl Pts',(0.515669355857966,52.6079984830573,1.37074452613733));
#47047=CARTESIAN_POINT('Ctrl Pts',(0.566950816112585,52.6110068152608,1.35034996121041));
#47048=CARTESIAN_POINT('Ctrl Pts',(0.616996857500184,52.6140151474643,1.32708218578764));
#47049=CARTESIAN_POINT('Ctrl Pts',(0.666952980342508,52.6170180745478,1.30385621595947));
#47050=CARTESIAN_POINT('Ctrl Pts',(0.715677613505122,52.6200210016314,1.27776750096769));
#47051=CARTESIAN_POINT('Ctrl Pts',(0.762824288771276,52.623023928715,1.24897211916864));
#47052=CARTESIAN_POINT('Ctrl Pts',(0.809923754991525,52.6260238488989,1.22020557084498));
#47053=CARTESIAN_POINT('Ctrl Pts',(0.855447944005862,52.6290237690828,1.18873799846579));
#47054=CARTESIAN_POINT('Ctrl Pts',(0.899074262649257,52.6320236892667,1.15477171780473));
#47055=CARTESIAN_POINT('Ctrl Pts',(0.94267418971227,52.6350217946599,1.12082598491974));
#47056=CARTESIAN_POINT('Ctrl Pts',(0.98437810538599,52.6380199000532,1.08438486379709));
#47057=CARTESIAN_POINT('Ctrl Pts',(1.02389368717946,52.6410180054464,1.04569305599399));
#47058=CARTESIAN_POINT('Ctrl Pts',(1.06340102636414,52.6440154854608,1.00700931896755));
#47059=CARTESIAN_POINT('Ctrl Pts',(1.10072056033147,52.6470129654752,0.96607619723495));
#47060=CARTESIAN_POINT('Ctrl Pts',(1.13559599889987,52.6500104454896,0.923176027246491));
#47061=CARTESIAN_POINT('Ctrl Pts',(1.17050369261746,52.6530106977749,0.880236180297959));
#47062=CARTESIAN_POINT('Ctrl Pts',(1.2029624399759,52.6560109500603,0.835326061356269));
#47063=CARTESIAN_POINT('Ctrl Pts',(1.23275652369796,52.6590112023456,0.788760802322296));
#47064=CARTESIAN_POINT('Ctrl Pts',(1.26256398241702,52.6620128014878,0.742174639467111));
#47065=CARTESIAN_POINT('Ctrl Pts',(1.28970413303551,52.66501440063,0.693932317105381));
#47066=CARTESIAN_POINT('Ctrl Pts',(1.31400662314741,52.6680159997721,0.644374770087052));
#47067=CARTESIAN_POINT('Ctrl Pts',(1.33835586057712,52.6710233726728,0.594721896112934));
#47068=CARTESIAN_POINT('Ctrl Pts',(1.35985632634852,52.6740307455735,0.543749231768453));
#47069=CARTESIAN_POINT('Ctrl Pts',(1.37838579892566,52.6770381184742,0.491817892435872));
#47070=CARTESIAN_POINT('Ctrl Pts',(1.39343330017515,52.6794803600054,0.449645246115749));
#47071=CARTESIAN_POINT('Ctrl Pts',(1.4065223972658,52.6819226015367,0.406840832596735));
#47072=CARTESIAN_POINT('Ctrl Pts',(1.41761237649152,52.684364843068,0.363603355344911));
#47073=CARTESIAN_POINT('Ctrl Pts',(1.43127291792989,52.6873731752715,0.310343801141272));
#47074=CARTESIAN_POINT('Ctrl Pts',(1.44195697891875,52.6903815074749,0.256199759131709));
#47075=CARTESIAN_POINT('Ctrl Pts',(1.44955713379634,52.6933898396784,0.201535023904365));
#47076=CARTESIAN_POINT('Ctrl Pts',(1.45714363335072,52.6963927667619,0.146968505705502));
#47077=CARTESIAN_POINT('Ctrl Pts',(1.46165714999721,52.6993956938455,0.0918836702770846));
#47078=CARTESIAN_POINT('Ctrl Pts',(1.46304086395174,52.702398620929,0.036656246498318));
#47079=CARTESIAN_POINT('Ctrl Pts',(1.4644231923618,52.7053985411129,-0.018515876795996));
#47080=CARTESIAN_POINT('Ctrl Pts',(1.46268191263403,52.7083984612968,-0.0738297795846173));
#47081=CARTESIAN_POINT('Ctrl Pts',(1.45781199954093,52.7113983814806,-0.128904708969369));
#47082=CARTESIAN_POINT('Ctrl Pts',(1.45294503248377,52.7143964868739,-0.183946320978928));
#47083=CARTESIAN_POINT('Ctrl Pts',(1.44495322959695,52.7173945922671,-0.238748720358541));
#47084=CARTESIAN_POINT('Ctrl Pts',(1.43388359375688,52.7203926976603,-0.292933592397393));
#47085=CARTESIAN_POINT('Ctrl Pts',(1.42281626694719,52.7233901776747,-0.347107161940224));
#47086=CARTESIAN_POINT('Ctrl Pts',(1.40867248773217,52.726387657689,-0.400662942018325));
#47087=CARTESIAN_POINT('Ctrl Pts',(1.3915504212787,52.7293851377034,-0.453232473504558));
#47088=CARTESIAN_POINT('Ctrl Pts',(1.37441251918756,52.7323853899887,-0.505850624826231));
#47089=CARTESIAN_POINT('Ctrl Pts',(1.35429099024574,52.735385642274,-0.557480201005298));
#47090=CARTESIAN_POINT('Ctrl Pts',(1.33133355935835,52.7383858945593,-0.607769038143786));
#47091=CARTESIAN_POINT('Ctrl Pts',(1.30836582254677,52.7413874937014,-0.658080450671743));
#47092=CARTESIAN_POINT('Ctrl Pts',(1.2825598929126,52.7443890928436,-0.707049455543295));
#47093=CARTESIAN_POINT('Ctrl Pts',(1.25410978013588,52.7473906919857,-0.754348002825965));
#47094=CARTESIAN_POINT('Ctrl Pts',(1.2256049418369,52.7503980648863,-0.801737531741041));
#47095=CARTESIAN_POINT('Ctrl Pts',(1.19444605759191,52.753405437787,-0.847449745331225));
#47096=CARTESIAN_POINT('Ctrl Pts',(1.16087019891324,52.7564128106876,-0.89118608117224));
#47097=CARTESIAN_POINT('Ctrl Pts',(1.13360375766034,52.7588550522191,-0.926703690512898));
#47098=CARTESIAN_POINT('Ctrl Pts',(1.10474424805654,52.7612972937506,-0.960918760075315));
#47099=CARTESIAN_POINT('Ctrl Pts',(1.07443651424841,52.7637395352821,-0.993689300963699));
#47100=CARTESIAN_POINT('Ctrl Pts',(1.03710370729502,52.7667478674856,-1.03405577258739));
#47101=CARTESIAN_POINT('Ctrl Pts',(0.997413273392782,52.7697561996891,-1.07240151421543));
#47102=CARTESIAN_POINT('Ctrl Pts',(0.955612560776801,52.7727645318925,-1.10843893998975));
#47103=CARTESIAN_POINT('Ctrl Pts',(0.913886952188335,52.7757674589761,-1.14441161672877));
#47104=CARTESIAN_POINT('Ctrl Pts',(0.87005898616825,52.7787703860596,-1.17808386526148));
#47105=CARTESIAN_POINT('Ctrl Pts',(0.824413487742079,52.7817733131432,-1.20920413960131));
#47106=CARTESIAN_POINT('Ctrl Pts',(0.778813695199047,52.7847732333271,-1.24029325249759));
#47107=CARTESIAN_POINT('Ctrl Pts',(0.731400409966574,52.7877731535109,-1.26883515643326));
#47108=CARTESIAN_POINT('Ctrl Pts',(0.682490773392749,52.7907730736948,-1.29461909233325));
#47109=CARTESIAN_POINT('Ctrl Pts',(0.633610724522977,52.793771179088,-1.32038743033642));
#47110=CARTESIAN_POINT('Ctrl Pts',(0.583236585237063,52.7967692844813,-1.34340086081427));
#47111=CARTESIAN_POINT('Ctrl Pts',(0.531711670956427,52.7997673898745,-1.36349365563934));
#47112=CARTESIAN_POINT('Ctrl Pts',(0.480197504327599,52.8027648698889,-1.38358225928106));
#47113=CARTESIAN_POINT('Ctrl Pts',(0.427533531783183,52.8057623499032,-1.40075124486874));
#47114=CARTESIAN_POINT('Ctrl Pts',(0.374082541870647,52.8087598299176,-1.41488321138799));
#47115=CARTESIAN_POINT('Ctrl Pts',(0.320582116890717,52.8117600822029,-1.42902824809955));
#47116=CARTESIAN_POINT('Ctrl Pts',(0.266293732613245,52.8147603344882,-1.44013051795475));
#47117=CARTESIAN_POINT('Ctrl Pts',(0.211593371524531,52.8177605867735,-1.44812309391394));
#47118=CARTESIAN_POINT('Ctrl Pts',(0.15686845464912,52.8207621859156,-1.45611925785659));
#47119=CARTESIAN_POINT('Ctrl Pts',(0.101731720078069,52.8237637850578,-1.46100289822506));
#47120=CARTESIAN_POINT('Ctrl Pts',(0.046563999296092,52.8267653841999,-1.46275905191852));
#47121=CARTESIAN_POINT('Ctrl Pts',(-0.00870983995210641,52.8297727571006,
-1.46451858368041));
#47122=CARTESIAN_POINT('Ctrl Pts',(-0.0640142543121039,52.8327801300012,
-1.46313862316723));
#47123=CARTESIAN_POINT('Ctrl Pts',(-0.118969825836467,52.8357875029019,
-1.45865637850058));
#47124=CARTESIAN_POINT('Ctrl Pts',(-0.163598404864021,52.8382297444333,
-1.45501641616779));
#47125=CARTESIAN_POINT('Ctrl Pts',(-0.207996882973535,52.8406719859648,
-1.44933157481369));
#47126=CARTESIAN_POINT('Ctrl Pts',(-0.251967406554764,52.8431142274963,
-1.44164651563206));
#47127=CARTESIAN_POINT('Ctrl Pts',(-0.30612992094532,52.8461225596997,-1.4321801255458));
#47128=CARTESIAN_POINT('Ctrl Pts',(-0.35987371977749,52.8491308919032,-1.41963697875378));
#47129=CARTESIAN_POINT('Ctrl Pts',(-0.412823031868646,52.8521392241067,
-1.40406887094572));
#47130=CARTESIAN_POINT('Ctrl Pts',(-0.465677209060325,52.8551421511902,
-1.38852873461288));
#47131=CARTESIAN_POINT('Ctrl Pts',(-0.517739228997993,52.8581450782738,
-1.36997457047864));
#47132=CARTESIAN_POINT('Ctrl Pts',(-0.568643268197576,52.8611480053573,
-1.34850920780452));
#47133=CARTESIAN_POINT('Ctrl Pts',(-0.619496336016655,52.8641479255412,
-1.32706533888976));
#47134=CARTESIAN_POINT('Ctrl Pts',(-0.669193235005333,52.8671478457251,
-1.30271625004196));
#47135=CARTESIAN_POINT('Ctrl Pts',(-0.717384876594728,52.870147765909,-1.2756140438366));
#47136=CARTESIAN_POINT('Ctrl Pts',(-0.765547364828624,52.8731458713022,
-1.24852823301074));
#47137=CARTESIAN_POINT('Ctrl Pts',(-0.812205940344729,52.8761439766955,
-1.21869286436914));
#47138=CARTESIAN_POINT('Ctrl Pts',(-0.8570351466989,52.8791420820887,-1.18630645590538));
#47139=CARTESIAN_POINT('Ctrl Pts',(-0.901855002067964,52.8821395621031,
-1.15392680296661));
#47140=CARTESIAN_POINT('Ctrl Pts',(-0.944845817479181,52.8851370421174,
-1.11899747631191));
#47141=CARTESIAN_POINT('Ctrl Pts',(-0.985712172587482,52.8881345221318,
-1.0817595679322));
#47142=CARTESIAN_POINT('Ctrl Pts',(-1.02661632364724,52.8911347744171,-1.0444872194324));
#47143=CARTESIAN_POINT('Ctrl Pts',(-1.06539169668125,52.8941350267024,-1.00490238004313));
#47144=CARTESIAN_POINT('Ctrl Pts',(-1.10177811711606,52.8971352789877,-0.963284605214991));
#47145=CARTESIAN_POINT('Ctrl Pts',(-1.13818087194359,52.9001368781299,-0.921648147563138));
#47146=CARTESIAN_POINT('Ctrl Pts',(-1.17219221067203,52.903138477272,-0.877977353199902));
#47147=CARTESIAN_POINT('Ctrl Pts',(-1.203592982875,52.9061400764142,-0.83258403874568));
#47148=CARTESIAN_POINT('Ctrl Pts',(-1.23505415637306,52.9091474493148,-0.787103407490333));
#47149=CARTESIAN_POINT('Ctrl Pts',(-1.26389445454505,52.9121548222155,-0.739894089129721));
#47150=CARTESIAN_POINT('Ctrl Pts',(-1.28993932232875,52.9151621951162,-0.691295012791242));
#47151=CARTESIAN_POINT('Ctrl Pts',(-1.31108996107004,52.9176044366476,-0.651828446274866));
#47152=CARTESIAN_POINT('Ctrl Pts',(-1.33039789737408,52.920046678179,-0.611445951610777));
#47153=CARTESIAN_POINT('Ctrl Pts',(-1.3477933260689,52.9224889197105,-0.57033797015815));
#47154=CARTESIAN_POINT('Ctrl Pts',(-1.37157131759644,52.9258272449372,-0.514147044838465));
#47155=CARTESIAN_POINT('Ctrl Pts',(-1.39186134356342,52.929165570164,-0.456396611155354));
#47156=CARTESIAN_POINT('Ctrl Pts',(-1.40848026768949,52.9325038953908,-0.397511742630756));
#47157=CARTESIAN_POINT('Ctrl Pts',(-1.4250404108123,52.9358304129877,-0.338835149420643));
#47158=CARTESIAN_POINT('Ctrl Pts',(-1.43795520456422,52.9391569305845,-0.279032416728898));
#47159=CARTESIAN_POINT('Ctrl Pts',(-1.44709009425181,52.9424834481814,-0.218546354621345));
#47160=CARTESIAN_POINT('Ctrl Pts',(-1.45617431336866,52.9457915138263,-0.158395804314613));
#47161=CARTESIAN_POINT('Ctrl Pts',(-1.46152030885999,52.9490995794712,-0.0975697894002547));
#47162=CARTESIAN_POINT('Ctrl Pts',(-1.46304423604721,52.9524076451162,-0.0365214097352111));
#47163=CARTESIAN_POINT('Ctrl Pts',(-1.46334171758207,52.9530534032953,-0.0246043274519001));
#47164=CARTESIAN_POINT('Ctrl Pts',(-1.46349370840455,52.9536991614744,-0.0126788176551808));
#47165=CARTESIAN_POINT('Ctrl Pts',(-1.4634998086868,52.9543449196535,-0.000748313909921448));
#47166=CARTESIAN_POINT('Ctrl Pts',(-1.46168684698443,53.0256544778977,-0.000904261258610456));
#47167=CARTESIAN_POINT('Ctrl Pts',(-1.4627153019643,53.0156480375759,-0.185461603358528));
#47168=CARTESIAN_POINT('Ctrl Pts',(-1.34465214268998,52.9791833665158,-0.856740950372973));
#47169=CARTESIAN_POINT('Ctrl Pts',(-0.337036094537274,52.9162604647181,
-1.69657654331278));
#47170=CARTESIAN_POINT('Ctrl Pts',(1.24245598610379,52.8368857725037,-1.20344024319159));
#47171=CARTESIAN_POINT('Ctrl Pts',(1.6849636373595,52.7575110802896,0.390976773113176));
#47172=CARTESIAN_POINT('Ctrl Pts',(0.58554349303632,52.6781363880753,1.62760686718302));
#47173=CARTESIAN_POINT('Ctrl Pts',(-1.00666498239691,52.600851258045,1.38145223997477));
#47174=CARTESIAN_POINT('Ctrl Pts',(-1.46296296025439,52.5500243587529,0.445771649118409));
#47175=CARTESIAN_POINT('Ctrl Pts',(-1.46552883361008,52.5256556901986,-0.000664216367255248));
#47176=CARTESIAN_POINT('Origin',(0.,55.715,0.));
#47177=CARTESIAN_POINT('',(-1.4634994347896,51.9543449541571,0.00128622335730389));
#47178=CARTESIAN_POINT('',(-1.4634993993698,52.025655045799,0.00132591260086994));
#47179=CARTESIAN_POINT('',(-1.4635,55.715,-1.79227059055215E-16));
#47180=CARTESIAN_POINT('Ctrl Pts',(-1.4634994347896,51.9543449541571,0.00128622335730389));
#47181=CARTESIAN_POINT('Ctrl Pts',(-1.46342941742781,51.9586837643365,0.0809538555928721));
#47182=CARTESIAN_POINT('Ctrl Pts',(-1.45685072552131,51.9630225745159,0.160344782218165));
#47183=CARTESIAN_POINT('Ctrl Pts',(-1.44391791303884,51.9673613846953,0.238607020863936));
#47184=CARTESIAN_POINT('Ctrl Pts',(-1.44130358770758,51.9682384608437,0.254427473936301));
#47185=CARTESIAN_POINT('Ctrl Pts',(-1.43842975380386,51.969115536992,0.27020190040974));
#47186=CARTESIAN_POINT('Ctrl Pts',(-1.43529790189955,51.9699926131404,0.285923386246649));
#47187=CARTESIAN_POINT('Ctrl Pts',(-1.42455578908048,51.9730009453427,0.339847383837681));
#47188=CARTESIAN_POINT('Ctrl Pts',(-1.41074765930891,51.976009277545,0.393280163984652));
#47189=CARTESIAN_POINT('Ctrl Pts',(-1.39393416290903,51.9790176097473,0.445847282682202));
#47190=CARTESIAN_POINT('Ctrl Pts',(-1.3771508755945,51.9820205368297,0.498319953173532));
#47191=CARTESIAN_POINT('Ctrl Pts',(-1.35737309683935,51.9850234639121,0.5499295491025));
#47192=CARTESIAN_POINT('Ctrl Pts',(-1.33471226153445,51.9880263909945,0.600312775900695));
#47193=CARTESIAN_POINT('Ctrl Pts',(-1.31207411704297,51.9910263111772,0.650645552819918));
#47194=CARTESIAN_POINT('Ctrl Pts',(-1.2865588501779,51.9940262313599,0.699753913120156));
#47195=CARTESIAN_POINT('Ctrl Pts',(-1.25832676043541,51.9970261515426,0.747292455449752));
#47196=CARTESIAN_POINT('Ctrl Pts',(-1.23011174959128,52.0000242569346,0.794802239513849));
#47197=CARTESIAN_POINT('Ctrl Pts',(-1.19918344268237,52.0030223623267,0.840743633927565));
#47198=CARTESIAN_POINT('Ctrl Pts',(-1.16574798392042,52.0060204677188,0.884795958391238));
#47199=CARTESIAN_POINT('Ctrl Pts',(-1.13231949950606,52.009017947732,0.928839093920941));
#47200=CARTESIAN_POINT('Ctrl Pts',(-1.09638522119433,52.0120154277452,0.970993520856203));
#47201=CARTESIAN_POINT('Ctrl Pts',(-1.05819314641334,52.0150129077584,1.01096959147337));
#47202=CARTESIAN_POINT('Ctrl Pts',(-1.01996574903474,52.0180131600426,1.0509826346474));
#47203=CARTESIAN_POINT('Ctrl Pts',(-0.979476749019557,52.0210134123268,
1.08881291271801));
#47204=CARTESIAN_POINT('Ctrl Pts',(-0.937011764659512,52.0240136646109,
1.12420692174069));
#47205=CARTESIAN_POINT('Ctrl Pts',(-0.894527717150933,52.0270152637519,
1.15961681964832));
#47206=CARTESIAN_POINT('Ctrl Pts',(-0.850066342559578,52.030016862893,1.19258795262113));
#47207=CARTESIAN_POINT('Ctrl Pts',(-0.803944543095699,52.033018462034,1.22290859087123));
#47208=CARTESIAN_POINT('Ctrl Pts',(-0.757734025544826,52.0360258349336,
1.25328755271349));
#47209=CARTESIAN_POINT('Ctrl Pts',(-0.709857161136456,52.0390332078331,
1.28100556834841));
#47210=CARTESIAN_POINT('Ctrl Pts',(-0.660656904481931,52.0420405807327,
1.30589613084669));
#47211=CARTESIAN_POINT('Ctrl Pts',(-0.62070212846228,52.0444828222733,1.32610937600524));
#47212=CARTESIAN_POINT('Ctrl Pts',(-0.579875171453695,52.0469250638139,
1.34445881403067));
#47213=CARTESIAN_POINT('Ctrl Pts',(-0.538368069328275,52.0493673053545,
1.36087915404996));
#47214=CARTESIAN_POINT('Ctrl Pts',(-0.487239976610686,52.0523756375563,
1.38110558817741));
#47215=CARTESIAN_POINT('Ctrl Pts',(-0.434861406560966,52.0553839697581,
1.39848982932012));
#47216=CARTESIAN_POINT('Ctrl Pts',(-0.381579825840558,52.0583923019598,
1.41287971409865));
#47217=CARTESIAN_POINT('Ctrl Pts',(-0.328393977013189,52.0613952290417,
1.42724374433436));
#47218=CARTESIAN_POINT('Ctrl Pts',(-0.27430884348231,52.0643981561235,1.43862395760165));
#47219=CARTESIAN_POINT('Ctrl Pts',(-0.219690073186104,52.0674010832053,
1.44691690215557));
#47220=CARTESIAN_POINT('Ctrl Pts',(-0.16512599391629,52.0704010033874,1.45520154279407));
#47221=CARTESIAN_POINT('Ctrl Pts',(-0.11002985655561,52.0734009235695,1.46040495909979));
#47222=CARTESIAN_POINT('Ctrl Pts',(-0.0547787834541315,52.0764008437516,
1.46247445614728));
#47223=CARTESIAN_POINT('Ctrl Pts',(0.000438865714139876,52.079398949143,
1.46454270126016));
#47224=CARTESIAN_POINT('Ctrl Pts',(0.055810737441721,52.0823970545345,1.46348076474494));
#47225=CARTESIAN_POINT('Ctrl Pts',(0.110955609096121,52.0853951599259,1.45928787523576));
#47226=CARTESIAN_POINT('Ctrl Pts',(0.166088978006442,52.0883926399384,1.45509586032714));
#47227=CARTESIAN_POINT('Ctrl Pts',(0.220994913799366,52.091390119951,1.44777422924706));
#47228=CARTESIAN_POINT('Ctrl Pts',(0.275295560985323,52.0943875999635,1.43737420461819));
#47229=CARTESIAN_POINT('Ctrl Pts',(0.32964642905838,52.097387852247,1.42696456134775));
#47230=CARTESIAN_POINT('Ctrl Pts',(0.383390369377223,52.1003881045305,1.41347093547737));
#47231=CARTESIAN_POINT('Ctrl Pts',(0.43615948329097,52.1033883568139,1.39699576060035));
#47232=CARTESIAN_POINT('Ctrl Pts',(0.48895228602622,52.1063899559542,1.38051318977809));
#47233=CARTESIAN_POINT('Ctrl Pts',(0.540768893944325,52.1093915550945,1.36104658804578));
#47234=CARTESIAN_POINT('Ctrl Pts',(0.59125953270791,52.1123931542348,1.33874733052284));
#47235=CARTESIAN_POINT('Ctrl Pts',(0.641847293285998,52.1154005271336,1.31640517902181));
#47236=CARTESIAN_POINT('Ctrl Pts',(0.691103516856547,52.1184079000324,1.29121972736791));
#47237=CARTESIAN_POINT('Ctrl Pts',(0.738702288430127,52.1214152729312,1.26338876798399));
#47238=CARTESIAN_POINT('Ctrl Pts',(0.777356522999696,52.123857514477,1.24078767142713));
#47239=CARTESIAN_POINT('Ctrl Pts',(0.814918099146787,52.1262997560229,1.21644285060387));
#47240=CARTESIAN_POINT('Ctrl Pts',(0.851227997708145,52.1287419975687,1.19048021651676));
#47241=CARTESIAN_POINT('Ctrl Pts',(0.895954219558794,52.1317503297734,1.15849966636333));
#47242=CARTESIAN_POINT('Ctrl Pts',(0.938971054269809,52.1347586619781,1.12392686811807));
#47243=CARTESIAN_POINT('Ctrl Pts',(0.979962189207295,52.1377669941828,1.08697118532372));
#47244=CARTESIAN_POINT('Ctrl Pts',(1.02087967469914,52.1407699212677,1.05008190141183));
#47245=CARTESIAN_POINT('Ctrl Pts',(1.05977829334223,52.1437728483525,1.01081858014419));
#47246=CARTESIAN_POINT('Ctrl Pts',(1.09637279239192,52.1467757754373,0.96943228237084));
#47247=CARTESIAN_POINT('Ctrl Pts',(1.13293064853169,52.1497756956224,0.928087425645212));
#47248=CARTESIAN_POINT('Ctrl Pts',(1.16718860656678,52.1527756158076,0.884624197387474));
#47249=CARTESIAN_POINT('Ctrl Pts',(1.19889782988811,52.1557755359927,0.839330830775079));
#47250=CARTESIAN_POINT('Ctrl Pts',(1.23058787083203,52.1587736413873,0.794064864217351));
#47251=CARTESIAN_POINT('Ctrl Pts',(1.25973193015169,52.1617717467818,0.74697138590056));
#47252=CARTESIAN_POINT('Ctrl Pts',(1.28612256760004,52.1647698521763,0.698370239278483));
#47253=CARTESIAN_POINT('Ctrl Pts',(1.3125077001896,52.167767332192,0.649779230435358));
#47254=CARTESIAN_POINT('Ctrl Pts',(1.33614029905837,52.1707648122077,0.599681642236049));
#47255=CARTESIAN_POINT('Ctrl Pts',(1.35685843015397,52.1737622922233,0.548422693294248));
#47256=CARTESIAN_POINT('Ctrl Pts',(1.37759572276949,52.1767625445099,0.497116336631775));
#47257=CARTESIAN_POINT('Ctrl Pts',(1.39541296315079,52.1797627967966,0.444646964508727));
#47258=CARTESIAN_POINT('Ctrl Pts',(1.41019664017959,52.1827630490832,0.39137921000763));
#47259=CARTESIAN_POINT('Ctrl Pts',(1.42498695381579,52.1857646482267,0.338087542837671));
#47260=CARTESIAN_POINT('Ctrl Pts',(1.43674087678561,52.1887662473701,0.283997296585355));
#47261=CARTESIAN_POINT('Ctrl Pts',(1.44539584476812,52.1917678465136,0.229484426327902));
#47262=CARTESIAN_POINT('Ctrl Pts',(1.45406746110791,52.1947752194155,0.174866697249202));
#47263=CARTESIAN_POINT('Ctrl Pts',(1.45962815996977,52.1977825923175,0.119825247692324));
#47264=CARTESIAN_POINT('Ctrl Pts',(1.46206731419165,52.2007899652194,0.0647411675243254));
#47265=CARTESIAN_POINT('Ctrl Pts',(1.46404811401639,52.2032322067406,0.0200082288015758));
#47266=CARTESIAN_POINT('Ctrl Pts',(1.46397131916159,52.2056744482617,-0.0247526510507388));
#47267=CARTESIAN_POINT('Ctrl Pts',(1.46185644726803,52.2081166897829,-0.0693395816318449));
#47268=CARTESIAN_POINT('Ctrl Pts',(1.45925136617019,52.2111250219861,-0.124261381113747));
#47269=CARTESIAN_POINT('Ctrl Pts',(1.45354131146121,52.2141333541893,-0.179153290527361));
#47270=CARTESIAN_POINT('Ctrl Pts',(1.44473058552518,52.2171416863925,-0.233636010169793));
#47271=CARTESIAN_POINT('Ctrl Pts',(1.4359356899653,52.2201446134758,-0.28802083981412));
#47272=CARTESIAN_POINT('Ctrl Pts',(1.42405126211438,52.2231475405591,-0.341997420855086));
#47273=CARTESIAN_POINT('Ctrl Pts',(1.40913348218309,52.2261504676424,-0.395189928250392));
#47274=CARTESIAN_POINT('Ctrl Pts',(1.39423063976656,52.2291503878261,-0.448329172769607));
#47275=CARTESIAN_POINT('Ctrl Pts',(1.37630060379322,52.2321503080097,-0.500685392135842));
#47276=CARTESIAN_POINT('Ctrl Pts',(1.35545053637126,52.2351502281933,-0.551893190255918));
#47277=CARTESIAN_POINT('Ctrl Pts',(1.3346130821206,52.2381483335863,-0.603070010407611));
#47278=CARTESIAN_POINT('Ctrl Pts',(1.31085929640091,52.2411464389793,-0.653099297377025));
#47279=CARTESIAN_POINT('Ctrl Pts',(1.28434535208418,52.2441445443723,-0.701633284971403));
#47280=CARTESIAN_POINT('Ctrl Pts',(1.25783693834707,52.2471420243864,-0.750157148795457));
#47281=CARTESIAN_POINT('Ctrl Pts',(1.22856976260241,52.2501395044005,-0.797185868677385));
#47282=CARTESIAN_POINT('Ctrl Pts',(1.19674599977527,52.2531369844147,-0.842396143166551));
#47283=CARTESIAN_POINT('Ctrl Pts',(1.16489280419369,52.2561372366997,-0.887648231155727));
#47284=CARTESIAN_POINT('Ctrl Pts',(1.13047860215334,52.2591374889848,-0.93107807988732));
#47285=CARTESIAN_POINT('Ctrl Pts',(1.09374814527682,52.2621377412699,-0.972392536326513));
#47286=CARTESIAN_POINT('Ctrl Pts',(1.05700119956465,52.2651393404118,-1.01372553942536));
#47287=CARTESIAN_POINT('Ctrl Pts',(1.01793630010504,52.2681409395537,-1.0529408817308));
#47288=CARTESIAN_POINT('Ctrl Pts',(0.976835345856191,52.2711425386956,-1.08978206862015));
#47289=CARTESIAN_POINT('Ctrl Pts',(0.935655331421994,52.274149911596,-1.12669412177324));
#47290=CARTESIAN_POINT('Ctrl Pts',(0.892431852070245,52.2771572844964,-1.16122256470015));
#47291=CARTESIAN_POINT('Ctrl Pts',(0.847479293493252,52.2801646573968,-1.19315174940163));
#47292=CARTESIAN_POINT('Ctrl Pts',(0.810974008240795,52.2826068989302,-1.21908095192766));
#47293=CARTESIAN_POINT('Ctrl Pts',(0.773329118366619,52.2850491404637,-1.2432967432468));
#47294=CARTESIAN_POINT('Ctrl Pts',(0.734724817516778,52.2874913819971,-1.26570600556564));
#47295=CARTESIAN_POINT('Ctrl Pts',(0.687172370372218,52.2904997142004,-1.29330954295674));
#47296=CARTESIAN_POINT('Ctrl Pts',(0.637960756872752,52.2935080464037,-1.31828840483469));
#47297=CARTESIAN_POINT('Ctrl Pts',(0.587410957263806,52.296516378607,-1.34044045644945));
#47298=CARTESIAN_POINT('Ctrl Pts',(0.53695198131096,52.2995193056903,-1.36255270710886));
#47299=CARTESIAN_POINT('Ctrl Pts',(0.48516007083935,52.3025222327737,-1.38184801576162));
#47300=CARTESIAN_POINT('Ctrl Pts',(0.432381427918273,52.305525159857,-1.3981697145881));
#47301=CARTESIAN_POINT('Ctrl Pts',(0.379655633461367,52.3085250800407,-1.41447507012365));
#47302=CARTESIAN_POINT('Ctrl Pts',(0.325945566384239,52.3115250002244,-1.42781255830531));
#47303=CARTESIAN_POINT('Ctrl Pts',(0.271616322349622,52.3145249204081,-1.43807399789902));
#47304=CARTESIAN_POINT('Ctrl Pts',(0.21731994459062,52.3175230258011,-1.44832922987272));
#47305=CARTESIAN_POINT('Ctrl Pts',(0.162405650853886,52.3205211311942,-1.45551200330532));
#47306=CARTESIAN_POINT('Ctrl Pts',(0.107250311706722,52.3235192365872,-1.45956487373423));
#47307=CARTESIAN_POINT('Ctrl Pts',(0.0521064774866472,52.3265167166014,
-1.46361689876938));
#47308=CARTESIAN_POINT('Ctrl Pts',(-0.00327777514903709,52.3295141966155,
-1.4645402783775));
#47309=CARTESIAN_POINT('Ctrl Pts',(-0.0585211746800166,52.3325116766297,
-1.46232948479953));
#47310=CARTESIAN_POINT('Ctrl Pts',(-0.113815667019152,52.3355119289148,
-1.4601166465311));
#47311=CARTESIAN_POINT('Ctrl Pts',(-0.168968516327793,52.3385121811999,
-1.45476386443413));
#47312=CARTESIAN_POINT('Ctrl Pts',(-0.223600683004577,52.341512433485,-1.44631773292036));
#47313=CARTESIAN_POINT('Ctrl Pts',(-0.278257374854556,52.3445140326269,
-1.43786780981546));
#47314=CARTESIAN_POINT('Ctrl Pts',(-0.332392399889933,52.3475156317689,
-1.42632187951638));
#47315=CARTESIAN_POINT('Ctrl Pts',(-0.385637364549656,52.3505172309108,
-1.41177762875858));
#47316=CARTESIAN_POINT('Ctrl Pts',(-0.438984749137255,52.3535246038113,
-1.39720540124987));
#47317=CARTESIAN_POINT('Ctrl Pts',(-0.491438150029499,52.3565319767117,
-1.37962349938454));
#47318=CARTESIAN_POINT('Ctrl Pts',(-0.542645866305165,52.3595393496122,
-1.35917905876375));
#47319=CARTESIAN_POINT('Ctrl Pts',(-0.58423086944253,52.3619815911452,-1.34257644124454));
#47320=CARTESIAN_POINT('Ctrl Pts',(-0.624994623049939,52.3644238326782,
-1.32408702064475));
#47321=CARTESIAN_POINT('Ctrl Pts',(-0.664761154561096,52.3668660742113,
-1.30381166484527));
#47322=CARTESIAN_POINT('Ctrl Pts',(-0.713745227493257,52.3698744064149,
-1.2788366552212));
#47323=CARTESIAN_POINT('Ctrl Pts',(-0.761424339089982,52.3728827386186,
-1.25104405257105));
#47324=CARTESIAN_POINT('Ctrl Pts',(-0.807454563614266,52.3758910708222,
-1.2205938627154));
#47325=CARTESIAN_POINT('Ctrl Pts',(-0.853402084877471,52.3788939979059,
-1.19019838321642));
#47326=CARTESIAN_POINT('Ctrl Pts',(-0.89770616060824,52.3818969249896,-1.15715508131275));
#47327=CARTESIAN_POINT('Ctrl Pts',(-0.940047380002483,52.3848998520733,
-1.121669814763));
#47328=CARTESIAN_POINT('Ctrl Pts',(-0.982346202163917,52.3878997722574,
-1.08622008042345));
#47329=CARTESIAN_POINT('Ctrl Pts',(-1.02268565786927,52.3908996924414,-1.04833356289356));
#47330=CARTESIAN_POINT('Ctrl Pts',(-1.06077682074949,52.3938996126255,-1.00825829357393));
#47331=CARTESIAN_POINT('Ctrl Pts',(-1.09884494052139,52.3968977180189,-0.968207267640473));
#47332=CARTESIAN_POINT('Ctrl Pts',(-1.13466709942395,52.3998958234123,-0.925970496657785));
#47333=CARTESIAN_POINT('Ctrl Pts',(-1.16799060738075,52.4028939288057,-0.881833425920308));
#47334=CARTESIAN_POINT('Ctrl Pts',(-1.20130716434185,52.4058914088203,-0.83770556179425));
#47335=CARTESIAN_POINT('Ctrl Pts',(-1.23212578672651,52.4088888888348,-0.79167860681229));
#47336=CARTESIAN_POINT('Ctrl Pts',(-1.26023501196336,52.4118863688493,-0.744069865417023));
#47337=CARTESIAN_POINT('Ctrl Pts',(-1.28837023450064,52.4148866211348,-0.696417092258431));
#47338=CARTESIAN_POINT('Ctrl Pts',(-1.31379078353157,52.4178868734203,-0.647180066041529));
#47339=CARTESIAN_POINT('Ctrl Pts',(-1.33633019456792,52.4208871257058,-0.596702489592641));
#47340=CARTESIAN_POINT('Ctrl Pts',(-1.35887972387331,52.4238887248481,-0.546202253026419));
#47341=CARTESIAN_POINT('Ctrl Pts',(-1.37854534854324,52.4268903239904,-0.494460851334243));
#47342=CARTESIAN_POINT('Ctrl Pts',(-1.39520930120319,52.4298919231327,-0.441840758459538));
#47343=CARTESIAN_POINT('Ctrl Pts',(-1.41190530798958,52.4328992960336,-0.389119447635857));
#47344=CARTESIAN_POINT('Ctrl Pts',(-1.42558797626905,52.4359066689344,-0.335516582714291));
#47345=CARTESIAN_POINT('Ctrl Pts',(-1.43619013507206,52.4389140418352,-0.281407437573529));
#47346=CARTESIAN_POINT('Ctrl Pts',(-1.44479998605859,52.4413562833653,-0.237466228492767));
#47347=CARTESIAN_POINT('Ctrl Pts',(-1.45137926737774,52.4437985248953,-0.193191457633103));
#47348=CARTESIAN_POINT('Ctrl Pts',(-1.45591726187338,52.4462407664254,-0.148785673299232));
#47349=CARTESIAN_POINT('Ctrl Pts',(-1.46093679807477,52.4489421623359,-0.099667843335173));
#47350=CARTESIAN_POINT('Ctrl Pts',(-1.46347129195106,52.4516435582465,-0.0502917836747106));
#47351=CARTESIAN_POINT('Ctrl Pts',(-1.4634997575168,52.4543449541571,-0.000842465582414598));
#47352=CARTESIAN_POINT('Ctrl Pts',(-1.46349984429797,52.5256550458429,-0.000675085045776301));
#47353=CARTESIAN_POINT('Ctrl Pts',(-1.46348221233139,52.5235656984443,-0.0388989806992069));
#47354=CARTESIAN_POINT('Ctrl Pts',(-1.4619672098159,52.5214763510457,-0.0770868883956254));
#47355=CARTESIAN_POINT('Ctrl Pts',(-1.45896244675631,52.5193870036471,-0.115155672699358));
#47356=CARTESIAN_POINT('Ctrl Pts',(-1.45463605973137,52.5163786714437,-0.169968744878602));
#47357=CARTESIAN_POINT('Ctrl Pts',(-1.44720716417161,52.5133703392402,-0.224654556156892));
#47358=CARTESIAN_POINT('Ctrl Pts',(-1.43669195684029,52.5103620070367,-0.278834128381786));
#47359=CARTESIAN_POINT('Ctrl Pts',(-1.42619564235484,52.5073590799532,-0.332916355278562));
#47360=CARTESIAN_POINT('Ctrl Pts',(-1.41262412003453,52.5043561528696,-0.386493633192423));
#47361=CARTESIAN_POINT('Ctrl Pts',(-1.39604532996566,52.5013532257861,-0.439192084037346));
#47362=CARTESIAN_POINT('Ctrl Pts',(-1.37948314061905,52.4983533056022,-0.49183776671632));
#47363=CARTESIAN_POINT('Ctrl Pts',(-1.35991980613222,52.4953533854183,-0.5436058634614));
#47364=CARTESIAN_POINT('Ctrl Pts',(-1.33747389630939,52.4923534652344,-0.594134519019868));
#47365=CARTESIAN_POINT('Ctrl Pts',(-1.31504156505682,52.4893553598411,-0.644632607454754));
#47366=CARTESIAN_POINT('Ctrl Pts',(-1.28973032877393,52.4863572544478,-0.693892258377518));
#47367=CARTESIAN_POINT('Ctrl Pts',(-1.26170719096556,52.4833591490546,-0.741570774953939));
#47368=CARTESIAN_POINT('Ctrl Pts',(-1.23368989854155,52.4803616690402,-0.789239346203877));
#47369=CARTESIAN_POINT('Ctrl Pts',(-1.20296209561939,52.4773641890257,-0.835326982267059));
#47370=CARTESIAN_POINT('Ctrl Pts',(-1.16973599780358,52.4743667090113,-0.879516881840516));
#47371=CARTESIAN_POINT('Ctrl Pts',(-1.13647917025973,52.471366456726,-0.923747651202649));
#47372=CARTESIAN_POINT('Ctrl Pts',(-1.10071974961237,52.4683662044406,-0.966076753465806));
#47373=CARTESIAN_POINT('Ctrl Pts',(-1.0627115616305,52.4653659521553,-1.00621885630158));
#47374=CARTESIAN_POINT('Ctrl Pts',(-1.02468631122093,52.4623643530131,-1.04637897951043));
#47375=CARTESIAN_POINT('Ctrl Pts',(-0.984410666551524,52.4593627538709,
-1.08434978262169));
#47376=CARTESIAN_POINT('Ctrl Pts',(-0.942174432683029,52.4563611547287,
-1.11988373878649));
#47377=CARTESIAN_POINT('Ctrl Pts',(-0.89985695484988,52.453353781828,-1.15548604667716));
#47378=CARTESIAN_POINT('Ctrl Pts',(-0.85557177787915,52.4503464089273,-1.1886418250489));
#47379=CARTESIAN_POINT('Ctrl Pts',(-0.809639896454233,52.4473390360266,
-1.2191453925064));
#47380=CARTESIAN_POINT('Ctrl Pts',(-0.772339318132137,52.4448967944953,
-1.24391687305007));
#47381=CARTESIAN_POINT('Ctrl Pts',(-0.733953435917443,52.442454552964,-1.266940042379));
#47382=CARTESIAN_POINT('Ctrl Pts',(-0.694665275384337,52.4400123114327,
-1.28812748017236));
#47383=CARTESIAN_POINT('Ctrl Pts',(-0.646270455693958,52.4370039792292,
-1.31422598460214));
#47384=CARTESIAN_POINT('Ctrl Pts',(-0.596299607221141,52.4339956470258,
-1.33764906610797));
#47385=CARTESIAN_POINT('Ctrl Pts',(-0.545079892123478,52.4309873148223,
-1.35820475672951));
#47386=CARTESIAN_POINT('Ctrl Pts',(-0.493952204329986,52.4279843877388,
-1.37872351460377));
#47387=CARTESIAN_POINT('Ctrl Pts',(-0.441580589407029,52.4249814606553,
-1.39638490970809));
#47388=CARTESIAN_POINT('Ctrl Pts',(-0.388315992885773,52.4219785335717,
-1.41104320971016));
#47389=CARTESIAN_POINT('Ctrl Pts',(-0.335104731425083,52.4189786133879,
-1.42568683202067));
#47390=CARTESIAN_POINT('Ctrl Pts',(-0.281002766876122,52.415978693204,-1.43733317602712));
#47391=CARTESIAN_POINT('Ctrl Pts',(-0.226378408317006,52.4129787730202,
-1.44588556471384));
#47392=CARTESIAN_POINT('Ctrl Pts',(-0.171787094561888,52.409980667627,-1.4544327796646));
#47393=CARTESIAN_POINT('Ctrl Pts',(-0.116674534556434,52.4069825622338,
-1.45988966712609));
#47394=CARTESIAN_POINT('Ctrl Pts',(-0.0614192151634559,52.4039844568406,
-1.46221063120493));
#47395=CARTESIAN_POINT('Ctrl Pts',(-0.00617542155252979,52.4009869768262,
-1.46453111115072));
#47396=CARTESIAN_POINT('Ctrl Pts',(0.0492105442026703,52.3979894968119,
-1.46371694433711));
#47397=CARTESIAN_POINT('Ctrl Pts',(0.104357424786168,52.3949920167976,-1.45977456406529));
#47398=CARTESIAN_POINT('Ctrl Pts',(0.159555308910696,52.3919917645123,-1.45582853761526));
#47399=CARTESIAN_POINT('Ctrl Pts',(0.214513137333803,52.388991512227,-1.44874855467913));
#47400=CARTESIAN_POINT('Ctrl Pts',(0.268853518339394,52.3859912599417,-1.43859307508292));
#47401=CARTESIAN_POINT('Ctrl Pts',(0.32321829353139,52.3829896607996,-1.42843303654439));
#47402=CARTESIAN_POINT('Ctrl Pts',(0.376964554247815,52.3799880616575,-1.41519487574425));
#47403=CARTESIAN_POINT('Ctrl Pts',(0.429727152053714,52.3769864625154,-1.39898778578936));
#47404=CARTESIAN_POINT('Ctrl Pts',(0.482591241925535,52.3739790896148,-1.38274952051121));
#47405=CARTESIAN_POINT('Ctrl Pts',(0.534467391389492,52.3709717167142,-1.36353110081879));
#47406=CARTESIAN_POINT('Ctrl Pts',(0.585008687370433,52.3679643438135,-1.34149062080252));
#47407=CARTESIAN_POINT('Ctrl Pts',(0.626052500753326,52.3655221022819,-1.32359188411404));
#47408=CARTESIAN_POINT('Ctrl Pts',(0.666216290259966,52.3630798607503,-1.30383303059522));
#47409=CARTESIAN_POINT('Ctrl Pts',(0.705327333557285,52.3606376192187,-1.28232039776998));
#47410=CARTESIAN_POINT('Ctrl Pts',(0.753503981746238,52.3576292870153,-1.25582132088878));
#47411=CARTESIAN_POINT('Ctrl Pts',(0.800287938591522,52.3546209548119,-1.22654696647804));
#47412=CARTESIAN_POINT('Ctrl Pts',(0.845340466043305,52.3516126226084,-1.19466804865188));
#47413=CARTESIAN_POINT('Ctrl Pts',(0.890312046878343,52.3486096955249,-1.16284640820147));
#47414=CARTESIAN_POINT('Ctrl Pts',(0.933557943449558,52.3456067684414,-1.12842979366184));
#47415=CARTESIAN_POINT('Ctrl Pts',(0.9747653586962,52.3426038413579,-1.09163397963139));
#47416=CARTESIAN_POINT('Ctrl Pts',(1.01593151201406,52.3396039211741,-1.05487501009237));
#47417=CARTESIAN_POINT('Ctrl Pts',(1.05506283468393,52.3366040009902,-1.01574191051119));
#47418=CARTESIAN_POINT('Ctrl Pts',(1.09187832183192,52.3336040808064,-0.9744916522544));
#47419=CARTESIAN_POINT('Ctrl Pts',(1.12867153758691,52.3306059754132,-0.933266348189026));
#47420=CARTESIAN_POINT('Ctrl Pts',(1.16315134293306,52.32760787002,-0.88992681756898));
#47421=CARTESIAN_POINT('Ctrl Pts',(1.19507412492466,52.3246097646268,-0.844766290719245));
#47422=CARTESIAN_POINT('Ctrl Pts',(1.22699024809984,52.3216122846125,-0.799615183965102));
#47423=CARTESIAN_POINT('Ctrl Pts',(1.25635010185372,52.3186148045982,-0.752644266816934));
#47424=CARTESIAN_POINT('Ctrl Pts',(1.28295227970449,52.3156173245838,-0.70417731999905));
#47425=CARTESIAN_POINT('Ctrl Pts',(1.30957906103701,52.3126170722986,-0.655665547691769));
#47426=CARTESIAN_POINT('Ctrl Pts',(1.33344281533899,52.3096168200133,-0.60565544577297));
#47427=CARTESIAN_POINT('Ctrl Pts',(1.35438794004212,52.306616567728,-0.554495769026658));
#47428=CARTESIAN_POINT('Ctrl Pts',(1.37534246731598,52.3036149685859,-0.5033131259583));
#47429=CARTESIAN_POINT('Ctrl Pts',(1.39337558042551,52.3006133694438,-0.450980380244922));
#47430=CARTESIAN_POINT('Ctrl Pts',(1.40838093870219,52.2976117703017,-0.397863521198329));
#47431=CARTESIAN_POINT('Ctrl Pts',(1.42341516069815,52.2946043974011,-0.344644488642768));
#47432=CARTESIAN_POINT('Ctrl Pts',(1.43540987731051,52.2915970245004,-0.290638847159452));
#47433=CARTESIAN_POINT('Ctrl Pts',(1.44430972084507,52.2885896515998,-0.236223792773784));
#47434=CARTESIAN_POINT('Ctrl Pts',(1.45153714764747,52.286147410068,-0.192034159439937));
#47435=CARTESIAN_POINT('Ctrl Pts',(1.45672454183031,52.2837051685362,-0.147574815969591));
#47436=CARTESIAN_POINT('Ctrl Pts',(1.45986754430988,52.2812629270044,-0.103048547154441));
#47437=CARTESIAN_POINT('Ctrl Pts',(1.46373906784771,52.2782545948007,-0.0482014705485008));
#47438=CARTESIAN_POINT('Ctrl Pts',(1.46452364628708,52.2752462625971,0.00698105278430778));
#47439=CARTESIAN_POINT('Ctrl Pts',(1.46218094840775,52.2722379303934,0.0621218489214135));
#47440=CARTESIAN_POINT('Ctrl Pts',(1.45984245969221,52.2692350033097,0.117163572683595));
#47441=CARTESIAN_POINT('Ctrl Pts',(1.45438786698462,52.266232076226,0.172163194004425));
#47442=CARTESIAN_POINT('Ctrl Pts',(1.44582876554686,52.2632291491423,0.226740888939868));
#47443=CARTESIAN_POINT('Ctrl Pts',(1.43727823453342,52.2602292289582,0.281263933979221));
#47444=CARTESIAN_POINT('Ctrl Pts',(1.42562943388078,52.2572293087742,0.335365369639398));
#47445=CARTESIAN_POINT('Ctrl Pts',(1.41094581340977,52.2542293885901,0.38866973334883));
#47446=CARTESIAN_POINT('Ctrl Pts',(1.39627107574074,52.2512312831967,0.441941850780256));
#47447=CARTESIAN_POINT('Ctrl Pts',(1.378565296993,52.2482331778033,0.494417343063966));
#47448=CARTESIAN_POINT('Ctrl Pts',(1.35794267088501,52.2452350724099,0.54573249178483));
#47449=CARTESIAN_POINT('Ctrl Pts',(1.33732434647859,52.2422375923953,0.597036936609169));
#47450=CARTESIAN_POINT('Ctrl Pts',(1.31379057988949,52.2392401123808,0.647181027993167));
#47451=CARTESIAN_POINT('Ctrl Pts',(1.28750412464189,52.2362426323663,0.695819932906582));
#47452=CARTESIAN_POINT('Ctrl Pts',(1.26119335791405,52.2332423800808,0.744503822347745));
#47453=CARTESIAN_POINT('Ctrl Pts',(1.23212506767509,52.2302421277953,0.791679277473329));
#47454=CARTESIAN_POINT('Ctrl Pts',(1.2005078340374,52.2272418755098,0.837026397681));
#47455=CARTESIAN_POINT('Ctrl Pts',(1.16887640696426,52.2242402763675,0.882393874869642));
#47456=CARTESIAN_POINT('Ctrl Pts',(1.13469408260439,52.2212386772252,0.925930964162548));
#47457=CARTESIAN_POINT('Ctrl Pts',(1.09821064151044,52.2182370780829,0.967349800678757));
#47458=CARTESIAN_POINT('Ctrl Pts',(1.06165702229867,52.2152297051821,1.00884830884604));
#47459=CARTESIAN_POINT('Ctrl Pts',(1.02279381580018,52.2122223322812,1.04822004642159));
#47460=CARTESIAN_POINT('Ctrl Pts',(0.981907867256102,52.2092149593804,1.0852138914613));
#47461=CARTESIAN_POINT('Ctrl Pts',(0.948705013861077,52.2067727178504,1.11525602713653));
#47462=CARTESIAN_POINT('Ctrl Pts',(0.914168974229151,52.2043304763203,1.14373065169785));
#47463=CARTESIAN_POINT('Ctrl Pts',(0.878467741568595,52.2018882347902,1.1705241035636));
#47464=CARTESIAN_POINT('Ctrl Pts',(0.834491268894918,52.198879902587,1.20352804813355));
#47465=CARTESIAN_POINT('Ctrl Pts',(0.788558493019324,52.1958715703837,1.23412063783018));
#47466=CARTESIAN_POINT('Ctrl Pts',(0.740964397071321,52.1928632381805,1.2620633947123));
#47467=CARTESIAN_POINT('Ctrl Pts',(0.693455814217933,52.1898603110971,1.28995594638376));
#47468=CARTESIAN_POINT('Ctrl Pts',(0.64429228690314,52.1868573840138,1.31520784746683));
#47469=CARTESIAN_POINT('Ctrl Pts',(0.593799191766317,52.1838544569304,1.33762280552391));
#47470=CARTESIAN_POINT('Ctrl Pts',(0.543356656522229,52.1808545367468,1.36001531897007));
#47471=CARTESIAN_POINT('Ctrl Pts',(0.491587671504272,52.1778546165631,1.37957630275564));
#47472=CARTESIAN_POINT('Ctrl Pts',(0.438842077635214,52.1748546963794,1.39615539281873));
#47473=CARTESIAN_POINT('Ctrl Pts',(0.386128392018362,52.1718565909864,1.41272445342251));
#47474=CARTESIAN_POINT('Ctrl Pts',(0.332439771952628,52.1688584855933,1.42631503715667));
#47475=CARTESIAN_POINT('Ctrl Pts',(0.278143717957992,52.1658603802003,1.43682578003059));
#47476=CARTESIAN_POINT('Ctrl Pts',(0.223858989650928,52.1628629001861,1.44733433045439));
#47477=CARTESIAN_POINT('Ctrl Pts',(0.168967597944205,52.159865420172,1.4547642151376));
#47478=CARTESIAN_POINT('Ctrl Pts',(0.11384751892074,52.1568679401578,1.45906510904606));
#47479=CARTESIAN_POINT('Ctrl Pts',(0.058676461144021,52.1538676878727,1.46336998071023));
#47480=CARTESIAN_POINT('Ctrl Pts',(0.0032768218967902,52.1508674355876,
1.46454003810465));
#47481=CARTESIAN_POINT('Ctrl Pts',(-0.0519695098638592,52.1478671833025,
1.46257697918589));
#47482=CARTESIAN_POINT('Ctrl Pts',(-0.10724064250541,52.1448655841605,1.46061303902145));
#47483=CARTESIAN_POINT('Ctrl Pts',(-0.162357802847613,52.1418639850186,
1.45551322747208));
#47484=CARTESIAN_POINT('Ctrl Pts',(-0.216943665905202,52.1388623858766,
1.44733123224216));
#47485=CARTESIAN_POINT('Ctrl Pts',(-0.271634528190421,52.1358550129762,
1.43913349844677));
#47486=CARTESIAN_POINT('Ctrl Pts',(-0.325791532254495,52.1328476400757,
1.42784184448758));
#47487=CARTESIAN_POINT('Ctrl Pts',(-0.379048114992458,52.1298402671752,
1.4135610268116));
#47488=CARTESIAN_POINT('Ctrl Pts',(-0.422296971245356,52.1273980256422,
1.40196379320987));
#47489=CARTESIAN_POINT('Ctrl Pts',(-0.46495215472597,52.1249557841091,1.38839627300597));
#47490=CARTESIAN_POINT('Ctrl Pts',(-0.506827052270095,52.1225135425761,
1.37293794072682));
#47491=CARTESIAN_POINT('Ctrl Pts',(-0.558408192417141,52.1195052103728,
1.35389649942204));
#47492=CARTESIAN_POINT('Ctrl Pts',(-0.609024760409792,52.1164968781696,
1.33190355763431));
#47493=CARTESIAN_POINT('Ctrl Pts',(-0.658316400906693,52.1134885459664,
1.30707756705456));
#47494=CARTESIAN_POINT('Ctrl Pts',(-0.707519478302657,52.1104856188831,
1.28229618174027));
#47495=CARTESIAN_POINT('Ctrl Pts',(-0.755401883695639,52.1074826917997,
1.25469208458097));
#47496=CARTESIAN_POINT('Ctrl Pts',(-0.801622214624486,52.1044797647164,
1.22443214390204));
#47497=CARTESIAN_POINT('Ctrl Pts',(-0.847796264077206,52.1014798445328,
1.19420250319486));
#47498=CARTESIAN_POINT('Ctrl Pts',(-0.892311095418834,52.0984799243492,
1.1613225748655));
#47499=CARTESIAN_POINT('Ctrl Pts',(-0.934850619701237,52.0954800041656,
1.12600469308268));
#47500=CARTESIAN_POINT('Ctrl Pts',(-0.977364409855472,52.0924818987726,
1.09070817672205));
#47501=CARTESIAN_POINT('Ctrl Pts',(-1.01790485514864,52.0894837933796,1.05297696701299));
#47502=CARTESIAN_POINT('Ctrl Pts',(-1.05618745181737,52.0864856879866,1.01306481363412));
#47503=CARTESIAN_POINT('Ctrl Pts',(-1.09446206306729,52.0834882079725,0.973160985585508));
#47504=CARTESIAN_POINT('Ctrl Pts',(-1.13047939493121,52.0804907279584,0.93107749861966));
#47505=CARTESIAN_POINT('Ctrl Pts',(-1.16399213862248,52.0774932479443,0.887104588661938));
#47506=CARTESIAN_POINT('Ctrl Pts',(-1.19753587715117,52.0744929956592,0.843091009602121));
#47507=CARTESIAN_POINT('Ctrl Pts',(-1.22857007782311,52.0714927433742,0.797184937546463));
#47508=CARTESIAN_POINT('Ctrl Pts',(-1.2568890134035,52.0684924910891,0.749708115192558));
#47509=CARTESIAN_POINT('Ctrl Pts',(-1.28522066176543,52.0654908919472,0.702209979803454));
#47510=CARTESIAN_POINT('Ctrl Pts',(-1.31083436989937,52.0624892928053,0.65314015814533));
#47511=CARTESIAN_POINT('Ctrl Pts',(-1.33357056241619,52.0594876936634,0.602844760329691));
#47512=CARTESIAN_POINT('Ctrl Pts',(-1.35635048938215,52.056480320763,0.552452616257335));
#47513=CARTESIAN_POINT('Ctrl Pts',(-1.37624165184502,52.0534729478626,0.500830681054212));
#47514=CARTESIAN_POINT('Ctrl Pts',(-1.39313321455586,52.0504655749622,0.448343725841303));
#47515=CARTESIAN_POINT('Ctrl Pts',(-1.40685059426998,52.0480233334288,0.405719872322318));
#47516=CARTESIAN_POINT('Ctrl Pts',(-1.41859071834354,52.0455810918954,0.362525986532535));
#47517=CARTESIAN_POINT('Ctrl Pts',(-1.42831912530962,52.0431388503619,0.31896195113959));
#47518=CARTESIAN_POINT('Ctrl Pts',(-1.44470142292229,52.0390262009033,0.245601636803999));
#47519=CARTESIAN_POINT('Ctrl Pts',(-1.45543708182968,52.0349135514447,0.170937601088179));
#47520=CARTESIAN_POINT('Ctrl Pts',(-1.46036746516698,52.030800901986,0.0957032741434123));
#47521=CARTESIAN_POINT('Ctrl Pts',(-1.4624238073246,52.029085616605,0.0643248786693624));
#47522=CARTESIAN_POINT('Ctrl Pts',(-1.46347084113317,52.0273703312239,0.0328475503915992));
#47523=CARTESIAN_POINT('Ctrl Pts',(-1.46349939936907,52.0256550458429,0.00132591340718779));
#47524=CARTESIAN_POINT('Origin',(0.,55.715,0.));
#47525=CARTESIAN_POINT('',(-1.46326096487245,51.4543449563653,2.91466190404779E-5));
#47526=CARTESIAN_POINT('',(-1.46349999166114,51.5256550458102,-0.00015623008169786));
#47527=CARTESIAN_POINT('',(-1.4635,55.715,-1.79227059055215E-16));
#47528=CARTESIAN_POINT('Ctrl Pts',(-1.46111644255208,51.4543449761763,2.9469711106117E-5));
#47529=CARTESIAN_POINT('Ctrl Pts',(-1.46115932464248,51.4674781374027,0.242492190997025));
#47530=CARTESIAN_POINT('Ctrl Pts',(-1.28920392493414,51.5070695293669,0.973365973503329));
#47531=CARTESIAN_POINT('Ctrl Pts',(-0.135188693436253,51.5731191520696,
1.72443892271662));
#47532=CARTESIAN_POINT('Ctrl Pts',(1.37535400909208,51.6524938442836,1.04898375450915));
#47533=CARTESIAN_POINT('Ctrl Pts',(1.62729589757749,51.7318685364977,-0.586407376508306));
#47534=CARTESIAN_POINT('Ctrl Pts',(0.39008234965916,51.811243228712,-1.68517100717997));
#47535=CARTESIAN_POINT('Ctrl Pts',(-1.09934054493347,51.8854019417222,-1.27095135834563));
#47536=CARTESIAN_POINT('Ctrl Pts',(-1.46045977152297,51.9331024239943,-0.388908969420869));
#47537=CARTESIAN_POINT('Ctrl Pts',(-1.46404229631382,51.9543446755284,0.00128158248083468));
#47538=CARTESIAN_POINT('Ctrl Pts',(-1.4634993993698,52.025655045799,0.00132591260086507));
#47539=CARTESIAN_POINT('Ctrl Pts',(-1.46354869863678,52.0226939958363,-0.0530890221102393));
#47540=CARTESIAN_POINT('Ctrl Pts',(-1.46055891101372,52.0197329458736,-0.107594537808096));
#47541=CARTESIAN_POINT('Ctrl Pts',(-1.4545263530835,52.0167718959108,-0.161818843728488));
#47542=CARTESIAN_POINT('Ctrl Pts',(-1.44849874612696,52.013813276108,-0.215998647281014));
#47543=CARTESIAN_POINT('Ctrl Pts',(-1.43943337148726,52.0108546563052,-0.269897158612643));
#47544=CARTESIAN_POINT('Ctrl Pts',(-1.42737854950162,52.0078960365024,-0.323145054770552));
#47545=CARTESIAN_POINT('Ctrl Pts',(-1.4153285359981,52.0049385968473,-0.37637171116587));
#47546=CARTESIAN_POINT('Ctrl Pts',(-1.40029155813435,52.0019811571922,-0.428947736076216));
#47547=CARTESIAN_POINT('Ctrl Pts',(-1.38236704141599,51.9990237175371,-0.480513904904738));
#47548=CARTESIAN_POINT('Ctrl Pts',(-1.36442889580751,51.9960640291954,-0.532119282023224));
#47549=CARTESIAN_POINT('Ctrl Pts',(-1.3435989973952,51.9931043408537,-0.582712751097336));
#47550=CARTESIAN_POINT('Ctrl Pts',(-1.32002617989456,51.990144652512,-0.631951844995319));
#47551=CARTESIAN_POINT('Ctrl Pts',(-1.29644571658337,51.9871840041995,-0.681206909524852));
#47552=CARTESIAN_POINT('Ctrl Pts',(-1.27012082155683,51.984223355887,-0.729106243757953));
#47553=CARTESIAN_POINT('Ctrl Pts',(-1.24124631062107,51.9812627075745,-0.775332087798249));
#47554=CARTESIAN_POINT('Ctrl Pts',(-1.21231567244277,51.9782963042546,-0.821647787184175));
#47555=CARTESIAN_POINT('Ctrl Pts',(-1.18082583043793,51.9753299009347,-0.86628304977985));
#47556=CARTESIAN_POINT('Ctrl Pts',(-1.1470142439362,51.9723634976147,-0.908950259479294));
#47557=CARTESIAN_POINT('Ctrl Pts',(-1.11434198296482,51.9694970511257,-0.9501797418684));
#47558=CARTESIAN_POINT('Ctrl Pts',(-1.07950236031916,51.9666306046367,-0.989571445912857));
#47559=CARTESIAN_POINT('Ctrl Pts',(-1.04274147209032,51.9637641581477,-1.02689944609144));
#47560=CARTESIAN_POINT('Ctrl Pts',(-1.00416096335152,51.9607558259461,-1.06607513815108));
#47561=CARTESIAN_POINT('Ctrl Pts',(-0.963287366499095,51.9577474937445,
-1.10315714890105));
#47562=CARTESIAN_POINT('Ctrl Pts',(-0.920376928025628,51.9547391615429,
-1.13786579189204));
#47563=CARTESIAN_POINT('Ctrl Pts',(-0.877543587442246,51.9517362344612,
-1.1725120732937));
#47564=CARTESIAN_POINT('Ctrl Pts',(-0.832681075231708,51.9487333073795,
-1.20479311914918));
#47565=CARTESIAN_POINT('Ctrl Pts',(-0.78608196587128,51.9457303802978,-1.23446644058554));
#47566=CARTESIAN_POINT('Ctrl Pts',(-0.739529517266323,51.9427304601158,
-1.26411004944554));
#47567=CARTESIAN_POINT('Ctrl Pts',(-0.691244359782136,51.9397305399338,
-1.29115082347741));
#47568=CARTESIAN_POINT('Ctrl Pts',(-0.641550089063736,51.9367306197518,
-1.31538805423431));
#47569=CARTESIAN_POINT('Ctrl Pts',(-0.591885880710703,51.9337325143604,
-1.33961062276806));
#47570=CARTESIAN_POINT('Ctrl Pts',(-0.540814722945341,51.930734408969,-1.36103277794393));
#47571=CARTESIAN_POINT('Ctrl Pts',(-0.488684960241562,51.9277363035776,
-1.37949964104153));
#47572=CARTESIAN_POINT('Ctrl Pts',(-0.436566071355437,51.924738823565,-1.39796265211119));
#47573=CARTESIAN_POINT('Ctrl Pts',(-0.383389514216903,51.9217413435525,
-1.4134714185952));
#47574=CARTESIAN_POINT('Ctrl Pts',(-0.329521581096066,51.9187438635399,
-1.4259199758724));
#47575=CARTESIAN_POINT('Ctrl Pts',(-0.275603827290023,51.9157436112564,
-1.43838004641209));
#47576=CARTESIAN_POINT('Ctrl Pts',(-0.220993936311395,51.9127433589729,
-1.44777413324175));
#47577=CARTESIAN_POINT('Ctrl Pts',(-0.166069804793557,51.9097431066893,
-1.45404713470225));
#47578=CARTESIAN_POINT('Ctrl Pts',(-0.111121017034867,51.9067415075489,
-1.46032295220427));
#47579=CARTESIAN_POINT('Ctrl Pts',(-0.0558582365253506,51.9037399084086,
-1.46347486104163));
#47580=CARTESIAN_POINT('Ctrl Pts',(-0.000662576695014244,51.9007383092682,
-1.46349985001438));
#47581=CARTESIAN_POINT('Ctrl Pts',(0.0546392553450768,51.8977309363692,
-1.46352488705494));
#47582=CARTESIAN_POINT('Ctrl Pts',(0.109873179261047,51.8947235634703,-1.46041101743114));
#47583=CARTESIAN_POINT('Ctrl Pts',(0.164661130782233,51.8917161905713,-1.45420733116345));
#47584=CARTESIAN_POINT('Ctrl Pts',(0.209153588457817,51.8892739490254,-1.44916941240514));
#47585=CARTESIAN_POINT('Ctrl Pts',(0.253351922077775,51.8868317074795,-1.44209483761692));
#47586=CARTESIAN_POINT('Ctrl Pts',(0.297059776139041,51.8843894659336,-1.43303445157478));
#47587=CARTESIAN_POINT('Ctrl Pts',(0.350898736126536,51.8813811337312,-1.42187394570985));
#47588=CARTESIAN_POINT('Ctrl Pts',(0.404222686025515,51.8783728015288,-1.40765132960243));
#47589=CARTESIAN_POINT('Ctrl Pts',(0.456657664065666,51.8753644693263,-1.39043015928528));
#47590=CARTESIAN_POINT('Ctrl Pts',(0.508998431318031,51.8723615422439,-1.37323993052819));
#47591=CARTESIAN_POINT('Ctrl Pts',(0.560452897965904,51.8693586151614,-1.35306200233425));
#47592=CARTESIAN_POINT('Ctrl Pts',(0.610658645679146,51.866355688079,-1.33001062719713));
#47593=CARTESIAN_POINT('Ctrl Pts',(0.66081412122682,51.8633557678963,-1.30698233393012));
#47594=CARTESIAN_POINT('Ctrl Pts',(0.709722876371364,51.8603558477135,-1.28108651255609));
#47595=CARTESIAN_POINT('Ctrl Pts',(0.757040764890917,51.8573559275308,-1.25248613976099));
#47596=CARTESIAN_POINT('Ctrl Pts',(0.80433002862821,51.8543578221387,-1.22390306865599));
#47597=CARTESIAN_POINT('Ctrl Pts',(0.850029881403249,51.8513597167466,-1.19261896174547));
#47598=CARTESIAN_POINT('Ctrl Pts',(0.893821253282568,51.8483616113545,-1.15884244709123));
#47599=CARTESIAN_POINT('Ctrl Pts',(0.937603490659938,51.8453641313413,-1.12507297792621));
#47600=CARTESIAN_POINT('Ctrl Pts',(0.979477619030784,51.8423666513281,-1.08881245612636));
#47601=CARTESIAN_POINT('Ctrl Pts',(1.01915592509,51.8393691713149,-1.05031112074182));
#47602=CARTESIAN_POINT('Ctrl Pts',(1.05887092831282,51.8363689190307,-1.01177417673525));
#47603=CARTESIAN_POINT('Ctrl Pts',(1.09638567101698,51.8333686667466,-0.970992647325472));
#47604=CARTESIAN_POINT('Ctrl Pts',(1.1314488747108,51.8303684144625,-0.928254110637631));
#47605=CARTESIAN_POINT('Ctrl Pts',(1.16652781878599,51.8273668153215,-0.885496387999963));
#47606=CARTESIAN_POINT('Ctrl Pts',(1.19915271761295,51.8243652161806,-0.840780334767258));
#47607=CARTESIAN_POINT('Ctrl Pts',(1.2291143085151,51.8213636170396,-0.794424487666041));
#47608=CARTESIAN_POINT('Ctrl Pts',(1.25913353235958,51.8183562441401,-0.747979472273609));
#47609=CARTESIAN_POINT('Ctrl Pts',(1.28647895112592,51.8153488712407,-0.699888822361476));
#47610=CARTESIAN_POINT('Ctrl Pts',(1.31098672592821,51.8123414983412,-0.650496775118848));
#47611=CARTESIAN_POINT('Ctrl Pts',(1.33088911505348,51.8098992568006,-0.61038624889416));
#47612=CARTESIAN_POINT('Ctrl Pts',(1.34892098079718,51.80745701526,-0.569418040334823));
#47613=CARTESIAN_POINT('Ctrl Pts',(1.36501852540261,51.8050147737194,-0.52778468650357));
#47614=CARTESIAN_POINT('Ctrl Pts',(1.38484734297908,51.8020064415064,-0.476501077825916));
#47615=CARTESIAN_POINT('Ctrl Pts',(1.40182434334399,51.7989981092935,-0.423989098985121));
#47616=CARTESIAN_POINT('Ctrl Pts',(1.41580006576566,51.7959897770805,-0.370597387710631));
#47617=CARTESIAN_POINT('Ctrl Pts',(1.42975067777728,51.7929868499874,-0.31730160620087));
#47618=CARTESIAN_POINT('Ctrl Pts',(1.44071057985552,51.7899839228944,-0.263129736274374));
#47619=CARTESIAN_POINT('Ctrl Pts',(1.44857916261137,51.7869809958013,-0.208448218145759));
#47620=CARTESIAN_POINT('Ctrl Pts',(1.45643986637511,51.7839810756079,-0.153821453873512));
#47621=CARTESIAN_POINT('Ctrl Pts',(1.46121530727312,51.7809811554145,-0.0986865730917024));
#47622=CARTESIAN_POINT('Ctrl Pts',(1.46285572030392,51.7779812352211,-0.0434210959567612));
#47623=CARTESIAN_POINT('Ctrl Pts',(1.46449514097292,51.7749831298184,0.011810948531835));
#47624=CARTESIAN_POINT('Ctrl Pts',(1.46300327682994,51.7719850244156,0.0671729052360835));
#47625=CARTESIAN_POINT('Ctrl Pts',(1.45838231670623,51.7689869190129,0.122283557024521));
#47626=CARTESIAN_POINT('Ctrl Pts',(1.4537623204749,51.765989438989,0.177382713206783));
#47627=CARTESIAN_POINT('Ctrl Pts',(1.44601456840762,51.7629919589652,0.232230141822435));
#47628=CARTESIAN_POINT('Ctrl Pts',(1.43519321561095,51.7599944789413,0.28644839651201));
#47629=CARTESIAN_POINT('Ctrl Pts',(1.42436185450047,51.7569942266466,0.340716795884744));
#47630=CARTESIAN_POINT('Ctrl Pts',(1.41045131650601,51.7539939743519,0.394354338834923));
#47631=CARTESIAN_POINT('Ctrl Pts',(1.39356688884657,51.7509937220573,0.446993933192053));
#47632=CARTESIAN_POINT('Ctrl Pts',(1.37667488152258,51.7479921229058,0.499657158226818));
#47633=CARTESIAN_POINT('Ctrl Pts',(1.3568065133307,51.7449905237543,0.551321047025914));
#47634=CARTESIAN_POINT('Ctrl Pts',(1.33411587080629,51.7419889246029,0.601637011214214));
#47635=CARTESIAN_POINT('Ctrl Pts',(1.3113815814526,51.7389815516931,0.652049761216168));
#47636=CARTESIAN_POINT('Ctrl Pts',(1.28581441695944,51.7359741787833,0.701108936269424));
#47637=CARTESIAN_POINT('Ctrl Pts',(1.25761469449969,51.7329668058736,0.748490167055289));
#47638=CARTESIAN_POINT('Ctrl Pts',(1.23471413201236,51.7305245644174,0.78696773852383));
#47639=CARTESIAN_POINT('Ctrl Pts',(1.21007838239006,51.7280823229613,0.824339144666384));
#47640=CARTESIAN_POINT('Ctrl Pts',(1.18383458759932,51.7256400815051,0.860446348823416));
#47641=CARTESIAN_POINT('Ctrl Pts',(1.15150770510008,51.7226317493178,0.90492289482096));
#47642=CARTESIAN_POINT('Ctrl Pts',(1.11660192598051,51.7196234171304,0.94766997657345));
#47643=CARTESIAN_POINT('Ctrl Pts',(1.07932906361815,51.7166150849431,0.988372916681332));
#47644=CARTESIAN_POINT('Ctrl Pts',(1.04212317001952,51.7136121578756,1.02900272514849));
#47645=CARTESIAN_POINT('Ctrl Pts',(1.0025589870473,51.710609230808,1.06759529338764));
#47646=CARTESIAN_POINT('Ctrl Pts',(0.960889782951117,51.7076063037405,1.10386732672915));
#47647=CARTESIAN_POINT('Ctrl Pts',(0.919262303182719,51.7046063835726,1.14010304005348));
#47648=CARTESIAN_POINT('Ctrl Pts',(0.87553437434542,51.7016064634047,1.17402247559887));
#47649=CARTESIAN_POINT('Ctrl Pts',(0.829996153126448,51.6986065432367,1.20537904237435));
#47650=CARTESIAN_POINT('Ctrl Pts',(0.784485480084899,51.6956084378594,1.23671664011147));
#47651=CARTESIAN_POINT('Ctrl Pts',(0.737167119800396,51.692610332482,1.26549414248036));
#47652=CARTESIAN_POINT('Ctrl Pts',(0.688362516843125,51.6896122271046,1.29150659905608));
#47653=CARTESIAN_POINT('Ctrl Pts',(0.639568094102268,51.686614747106,1.31751362965921));
#47654=CARTESIAN_POINT('Ctrl Pts',(0.58928851070837,51.6836172671073,1.34075651104833));
#47655=CARTESIAN_POINT('Ctrl Pts',(0.537870232273453,51.6806197871087,1.36107599465794));
#47656=CARTESIAN_POINT('Ctrl Pts',(0.486404398753673,51.6776195348388,1.3814142710937));
#47657=CARTESIAN_POINT('Ctrl Pts',(0.433798258887482,51.6746192825689,1.39882355260789));
#47658=CARTESIAN_POINT('Ctrl Pts',(0.380417316169004,51.671619030299,1.4131931628616));
#47659=CARTESIAN_POINT('Ctrl Pts',(0.327012409967135,51.6686174311722,1.42756922384284));
#47660=CARTESIAN_POINT('Ctrl Pts',(0.272832526168473,51.6656158320453,1.43890278480729));
#47661=CARTESIAN_POINT('Ctrl Pts',(0.218254094321258,51.6626142329184,1.44713420259215));
#47662=CARTESIAN_POINT('Ctrl Pts',(0.163570677532388,51.6596068600326,1.45538145401103));
#47663=CARTESIAN_POINT('Ctrl Pts',(0.108487709142944,51.6565994871467,1.46051459160544));
#47664=CARTESIAN_POINT('Ctrl Pts',(0.0533863500468608,51.6535921142609,
1.46252594767706));
#47665=CARTESIAN_POINT('Ctrl Pts',(0.0086393766485887,51.6511498726043,
1.46415933926862));
#47666=CARTESIAN_POINT('Ctrl Pts',(-0.0361195599308845,51.6487076309477,
1.46373498102298));
#47667=CARTESIAN_POINT('Ctrl Pts',(-0.0806887268960853,51.6462653892911,
1.46127395766567));
#47668=CARTESIAN_POINT('Ctrl Pts',(-0.135588642225334,51.6432570570899,
1.45824249032761));
#47669=CARTESIAN_POINT('Ctrl Pts',(-0.190434558441944,51.6402487248887,
1.45210637508921));
#47670=CARTESIAN_POINT('Ctrl Pts',(-0.244847220686593,51.6372403926875,
1.44287285944467));
#47671=CARTESIAN_POINT('Ctrl Pts',(-0.299162118801187,51.6342374656065,
1.43365593381039));
#47672=CARTESIAN_POINT('Ctrl Pts',(-0.353044790576555,51.6312345385255,
1.42135273906261));
#47673=CARTESIAN_POINT('Ctrl Pts',(-0.406119858537471,51.6282316114445,
1.4060223719776));
#47674=CARTESIAN_POINT('Ctrl Pts',(-0.459141781213952,51.6252316912634,
1.39070735554121));
#47675=CARTESIAN_POINT('Ctrl Pts',(-0.511357196357732,51.6222317710822,
1.37237131696433));
#47676=CARTESIAN_POINT('Ctrl Pts',(-0.562401550999693,51.6192318509011,
1.35112425240358));
#47677=CARTESIAN_POINT('Ctrl Pts',(-0.613415026545028,51.6162337455108,
1.32989004117723));
#47678=CARTESIAN_POINT('Ctrl Pts',(-0.663258358355904,51.6132356401204,
1.30574849693959));
#47679=CARTESIAN_POINT('Ctrl Pts',(-0.711585003397819,51.6102375347301,
1.27885848823837));
#47680=CARTESIAN_POINT('Ctrl Pts',(-0.759901567916541,51.6072400547188,
1.25197408856207));
#47681=CARTESIAN_POINT('Ctrl Pts',(-0.806701611939131,51.6042425747075,
1.22234261976295));
#47682=CARTESIAN_POINT('Ctrl Pts',(-0.851663413638878,51.6012450946962,
1.19016876108768));
#47683=CARTESIAN_POINT('Ctrl Pts',(-0.896666799031075,51.5982448424141,
1.1579651458681));
#47684=CARTESIAN_POINT('Ctrl Pts',(-0.939828114034045,51.5952445901321,
1.12321475098883));
#47685=CARTESIAN_POINT('Ctrl Pts',(-0.980856114933589,51.5922443378501,
1.08616459700977));
#47686=CARTESIAN_POINT('Ctrl Pts',(-1.02190253389697,51.5892427387113,1.04909781067996));
#47687=CARTESIAN_POINT('Ctrl Pts',(-1.06081335713255,51.5862411395726,1.00972958400529));
#47688=CARTESIAN_POINT('Ctrl Pts',(-1.09733428667997,51.5832395404339,0.968343799110916));
#47689=CARTESIAN_POINT('Ctrl Pts',(-1.13392546645469,51.5802321675368,0.926878406144349));
#47690=CARTESIAN_POINT('Ctrl Pts',(-1.16811724047725,51.5772247946397,0.883388118469462));
#47691=CARTESIAN_POINT('Ctrl Pts',(-1.19969640843694,51.5742174217426,0.838188986794449));
#47692=CARTESIAN_POINT('Ctrl Pts',(-1.22534136797843,51.5717751801874,0.801483462931507));
#47693=CARTESIAN_POINT('Ctrl Pts',(-1.2492641189705,51.5693329386321,0.76365167332456));
#47694=CARTESIAN_POINT('Ctrl Pts',(-1.27137294561791,51.5668906970769,0.724874529246846));
#47695=CARTESIAN_POINT('Ctrl Pts',(-1.2997668503311,51.5637541772103,0.675073852279607));
#47696=CARTESIAN_POINT('Ctrl Pts',(-1.32528023419885,51.5606176573437,0.623516209451306));
#47697=CARTESIAN_POINT('Ctrl Pts',(-1.34770252112457,51.5574811374771,0.570552508148441));
#47698=CARTESIAN_POINT('Ctrl Pts',(-1.37006162486433,51.5543534559292,0.517738051898046));
#47699=CARTESIAN_POINT('Ctrl Pts',(-1.38934677995713,51.5512257743813,0.463525844821878));
#47700=CARTESIAN_POINT('Ctrl Pts',(-1.40539355836495,51.5480980928334,0.408290578027837));
#47701=CARTESIAN_POINT('Ctrl Pts',(-1.42141300606684,51.5449757383202,0.353149387365186));
#47702=CARTESIAN_POINT('Ctrl Pts',(-1.43420490088096,51.5418533838069,0.296989040883462));
#47703=CARTESIAN_POINT('Ctrl Pts',(-1.44365328872406,51.5387310292937,0.240202897476707));
#47704=CARTESIAN_POINT('Ctrl Pts',(-1.45308371483079,51.5356146104924,0.183524706638624));
#47705=CARTESIAN_POINT('Ctrl Pts',(-1.45918319990495,51.5324981916911,0.12622354192248));
#47706=CARTESIAN_POINT('Ctrl Pts',(-1.4618864308277,51.5293817728898,0.0687045366903423));
#47707=CARTESIAN_POINT('Ctrl Pts',(-1.46296397147466,51.5281395305409,0.0457767632662445));
#47708=CARTESIAN_POINT('Ctrl Pts',(-1.46350244379955,51.5268972881919,0.0228144961225602));
#47709=CARTESIAN_POINT('Ctrl Pts',(-1.46349999166121,51.5256550458429,-0.00015622947666356));
#47710=CARTESIAN_POINT('Origin',(0.,55.715,0.));
#47711=CARTESIAN_POINT('',(-1.46349942146382,50.9543449542045,-0.00130129745633658));
#47712=CARTESIAN_POINT('',(-1.46349947235337,51.0256550458841,-0.00124274752362485));
#47713=CARTESIAN_POINT('',(-1.4635,55.715,-1.79227059055215E-16));
#47714=CARTESIAN_POINT('Ctrl Pts',(-1.46349942146382,50.9543449542045,-0.00130129745634145));
#47715=CARTESIAN_POINT('Ctrl Pts',(-1.46354775243707,50.9573044486033,0.0530539547187437));
#47716=CARTESIAN_POINT('Ctrl Pts',(-1.4605636570072,50.9602639430021,0.107505650961708));
#47717=CARTESIAN_POINT('Ctrl Pts',(-1.45454150093415,50.963223437401,0.161682627577081));
#47718=CARTESIAN_POINT('Ctrl Pts',(-1.44852471886776,50.9661802908283,0.215811258146704));
#47719=CARTESIAN_POINT('Ctrl Pts',(-1.4394753011775,50.9691371442556,0.269665114545852));
#47720=CARTESIAN_POINT('Ctrl Pts',(-1.42743962380975,50.972093997683,0.322875162218907));
#47721=CARTESIAN_POINT('Ctrl Pts',(-1.41540959591354,50.9750494631818,0.376060233429001));
#47722=CARTESIAN_POINT('Ctrl Pts',(-1.40039620510289,50.9780049286807,0.428601563323481));
#47723=CARTESIAN_POINT('Ctrl Pts',(-1.38249699180053,50.9809603941795,0.480139893846038));
#47724=CARTESIAN_POINT('Ctrl Pts',(-1.36405759284825,50.9840050535454,0.53323361488209));
#47725=CARTESIAN_POINT('Ctrl Pts',(-1.3425554930314,50.9870497129113,0.5852622190069));
#47726=CARTESIAN_POINT('Ctrl Pts',(-1.31815189464282,50.9900943722772,0.635852052485128));
#47727=CARTESIAN_POINT('Ctrl Pts',(-1.29443999713118,50.9930527331587,0.685007956768811));
#47728=CARTESIAN_POINT('Ctrl Pts',(-1.26798925696604,50.9960110940403,0.732805119962041));
#47729=CARTESIAN_POINT('Ctrl Pts',(-1.23899417013095,50.9989694549218,0.778925989026888));
#47730=CARTESIAN_POINT('Ctrl Pts',(-1.20873035773429,51.0020572635299,0.827064949150997));
#47731=CARTESIAN_POINT('Ctrl Pts',(-1.17569472915931,51.0051450721379,0.873376958923684));
#47732=CARTESIAN_POINT('Ctrl Pts',(-1.14015637285819,51.008232880746,0.917537844140967));
#47733=CARTESIAN_POINT('Ctrl Pts',(-1.10461801655707,51.011320689354,0.961698729358252));
#47734=CARTESIAN_POINT('Ctrl Pts',(-1.0665774408942,51.0144084979621,1.00370805193639));
#47735=CARTESIAN_POINT('Ctrl Pts',(-1.02634574315155,51.0174963065702,1.04328647336899));
#47736=CARTESIAN_POINT('Ctrl Pts',(-0.987149488474935,51.0205046442587,
1.08184626510569));
#47737=CARTESIAN_POINT('Ctrl Pts',(-0.945693589253863,51.0235129819473,
1.11827630448752));
#47738=CARTESIAN_POINT('Ctrl Pts',(-0.902238692061223,51.0265213196358,
1.15230099910902));
#47739=CARTESIAN_POINT('Ctrl Pts',(-0.858861867268464,51.0295242524527,
1.18626456392156));
#47740=CARTESIAN_POINT('Ctrl Pts',(-0.813493584401582,51.0325271852696,
1.21783103629103));
#47741=CARTESIAN_POINT('Ctrl Pts',(-0.766430224103125,51.0355301180865,
1.24676259230907));
#47742=CARTESIAN_POINT('Ctrl Pts',(-0.719413987022348,51.0385300441513,
1.27566517997459));
#47743=CARTESIAN_POINT('Ctrl Pts',(-0.670706482677944,51.0415299702161,
1.30193780161427));
#47744=CARTESIAN_POINT('Ctrl Pts',(-0.620634447017156,51.0445298962809,
1.32538490001045));
#47745=CARTESIAN_POINT('Ctrl Pts',(-0.570592699902108,51.0475280076922,
1.34881781527022));
#47746=CARTESIAN_POINT('Ctrl Pts',(-0.5191885353183,51.0505261191034,1.36942837083828));
#47747=CARTESIAN_POINT('Ctrl Pts',(-0.466772708834034,51.0535242305147,
1.38706722558344));
#47748=CARTESIAN_POINT('Ctrl Pts',(-0.414367813600106,51.0565217166738,
1.40470240176909));
#47749=CARTESIAN_POINT('Ctrl Pts',(-0.360952176354885,51.0595192028329,
1.41936693908409));
#47750=CARTESIAN_POINT('Ctrl Pts',(-0.306893723269394,51.062516688992,1.43096068870457));
#47751=CARTESIAN_POINT('Ctrl Pts',(-0.252785270710211,51.0655169475711,
1.44256516155788));
#47752=CARTESIAN_POINT('Ctrl Pts',(-0.19803333262019,51.0685172061501,1.45109306056883));
#47753=CARTESIAN_POINT('Ctrl Pts',(-0.143016632303413,51.0715174647291,
1.45649527733));
#47754=CARTESIAN_POINT('Ctrl Pts',(-0.0879752325467467,51.0745190702574,
1.46189991938616));
#47755=CARTESIAN_POINT('Ctrl Pts',(-0.0326693630243806,51.0775206757857,
1.46417605998132));
#47756=CARTESIAN_POINT('Ctrl Pts',(0.0225198617747103,51.0805222813141,
1.4633267255899));
#47757=CARTESIAN_POINT('Ctrl Pts',(0.0778152475168805,51.0835296606737,
1.46247575743499));
#47758=CARTESIAN_POINT('Ctrl Pts',(0.132993011308516,51.0865370400333,1.45848734130476));
#47759=CARTESIAN_POINT('Ctrl Pts',(0.187675912787505,51.0895444193929,1.45141655005011));
#47760=CARTESIAN_POINT('Ctrl Pts',(0.23208208519796,51.0919866125234,1.44567459475806));
#47761=CARTESIAN_POINT('Ctrl Pts',(0.276161922100405,51.0944288056539,1.4379009804281));
#47762=CARTESIAN_POINT('Ctrl Pts',(0.319719910248125,51.0968709987844,1.42814965216917));
#47763=CARTESIAN_POINT('Ctrl Pts',(0.373375188595168,51.0998793230382,1.41613784321666));
#47764=CARTESIAN_POINT('Ctrl Pts',(0.426467031557936,51.1028876472921,1.40107248196408));
#47765=CARTESIAN_POINT('Ctrl Pts',(0.478622532392679,51.1058959715459,1.38302303722173));
#47766=CARTESIAN_POINT('Ctrl Pts',(0.530684320895155,51.1088988904815,1.36500602348926));
#47767=CARTESIAN_POINT('Ctrl Pts',(0.581812610201623,51.1119018094171,1.34401573773514));
#47768=CARTESIAN_POINT('Ctrl Pts',(0.631646838239741,51.1149047283526,1.32017215610001));
#47769=CARTESIAN_POINT('Ctrl Pts',(0.681431164075527,51.1179046402732,1.29635245056935));
#47770=CARTESIAN_POINT('Ctrl Pts',(0.729923520747108,51.1209045521939,1.26968533580423));
#47771=CARTESIAN_POINT('Ctrl Pts',(0.776782387469093,51.1239044641145,1.24033921671364));
#47772=CARTESIAN_POINT('Ctrl Pts',(0.823612905445474,51.126902561144,1.21101085148103));
#47773=CARTESIAN_POINT('Ctrl Pts',(0.868811444729117,51.1299006581735,1.17900697421605));
#47774=CARTESIAN_POINT('Ctrl Pts',(0.912062280534688,51.1328987552031,1.14454123841208));
#47775=CARTESIAN_POINT('Ctrl Pts',(0.955304093326832,51.1358962267679,1.11008269286909));
#47776=CARTESIAN_POINT('Ctrl Pts',(0.996598596050201,51.1388936983328,1.0731636379759));
#47777=CARTESIAN_POINT('Ctrl Pts',(1.03566207553139,51.1418911698976,1.03403883645926));
#47778=CARTESIAN_POINT('Ctrl Pts',(1.07476168278522,51.1448914136674,0.994877850456428));
#47779=CARTESIAN_POINT('Ctrl Pts',(1.11162576951702,51.1478916574373,0.953507416879683));
#47780=CARTESIAN_POINT('Ctrl Pts',(1.14600764409953,51.1508919012071,0.910219055868122));
#47781=CARTESIAN_POINT('Ctrl Pts',(1.1804049526737,51.1538934917835,0.866911262751374));
#47782=CARTESIAN_POINT('Ctrl Pts',(1.21231752230337,51.15689508236,0.821684258810234));
#47783=CARTESIAN_POINT('Ctrl Pts',(1.2415411621936,51.1598966729364,0.774859853508333));
#47784=CARTESIAN_POINT('Ctrl Pts',(1.27082101594373,51.1629040372972,0.727945377956145));
#47785=CARTESIAN_POINT('Ctrl Pts',(1.2974013515941,51.1659114016579,0.679427827356803));
#47786=CARTESIAN_POINT('Ctrl Pts',(1.3211238034719,51.1689187660186,0.629653989028841));
#47787=CARTESIAN_POINT('Ctrl Pts',(1.34038902537399,51.1713610743452,0.589232195984588));
#47788=CARTESIAN_POINT('Ctrl Pts',(1.35777027111542,51.1738033826719,0.54798240600597));
#47789=CARTESIAN_POINT('Ctrl Pts',(1.37320679552036,51.1762456909985,0.506098159191196));
#47790=CARTESIAN_POINT('Ctrl Pts',(1.39222087281822,51.179254026171,0.454506862756334));
#47791=CARTESIAN_POINT('Ctrl Pts',(1.40836402779826,51.1822623613435,0.401732519203797));
#47792=CARTESIAN_POINT('Ctrl Pts',(1.4214923408129,51.185270696516,0.348126090677296));
#47793=CARTESIAN_POINT('Ctrl Pts',(1.43459706619233,51.1882736266137,0.294615976801396));
#47794=CARTESIAN_POINT('Ctrl Pts',(1.44469757393154,51.1912765567115,0.240277254096569));
#47795=CARTESIAN_POINT('Ctrl Pts',(1.4516990716003,51.1942794868093,0.185477911123728));
#47796=CARTESIAN_POINT('Ctrl Pts',(1.45869355857537,51.1972794100328,0.130733439469351));
#47797=CARTESIAN_POINT('Ctrl Pts',(1.46259511539236,51.2002793332563,0.0755297831083064));
#47798=CARTESIAN_POINT('Ctrl Pts',(1.46335996314126,51.2032792564798,0.0202452037584424));
#47799=CARTESIAN_POINT('Ctrl Pts',(1.46412434820389,51.2062773649326,-0.0350059317910204));
#47800=CARTESIAN_POINT('Ctrl Pts',(1.4617557775826,51.2092754733855,-0.0903373655677598));
#47801=CARTESIAN_POINT('Ctrl Pts',(1.45626247824288,51.2122735818383,-0.145367962295394));
#47802=CARTESIAN_POINT('Ctrl Pts',(1.45077032473011,51.2152710649268,-0.200387080394777));
#47803=CARTESIAN_POINT('Ctrl Pts',(1.44215478914101,51.2182685480153,-0.255104960072816));
#47804=CARTESIAN_POINT('Ctrl Pts',(1.43047599846893,51.2212660311038,-0.309145059485551));
#47805=CARTESIAN_POINT('Ctrl Pts',(1.41878640648588,51.2242662864611,-0.363235138723685));
#47806=CARTESIAN_POINT('Ctrl Pts',(1.4040280106138,51.2272665418184,-0.416645667089213));
#47807=CARTESIAN_POINT('Ctrl Pts',(1.38631189953782,51.2302667971757,-0.469011265536161));
#47808=CARTESIAN_POINT('Ctrl Pts',(1.36858783542824,51.2332683993936,-0.521400371702286));
#47809=CARTESIAN_POINT('Ctrl Pts',(1.34790360719099,51.2362700016115,-0.572743121336616));
#47810=CARTESIAN_POINT('Ctrl Pts',(1.32441880362076,51.2392716038293,-0.622693409805949));
#47811=CARTESIAN_POINT('Ctrl Pts',(1.30088882590766,51.2422789797726,-0.672739780044094));
#47812=CARTESIAN_POINT('Ctrl Pts',(1.27454776293348,51.2452863557159,-0.72138787160505));
#47813=CARTESIAN_POINT('Ctrl Pts',(1.24560104472301,51.2482937316593,-0.768316528121675));
#47814=CARTESIAN_POINT('Ctrl Pts',(1.22209411576546,51.2507359488437,-0.806426153772103));
#47815=CARTESIAN_POINT('Ctrl Pts',(1.1968697725791,51.2531781660282,-0.8434022913186));
#47816=CARTESIAN_POINT('Ctrl Pts',(1.17005764014261,51.2556203832127,-0.879088942453439));
#47817=CARTESIAN_POINT('Ctrl Pts',(1.13703035115398,51.2586287158366,-0.923047898081409));
#47818=CARTESIAN_POINT('Ctrl Pts',(1.10145188110206,51.2616370484605,-0.96523675864193));
#47819=CARTESIAN_POINT('Ctrl Pts',(1.06353900112097,51.2646453810844,-1.00534424109089));
#47820=CARTESIAN_POINT('Ctrl Pts',(1.025694239492,51.2676483086148,-1.04537966212922));
#47821=CARTESIAN_POINT('Ctrl Pts',(0.985523751349286,51.2706512361452,-1.08334074485816));
#47822=CARTESIAN_POINT('Ctrl Pts',(0.943285260418776,51.2736541636756,-1.11894824164332));
#47823=CARTESIAN_POINT('Ctrl Pts',(0.901089063627699,51.2766540843221,-1.15452008401942));
#47824=CARTESIAN_POINT('Ctrl Pts',(0.856829368080939,51.2796540049687,-1.18774266942952));
#47825=CARTESIAN_POINT('Ctrl Pts',(0.810800199953619,51.2826539256153,-1.21837403360182));
#47826=CARTESIAN_POINT('Ctrl Pts',(0.764798876766984,51.2856520314862,-1.2489868675996));
#47827=CARTESIAN_POINT('Ctrl Pts',(0.717030641866566,51.2886501373571,-1.2770112946511));
#47828=CARTESIAN_POINT('Ctrl Pts',(0.667820145829448,51.2916482432281,-1.30224748140449));
#47829=CARTESIAN_POINT('Ctrl Pts',(0.618619914441686,51.2946457237343,-1.32747840422784));
#47830=CARTESIAN_POINT('Ctrl Pts',(0.567978489586788,51.2976432042406,-1.34992200033207));
#47831=CARTESIAN_POINT('Ctrl Pts',(0.516244815862946,51.3006406847469,-1.36942452880567));
#47832=CARTESIAN_POINT('Ctrl Pts',(0.464463295053354,51.3036409375424,-1.3889450946442));
#47833=CARTESIAN_POINT('Ctrl Pts',(0.411588002911127,51.3066411903379,-1.40551897085507));
#47834=CARTESIAN_POINT('Ctrl Pts',(0.357986150186023,51.3096414431334,-1.41904128420388));
#47835=CARTESIAN_POINT('Ctrl Pts',(0.304360234619387,51.3126430427967,-1.43256966796381));
#47836=CARTESIAN_POINT('Ctrl Pts',(0.250007628546447,51.3156446424599,-1.44304365767043));
#47837=CARTESIAN_POINT('Ctrl Pts',(0.195305659078757,51.3186462421232,-1.45040957992279));
#47838=CARTESIAN_POINT('Ctrl Pts',(0.140498466852667,51.3216536155566,-1.45778967100061));
#47839=CARTESIAN_POINT('Ctrl Pts',(0.085341097405475,51.32466098899,-1.46204970956164));
#47840=CARTESIAN_POINT('Ctrl Pts',(0.0302147853571012,51.3276683624233,
-1.46318806608919));
#47841=CARTESIAN_POINT('Ctrl Pts',(-0.0145523706873162,51.3301106000912,
-1.46411250638656));
#47842=CARTESIAN_POINT('Ctrl Pts',(-0.0592988958543302,51.3325528377591,
-1.46297927242488));
#47843=CARTESIAN_POINT('Ctrl Pts',(-0.103823417662204,51.334995075427,-1.45981264138414));
#47844=CARTESIAN_POINT('Ctrl Pts',(-0.158668410827807,51.3380034066288,
-1.45591200751464));
#47845=CARTESIAN_POINT('Ctrl Pts',(-0.21341023872285,51.3410117378307,-1.44890797275119));
#47846=CARTESIAN_POINT('Ctrl Pts',(-0.267669809080525,51.3440200690326,
-1.4388137903519));
#47847=CARTESIAN_POINT('Ctrl Pts',(-0.321831889869015,51.3470229950882,
-1.42873774443041));
#47848=CARTESIAN_POINT('Ctrl Pts',(-0.375512916934494,51.3500259211439,
-1.4155826645423));
#47849=CARTESIAN_POINT('Ctrl Pts',(-0.428338496100367,51.3530288471995,
-1.39941358531296));
#47850=CARTESIAN_POINT('Ctrl Pts',(-0.481111179516009,51.3560287663401,
-1.38326069664111));
#47851=CARTESIAN_POINT('Ctrl Pts',(-0.533029608593966,51.3590286854808,
-1.36409994071798));
#47852=CARTESIAN_POINT('Ctrl Pts',(-0.583731018456037,51.3620286046214,
-1.34204707372442));
#47853=CARTESIAN_POINT('Ctrl Pts',(-0.634401756449242,51.3650267089579,
-1.32000754763492));
#47854=CARTESIAN_POINT('Ctrl Pts',(-0.683856450380088,51.3680248132945,
-1.29507958848854));
#47855=CARTESIAN_POINT('Ctrl Pts',(-0.731751117097538,51.371022917631,-1.26742753348131));
#47856=CARTESIAN_POINT('Ctrl Pts',(-0.77963579321242,51.374020396577,-1.23978124656289));
#47857=CARTESIAN_POINT('Ctrl Pts',(-0.825960630477322,51.3770178755231,
-1.20941225633633));
#47858=CARTESIAN_POINT('Ctrl Pts',(-0.870407189400394,51.3800153544691,
-1.17653031182376));
#47859=CARTESIAN_POINT('Ctrl Pts',(-0.914894855361113,51.3830156056766,
-1.14361795597308));
#47860=CARTESIAN_POINT('Ctrl Pts',(-0.957500345878216,51.386015856884,-1.10818831725159));
#47861=CARTESIAN_POINT('Ctrl Pts',(-0.997936366369565,51.3890161080915,
-1.070492997958));
#47862=CARTESIAN_POINT('Ctrl Pts',(-1.03839053908992,51.3920177061488,-1.03278075677002));
#47863=CARTESIAN_POINT('Ctrl Pts',(-1.07667293382798,51.395019304206,-0.99280119012461));
#47864=CARTESIAN_POINT('Ctrl Pts',(-1.11253378095445,51.3980209022633,-0.950842172095447));
#47865=CARTESIAN_POINT('Ctrl Pts',(-1.1484636086523,51.4010282740812,-0.908802443283636));
#47866=CARTESIAN_POINT('Ctrl Pts',(-1.18196226166673,51.4040356458992,-0.864776078176582));
#47867=CARTESIAN_POINT('Ctrl Pts',(-1.21282157236841,51.4070430177172,-0.819082464467298));
#47868=CARTESIAN_POINT('Ctrl Pts',(-1.23788204222071,51.4094852676918,-0.78197523806571));
#47869=CARTESIAN_POINT('Ctrl Pts',(-1.26120266896233,51.4119275176664,-0.743769156872513));
#47870=CARTESIAN_POINT('Ctrl Pts',(-1.28269461278464,51.4143697676411,-0.704646564125072));
#47871=CARTESIAN_POINT('Ctrl Pts',(-1.31048195579659,51.4175273990925,-0.654064219727654));
#47872=CARTESIAN_POINT('Ctrl Pts',(-1.33532006112789,51.420685030544,-0.601751349239927));
#47873=CARTESIAN_POINT('Ctrl Pts',(-1.3570020772859,51.4238426619954,-0.548067160338722));
#47874=CARTESIAN_POINT('Ctrl Pts',(-1.3786187933309,51.4269907835522,-0.494544653062373));
#47875=CARTESIAN_POINT('Ctrl Pts',(-1.39709816577733,51.4301389051089,-0.439659463057376));
#47876=CARTESIAN_POINT('Ctrl Pts',(-1.41227996488216,51.4332870266657,-0.383793630474047));
#47877=CARTESIAN_POINT('Ctrl Pts',(-1.42743363924789,51.4364293162326,-0.32803129102451));
#47878=CARTESIAN_POINT('Ctrl Pts',(-1.43930175669946,51.4395716057996,-0.271292351947302));
#47879=CARTESIAN_POINT('Ctrl Pts',(-1.44777284090111,51.4427138953665,-0.213976753758748));
#47880=CARTESIAN_POINT('Ctrl Pts',(-1.45622563919931,51.4458494019052,-0.156784878516293));
#47881=CARTESIAN_POINT('Ctrl Pts',(-1.46129592542497,51.4489849084439,-0.0990192666897063));
#47882=CARTESIAN_POINT('Ctrl Pts',(-1.46292302961044,51.4521204149826,-0.0410908680292959));
#47883=CARTESIAN_POINT('Ctrl Pts',(-1.46330782198311,51.4528619280408,-0.0273914342964181));
#47884=CARTESIAN_POINT('Ctrl Pts',(-1.46350027245807,51.4536034410989,-0.013682939758203));
#47885=CARTESIAN_POINT('Ctrl Pts',(-1.46349999971048,51.4543449541571,2.91106062376064E-5));
#47886=CARTESIAN_POINT('Ctrl Pts',(-1.46349999166114,51.5256550458102,-0.000156230081695943));
#47887=CARTESIAN_POINT('Ctrl Pts',(-1.46349371788756,51.5224767923979,-0.0589263944364653));
#47888=CARTESIAN_POINT('Ctrl Pts',(-1.45994303350198,51.5192985389856,-0.117616406012124));
#47889=CARTESIAN_POINT('Ctrl Pts',(-1.45290268375024,51.5161202855733,-0.175801142064967));
#47890=CARTESIAN_POINT('Ctrl Pts',(-1.44586580081156,51.5129435971984,-0.233957226756734));
#47891=CARTESIAN_POINT('Ctrl Pts',(-1.43534283904945,51.5097669088235,-0.291608116930657));
#47892=CARTESIAN_POINT('Ctrl Pts',(-1.42143930082676,51.5065902204486,-0.34834259582361));
#47893=CARTESIAN_POINT('Ctrl Pts',(-1.40748602039149,51.5034021669444,-0.405280051718877));
#47894=CARTESIAN_POINT('Ctrl Pts',(-1.39012810097255,51.5002141134403,-0.461294120731727));
#47895=CARTESIAN_POINT('Ctrl Pts',(-1.36952103538481,51.4970260599362,-0.515988743712996));
#47896=CARTESIAN_POINT('Ctrl Pts',(-1.34903054608504,51.4938560415784,-0.570373953590711));
#47897=CARTESIAN_POINT('Ctrl Pts',(-1.32532785188886,51.4906860232206,-0.623454270906817));
#47898=CARTESIAN_POINT('Ctrl Pts',(-1.29861052459124,51.4875160048627,-0.674865138691329));
#47899=CARTESIAN_POINT('Ctrl Pts',(-1.2732559103757,51.4845076727933,-0.723653803240071));
#47900=CARTESIAN_POINT('Ctrl Pts',(-1.24509392124162,51.4814993407239,-0.771115667504255));
#47901=CARTESIAN_POINT('Ctrl Pts',(-1.21428722872449,51.4784910086545,-0.81690805857));
#47902=CARTESIAN_POINT('Ctrl Pts',(-1.18353588709454,51.4754880817044,-0.862618173699423));
#47903=CARTESIAN_POINT('Ctrl Pts',(-1.15014956433339,51.4724851547543,-0.906664332828394));
#47904=CARTESIAN_POINT('Ctrl Pts',(-1.1143365921763,51.4694822278042,-0.94872873327254));
#47905=CARTESIAN_POINT('Ctrl Pts',(-1.07855948036464,51.4664823077533,-0.990751013673588));
#47906=CARTESIAN_POINT('Ctrl Pts',(-1.04036087335701,51.4634823877025,-1.03079506539789));
#47907=CARTESIAN_POINT('Ctrl Pts',(-0.999991038550154,51.4604824676516,
-1.06857389675183));
#47908=CARTESIAN_POINT('Ctrl Pts',(-0.959645625317653,51.4574843623906,
-1.10632987394886));
#47909=CARTESIAN_POINT('Ctrl Pts',(-0.917131972827282,51.4544862571297,
-1.14182298600698));
#47910=CARTESIAN_POINT('Ctrl Pts',(-0.872737479869535,51.4514881518688,
-1.17480276694898));
#47911=CARTESIAN_POINT('Ctrl Pts',(-0.828352247206295,51.4484906719858,
-1.20777566860339));
#47912=CARTESIAN_POINT('Ctrl Pts',(-0.782087377374449,51.4454931921028,
-1.23823596487485));
#47913=CARTESIAN_POINT('Ctrl Pts',(-0.734261807223034,51.4424957122199,
-1.26597466343271));
#47914=CARTESIAN_POINT('Ctrl Pts',(-0.686392004729485,51.4394954600635,
-1.29373901662681));
#47915=CARTESIAN_POINT('Ctrl Pts',(-0.636959076313892,51.4364952079071,
-1.31877647675021));
#47916=CARTESIAN_POINT('Ctrl Pts',(-0.586308007005538,51.4334949557508,
-1.34092325318088));
#47917=CARTESIAN_POINT('Ctrl Pts',(-0.535634199676096,51.4304933567364,
-1.36307997163008));
#47918=CARTESIAN_POINT('Ctrl Pts',(-0.483741658060411,51.4274917577221,
-1.38234323505235));
#47919=CARTESIAN_POINT('Ctrl Pts',(-0.430993759607402,51.4244901587077,
-1.39859809422846));
#47920=CARTESIAN_POINT('Ctrl Pts',(-0.378144397297677,51.4214827859314,
-1.41488422063512));
#47921=CARTESIAN_POINT('Ctrl Pts',(-0.324436905909344,51.418475413155,-1.42815025441349));
#47922=CARTESIAN_POINT('Ctrl Pts',(-0.270247069561249,51.4154680403787,
-1.43833194061509));
#47923=CARTESIAN_POINT('Ctrl Pts',(-0.226240311703689,51.4130257978019,
-1.44660033611968));
#47924=CARTESIAN_POINT('Ctrl Pts',(-0.181915769092783,51.4105835552252,
-1.4528356313487));
#47925=CARTESIAN_POINT('Ctrl Pts',(-0.13747606741555,51.4081413126484,-1.45702868224615));
#47926=CARTESIAN_POINT('Ctrl Pts',(-0.0827356464006351,51.4051329804179,
-1.46219364426886));
#47927=CARTESIAN_POINT('Ctrl Pts',(-0.0275870130885459,51.4021246481873,
-1.46428043842858));
#47928=CARTESIAN_POINT('Ctrl Pts',(0.0275937155764213,51.3991163159568,
-1.46323984256194));
#47929=CARTESIAN_POINT('Ctrl Pts',(0.0826753000794172,51.3961133888484,
-1.46220111635174));
#47930=CARTESIAN_POINT('Ctrl Pts',(0.137788341101494,51.39311046174,-1.45804616047742));
#47931=CARTESIAN_POINT('Ctrl Pts',(0.192552846829943,51.3901075346315,-1.45077760224567));
#47932=CARTESIAN_POINT('Ctrl Pts',(0.247262515580034,51.3871076144242,-1.44351632219099));
#47933=CARTESIAN_POINT('Ctrl Pts',(0.301623818697801,51.3841076942168,-1.43314768461669));
#47934=CARTESIAN_POINT('Ctrl Pts',(0.355259900639993,51.3811077740094,-1.41972625988155));
#47935=CARTESIAN_POINT('Ctrl Pts',(0.408863535607975,51.3781096685941,-1.40631295439388));
#47936=CARTESIAN_POINT('Ctrl Pts',(0.461742306892657,51.3751115631787,-1.38985064998074));
#47937=CARTESIAN_POINT('Ctrl Pts',(0.513529902161674,51.3721134577634,-1.37044492395201));
#47938=CARTESIAN_POINT('Ctrl Pts',(0.56530669496165,51.3691159777283,-1.35104324579909));
#47939=CARTESIAN_POINT('Ctrl Pts',(0.615992268706816,51.3661184976932,-1.3286995505863));
#47940=CARTESIAN_POINT('Ctrl Pts',(0.665238045064347,51.3631210176582,-1.30356840764072));
#47941=CARTESIAN_POINT('Ctrl Pts',(0.714529367186659,51.3601207653545,-1.27841402174499));
#47942=CARTESIAN_POINT('Ctrl Pts',(0.762377759096981,51.3571205130508,-1.25046727795835));
#47943=CARTESIAN_POINT('Ctrl Pts',(0.808458486331006,51.3541202607471,-1.21992914789318));
#47944=CARTESIAN_POINT('Ctrl Pts',(0.854559899853462,51.3511186615878,-1.18937730883068));
#47945=CARTESIAN_POINT('Ctrl Pts',(0.898891642411422,51.3481170624285,-1.15623208169307));
#47946=CARTESIAN_POINT('Ctrl Pts',(0.941160033911184,51.3451154632693,-1.12073638317327));
#47947=CARTESIAN_POINT('Ctrl Pts',(0.983509731200422,51.3421080903538,-1.08517240654568));
#47948=CARTESIAN_POINT('Ctrl Pts',(1.02378776191686,51.3391007174382,-1.04724928930633));
#47949=CARTESIAN_POINT('Ctrl Pts',(1.06173630385517,51.3360933445227,-1.00724786973017));
#47950=CARTESIAN_POINT('Ctrl Pts',(1.09255373201681,51.3336511031599,-0.974763331163288));
#47951=CARTESIAN_POINT('Ctrl Pts',(1.12183555220237,51.3312088617972,-0.940908981056737));
#47952=CARTESIAN_POINT('Ctrl Pts',(1.14946416948652,51.3287666204344,-0.905850083107941));
#47953=CARTESIAN_POINT('Ctrl Pts',(1.18349687119876,51.3257582877714,-0.862664823274632));
#47954=CARTESIAN_POINT('Ctrl Pts',(1.21516506212638,51.3227499551084,-0.817466891271791));
#47955=CARTESIAN_POINT('Ctrl Pts',(1.24422336847353,51.3197416224454,-0.770545559551409));
#47956=CARTESIAN_POINT('Ctrl Pts',(1.27322946531484,51.3167386949,-0.723708532109218));
#47957=CARTESIAN_POINT('Ctrl Pts',(1.29963470676274,51.3137357673545,-0.675154695503419));
#47958=CARTESIAN_POINT('Ctrl Pts',(1.32323517542342,51.3107328398091,-0.625204702895095));
#47959=CARTESIAN_POINT('Ctrl Pts',(1.34681201240667,51.3077329191622,-0.575304726332241));
#47960=CARTESIAN_POINT('Ctrl Pts',(1.36758941486602,51.3047329985153,-0.524011838713086));
#47961=CARTESIAN_POINT('Ctrl Pts',(1.38540880358005,51.3017330778685,-0.471672234674566));
#47962=CARTESIAN_POINT('Ctrl Pts',(1.40321741252416,51.2987349720119,-0.419364293276008));
#47963=CARTESIAN_POINT('Ctrl Pts',(1.41807138410431,51.2957368661553,-0.366011390038988));
#47964=CARTESIAN_POINT('Ctrl Pts',(1.42986070871547,51.2927387602988,-0.311978530786503));
#47965=CARTESIAN_POINT('Ctrl Pts',(1.4416475741738,51.2897412798216,-0.2579569423288));
#47966=CARTESIAN_POINT('Ctrl Pts',(1.45037094927048,51.2867437993444,-0.203256195905757));
#47967=CARTESIAN_POINT('Ctrl Pts',(1.45597160189233,51.2837463188673,-0.148252974617942));
#47968=CARTESIAN_POINT('Ctrl Pts',(1.46157743436492,51.2807460661236,-0.0931988827450114));
#47969=CARTESIAN_POINT('Ctrl Pts',(1.46405472000038,51.27774581338,-0.0378422843772192));
#47970=CARTESIAN_POINT('Ctrl Pts',(1.46339614283138,51.2747455606364,0.0174349977411516));
#47971=CARTESIAN_POINT('Ctrl Pts',(1.46273727001795,51.2717439610376,0.0727370945985477));
#47972=CARTESIAN_POINT('Ctrl Pts',(1.45893976440794,51.2687423614389,0.127959275605072));
#47973=CARTESIAN_POINT('Ctrl Pts',(1.45204839301903,51.2657407618402,0.182723053638169));
#47974=CARTESIAN_POINT('Ctrl Pts',(1.44514376568009,51.2627333884916,0.237592172954387));
#47975=CARTESIAN_POINT('Ctrl Pts',(1.43513347892081,51.2597260151431,0.292000606083937));
#47976=CARTESIAN_POINT('Ctrl Pts',(1.42211360828021,51.2567186417945,0.345579419445437));
#47977=CARTESIAN_POINT('Ctrl Pts',(1.41154038796423,51.2542764039364,0.389089882304661));
#47978=CARTESIAN_POINT('Ctrl Pts',(1.39898342387764,51.2518341660783,0.432053342607236));
#47979=CARTESIAN_POINT('Ctrl Pts',(1.38451776352351,51.2493919282201,0.474281364263733));
#47980=CARTESIAN_POINT('Ctrl Pts',(1.36669906659865,51.2463835971003,0.526297539205796));
#47981=CARTESIAN_POINT('Ctrl Pts',(1.34590692717192,51.2433752659804,0.577419073981439));
#47982=CARTESIAN_POINT('Ctrl Pts',(1.32225125853123,51.2403669348606,0.627282918078111));
#47983=CARTESIAN_POINT('Ctrl Pts',(1.2986380924074,51.2373640088572,0.677057171011373));
#47984=CARTESIAN_POINT('Ctrl Pts',(1.2721718315674,51.2343610828538,0.725577743591005));
#47985=CARTESIAN_POINT('Ctrl Pts',(1.24301123978448,51.2313581568505,0.772499390141801));
#47986=CARTESIAN_POINT('Ctrl Pts',(1.21387984715273,51.2283582377439,0.819374053001011));
#47987=CARTESIAN_POINT('Ctrl Pts',(1.18205974533812,51.2253583186373,0.86465251425162));
#47988=CARTESIAN_POINT('Ctrl Pts',(1.14775574875542,51.2223583995308,0.908013761569116));
#47989=CARTESIAN_POINT('Ctrl Pts',(1.11347250420261,51.2193602952101,0.951348777718505));
#47990=CARTESIAN_POINT('Ctrl Pts',(1.07670867038285,51.2163621908895,0.99276846463294));
#47991=CARTESIAN_POINT('Ctrl Pts',(1.03771121117154,51.2133640865689,1.03198240886601));
#47992=CARTESIAN_POINT('Ctrl Pts',(0.998721886411359,51.2103666076207,1.0711881734915));
#47993=CARTESIAN_POINT('Ctrl Pts',(0.957500234080089,51.2073691286724,1.10818873418212));
#47994=CARTESIAN_POINT('Ctrl Pts',(0.914330572024747,51.2043716497241,1.1427300009455));
#47995=CARTESIAN_POINT('Ctrl Pts',(0.871120983484007,51.2013713984864,1.17730321401833));
#47996=CARTESIAN_POINT('Ctrl Pts',(0.825960199223298,51.1983711472487,1.20941225728892));
#47997=CARTESIAN_POINT('Ctrl Pts',(0.779165016506029,51.195370896011,1.23884386710076));
#47998=CARTESIAN_POINT('Ctrl Pts',(0.732348826610749,51.1923692979078,1.26828868927829));
#47999=CARTESIAN_POINT('Ctrl Pts',(0.683897239400804,51.1893676998047,1.29505342568246));
#48000=CARTESIAN_POINT('Ctrl Pts',(0.634152502047362,51.1863661017016,1.3189703765237));
#48001=CARTESIAN_POINT('Ctrl Pts',(0.584312077181155,51.1833587298127,1.3429333333077));
#48002=CARTESIAN_POINT('Ctrl Pts',(0.533174022850266,51.1803513579239,1.36403735821174));
#48003=CARTESIAN_POINT('Ctrl Pts',(0.481100392408416,51.177343986035,1.38216303756991));
#48004=CARTESIAN_POINT('Ctrl Pts',(0.438812032622073,51.1749017360253,1.39688268057475));
#48005=CARTESIAN_POINT('Ctrl Pts',(0.395907127134563,51.1724594860157,1.40963905926866));
#48006=CARTESIAN_POINT('Ctrl Pts',(0.352584691729241,51.170017236006,1.4203930037698));
#48007=CARTESIAN_POINT('Ctrl Pts',(0.299220662541903,51.1670089032662,1.4336395768876));
#48008=CARTESIAN_POINT('Ctrl Pts',(0.244995284244615,51.1640005705265,1.44390289048352));
#48009=CARTESIAN_POINT('Ctrl Pts',(0.190273174697797,51.1609922377867,1.45107834695113));
#48010=CARTESIAN_POINT('Ctrl Pts',(0.135649385547883,51.1579893101833,1.45824091112102));
#48011=CARTESIAN_POINT('Ctrl Pts',(0.0805311562522271,51.15498638258,1.46232655952096));
#48012=CARTESIAN_POINT('Ctrl Pts',(0.0252946456500175,51.1519834549766,
1.46328139156535));
#48013=CARTESIAN_POINT('Ctrl Pts',(-0.0298865551868294,51.1489835342834,
1.4642352675114));
#48014=CARTESIAN_POINT('Ctrl Pts',(-0.0851852765983605,51.1459836135901,
1.4620645277722));
#48015=CARTESIAN_POINT('Ctrl Pts',(-0.140220738055422,51.1429836928969,
1.45676710376751));
#48016=CARTESIAN_POINT('Ctrl Pts',(-0.195222905814022,51.1399855870054,
1.4514728844391));
#48017=CARTESIAN_POINT('Ctrl Pts',(-0.249961603889136,51.136987481114,1.44305578014748));
#48018=CARTESIAN_POINT('Ctrl Pts',(-0.304058893854024,51.1339893752225,
1.43156572991542));
#48019=CARTESIAN_POINT('Ctrl Pts',(-0.358144899378313,51.1309918947219,
1.42007807645387));
#48020=CARTESIAN_POINT('Ctrl Pts',(-0.411589245401469,51.1279944142213,
1.40551885961797));
#48021=CARTESIAN_POINT('Ctrl Pts',(-0.464024246046617,51.1249969337206,
1.38798910265206));
#48022=CARTESIAN_POINT('Ctrl Pts',(-0.516507741708372,51.1219966809712,
1.37044313312117));
#48023=CARTESIAN_POINT('Ctrl Pts',(-0.567979524064569,51.1189964282218,
1.34992130211764));
#48024=CARTESIAN_POINT('Ctrl Pts',(-0.618088586797045,51.1159961754724,
1.3265740646007));
#48025=CARTESIAN_POINT('Ctrl Pts',(-0.668220144020035,51.1129945758776,
1.30321634626085));
#48026=CARTESIAN_POINT('Ctrl Pts',(-0.716987295275605,51.1099929762829,
1.27703094357738));
#48027=CARTESIAN_POINT('Ctrl Pts',(-0.764063506869514,51.1069913766881,
1.24821440765209));
#48028=CARTESIAN_POINT('Ctrl Pts',(-0.811230272020899,51.1039840033594,
1.21934244161138));
#48029=CARTESIAN_POINT('Ctrl Pts',(-0.85669916342403,51.1009766300307,1.18782953311385));
#48030=CARTESIAN_POINT('Ctrl Pts',(-0.900173468365905,51.097969256702,1.15391506483367));
#48031=CARTESIAN_POINT('Ctrl Pts',(-0.935478225094219,51.0955270190653,
1.12637369174438));
#48032=CARTESIAN_POINT('Ctrl Pts',(-0.969468115397339,51.0930847814285,
1.09724941745909));
#48033=CARTESIAN_POINT('Ctrl Pts',(-1.00200228000408,51.0906425437917,1.06668818352255));
#48034=CARTESIAN_POINT('Ctrl Pts',(-1.04146882826977,51.0876799138692,1.02961495822861));
#48035=CARTESIAN_POINT('Ctrl Pts',(-1.07897116203487,51.0847172839467,0.990257845560917));
#48036=CARTESIAN_POINT('Ctrl Pts',(-1.11422790346054,51.0817546540242,0.948856379622301));
#48037=CARTESIAN_POINT('Ctrl Pts',(-1.1494344329215,51.0787962434216,0.907513876845407));
#48038=CARTESIAN_POINT('Ctrl Pts',(-1.18240134639486,51.075837832819,0.864133192028604));
#48039=CARTESIAN_POINT('Ctrl Pts',(-1.21288281519522,51.0728794222163,0.818991774442275));
#48040=CARTESIAN_POINT('Ctrl Pts',(-1.24333380476329,51.0699239698072,0.773895494961382));
#48041=CARTESIAN_POINT('Ctrl Pts',(-1.27130396502406,51.0669685173981,0.727042417870797));
#48042=CARTESIAN_POINT('Ctrl Pts',(-1.29658827545769,51.064013064989,0.67874228831395));
#48043=CARTESIAN_POINT('Ctrl Pts',(-1.3218580231019,51.0610593148067,0.630469977772274));
#48044=CARTESIAN_POINT('Ctrl Pts',(-1.34444473358649,51.0581055646244,0.580752749081789));
#48045=CARTESIAN_POINT('Ctrl Pts',(-1.36418854276114,51.0551518144421,0.529926287137395));
#48046=CARTESIAN_POINT('Ctrl Pts',(-1.38393833124246,51.0521971697324,0.479084432671739));
#48047=CARTESIAN_POINT('Ctrl Pts',(-1.4008432919116,51.0492425250227,0.427133179797992));
#48048=CARTESIAN_POINT('Ctrl Pts',(-1.41479191016864,51.0462878803131,0.37442769785551));
#48049=CARTESIAN_POINT('Ctrl Pts',(-1.42874312731249,51.0433326850982,0.321712395902229));
#48050=CARTESIAN_POINT('Ctrl Pts',(-1.43973678590469,51.0403774898832,0.268243118242051));
#48051=CARTESIAN_POINT('Ctrl Pts',(-1.44771220919992,51.0374222946683,0.214386588511222));
#48052=CARTESIAN_POINT('Ctrl Pts',(-1.45569720330142,51.0344635531086,0.160465428930283));
#48053=CARTESIAN_POINT('Ctrl Pts',(-1.46065668292314,51.0315048115489,0.106156633517691));
#48054=CARTESIAN_POINT('Ctrl Pts',(-1.46258187645247,51.0285460699892,0.0518315027059542));
#48055=CARTESIAN_POINT('Ctrl Pts',(-1.46320892016773,51.0275823952875,0.0341375766995819));
#48056=CARTESIAN_POINT('Ctrl Pts',(-1.46351448948394,51.0266187205858,0.0164419086505343));
#48057=CARTESIAN_POINT('Ctrl Pts',(-1.46349947235337,51.0256550458841,-0.0012427475236237));
#48058=CARTESIAN_POINT('Origin',(0.,55.715,0.));
#48059=CARTESIAN_POINT('',(-1.46391036891612,50.4543447982886,0.00080102880736226));
#48060=CARTESIAN_POINT('',(-1.46349969347884,50.5256550458075,0.00094719973096371));
#48061=CARTESIAN_POINT('',(-1.4635,55.715,-1.79227059055215E-16));
#48062=CARTESIAN_POINT('Ctrl Pts',(-1.46349977934093,50.4543449541571,0.000803659790552031));
#48063=CARTESIAN_POINT('Ctrl Pts',(-1.46347455770472,50.4568544564617,0.0467333671772216));
#48064=CARTESIAN_POINT('Ctrl Pts',(-1.46128737451521,50.4593639587663,0.0926024254620283));
#48065=CARTESIAN_POINT('Ctrl Pts',(-1.45695412945267,50.4618734610709,0.138263931199737));
#48066=CARTESIAN_POINT('Ctrl Pts',(-1.45175846780538,50.4648824127202,0.193013138940129));
#48067=CARTESIAN_POINT('Ctrl Pts',(-1.44346142373346,50.4678913643695,0.247585534401134));
#48068=CARTESIAN_POINT('Ctrl Pts',(-1.43208529592634,50.4709003160188,0.301602312974477));
#48069=CARTESIAN_POINT('Ctrl Pts',(-1.42072960126165,50.4739038631633,0.355522069736163));
#48070=CARTESIAN_POINT('Ctrl Pts',(-1.4063059058018,50.4769074103078,0.408887677011401));
#48071=CARTESIAN_POINT('Ctrl Pts',(-1.38888816280316,50.4799109574523,0.461326263316182));
#48072=CARTESIAN_POINT('Ctrl Pts',(-1.37148785750537,50.4829114976081,0.513712350948678));
#48073=CARTESIAN_POINT('Ctrl Pts',(-1.35109960799791,50.4859120377639,0.565172756848002));
#48074=CARTESIAN_POINT('Ctrl Pts',(-1.32784779785606,50.4889125779197,0.615347443099267));
#48075=CARTESIAN_POINT('Ctrl Pts',(-1.30461006026922,50.4919113020764,0.665491762423053));
#48076=CARTESIAN_POINT('Ctrl Pts',(-1.27851241873977,50.494910026233,0.714351425691465));
#48077=CARTESIAN_POINT('Ctrl Pts',(-1.24972737818508,50.4979087503897,0.761586324860581));
#48078=CARTESIAN_POINT('Ctrl Pts',(-1.22094836304363,50.5009068468401,0.808811336609645));
#48079=CARTESIAN_POINT('Ctrl Pts',(-1.18948334077739,50.5039049432904,0.854411808402353));
#48080=CARTESIAN_POINT('Ctrl Pts',(-1.15554961053038,50.5069030397407,0.898074243925904));
#48081=CARTESIAN_POINT('Ctrl Pts',(-1.12158460055204,50.5099038998027,0.941776926992022));
#48082=CARTESIAN_POINT('Ctrl Pts',(-1.08514666077922,50.5129047598647,0.983537585944588));
#48083=CARTESIAN_POINT('Ctrl Pts',(-1.04649419523657,50.5159056199267,1.02307485030967));
#48084=CARTESIAN_POINT('Ctrl Pts',(-1.00782443070391,50.5189078230297,1.06262980965829));
#48085=CARTESIAN_POINT('Ctrl Pts',(-0.966938555633143,50.5219100261327,
1.09995903351445));
#48086=CARTESIAN_POINT('Ctrl Pts',(-0.92413035215595,50.5249122292358,1.13481951967003));
#48087=CARTESIAN_POINT('Ctrl Pts',(-0.881240022136062,50.5279201919956,
1.16974688485748));
#48088=CARTESIAN_POINT('Ctrl Pts',(-0.836420425108368,50.5309281547555,
1.20219573920285));
#48089=CARTESIAN_POINT('Ctrl Pts',(-0.789995868594206,50.5339361175154,
1.23196541250316));
#48090=CARTESIAN_POINT('Ctrl Pts',(-0.752378157990058,50.5363734627719,
1.25608770981902));
#48091=CARTESIAN_POINT('Ctrl Pts',(-0.713707314398565,50.5388108080285,
1.27845169181399));
#48092=CARTESIAN_POINT('Ctrl Pts',(-0.674166557648519,50.5412481532851,
1.29897332634213));
#48093=CARTESIAN_POINT('Ctrl Pts',(-0.625353734488048,50.5442570411458,
1.3243071590636));
#48094=CARTESIAN_POINT('Ctrl Pts',(-0.575007291188768,50.5472659290066,
1.34693952004985));
#48095=CARTESIAN_POINT('Ctrl Pts',(-0.523457587380063,50.5502748168673,
1.36668372501257));
#48096=CARTESIAN_POINT('Ctrl Pts',(-0.472000164466407,50.5532783184146,
1.38639258519596));
#48097=CARTESIAN_POINT('Ctrl Pts',(-0.419344245117153,50.5562818199619,
1.40322336171202));
#48098=CARTESIAN_POINT('Ctrl Pts',(-0.365843215951807,50.5592853215091,
1.41703598801937));
#48099=CARTESIAN_POINT('Ctrl Pts',(-0.312395551090045,50.5622858272305,
1.43083483699954));
#48100=CARTESIAN_POINT('Ctrl Pts',(-0.258104955463595,50.5652863329519,
1.44162136748116));
#48101=CARTESIAN_POINT('Ctrl Pts',(-0.203341378283216,50.5682868386733,
1.4493048450474));
#48102=CARTESIAN_POINT('Ctrl Pts',(-0.148610740738315,50.5712855396264,
1.45698370109396));
#48103=CARTESIAN_POINT('Ctrl Pts',(-0.0934082079420693,50.5742842405795,
1.46156313010151));
#48104=CARTESIAN_POINT('Ctrl Pts',(-0.0381130768592489,50.5772829415327,
1.46300363751165));
#48105=CARTESIAN_POINT('Ctrl Pts',(0.0171706881136775,50.5802810260922,
1.4644438488204));
#48106=CARTESIAN_POINT('Ctrl Pts',(0.0725464854021787,50.5832791106517,
1.46274640593892));
#48107=CARTESIAN_POINT('Ctrl Pts',(0.127633088951927,50.5862771952113,1.45792388162228));
#48108=CARTESIAN_POINT('Ctrl Pts',(0.182770798663487,50.5892780612201,1.45309688324677));
#48109=CARTESIAN_POINT('Ctrl Pts',(0.237618250753981,50.592278927229,1.44513905673968));
#48110=CARTESIAN_POINT('Ctrl Pts',(0.291798921557676,50.5952797932378,1.43411493241573));
#48111=CARTESIAN_POINT('Ctrl Pts',(0.34600401928565,50.5982820121632,1.42308583795305));
#48112=CARTESIAN_POINT('Ctrl Pts',(0.399541224279997,50.6012842310886,1.40898782469742));
#48113=CARTESIAN_POINT('Ctrl Pts',(0.452047068900792,50.604286450014,1.39193595308771));
#48114=CARTESIAN_POINT('Ctrl Pts',(0.50465392915194,50.6072944448876,1.37485127550046));
#48115=CARTESIAN_POINT('Ctrl Pts',(0.556224970783227,50.6103024397611,1.35480157811856));
#48116=CARTESIAN_POINT('Ctrl Pts',(0.60641574197187,50.6133104346347,1.33195052381412));
#48117=CARTESIAN_POINT('Ctrl Pts',(0.647086859661879,50.6157479049229,1.31343361528798));
#48118=CARTESIAN_POINT('Ctrl Pts',(0.686851949166193,50.6181853752111,1.29307821329013));
#48119=CARTESIAN_POINT('Ctrl Pts',(0.725541042079325,50.6206228454993,1.27099270110353));
#48120=CARTESIAN_POINT('Ctrl Pts',(0.773283808923846,50.6236307106855,1.24373893577659));
#48121=CARTESIAN_POINT('Ctrl Pts',(0.819590948990178,50.6266385758717,1.21373305763258));
#48122=CARTESIAN_POINT('Ctrl Pts',(0.864126513841084,50.6296464410579,1.18115097175461));
#48123=CARTESIAN_POINT('Ctrl Pts',(0.90858189309974,50.6326488906296,1.1486275494158));
#48124=CARTESIAN_POINT('Ctrl Pts',(0.951271603300684,50.6356513402013,1.11353743357303));
#48125=CARTESIAN_POINT('Ctrl Pts',(0.991886332749048,50.638653789773,1.07610118153715));
#48126=CARTESIAN_POINT('Ctrl Pts',(1.03246030521508,50.6416532263791,1.03870249687359));
#48127=CARTESIAN_POINT('Ctrl Pts',(1.07096303435184,50.6446526629852,0.998962696223431));
#48128=CARTESIAN_POINT('Ctrl Pts',(1.10711763680155,50.6476520995912,0.957143034390863));
#48129=CARTESIAN_POINT('Ctrl Pts',(1.14325030143847,50.6506497162055,0.915348747803772));
#48130=CARTESIAN_POINT('Ctrl Pts',(1.17703731783404,50.6536473328198,0.871477500586006));
#48131=CARTESIAN_POINT('Ctrl Pts',(1.20823975515763,50.6566449494341,0.825826219041649));
#48132=CARTESIAN_POINT('Ctrl Pts',(1.23943563764072,50.6596419363252,0.780184527673417));
#48133=CARTESIAN_POINT('Ctrl Pts',(1.26804772071684,50.6626389232163,0.732763980984989));
#48134=CARTESIAN_POINT('Ctrl Pts',(1.29387975260718,50.6656359101074,0.683891391810999));
#48135=CARTESIAN_POINT('Ctrl Pts',(1.31973565535281,50.6686356664531,0.63497364047133));
#48136=CARTESIAN_POINT('Ctrl Pts',(1.34280612603492,50.6716354227989,0.584601634386629));
#48137=CARTESIAN_POINT('Ctrl Pts',(1.36294110295681,50.6746351791446,0.533126438915635));
#48138=CARTESIAN_POINT('Ctrl Pts',(1.38308510443959,50.6776362799907,0.481628172097829));
#48139=CARTESIAN_POINT('Ctrl Pts',(1.40029082451669,50.6806373808368,0.429026233991788));
#48140=CARTESIAN_POINT('Ctrl Pts',(1.41445772863024,50.6836384816829,0.375688147162209));
#48141=CARTESIAN_POINT('Ctrl Pts',(1.4286518996745,50.6866453587246,0.322247400929708));
#48142=CARTESIAN_POINT('Ctrl Pts',(1.43979546294892,50.6896522357662,0.268068194976788));
#48143=CARTESIAN_POINT('Ctrl Pts',(1.44783902743882,50.6926591128079,0.213528453900192));
#48144=CARTESIAN_POINT('Ctrl Pts',(1.45438259331181,50.6951052544431,0.169159519097881));
#48145=CARTESIAN_POINT('Ctrl Pts',(1.45887553632095,50.6975513960783,0.124552255462931));
#48146=CARTESIAN_POINT('Ctrl Pts',(1.46131672144697,50.6999975377135,0.0799105100689137));
#48147=CARTESIAN_POINT('Ctrl Pts',(1.4643190718301,50.7030059839789,0.0250067832033121));
#48148=CARTESIAN_POINT('Ctrl Pts',(1.46422929886921,50.7060144302444,-0.0301834016102755));
#48149=CARTESIAN_POINT('Ctrl Pts',(1.46101306892529,50.7090228765098,-0.0852822515503883));
#48150=CARTESIAN_POINT('Ctrl Pts',(1.45780261640381,50.7120259186016,-0.140282125566023));
#48151=CARTESIAN_POINT('Ctrl Pts',(1.45147688225879,50.7150289606935,-0.195190466727399));
#48152=CARTESIAN_POINT('Ctrl Pts',(1.44205349495465,50.7180320027853,-0.249627658101197));
#48153=CARTESIAN_POINT('Ctrl Pts',(1.43263954159519,50.7210320384706,-0.304010351295545));
#48154=CARTESIAN_POINT('Ctrl Pts',(1.42013416757001,50.724032074156,-0.357922310554726));
#48155=CARTESIAN_POINT('Ctrl Pts',(1.4046067800889,50.7270321098413,-0.410989103661276));
#48156=CARTESIAN_POINT('Ctrl Pts',(1.38908878400445,50.7300303310214,-0.464023800492489));
#48157=CARTESIAN_POINT('Ctrl Pts',(1.37055254518906,50.7330285522015,-0.516213837771159));
#48158=CARTESIAN_POINT('Ctrl Pts',(1.34911802190673,50.7360267733817,-0.567197331593228));
#48159=CARTESIAN_POINT('Ctrl Pts',(1.32768796894709,50.7390243692614,-0.618170192444067));
#48160=CARTESIAN_POINT('Ctrl Pts',(1.30336103655147,50.7420219651411,-0.667936522245004));
#48161=CARTESIAN_POINT('Ctrl Pts',(1.27630543707061,50.7450195610209,-0.716154090474954));
#48162=CARTESIAN_POINT('Ctrl Pts',(1.24922482309904,50.748019928354,-0.764416238678561));
#48163=CARTESIAN_POINT('Ctrl Pts',(1.21941076060294,50.7510202956872,-0.811126301991854));
#48164=CARTESIAN_POINT('Ctrl Pts',(1.1870768873791,50.7540206630203,-0.855967705845461));
#48165=CARTESIAN_POINT('Ctrl Pts',(1.1547285024467,50.7570223769431,-0.900829234890378));
#48166=CARTESIAN_POINT('Ctrl Pts',(1.11985838603432,50.7600240908658,-0.943820021077674));
#48167=CARTESIAN_POINT('Ctrl Pts',(1.08272086373127,50.7630258047885,-0.98465617412425));
#48168=CARTESIAN_POINT('Ctrl Pts',(1.04551193157149,50.7660332905546,-1.02557084893689));
#48169=CARTESIAN_POINT('Ctrl Pts',(1.00602726164272,50.7690407763207,-1.06432224203247));
#48170=CARTESIAN_POINT('Ctrl Pts',(0.964557657605331,50.7720482620868,-1.1006637884272));
#48171=CARTESIAN_POINT('Ctrl Pts',(0.930894761090083,50.7744895847004,-1.13016399089807));
#48172=CARTESIAN_POINT('Ctrl Pts',(0.895924684517973,50.776930907314,-1.15807693695955));
#48173=CARTESIAN_POINT('Ctrl Pts',(0.859816996954149,50.7793722299277,-1.18429176377646));
#48174=CARTESIAN_POINT('Ctrl Pts',(0.815322256397643,50.7823806202079,-1.21659574103587));
#48175=CARTESIAN_POINT('Ctrl Pts',(0.768909613199299,50.7853890104881,-1.24645753244705));
#48176=CARTESIAN_POINT('Ctrl Pts',(0.720877813142877,50.7883974007683,-1.27364336786965));
#48177=CARTESIAN_POINT('Ctrl Pts',(0.672932275764584,50.7914003881321,-1.3007803789099));
#48178=CARTESIAN_POINT('Ctrl Pts',(0.623373808483145,50.7944033754959,-1.32525071247325));
#48179=CARTESIAN_POINT('Ctrl Pts',(0.572530876490621,50.7974063628596,-1.34686326160634));
#48180=CARTESIAN_POINT('Ctrl Pts',(0.521738831608448,50.8004063446267,-1.36845417941077));
#48181=CARTESIAN_POINT('Ctrl Pts',(0.469665352757049,50.8034063263938,-1.38719277258399));
#48182=CARTESIAN_POINT('Ctrl Pts',(0.416662636605764,50.8064063081608,-1.40293424552141));
#48183=CARTESIAN_POINT('Ctrl Pts',(0.363691962520342,50.80940447633,-1.41866620216704));
#48184=CARTESIAN_POINT('Ctrl Pts',(0.309793670411534,50.8124026444992,-1.43140447926226));
#48185=CARTESIAN_POINT('Ctrl Pts',(0.255336836086297,50.8154008126684,-1.44105355561042));
#48186=CARTESIAN_POINT('Ctrl Pts',(0.20089134105466,50.8183983565429,-1.45070062277625));
#48187=CARTESIAN_POINT('Ctrl Pts',(0.14588805518517,50.8213959004175,-1.45725967419364));
#48188=CARTESIAN_POINT('Ctrl Pts',(0.0907057182243708,50.824393444292,-1.46068638751835));
#48189=CARTESIAN_POINT('Ctrl Pts',(0.0354723242544452,50.8273937616197,
-1.46411627138173));
#48190=CARTESIAN_POINT('Ctrl Pts',(-0.0199399228048711,50.8303940789474,
-1.46440799352035));
#48191=CARTESIAN_POINT('Ctrl Pts',(-0.0751491963403478,50.8333943962751,
-1.46156931012162));
#48192=CARTESIAN_POINT('Ctrl Pts',(-0.130383267536119,50.8363960612178,
-1.45872935170691));
#48193=CARTESIAN_POINT('Ctrl Pts',(-0.185413656714807,50.8393977261606,
-1.45275624195342));
#48194=CARTESIAN_POINT('Ctrl Pts',(-0.239863925455392,50.8423993911034,
-1.4437096478396));
#48195=CARTESIAN_POINT('Ctrl Pts',(-0.294418938010553,50.8454068302295,
-1.43464565115278));
#48196=CARTESIAN_POINT('Ctrl Pts',(-0.348391083256365,50.8484142693556,
-1.4224964746592));
#48197=CARTESIAN_POINT('Ctrl Pts',(-0.401415493228798,50.8514217084818,
-1.40737267693951));
#48198=CARTESIAN_POINT('Ctrl Pts',(-0.444465977484462,50.8538634463685,
-1.3950936753258));
#48199=CARTESIAN_POINT('Ctrl Pts',(-0.486891887937306,50.8563051842551,
-1.38085487095812));
#48200=CARTESIAN_POINT('Ctrl Pts',(-0.528508014289907,50.8587469221418,
-1.36473863022607));
#48201=CARTESIAN_POINT('Ctrl Pts',(-0.579779925614663,50.8617551927181,
-1.34488309492947));
#48202=CARTESIAN_POINT('Ctrl Pts',(-0.630040734325549,50.8647634632944,
-1.32209182286124));
#48203=CARTESIAN_POINT('Ctrl Pts',(-0.678932014993594,50.8677717338707,
-1.29648893902599));
#48204=CARTESIAN_POINT('Ctrl Pts',(-0.727735426344551,50.8707745978657,
-1.27093206969245));
#48205=CARTESIAN_POINT('Ctrl Pts',(-0.775173729354133,50.8737774618607,
-1.24257385940806));
#48206=CARTESIAN_POINT('Ctrl Pts',(-0.820908213835026,50.8767803258557,
-1.21158654435339));
#48207=CARTESIAN_POINT('Ctrl Pts',(-0.866596889467469,50.8797801821041,
-1.18063026699894));
#48208=CARTESIAN_POINT('Ctrl Pts',(-0.910584691336295,50.8827800383525,
-1.14705039625305));
#48209=CARTESIAN_POINT('Ctrl Pts',(-0.952558937867875,50.8857798946009,
-1.11106422851608));
#48210=CARTESIAN_POINT('Ctrl Pts',(-0.994507781445313,50.8887779353263,
-1.07509983972797));
#48211=CARTESIAN_POINT('Ctrl Pts',(-1.03444508413165,50.8917759760517,-1.03673238372182));
#48212=CARTESIAN_POINT('Ctrl Pts',(-1.07209040014527,50.8947740167771,-0.996220068015273));
#48213=CARTESIAN_POINT('Ctrl Pts',(-1.10972785573044,50.8977714315047,-0.955716211373298));
#48214=CARTESIAN_POINT('Ctrl Pts',(-1.14507391504389,50.9007688462322,-0.91306877149604));
#48215=CARTESIAN_POINT('Ctrl Pts',(-1.17788589952651,50.9037662609598,-0.868571849472821));
#48216=CARTESIAN_POINT('Ctrl Pts',(-1.21072822657144,50.9067664475174,-0.824033779355371));
#48217=CARTESIAN_POINT('Ctrl Pts',(-1.24103148194678,50.909766634075,-0.77764323641579));
#48218=CARTESIAN_POINT('Ctrl Pts',(-1.26859506181715,50.9127668206326,-0.729725166849231));
#48219=CARTESIAN_POINT('Ctrl Pts',(-1.29617101243885,50.9157683536975,-0.68178559127635));
#48220=CARTESIAN_POINT('Ctrl Pts',(-1.3210045986092,50.9187698867624,-0.632317595956556));
#48221=CARTESIAN_POINT('Ctrl Pts',(-1.34294174817087,50.9217714198273,-0.581669761135786));
#48222=CARTESIAN_POINT('Ctrl Pts',(-1.36492109801395,50.9247787269122,-0.530924495567432));
#48223=CARTESIAN_POINT('Ctrl Pts',(-1.38399269674653,50.9277860339971,-0.478995353963776));
#48224=CARTESIAN_POINT('Ctrl Pts',(-1.40005150163908,50.930793341082,-0.426248803820208));
#48225=CARTESIAN_POINT('Ctrl Pts',(-1.4130956534759,50.93323609884,-0.383404145482011));
#48226=CARTESIAN_POINT('Ctrl Pts',(-1.42415292766332,50.935678856598,-0.340020587674471));
#48227=CARTESIAN_POINT('Ctrl Pts',(-1.43319201428126,50.938121614356,-0.296298667226898));
#48228=CARTESIAN_POINT('Ctrl Pts',(-1.44896036148208,50.9423829135429,-0.220027418698728));
#48229=CARTESIAN_POINT('Ctrl Pts',(-1.45864431504176,50.9466442127298,-0.142458225153691));
#48230=CARTESIAN_POINT('Ctrl Pts',(-1.46208250160868,50.9509055119168,-0.0643972708248851));
#48231=CARTESIAN_POINT('Ctrl Pts',(-1.46300752811584,50.9520519926635,-0.0433953703978048));
#48232=CARTESIAN_POINT('Ctrl Pts',(-1.46348069847868,50.9531984734103,-0.0223580200854855));
#48233=CARTESIAN_POINT('Ctrl Pts',(-1.46349942146304,50.9543449541571,-0.00130129832626773));
#48234=CARTESIAN_POINT('Ctrl Pts',(-1.46349947235273,51.0256550458429,-0.00124274828025101));
#48235=CARTESIAN_POINT('Ctrl Pts',(-1.46342876260759,51.0211174845061,-0.0845127687219559));
#48236=CARTESIAN_POINT('Ctrl Pts',(-1.45624797044794,51.0165799231693,-0.16748978317585));
#48237=CARTESIAN_POINT('Ctrl Pts',(-1.44212460500004,51.0120423618326,-0.249216519623962));
#48238=CARTESIAN_POINT('Ctrl Pts',(-1.44132103890206,51.0117841917476,-0.25386646194476));
#48239=CARTESIAN_POINT('Ctrl Pts',(-1.4404950095162,51.0115260216626,-0.258512364733264));
#48240=CARTESIAN_POINT('Ctrl Pts',(-1.439646551692,51.0112678515777,-0.263154054122935));
#48241=CARTESIAN_POINT('Ctrl Pts',(-1.42975990758924,51.0082595279165,-0.317241281233215));
#48242=CARTESIAN_POINT('Ctrl Pts',(-1.4167998670086,51.0052512042553,-0.37088592099037));
#48243=CARTESIAN_POINT('Ctrl Pts',(-1.4008211405863,51.0022428805941,-0.42371261733219));
#48244=CARTESIAN_POINT('Ctrl Pts',(-1.38487112339493,50.9992399620357,-0.476444399111713));
#48245=CARTESIAN_POINT('Ctrl Pts',(-1.36591333510058,50.9962370434773,-0.528360651755262));
#48246=CARTESIAN_POINT('Ctrl Pts',(-1.34405344116184,50.9932341249189,-0.579096362707456));
#48247=CARTESIAN_POINT('Ctrl Pts',(-1.32221543597803,50.9902342132437,-0.629781270963807));
#48248=CARTESIAN_POINT('Ctrl Pts',(-1.29748128946475,50.9872343015685,-0.67928749577689));
#48249=CARTESIAN_POINT('Ctrl Pts',(-1.27000580900265,50.9842343898933,-0.727267141495828));
#48250=CARTESIAN_POINT('Ctrl Pts',(-1.24254694949504,50.9812362929779,-0.775217762517333));
#48251=CARTESIAN_POINT('Ctrl Pts',(-1.21235030497094,50.9782381960624,-0.821643176682928));
#48252=CARTESIAN_POINT('Ctrl Pts',(-1.17961691336254,50.9752400991469,-0.866219480102497));
#48253=CARTESIAN_POINT('Ctrl Pts',(-1.14689034918043,50.9722426275649,-0.910786485939042));
#48254=CARTESIAN_POINT('Ctrl Pts',(-1.11162840134636,50.9692451559829,-0.953504720769974));
#48255=CARTESIAN_POINT('Ctrl Pts',(-1.07407444729542,50.9662476844009,-0.994080646460353));
#48256=CARTESIAN_POINT('Ctrl Pts',(-1.03648575900856,50.9632474404109,-1.03469410145521));
#48257=CARTESIAN_POINT('Ctrl Pts',(-0.996601188783579,50.9602471964208,
-1.07316089917715));
#48258=CARTESIAN_POINT('Ctrl Pts',(-0.954702302684935,50.9572469524307,
-1.10922304485982));
#48259=CARTESIAN_POINT('Ctrl Pts',(-0.912784606643465,50.9542453615214,
-1.145301380159));
#48260=CARTESIAN_POINT('Ctrl Pts',(-0.868851212548808,50.951243770612,-1.17897258901797));
#48261=CARTESIAN_POINT('Ctrl Pts',(-0.823215628063835,50.9482421797026,
-1.21001995012953));
#48262=CARTESIAN_POINT('Ctrl Pts',(-0.777492257362881,50.9452348148274,
-1.2411270350373));
#48263=CARTESIAN_POINT('Ctrl Pts',(-0.73006060926692,50.9422274499522,-1.26959991548894));
#48264=CARTESIAN_POINT('Ctrl Pts',(-0.681260956796725,50.9392200850769,
-1.29526667476023));
#48265=CARTESIAN_POINT('Ctrl Pts',(-0.64163031188215,50.9367777765057,-1.31611088514491));
#48266=CARTESIAN_POINT('Ctrl Pts',(-0.601098024097525,50.9343354679346,
-1.33510523574745));
#48267=CARTESIAN_POINT('Ctrl Pts',(-0.559855087663332,50.9318931593634,
-1.35218139715701));
#48268=CARTESIAN_POINT('Ctrl Pts',(-0.509053676778809,50.9288848206766,
-1.37321513449726));
#48269=CARTESIAN_POINT('Ctrl Pts',(-0.456956925343664,50.9258764819898,
-1.39142683058595));
#48270=CARTESIAN_POINT('Ctrl Pts',(-0.403909847570677,50.922868143303,-1.40665883747106));
#48271=CARTESIAN_POINT('Ctrl Pts',(-0.350958082281005,50.9198652098571,
-1.42186347620578));
#48272=CARTESIAN_POINT('Ctrl Pts',(-0.297059883158429,50.9168622764111,
-1.43409890505244));
#48273=CARTESIAN_POINT('Ctrl Pts',(-0.242579214891096,50.9138593429652,
-1.44325589363176));
#48274=CARTESIAN_POINT('Ctrl Pts',(-0.188153100665166,50.9108594164969,
-1.45240371289012));
#48275=CARTESIAN_POINT('Ctrl Pts',(-0.133146191533447,50.9078594900287,
-1.45847911066817));
#48276=CARTESIAN_POINT('Ctrl Pts',(-0.0779347290763724,50.9048595635605,
-1.46142342529597));
#48277=CARTESIAN_POINT('Ctrl Pts',(-0.0227566681379459,50.9018614519708,
-1.46436595868893));
#48278=CARTESIAN_POINT('Ctrl Pts',(0.032625173825781,50.8988633403812,-1.46418113498521));
#48279=CARTESIAN_POINT('Ctrl Pts',(0.087829633035611,50.8958652287915,-1.46086214461216));
#48280=CARTESIAN_POINT('Ctrl Pts',(0.143022575293431,50.8928677426787,-1.45754384665876));
#48281=CARTESIAN_POINT('Ctrl Pts',(0.198037680648211,50.8898702565658,-1.45109271203716));
#48282=CARTESIAN_POINT('Ctrl Pts',(0.252496328463599,50.8868727704529,-1.44155397197344));
#48283=CARTESIAN_POINT('Ctrl Pts',(0.307005339582375,50.8838725122679,-1.43200641049239));
#48284=CARTESIAN_POINT('Ctrl Pts',(0.360956342816656,50.8808722540828,-1.41936562965639));
#48285=CARTESIAN_POINT('Ctrl Pts',(0.413979861946499,50.8778719958978,-1.40372822294871));
#48286=CARTESIAN_POINT('Ctrl Pts',(0.467027182283583,50.8748703909563,-1.38808379691898));
#48287=CARTESIAN_POINT('Ctrl Pts',(0.519145689647756,50.8718687860147,-1.36944024194494));
#48288=CARTESIAN_POINT('Ctrl Pts',(0.569983254564791,50.8688671810732,-1.34794337400194));
#48289=CARTESIAN_POINT('Ctrl Pts',(0.62091860441094,50.8658598026112,-1.32640515731001));
#48290=CARTESIAN_POINT('Ctrl Pts',(0.670567613442345,50.8628524241491,-1.30200289686416));
#48291=CARTESIAN_POINT('Ctrl Pts',(0.718601273244825,50.859845045687,-1.2749291980698));
#48292=CARTESIAN_POINT('Ctrl Pts',(0.757607823904044,50.8574028528411,-1.25294354034776));
#48293=CARTESIAN_POINT('Ctrl Pts',(0.795549513672652,50.8549606599952,-1.22919714062126));
#48294=CARTESIAN_POINT('Ctrl Pts',(0.832265358514905,50.8525184671493,-1.20381336718615));
#48295=CARTESIAN_POINT('Ctrl Pts',(0.877492811124125,50.8495101158046,-1.17254503017764));
#48296=CARTESIAN_POINT('Ctrl Pts',(0.921052116665841,50.84650176446,-1.13865766713958));
#48297=CARTESIAN_POINT('Ctrl Pts',(0.962623684385345,50.8434934131153,-1.10235561061773));
#48298=CARTESIAN_POINT('Ctrl Pts',(1.00412056290765,50.8404904666991,-1.06611877587141));
#48299=CARTESIAN_POINT('Ctrl Pts',(1.04363639538093,50.8374875202828,-1.02747620167254));
#48300=CARTESIAN_POINT('Ctrl Pts',(1.08088198703955,50.8344845738666,-0.986674404296291));
#48301=CARTESIAN_POINT('Ctrl Pts',(1.11809028534983,50.8314846342471,-0.945913461033893));
#48302=CARTESIAN_POINT('Ctrl Pts',(1.15303249076323,50.8284846946277,-0.90299796571356));
#48303=CARTESIAN_POINT('Ctrl Pts',(1.18545523163875,50.8254847550083,-0.858212178764858));
#48304=CARTESIAN_POINT('Ctrl Pts',(1.21785835936004,50.8224866301114,-0.813453483620316));
#48305=CARTESIAN_POINT('Ctrl Pts',(1.2477447336037,50.8194885052145,-0.766827166632986));
#48306=CARTESIAN_POINT('Ctrl Pts',(1.27490187343789,50.8164903803176,-0.718649749950941));
#48307=CARTESIAN_POINT('Ctrl Pts',(1.30205334886781,50.813492880766,-0.670482382057797));
#48308=CARTESIAN_POINT('Ctrl Pts',(1.32647646063315,50.8104953812145,-0.62076501730944));
#48309=CARTESIAN_POINT('Ctrl Pts',(1.34800382649144,50.807497881663,-0.569840270395509));
#48310=CARTESIAN_POINT('Ctrl Pts',(1.36955110141698,50.804497609946,-0.518868426952557));
#48311=CARTESIAN_POINT('Ctrl Pts',(1.38819707305615,50.801497338229,-0.466687458465234));
#48312=CARTESIAN_POINT('Ctrl Pts',(1.40382246858234,50.798497066512,-0.413660158467528));
#48313=CARTESIAN_POINT('Ctrl Pts',(1.41945487838904,50.7954954479652,-0.360609054377571));
#48314=CARTESIAN_POINT('Ctrl Pts',(1.43206388827817,50.7924938294185,-0.306711377327725));
#48315=CARTESIAN_POINT('Ctrl Pts',(1.44158098649968,50.7894922108717,-0.252342048344332));
#48316=CARTESIAN_POINT('Ctrl Pts',(1.45111639039091,50.7864848188595,-0.197868142634271));
#48317=CARTESIAN_POINT('Ctrl Pts',(1.45754793952193,50.7834774268474,-0.142921299290412));
#48318=CARTESIAN_POINT('Ctrl Pts',(1.46085897144578,50.7804700348352,-0.0878823961120183));
#48319=CARTESIAN_POINT('Ctrl Pts',(1.46354762220071,50.7780279482018,-0.0431892635827417));
#48320=CARTESIAN_POINT('Ctrl Pts',(1.46417964027166,50.7755858615684,0.00156438341266757));
#48321=CARTESIAN_POINT('Ctrl Pts',(1.46277133862608,50.773143774935,0.0461764105801477));
#48322=CARTESIAN_POINT('Ctrl Pts',(1.46103653263137,50.7701355085281,0.101131407195287));
#48323=CARTESIAN_POINT('Ctrl Pts',(1.45619680074368,50.7671272421212,0.156105727972618));
#48324=CARTESIAN_POINT('Ctrl Pts',(1.44825042847767,50.7641189757143,0.210720066472687));
#48325=CARTESIAN_POINT('Ctrl Pts',(1.44031833374732,50.7611161143689,0.265236277407166));
#48326=CARTESIAN_POINT('Ctrl Pts',(1.42929075075258,50.7581132530235,0.319393270513705));
#48327=CARTESIAN_POINT('Ctrl Pts',(1.41521789141983,50.7551103916782,0.372814390555439));
#48328=CARTESIAN_POINT('Ctrl Pts',(1.40115912348797,50.7521105371505,0.426182019092628));
#48329=CARTESIAN_POINT('Ctrl Pts',(1.38406125330985,50.7491106826229,0.478814725233145));
#48330=CARTESIAN_POINT('Ctrl Pts',(1.36402563367689,50.7461108280952,0.530345472944148));
#48331=CARTESIAN_POINT('Ctrl Pts',(1.34400213348727,50.7431127881642,0.58184504997071));
#48332=CARTESIAN_POINT('Ctrl Pts',(1.32104459699756,50.7401147482331,0.632243497694544));
#48333=CARTESIAN_POINT('Ctrl Pts',(1.29530366105929,50.7371167083021,0.681190630915026));
#48334=CARTESIAN_POINT('Ctrl Pts',(1.26956809194593,50.7341192934437,0.730127558962903));
#48335=CARTESIAN_POINT('Ctrl Pts',(1.24105052168738,50.7311218785853,0.77761330546091));
#48336=CARTESIAN_POINT('Ctrl Pts',(1.20994797104225,50.7281244637269,0.823321418020167));
#48337=CARTESIAN_POINT('Ctrl Pts',(1.17881664375618,50.7251242756062,0.869071820549729));
#48338=CARTESIAN_POINT('Ctrl Pts',(1.145095855535,50.7221240874855,0.913040864647186));
#48339=CARTESIAN_POINT('Ctrl Pts',(1.10902567610588,50.7191238993648,0.954931568091603));
#48340=CARTESIAN_POINT('Ctrl Pts',(1.07293929855558,50.7161223639425,0.996841083493761));
#48341=CARTESIAN_POINT('Ctrl Pts',(1.03450179452092,50.7131208285202,1.0366700163551));
#48342=CARTESIAN_POINT('Ctrl Pts',(0.993990956745005,50.7101192930979,1.07415745024142));
#48343=CARTESIAN_POINT('Ctrl Pts',(0.953402171440967,50.707111982375,1.11171701427778));
#48344=CARTESIAN_POINT('Ctrl Pts',(0.91073249143381,50.704104671652,1.1469257408952));
#48345=CARTESIAN_POINT('Ctrl Pts',(0.866292838772237,50.7010973609291,1.1795630409147));
#48346=CARTESIAN_POINT('Ctrl Pts',(0.830195677755104,50.6986546015264,1.206073461303));
#48347=CARTESIAN_POINT('Ctrl Pts',(0.792931412066315,50.6962118421236,1.23088802403368));
#48348=CARTESIAN_POINT('Ctrl Pts',(0.754678858566674,50.6937690827209,1.2539107107097));
#48349=CARTESIAN_POINT('Ctrl Pts',(0.707568640778594,50.6907606841451,1.28226447233202));
#48350=CARTESIAN_POINT('Ctrl Pts',(0.658757845635839,50.6877522855694,1.30802005425201));
#48351=CARTESIAN_POINT('Ctrl Pts',(0.608564225018396,50.6847438869936,1.33097026038442));
#48352=CARTESIAN_POINT('Ctrl Pts',(0.558460800518663,50.6817408944011,1.3538792258279));
#48353=CARTESIAN_POINT('Ctrl Pts',(0.5069799585649,50.6787379018086,1.37399260114022));
#48354=CARTESIAN_POINT('Ctrl Pts',(0.454465389109663,50.6757349092161,1.39114825238053));
#48355=CARTESIAN_POINT('Ctrl Pts',(0.40200341254252,50.6727349240947,1.40828672238418));
#48356=CARTESIAN_POINT('Ctrl Pts',(0.348510259315172,50.6697349389734,1.42247317234456));
#48357=CARTESIAN_POINT('Ctrl Pts',(0.294349278233204,50.666734953852,1.43359364968027));
#48358=CARTESIAN_POINT('Ctrl Pts',(0.240221073141164,50.6637367841978,1.44470739736215));
#48359=CARTESIAN_POINT('Ctrl Pts',(0.185426358146335,50.6607386145436,1.45275874348916));
#48360=CARTESIAN_POINT('Ctrl Pts',(0.130341059055819,50.6577404448894,1.45768427937061));
#48361=CARTESIAN_POINT('Ctrl Pts',(0.0752672644074769,50.6547429013963,
1.46260878656485));
#48362=CARTESIAN_POINT('Ctrl Pts',(0.0199035326198596,50.6517453579032,
1.46440873264817));
#48363=CARTESIAN_POINT('Ctrl Pts',(-0.0353689875074307,50.64874781441,1.46307254937091));
#48364=CARTESIAN_POINT('Ctrl Pts',(-0.0906925948275551,50.6457475003524,
1.4617351310884));
#48365=CARTESIAN_POINT('Ctrl Pts',(-0.14592429216002,50.6427471862947,1.45725580448248));
#48366=CARTESIAN_POINT('Ctrl Pts',(-0.200684336464834,50.6397468722371,
1.44967515226608));
#48367=CARTESIAN_POINT('Ctrl Pts',(-0.255468947440346,50.6367452121665,
1.44209109918707));
#48368=CARTESIAN_POINT('Ctrl Pts',(-0.309780963692739,50.633743552096,1.43140304914164));
#48369=CARTESIAN_POINT('Ctrl Pts',(-0.363250476642326,50.6307418920254,
1.41770283953271));
#48370=CARTESIAN_POINT('Ctrl Pts',(-0.416822800948029,50.6277344603529,
1.4039762871155));
#48371=CARTESIAN_POINT('Ctrl Pts',(-0.469548880081667,50.6247270286804,
1.38722616461457));
#48372=CARTESIAN_POINT('Ctrl Pts',(-0.521074711920323,50.621719597008,1.36759401673053));
#48373=CARTESIAN_POINT('Ctrl Pts',(-0.562908564353531,50.6192778615076,
1.35165466459936));
#48374=CARTESIAN_POINT('Ctrl Pts',(-0.603951475876654,50.6168361260072,
1.33381652431876));
#48375=CARTESIAN_POINT('Ctrl Pts',(-0.644026008875002,50.6143943905067,
1.31417759450256));
#48376=CARTESIAN_POINT('Ctrl Pts',(-0.69340155100613,50.6113859458649,1.28998061118176));
#48377=CARTESIAN_POINT('Ctrl Pts',(-0.741516750164403,50.608377501223,1.26294552122677));
#48378=CARTESIAN_POINT('Ctrl Pts',(-0.788025175090753,50.6053690565812,
1.2332268945426));
#48379=CARTESIAN_POINT('Ctrl Pts',(-0.83445006565773,50.6023660154441,1.20356164585276));
#48380=CARTESIAN_POINT('Ctrl Pts',(-0.879273466979466,50.599362974307,1.17122270757813));
#48381=CARTESIAN_POINT('Ctrl Pts',(-0.922172736471481,50.5963599331699,
1.13641088260748));
#48382=CARTESIAN_POINT('Ctrl Pts',(-0.965029064456583,50.5933598980306,
1.10163390373654));
#48383=CARTESIAN_POINT('Ctrl Pts',(-1.00596466714275,50.5903598628914,1.06438927286245));
#48384=CARTESIAN_POINT('Ctrl Pts',(-1.04468671702488,50.5873598277522,1.02492044241091));
#48385=CARTESIAN_POINT('Ctrl Pts',(-1.08338535198395,50.5843616067109,0.985475478454843));
#48386=CARTESIAN_POINT('Ctrl Pts',(-1.11987271736089,50.5813633856696,0.943809357216002));
#48387=CARTESIAN_POINT('Ctrl Pts',(-1.15389162651969,50.5783651646283,0.900203512683514));
#48388=CARTESIAN_POINT('Ctrl Pts',(-1.18790344540187,50.5753675684812,0.856606756552381));
#48389=CARTESIAN_POINT('Ctrl Pts',(-1.21944750449566,50.572369972334,0.811071496575774));
#48390=CARTESIAN_POINT('Ctrl Pts',(-1.2483073359531,50.5693723761869,0.763911673562907));
#48391=CARTESIAN_POINT('Ctrl Pts',(-1.27719385605675,50.566372007959,0.71670823865876));
#48392=CARTESIAN_POINT('Ctrl Pts',(-1.30339091205091,50.5633716397311,0.667877690987514));
#48393=CARTESIAN_POINT('Ctrl Pts',(-1.3267266110265,50.5603712715032,0.617761078082899));
#48394=CARTESIAN_POINT('Ctrl Pts',(-1.35007278596125,50.5573695563375,0.567621966619721));
#48395=CARTESIAN_POINT('Ctrl Pts',(-1.3705548470833,50.5543678411718,0.516196131186225));
#48396=CARTESIAN_POINT('Ctrl Pts',(-1.38804929530734,50.5513661260061,0.46384415895512));
#48397=CARTESIAN_POINT('Ctrl Pts',(-1.4055773859604,50.5483586384383,0.411391512070742));
#48398=CARTESIAN_POINT('Ctrl Pts',(-1.42010624628452,50.5453511508705,0.358009681929733));
#48399=CARTESIAN_POINT('Ctrl Pts',(-1.4315627645176,50.5423436633027,0.304072855162587));
#48400=CARTESIAN_POINT('Ctrl Pts',(-1.4408625689543,50.5399023416327,0.26028975015062));
#48401=CARTESIAN_POINT('Ctrl Pts',(-1.44813886589741,50.5374610199626,0.216141274358366));
#48402=CARTESIAN_POINT('Ctrl Pts',(-1.45337774111322,50.5350196982925,0.171829542386152));
#48403=CARTESIAN_POINT('Ctrl Pts',(-1.4600763320478,50.5318981474759,0.115171165567171));
#48404=CARTESIAN_POINT('Ctrl Pts',(-1.46346269457913,50.5287765966594,0.0581134335821789));
#48405=CARTESIAN_POINT('Ctrl Pts',(-1.46349969347842,50.5256550458429,0.000947200379455493));
#48406=CARTESIAN_POINT('Origin',(0.,55.715,0.));
#48407=CARTESIAN_POINT('',(-1.28852825769066,50.065,0.693921594369763));
#48408=CARTESIAN_POINT('Ctrl Pts',(-1.46349969347884,50.5256550458075,0.000947199730964576));
#48409=CARTESIAN_POINT('Ctrl Pts',(-1.46353482282959,50.5226912244331,-0.0533304698703549));
#48410=CARTESIAN_POINT('Ctrl Pts',(-1.4605461735546,50.5197274030587,-0.107727267896845));
#48411=CARTESIAN_POINT('Ctrl Pts',(-1.45452035935177,50.5167635816843,-0.161872709964321));
#48412=CARTESIAN_POINT('Ctrl Pts',(-1.44850182572144,50.5138033412893,-0.215952731857356));
#48413=CARTESIAN_POINT('Ctrl Pts',(-1.43945344630703,50.5108431008942,-0.26978146135027));
#48414=CARTESIAN_POINT('Ctrl Pts',(-1.42741383466044,50.5078828604992,-0.322989155576445));
#48415=CARTESIAN_POINT('Ctrl Pts',(-1.41538368556614,50.5049249467099,-0.376155031129087));
#48416=CARTESIAN_POINT('Ctrl Pts',(-1.40036707739651,50.5019670329206,-0.428700307980801));
#48417=CARTESIAN_POINT('Ctrl Pts',(-1.38245400783414,50.4990091191313,-0.480263642412506));
#48418=CARTESIAN_POINT('Ctrl Pts',(-1.36454745537885,50.4960522814859,-0.531808217146408));
#48419=CARTESIAN_POINT('Ctrl Pts',(-1.34374670863753,50.4930954438406,-0.582371043352419));
#48420=CARTESIAN_POINT('Ctrl Pts',(-1.32019138050361,50.4901386061952,-0.631606656744505));
#48421=CARTESIAN_POINT('Ctrl Pts',(-1.29661750760403,50.4871794406747,-0.680881032615597));
#48422=CARTESIAN_POINT('Ctrl Pts',(-1.27028495177837,50.4842202751543,-0.728825613385225));
#48423=CARTESIAN_POINT('Ctrl Pts',(-1.24138048400446,50.4812611096338,-0.775117245281548));
#48424=CARTESIAN_POINT('Ctrl Pts',(-1.21246571703341,50.4783008897079,-0.821425371743577));
#48425=CARTESIAN_POINT('Ctrl Pts',(-1.18097752545467,50.475340669782,-0.866078928781415));
#48426=CARTESIAN_POINT('Ctrl Pts',(-1.14714552231686,50.4723804498561,-0.90878457327816));
#48427=CARTESIAN_POINT('Ctrl Pts',(-1.11324870640735,50.4694145589666,-0.951572029992054));
#48428=CARTESIAN_POINT('Ctrl Pts',(-1.07699947243047,50.466448668077,-0.992403711374319));
#48429=CARTESIAN_POINT('Ctrl Pts',(-1.03866628085557,50.4634827771875,-1.03102114770438));
#48430=CARTESIAN_POINT('Ctrl Pts',(-1.00489938555175,50.4608701868178,-1.0650384281834));
#48431=CARTESIAN_POINT('Ctrl Pts',(-0.969516194411335,50.4582575964481,
-1.0973379734395));
#48432=CARTESIAN_POINT('Ctrl Pts',(-0.9327204188105,50.4556450060784,-1.12776986585649));
#48433=CARTESIAN_POINT('Ctrl Pts',(-0.890342237235046,50.4526360511844,
-1.16281867897358));
#48434=CARTESIAN_POINT('Ctrl Pts',(-0.845895538558477,50.4496270962905,
-1.19555012316991));
#48435=CARTESIAN_POINT('Ctrl Pts',(-0.799663853035677,50.4466181413966,
-1.22571202659847));
#48436=CARTESIAN_POINT('Ctrl Pts',(-0.753515307750692,50.4436145976232,
-1.25581968870325));
#48437=CARTESIAN_POINT('Ctrl Pts',(-0.705588584788405,50.4406110538499,
-1.28336669349437));
#48438=CARTESIAN_POINT('Ctrl Pts',(-0.656199557617031,50.4376075100765,
-1.30814157895207));
#48439=CARTESIAN_POINT('Ctrl Pts',(-0.606860041905433,50.4346069772926,
-1.33289162810877));
#48440=CARTESIAN_POINT('Ctrl Pts',(-0.556061595897285,50.4316064445086,
-1.35487482683292));
#48441=CARTESIAN_POINT('Ctrl Pts',(-0.504146693165044,50.4286059117247,
-1.37392443815908));
#48442=CARTESIAN_POINT('Ctrl Pts',(-0.452263277975644,50.4256071988306,
-1.3929624954724));
#48443=CARTESIAN_POINT('Ctrl Pts',(-0.399265243405242,50.4226084859365,
-1.40907031007267));
#48444=CARTESIAN_POINT('Ctrl Pts',(-0.34551501355974,50.4196097730424,-1.42212925762914));
#48445=CARTESIAN_POINT('Ctrl Pts',(-0.291776102853237,50.4166116916404,
-1.43518545513147));
#48446=CARTESIAN_POINT('Ctrl Pts',(-0.237285824802378,50.4136136102384,
-1.44519393568715));
#48447=CARTESIAN_POINT('Ctrl Pts',(-0.182419477212928,50.4106155288365,
-1.45208656227284));
#48448=CARTESIAN_POINT('Ctrl Pts',(-0.127502655314952,50.4076146893489,
-1.45898552973188));
#48449=CARTESIAN_POINT('Ctrl Pts',(-0.0722095982901611,50.4046138498613,
-1.46276284973304));
#48450=CARTESIAN_POINT('Ctrl Pts',(-0.0169219692928829,50.4016130103737,
-1.46340216514643));
#48451=CARTESIAN_POINT('Ctrl Pts',(0.0383903471274892,50.39861083093,-1.46404176603146));
#48452=CARTESIAN_POINT('Ctrl Pts',(0.0936967015878671,50.3956086514863,
-1.46154059277131));
#48453=CARTESIAN_POINT('Ctrl Pts',(0.14861752829933,50.3926064720427,-1.45593443543389));
#48454=CARTESIAN_POINT('Ctrl Pts',(0.203643636320153,50.3895985375257,-1.45031753128837));
#48455=CARTESIAN_POINT('Ctrl Pts',(0.258282216616718,50.3865906030087,-1.44158383518267));
#48456=CARTESIAN_POINT('Ctrl Pts',(0.312162035999495,50.3835826684918,-1.42982065773322));
#48457=CARTESIAN_POINT('Ctrl Pts',(0.355823042622614,50.3811452169492,-1.42028847714291));
#48458=CARTESIAN_POINT('Ctrl Pts',(0.398985900736044,50.3787077654067,-1.4087680018665));
#48459=CARTESIAN_POINT('Ctrl Pts',(0.441461587347743,50.3762703138641,-1.39532932202273));
#48460=CARTESIAN_POINT('Ctrl Pts',(0.493895812924911,50.3732613952518,-1.37873990754595));
#48461=CARTESIAN_POINT('Ctrl Pts',(0.54550501015341,50.3702524766396,-1.35915555163723));
#48462=CARTESIAN_POINT('Ctrl Pts',(0.595923536242905,50.3672435580273,-1.33667774311977));
#48463=CARTESIAN_POINT('Ctrl Pts',(0.646251713829184,50.3642400313079,-1.31424021416842));
#48464=CARTESIAN_POINT('Ctrl Pts',(0.695392975524007,50.3612365045885,-1.28891973535305));
#48465=CARTESIAN_POINT('Ctrl Pts',(0.742998345345203,50.3582329778691,-1.26086704644633));
#48466=CARTESIAN_POINT('Ctrl Pts',(0.79055617710117,50.3552324504301,-1.23284237056755));
#48467=CARTESIAN_POINT('Ctrl Pts',(0.836580701893695,50.352231922991,-1.20209115605839));
#48468=CARTESIAN_POINT('Ctrl Pts',(0.880746100695365,50.349231395552,-1.16881074435082));
#48469=CARTESIAN_POINT('Ctrl Pts',(0.924884882543173,50.3462326764267,-1.13555038959296));
#48470=CARTESIAN_POINT('Ctrl Pts',(0.967166337697631,50.3432339573015,-1.09976417610463));
#48471=CARTESIAN_POINT('Ctrl Pts',(1.00729425568835,50.3402352381762,-1.06169229650462));
#48472=CARTESIAN_POINT('Ctrl Pts',(1.04741387657129,50.3372371390855,-1.0236282888926));
#48473=CARTESIAN_POINT('Ctrl Pts',(1.08538046116735,50.3342390399948,-0.98327991721212));
#48474=CARTESIAN_POINT('Ctrl Pts',(1.12093323976277,50.3312409409041,-0.94092556666026));
#48475=CARTESIAN_POINT('Ctrl Pts',(1.15651893115896,50.3282400663387,-0.898532006787599));
#48476=CARTESIAN_POINT('Ctrl Pts',(1.1896860111028,50.3252391917733,-0.854129163371487));
#48477=CARTESIAN_POINT('Ctrl Pts',(1.22021376407475,50.3222383172079,-0.808028848471721));
#48478=CARTESIAN_POINT('Ctrl Pts',(1.25075524670215,50.319236093019,-0.761907800259525));
#48479=CARTESIAN_POINT('Ctrl Pts',(1.2786547690964,50.31623386883,-0.714088216096344));
#48480=CARTESIAN_POINT('Ctrl Pts',(1.30373656897248,50.3132316446411,-0.664908421306164));
#48481=CARTESIAN_POINT('Ctrl Pts',(1.32886657582411,50.3102236502064,-0.615634103428473));
#48482=CARTESIAN_POINT('Ctrl Pts',(1.3511678269104,50.3072156557718,-0.564994837064679));
#48483=CARTESIAN_POINT('Ctrl Pts',(1.37051236645305,50.3042076613371,-0.513349883996552));
#48484=CARTESIAN_POINT('Ctrl Pts',(1.38618704537271,50.3017703147747,-0.471502516403251));
#48485=CARTESIAN_POINT('Ctrl Pts',(1.39992134641109,50.2993329682124,-0.428995320515241));
#48486=CARTESIAN_POINT('Ctrl Pts',(1.41167166311979,50.29689562165,-0.386025084087313));
#48487=CARTESIAN_POINT('Ctrl Pts',(1.42615711337943,50.2938909313705,-0.333052620633494));
#48488=CARTESIAN_POINT('Ctrl Pts',(1.43768809010586,50.2908862410911,-0.279149052216486));
#48489=CARTESIAN_POINT('Ctrl Pts',(1.44615115225048,50.2878815508116,-0.224675532367466));
#48490=CARTESIAN_POINT('Ctrl Pts',(1.45459897720145,50.2848822702819,-0.170300088552479));
#48491=CARTESIAN_POINT('Ctrl Pts',(1.45998976692289,50.2818829897521,-0.115357249028846));
#48492=CARTESIAN_POINT('Ctrl Pts',(1.46226047055535,50.2788837092223,-0.0602209784978448));
#48493=CARTESIAN_POINT('Ctrl Pts',(1.46452889744066,50.2758874359557,-0.00513999098368401));
#48494=CARTESIAN_POINT('Ctrl Pts',(1.46368341260466,50.2728911626891,0.0501335162761768));
#48495=CARTESIAN_POINT('Ctrl Pts',(1.45971266687425,50.2698948894225,0.105219675759159));
#48496=CARTESIAN_POINT('Ctrl Pts',(1.4557443184603,50.2669004251399,0.160272577268573));
#48497=CARTESIAN_POINT('Ctrl Pts',(1.44865448637538,50.2639059608572,0.215137827320708));
#48498=CARTESIAN_POINT('Ctrl Pts',(1.43848388312004,50.2609114965745,0.269437131820935));
#48499=CARTESIAN_POINT('Ctrl Pts',(1.42831536328326,50.2579176456992,0.323725313266256));
#48500=CARTESIAN_POINT('Ctrl Pts',(1.41506742283674,50.2549237948238,0.377447258392881));
#48501=CARTESIAN_POINT('Ctrl Pts',(1.39883209022656,50.2519299439485,0.430233696207518));
#48502=CARTESIAN_POINT('Ctrl Pts',(1.38258146762911,50.2489332735471,0.483069846829524));
#48503=CARTESIAN_POINT('Ctrl Pts',(1.36333798780192,50.2459366031458,0.534968221800448));
#48504=CARTESIAN_POINT('Ctrl Pts',(1.34124349563131,50.2429399327445,0.585575046793066));
#48505=CARTESIAN_POINT('Ctrl Pts',(1.31913892395465,50.2399418952623,0.636204958616343));
#48506=CARTESIAN_POINT('Ctrl Pts',(1.29418098750364,50.2369438577801,0.685541672072548));
#48507=CARTESIAN_POINT('Ctrl Pts',(1.26655818513784,50.233945820298,0.733254808139941));
#48508=CARTESIAN_POINT('Ctrl Pts',(1.23888146057457,50.2309419303767,0.781061084545183));
#48509=CARTESIAN_POINT('Ctrl Pts',(1.20852976973247,50.2279380404554,0.827237007586373));
#48510=CARTESIAN_POINT('Ctrl Pts',(1.17573512600955,50.2249341505341,0.871481017273076));
#48511=CARTESIAN_POINT('Ctrl Pts',(1.14875744583217,50.2224630768347,0.907877227373038));
#48512=CARTESIAN_POINT('Ctrl Pts',(1.12012747192073,50.2199920031353,0.94296656694366));
#48513=CARTESIAN_POINT('Ctrl Pts',(1.08999331599448,50.2175209294358,0.976599621691185));
#48514=CARTESIAN_POINT('Ctrl Pts',(1.05323995169542,50.2145070646339,1.01762044592303));
#48515=CARTESIAN_POINT('Ctrl Pts',(1.01409059008519,50.2114931998319,1.05664969724153));
#48516=CARTESIAN_POINT('Ctrl Pts',(0.972789141077472,50.2084793350299,1.09339541658165));
#48517=CARTESIAN_POINT('Ctrl Pts',(0.931562323867634,50.2054709162874,1.13007473633616));
#48518=CARTESIAN_POINT('Ctrl Pts',(0.888191527718388,50.2024624975449,1.16447836631213));
#48519=CARTESIAN_POINT('Ctrl Pts',(0.842958644095413,50.1994540788024,1.19634985449275));
#48520=CARTESIAN_POINT('Ctrl Pts',(0.797771407815691,50.1964486960442,1.22818917915328));
#48521=CARTESIAN_POINT('Ctrl Pts',(0.750726235319475,50.1934433132859,1.2575011225332));
#48522=CARTESIAN_POINT('Ctrl Pts',(0.702137934126864,50.1904379305277,1.28406953529007));
#48523=CARTESIAN_POINT('Ctrl Pts',(0.653579593944909,50.1874344009791,1.31062156516304));
#48524=CARTESIAN_POINT('Ctrl Pts',(0.603480472428103,50.1844308714304,1.33443316555242));
#48525=CARTESIAN_POINT('Ctrl Pts',(0.55218223856742,50.1814273418817,1.35533280983332));
#48526=CARTESIAN_POINT('Ctrl Pts',(0.500895501923475,50.1784244854991,1.37622776998141));
#48527=CARTESIAN_POINT('Ctrl Pts',(0.448410674124299,50.1754216291166,1.39421187125809));
#48528=CARTESIAN_POINT('Ctrl Pts',(0.395089662303164,50.172418772734,1.40916159780955));
#48529=CARTESIAN_POINT('Ctrl Pts',(0.341721495107952,50.1694132607225,1.42412454541448));
#48530=CARTESIAN_POINT('Ctrl Pts',(0.28751617447663,50.1664077487111,1.43604761333399));
#48531=CARTESIAN_POINT('Ctrl Pts',(0.232849607511033,50.1634022366997,1.44485753978791));
#48532=CARTESIAN_POINT('Ctrl Pts',(0.178159567937786,50.1603954341883,1.45367124902824));
#48533=CARTESIAN_POINT('Ctrl Pts',(0.1230084120419,50.1573886316769,1.45936909650855));
#48534=CARTESIAN_POINT('Ctrl Pts',(0.0677777807641783,50.1543818291655,
1.46192969134452));
#48535=CARTESIAN_POINT('Ctrl Pts',(0.0124440031447415,50.1513694112795,
1.46449506823682));
#48536=CARTESIAN_POINT('Ctrl Pts',(-0.0429690181593199,50.1483569933936,
1.46391149169015));
#48537=CARTESIAN_POINT('Ctrl Pts',(-0.0980801710523986,50.1453445755077,
1.46020975549622));
#48538=CARTESIAN_POINT('Ctrl Pts',(-0.141977215097185,50.1429451294123,
1.45726125472611));
#48539=CARTESIAN_POINT('Ctrl Pts',(-0.185682698960755,50.140545683317,1.45233551036316));
#48540=CARTESIAN_POINT('Ctrl Pts',(-0.229008582239096,50.1381462372216,
1.44547131388376));
#48541=CARTESIAN_POINT('Ctrl Pts',(-0.284040820412925,50.1350984773374,
1.43675245884971));
#48542=CARTESIAN_POINT('Ctrl Pts',(-0.338705226109161,50.1320507174532,
1.4248654024174));
#48543=CARTESIAN_POINT('Ctrl Pts',(-0.392604340574882,50.1290029575689,
1.40985605001424));
#48544=CARTESIAN_POINT('Ctrl Pts',(-0.445154391254212,50.1260314813589,
1.39522237305557));
#48545=CARTESIAN_POINT('Ctrl Pts',(-0.496976453258863,50.1230600051489,
1.37762101676102));
#48546=CARTESIAN_POINT('Ctrl Pts',(-0.547709178015198,50.1200885289389,
1.35714660457812));
#48547=CARTESIAN_POINT('Ctrl Pts',(-0.598393489551697,50.117119888349,1.33669173071536));
#48548=CARTESIAN_POINT('Ctrl Pts',(-0.647990022335606,50.114151247759,1.31336942968564));
#48549=CARTESIAN_POINT('Ctrl Pts',(-0.696153357328885,50.1111826071691,
1.28732387264422));
#48550=CARTESIAN_POINT('Ctrl Pts',(-0.744290795247793,50.1082155627955,
1.2612923201091));
#48551=CARTESIAN_POINT('Ctrl Pts',(-0.790996087047045,50.105248518422,1.23254066940583));
#48552=CARTESIAN_POINT('Ctrl Pts',(-0.8359468332237,50.1022814740484,1.20125981453775));
#48553=CARTESIAN_POINT('Ctrl Pts',(-0.883014719253845,50.0991746845444,
1.16850565944385));
#48554=CARTESIAN_POINT('Ctrl Pts',(-0.928158107811135,50.0960678950404,
1.13297842579747));
#48555=CARTESIAN_POINT('Ctrl Pts',(-0.971041640784116,50.0929611055363,
1.09494766170045));
#48556=CARTESIAN_POINT('Ctrl Pts',(-1.01202925853428,50.0899916696761,1.05859826804073));
#48557=CARTESIAN_POINT('Ctrl Pts',(-1.05095229273905,50.087022233816,1.01996252088922));
#48558=CARTESIAN_POINT('Ctrl Pts',(-1.08755484312706,50.0840527979558,0.979314409773936));
#48559=CARTESIAN_POINT('Ctrl Pts',(-1.12417879476268,50.0810816258878,0.938642532000828));
#48560=CARTESIAN_POINT('Ctrl Pts',(-1.15847922710366,50.0781104538199,0.895956372875629));
#48561=CARTESIAN_POINT('Ctrl Pts',(-1.19024132733919,50.0751392817519,0.851561995801738));
#48562=CARTESIAN_POINT('Ctrl Pts',(-1.2220545016143,50.0721633319848,0.807096231755478));
#48563=CARTESIAN_POINT('Ctrl Pts',(-1.251320922671,50.0691873822177,0.760917232211028));
#48564=CARTESIAN_POINT('Ctrl Pts',(-1.27787071671936,50.0662114324505,0.713357330761477));
#48565=CARTESIAN_POINT('Ctrl Pts',(-1.28147329568094,50.0658076216337,0.706903860724575));
#48566=CARTESIAN_POINT('Ctrl Pts',(-1.28502592793118,50.0654038108168,0.700424996050097));
#48567=CARTESIAN_POINT('Ctrl Pts',(-1.28852825769066,50.065,0.693921594369763));
#48568=CARTESIAN_POINT('',(-0.262389908308853,50.065,1.43978602091341));
#48569=CARTESIAN_POINT('Origin',(0.,50.065,0.));
#48570=CARTESIAN_POINT('Ctrl Pts',(-0.262389908308852,50.065,1.43978602091341));
#48571=CARTESIAN_POINT('Ctrl Pts',(0.216315810969557,50.0914582307381,1.52702644967428));
#48572=CARTESIAN_POINT('Ctrl Pts',(1.25937612909543,50.1443746922141,1.1847701442246));
#48573=CARTESIAN_POINT('Ctrl Pts',(1.67952585005074,50.2237493844286,-0.41815389563593));
#48574=CARTESIAN_POINT('Ctrl Pts',(0.5592028946949,50.3031240766425,-1.6364077241352));
#48575=CARTESIAN_POINT('Ctrl Pts',(-1.01956042907598,50.3799890265663,-1.36693371954133));
#48576=CARTESIAN_POINT('Ctrl Pts',(-1.4624799194635,50.4303957457519,-0.438091132407085));
#48577=CARTESIAN_POINT('Ctrl Pts',(-1.46539629526008,50.4543442341995,0.000791507262081051));
#48578=CARTESIAN_POINT('Origin',(0.,56.5393671147362,0.));
#48579=CARTESIAN_POINT('',(-1.17776886881611,50.2893670693371,0.000646086109262299));
#48580=CARTESIAN_POINT('Ctrl Pts',(0.18873835403253,50.4271343927849,1.16119835837062));
#48581=CARTESIAN_POINT('Ctrl Pts',(-0.0598496141700551,50.4101796998113,
1.19981666554508));
#48582=CARTESIAN_POINT('Ctrl Pts',(-0.73034770528701,50.3667667760997,1.1033036474199));
#48583=CARTESIAN_POINT('Ctrl Pts',(-1.16118938021621,50.3208443500834,0.464624652439107));
#48584=CARTESIAN_POINT('Ctrl Pts',(-1.17952169233894,50.2918766170408,0.0376575097721022));
#48585=CARTESIAN_POINT('Ctrl Pts',(-1.17927611201048,50.2893671147362,0.000647582463977861));
#48586=CARTESIAN_POINT('',(1.11732377115968,50.0650022861545,-0.372401198845414));
#48587=CARTESIAN_POINT('Ctrl Pts',(-1.17774982279649,50.2893670687634,0.000646067200833073));
#48588=CARTESIAN_POINT('Ctrl Pts',(-1.17777512123915,50.2862359274727,-0.0454717922400353));
#48589=CARTESIAN_POINT('Ctrl Pts',(-1.17508737128827,50.2831047861821,-0.0917002762411251));
#48590=CARTESIAN_POINT('Ctrl Pts',(-1.16967387860585,50.2799736448915,-0.137688344485505));
#48591=CARTESIAN_POINT('Ctrl Pts',(-1.16426758621388,50.2768466682185,-0.183615245666733));
#48592=CARTESIAN_POINT('Ctrl Pts',(-1.15614278161509,50.2737196915454,-0.229301796990624));
#48593=CARTESIAN_POINT('Ctrl Pts',(-1.1453387574601,50.2705927148724,-0.274397873825134));
#48594=CARTESIAN_POINT('Ctrl Pts',(-1.13454402590275,50.2674684277283,-0.319455163288285));
#48595=CARTESIAN_POINT('Ctrl Pts',(-1.12107476478285,50.2643441405842,-0.363922425653406));
#48596=CARTESIAN_POINT('Ctrl Pts',(-1.10502154489056,50.2612198534402,-0.407458522831076));
#48597=CARTESIAN_POINT('Ctrl Pts',(-1.08897459093607,50.2580967857766,-0.450977626877231));
#48598=CARTESIAN_POINT('Ctrl Pts',(-1.07034587439882,50.2549737181131,-0.493565746964381));
#48599=CARTESIAN_POINT('Ctrl Pts',(-1.04927525504211,50.2518506504495,-0.534898590067613));
#48600=CARTESIAN_POINT('Ctrl Pts',(-1.02818743552271,50.2487250333938,-0.5762651735946));
#48601=CARTESIAN_POINT('Ctrl Pts',(-1.00465399029067,50.2455994163381,-0.616373918841575));
#48602=CARTESIAN_POINT('Ctrl Pts',(-0.978861277365035,50.2424737992824,
-0.654924165209448));
#48603=CARTESIAN_POINT('Ctrl Pts',(-0.953057907966577,50.2393468908521,
-0.693490338930674));
#48604=CARTESIAN_POINT('Ctrl Pts',(-0.924993758960615,50.2362199824218,
-0.730496272194395));
#48605=CARTESIAN_POINT('Ctrl Pts',(-0.894896920286096,50.2330930739916,
-0.765672622314825));
#48606=CARTESIAN_POINT('Ctrl Pts',(-0.864741962809198,50.2299601273134,
-0.800916900079192));
#48607=CARTESIAN_POINT('Ctrl Pts',(-0.832546880296198,50.2268271806352,
-0.834324128454841));
#48608=CARTESIAN_POINT('Ctrl Pts',(-0.798576897345711,50.223694233957,-0.865661597580543));
#48609=CARTESIAN_POINT('Ctrl Pts',(-0.776264883462669,50.2216364657833,
-0.886244535382166));
#48610=CARTESIAN_POINT('Ctrl Pts',(-0.753187891129945,50.2195786976095,
-0.905935366721064));
#48611=CARTESIAN_POINT('Ctrl Pts',(-0.729428030643133,50.2175209294358,
-0.924678220037695));
#48612=CARTESIAN_POINT('Ctrl Pts',(-0.691240792213901,50.2142136505935,
-0.954802042054396));
#48613=CARTESIAN_POINT('Ctrl Pts',(-0.651096382328785,50.2109063717513,
-0.982625730784162));
#48614=CARTESIAN_POINT('Ctrl Pts',(-0.609305396523816,50.207599092909,-1.00788987308483));
#48615=CARTESIAN_POINT('Ctrl Pts',(-0.5691739691615,50.2044231491482,-1.03215075308278));
#48616=CARTESIAN_POINT('Ctrl Pts',(-0.527524815107055,50.2012472053874,
-1.05405123231057));
#48617=CARTESIAN_POINT('Ctrl Pts',(-0.484665993251312,50.1980712616266,
-1.07340297068981));
#48618=CARTESIAN_POINT('Ctrl Pts',(-0.441850609314778,50.1948985367221,
-1.09273509585498));
#48619=CARTESIAN_POINT('Ctrl Pts',(-0.397828488955413,50.1917258118176,
-1.1095233654687));
#48620=CARTESIAN_POINT('Ctrl Pts',(-0.352932200540133,50.1885530869131,
-1.12362534873591));
#48621=CARTESIAN_POINT('Ctrl Pts',(-0.308061769503081,50.1853821892944,
-1.1377192101666));
#48622=CARTESIAN_POINT('Ctrl Pts',(-0.262318697469956,50.1822112916756,
-1.14912968372275));
#48623=CARTESIAN_POINT('Ctrl Pts',(-0.216052893589172,50.1790403940568,
-1.15776345151838));
#48624=CARTESIAN_POINT('Ctrl Pts',(-0.169793492708456,50.1758699352775,
-1.16639602443547));
#48625=CARTESIAN_POINT('Ctrl Pts',(-0.12301205036318,50.1726994764981,-1.17225255427138));
#48626=CARTESIAN_POINT('Ctrl Pts',(-0.0760682379740762,50.1695290177188,
-1.17529089406475));
#48627=CARTESIAN_POINT('Ctrl Pts',(-0.0290785465389814,50.1663554603921,
-1.17833220328314));
#48628=CARTESIAN_POINT('Ctrl Pts',(0.0180732756024785,50.1631819030654,
-1.17854979153053));
#48629=CARTESIAN_POINT('Ctrl Pts',(0.0650248635361245,50.1600083457387,
-1.17595358310696));
#48630=CARTESIAN_POINT('Ctrl Pts',(0.112003821854029,50.1568329383898,-1.17335586122612));
#48631=CARTESIAN_POINT('Ctrl Pts',(0.158781760840182,50.1536575310408,-1.16794114135168));
#48632=CARTESIAN_POINT('Ctrl Pts',(0.205002381111276,50.1504821236918,-1.15977113528433));
#48633=CARTESIAN_POINT('Ctrl Pts',(0.251305107393855,50.1473010755698,-1.15158661607094));
#48634=CARTESIAN_POINT('Ctrl Pts',(0.29704799991131,50.1441200274477,-1.14063717773628));
#48635=CARTESIAN_POINT('Ctrl Pts',(0.341887748020115,50.1409389793256,-1.12703497295059));
#48636=CARTESIAN_POINT('Ctrl Pts',(0.355009822639454,50.140008065291,-1.12305437195006));
#48637=CARTESIAN_POINT('Ctrl Pts',(0.3680546771462,50.1390771512563,-1.11884690372938));
#48638=CARTESIAN_POINT('Ctrl Pts',(0.381014047717165,50.1381462372216,-1.11441615114919));
#48639=CARTESIAN_POINT('Ctrl Pts',(0.424750478343914,50.1350045061573,-1.09946285524747));
#48640=CARTESIAN_POINT('Ctrl Pts',(0.467712432024237,50.131862775093,-1.08189410993567));
#48641=CARTESIAN_POINT('Ctrl Pts',(0.509561861228147,50.1287210440287,-1.06181061026989));
#48642=CARTESIAN_POINT('Ctrl Pts',(0.551350779696744,50.1255838556418,-1.04175614964611));
#48643=CARTESIAN_POINT('Ctrl Pts',(0.592029843000789,50.1224466672549,-1.01919436609024));
#48644=CARTESIAN_POINT('Ctrl Pts',(0.63127840950339,50.119309478868,-0.994274927872));
#48645=CARTESIAN_POINT('Ctrl Pts',(0.670488458522769,50.116175369233,-0.969379944917456));
#48646=CARTESIAN_POINT('Ctrl Pts',(0.708270307016205,50.1130412595981,-0.942132187805565));
#48647=CARTESIAN_POINT('Ctrl Pts',(0.744328103564076,50.1099071499631,-0.91272708776759));
#48648=CARTESIAN_POINT('Ctrl Pts',(0.780367258885852,50.106774660606,-0.88333718963241));
#48649=CARTESIAN_POINT('Ctrl Pts',(0.814683685085752,50.1036421712488,-0.851792517324745));
#48650=CARTESIAN_POINT('Ctrl Pts',(0.84701310639821,50.1005096818916,-0.818329921296817));
#48651=CARTESIAN_POINT('Ctrl Pts',(0.879363404201221,50.0973751697521,-0.784845717038939));
#48652=CARTESIAN_POINT('Ctrl Pts',(0.909723729823394,50.0942406576125,-0.749441520262926));
#48653=CARTESIAN_POINT('Ctrl Pts',(0.937866933143905,50.0911061454729,-0.712390818452376));
#48654=CARTESIAN_POINT('Ctrl Pts',(0.966018410066383,50.0879707118425,-0.675329224393495));
#48655=CARTESIAN_POINT('Ctrl Pts',(0.991951141948852,50.084835278212,-0.636620632544208));
#48656=CARTESIAN_POINT('Ctrl Pts',(1.01548083214313,50.0816998445815,-0.596568304597124));
#48657=CARTESIAN_POINT('Ctrl Pts',(1.03905380048362,50.0785586439497,-0.55644230842533));
#48658=CARTESIAN_POINT('Ctrl Pts',(1.06021463686071,50.0754174433179,-0.514968148918674));
#48659=CARTESIAN_POINT('Ctrl Pts',(1.07882547523649,50.072276242686,-0.472472916134642));
#48660=CARTESIAN_POINT('Ctrl Pts',(1.09319094088995,50.0698515905089,-0.439671395071001));
#48661=CARTESIAN_POINT('Ctrl Pts',(1.10603804082557,50.0674269383317,-0.406262031775874));
#48662=CARTESIAN_POINT('Ctrl Pts',(1.11732377115968,50.0650022861545,-0.372401198845414));
#48663=CARTESIAN_POINT('',(0.00936663037036535,50.065,-1.17771275306651));
#48664=CARTESIAN_POINT('Origin',(0.,50.065,0.));
#48665=CARTESIAN_POINT('',(-1.17774995261315,50.1906328853284,0.000334095391369985));
#48666=CARTESIAN_POINT('Ctrl Pts',(-1.17774995261342,50.1906328852638,0.00033409442925833));
#48667=CARTESIAN_POINT('Ctrl Pts',(-1.17776337198618,50.1874545667427,-0.0469718892821487));
#48668=CARTESIAN_POINT('Ctrl Pts',(-1.17492228750547,50.1842762482216,-0.0942679073399217));
#48669=CARTESIAN_POINT('Ctrl Pts',(-1.16925640012487,50.1810979297006,-0.141189706661034));
#48670=CARTESIAN_POINT('Ctrl Pts',(-1.1635813242645,50.1779144568385,-0.188187599976752));
#48671=CARTESIAN_POINT('Ctrl Pts',(-1.15507236871164,50.1747309839765,-0.234809516368601));
#48672=CARTESIAN_POINT('Ctrl Pts',(-1.1438109064012,50.1715475111144,-0.280698544523596));
#48673=CARTESIAN_POINT('Ctrl Pts',(-1.13254022492645,50.1683614321113,-0.326625139601852));
#48674=CARTESIAN_POINT('Ctrl Pts',(-1.11851271896753,50.1651753531082,-0.371817128265236));
#48675=CARTESIAN_POINT('Ctrl Pts',(-1.1018593880314,50.1619892741051,-0.415933830683532));
#48676=CARTESIAN_POINT('Ctrl Pts',(-1.0851621986251,50.158794804195,-0.460166719532286));
#48677=CARTESIAN_POINT('Ctrl Pts',(-1.06582559866182,50.1556003342849,-0.503318164050547));
#48678=CARTESIAN_POINT('Ctrl Pts',(-1.04402789396152,50.1524058643748,-0.545069554396752));
#48679=CARTESIAN_POINT('Ctrl Pts',(-1.02576079236807,50.1497288069879,-0.580058416738353));
#48680=CARTESIAN_POINT('Ctrl Pts',(-1.00576619787879,50.147051749601,-0.614064346226491));
#48681=CARTESIAN_POINT('Ctrl Pts',(-0.98417163956616,50.1443746922142,-0.646916722904622));
#48682=CARTESIAN_POINT('Ctrl Pts',(-0.957493382250771,50.1410674133719,
-0.687503066267285));
#48683=CARTESIAN_POINT('Ctrl Pts',(-0.928250578353563,50.1377601345296,
-0.726512868370853));
#48684=CARTESIAN_POINT('Ctrl Pts',(-0.89665288202166,50.1344528556874,-0.763615526074641));
#48685=CARTESIAN_POINT('Ctrl Pts',(-0.865550916610211,50.1311974641842,
-0.800136086448879));
#48686=CARTESIAN_POINT('Ctrl Pts',(-0.832167754761042,50.1279420726811,
-0.834808491110521));
#48687=CARTESIAN_POINT('Ctrl Pts',(-0.796747002603892,50.124686681178,-0.867346111043172));
#48688=CARTESIAN_POINT('Ctrl Pts',(-0.761373237829212,50.1214356081129,
-0.899840568211077));
#48689=CARTESIAN_POINT('Ctrl Pts',(-0.723967625987618,50.1181845350479,
-0.930205506818803));
#48690=CARTESIAN_POINT('Ctrl Pts',(-0.684811448333999,50.1149334619828,
-0.958190139132464));
#48691=CARTESIAN_POINT('Ctrl Pts',(-0.645693425711961,50.1116855568673,
-0.98614750232555));
#48692=CARTESIAN_POINT('Ctrl Pts',(-0.604828645240271,50.1084376517518,
-1.01172885962529));
#48693=CARTESIAN_POINT('Ctrl Pts',(-0.562530619339646,50.1051897466363,
-1.03472429410223));
#48694=CARTESIAN_POINT('Ctrl Pts',(-0.518914121840659,50.1018406010833,
-1.05843651917646));
#48695=CARTESIAN_POINT('Ctrl Pts',(-0.473773979815151,50.0984914555303,
-1.07939853978092));
#48696=CARTESIAN_POINT('Ctrl Pts',(-0.427483669944292,50.0951423099773,
-1.09743007723999));
#48697=CARTESIAN_POINT('Ctrl Pts',(-0.38261975794465,50.0918963655931,-1.11490598768514));
#48698=CARTESIAN_POINT('Ctrl Pts',(-0.336676080022107,50.088650421209,-1.12962928489099));
#48699=CARTESIAN_POINT('Ctrl Pts',(-0.290012540618924,50.0854044768249,
-1.14148490519312));
#48700=CARTESIAN_POINT('Ctrl Pts',(-0.241123578700135,50.0820037306874,
-1.15390592976365));
#48701=CARTESIAN_POINT('Ctrl Pts',(-0.191444948498638,50.0786029845499,
-1.16317864132221));
#48702=CARTESIAN_POINT('Ctrl Pts',(-0.141404631578315,50.0752022384124,
-1.16923042753266));
#48703=CARTESIAN_POINT('Ctrl Pts',(-0.0913643146579857,50.071801492275,
-1.17528221374311));
#48704=CARTESIAN_POINT('Ctrl Pts',(-0.0409629669169127,50.0684007461375,
-1.17811303635567));
#48705=CARTESIAN_POINT('Ctrl Pts',(0.00936663037036528,50.065,-1.17771275306651));
#48706=CARTESIAN_POINT('Ctrl Pts',(0.188938462403167,50.3284861847587,1.16249615910106));
#48707=CARTESIAN_POINT('Ctrl Pts',(0.14248009936766,50.3253116014759,1.17004695538454));
#48708=CARTESIAN_POINT('Ctrl Pts',(0.0956040622939412,50.3221370181931,
1.17480267720841));
#48709=CARTESIAN_POINT('Ctrl Pts',(0.0486718089546751,50.3189624349103,
1.17674386232225));
#48710=CARTESIAN_POINT('Ctrl Pts',(0.0016509726456754,50.3157818597138,
1.17868871135439));
#48711=CARTESIAN_POINT('Ctrl Pts',(-0.0454257344863767,50.3126012845172,
1.17780842344634));
#48712=CARTESIAN_POINT('Ctrl Pts',(-0.0921978227533305,50.3094207093207,
1.17413569231991));
#48713=CARTESIAN_POINT('Ctrl Pts',(-0.12306295890079,50.3073218317613,1.17171203858857));
#48714=CARTESIAN_POINT('Ctrl Pts',(-0.153795520395974,50.3052229542019,
1.16807342677931));
#48715=CARTESIAN_POINT('Ctrl Pts',(-0.184294402276791,50.3031240766425,
1.16324143486614));
#48716=CARTESIAN_POINT('Ctrl Pts',(-0.232352616204662,50.2998167978003,
1.15562748685427));
#48717=CARTESIAN_POINT('Ctrl Pts',(-0.280048180995003,50.296509518958,1.14501289851391));
#48718=CARTESIAN_POINT('Ctrl Pts',(-0.32697913045126,50.2932022401158,1.13145026879193));
#48719=CARTESIAN_POINT('Ctrl Pts',(-0.372007028384608,50.2900290715378,
1.11843760414516));
#48720=CARTESIAN_POINT('Ctrl Pts',(-0.416330533826876,50.2868559029599,
1.10271157111116));
#48721=CARTESIAN_POINT('Ctrl Pts',(-0.459602722373217,50.283682734382,1.08437096977332));
#48722=CARTESIAN_POINT('Ctrl Pts',(-0.502832382507399,50.2805126844312,
1.06604839379262));
#48723=CARTESIAN_POINT('Ctrl Pts',(-0.545012260170822,50.2773426344804,
1.04511655198512));
#48724=CARTESIAN_POINT('Ctrl Pts',(-0.58581260118302,50.2741725845297,1.02172337684678));
#48725=CARTESIAN_POINT('Ctrl Pts',(-0.626590765441402,50.2710042576384,
0.998342916913098));
#48726=CARTESIAN_POINT('Ctrl Pts',(-0.665990395956384,50.2678359307472,
0.972504050473419));
#48727=CARTESIAN_POINT('Ctrl Pts',(-0.703706131398171,50.264667603856,0.944400732280858));
#48728=CARTESIAN_POINT('Ctrl Pts',(-0.741417932828378,50.2614996074431,
0.916300345458397));
#48729=CARTESIAN_POINT('Ctrl Pts',(-0.777445742742863,50.2583316110302,
0.885936310231308));
#48730=CARTESIAN_POINT('Ctrl Pts',(-0.811515247945782,50.2551636146174,
0.853544412934381));
#48731=CARTESIAN_POINT('Ctrl Pts',(-0.845619973557182,50.2519923431899,
0.821119029508215));
#48732=CARTESIAN_POINT('Ctrl Pts',(-0.877761951698038,50.2488210717624,
0.78666198668075));
#48733=CARTESIAN_POINT('Ctrl Pts',(-0.907703359196014,50.2456498003349,
0.750446316670467));
#48734=CARTESIAN_POINT('Ctrl Pts',(-0.937663178849942,50.2424765787672,
0.714208376212005));
#48735=CARTESIAN_POINT('Ctrl Pts',(-0.965419406449462,50.2393033571994,
0.676210106592592));
#48736=CARTESIAN_POINT('Ctrl Pts',(-0.990776454845308,50.2361301356317,
0.636755116998806));
#48737=CARTESIAN_POINT('Ctrl Pts',(-1.01617991710229,50.2329511057592,0.597227908494544));
#48738=CARTESIAN_POINT('Ctrl Pts',(-1.03917516977404,50.2297720758867,0.556239147564299));
#48739=CARTESIAN_POINT('Ctrl Pts',(-1.05961254906646,50.2265930460142,0.514117018159183));
#48740=CARTESIAN_POINT('Ctrl Pts',(-1.06570633582303,50.2256451588189,0.501557517713692));
#48741=CARTESIAN_POINT('Ctrl Pts',(-1.0715730451748,50.2246972716236,0.48889738151205));
#48742=CARTESIAN_POINT('Ctrl Pts',(-1.07720955856848,50.2237493844284,0.476145596880503));
#48743=CARTESIAN_POINT('Ctrl Pts',(-1.09783991697972,50.2202799963145,0.429472437613947));
#48744=CARTESIAN_POINT('Ctrl Pts',(-1.11546555051765,50.2168106082007,0.381383059316153));
#48745=CARTESIAN_POINT('Ctrl Pts',(-1.12990975478779,50.2133412200869,0.332263462534478));
#48746=CARTESIAN_POINT('Ctrl Pts',(-1.14430397109725,50.2098838387013,0.283313857012021));
#48747=CARTESIAN_POINT('Ctrl Pts',(-1.15553853907606,50.2064264573158,0.233341485789629));
#48748=CARTESIAN_POINT('Ctrl Pts',(-1.16348484842626,50.2029690759303,0.182751388455792));
#48749=CARTESIAN_POINT('Ctrl Pts',(-1.17139080064078,50.1995292536409,0.132418224414226));
#48750=CARTESIAN_POINT('Ctrl Pts',(-1.17604165465704,50.1960894313515,0.0814739523451495));
#48751=CARTESIAN_POINT('Ctrl Pts',(-1.17735926665214,50.1926496090621,0.0303351236742758));
#48752=CARTESIAN_POINT('Ctrl Pts',(-1.17761676632884,50.1919773678176,0.0203411103391975));
#48753=CARTESIAN_POINT('Ctrl Pts',(-1.17774711429415,50.191305126573,0.0103397109874767));
#48754=CARTESIAN_POINT('Ctrl Pts',(-1.17774995261315,50.1906328853284,0.000334095391379412));
#48755=CARTESIAN_POINT('Origin',(3.28582941601228E-17,50.065,0.));
#48756=CARTESIAN_POINT('',(-1.30071912068084,50.065,0.670792083357623));
#48757=CARTESIAN_POINT('',(-1.4635,50.065,1.79227059055215E-16));
#48758=CARTESIAN_POINT('Origin',(0.,50.065,0.));
#48759=CARTESIAN_POINT('Ctrl Pts',(-1.30071912068084,50.065,0.670792083357622));
#48760=CARTESIAN_POINT('Ctrl Pts',(-1.31175604994526,50.065,0.643640642407746));
#48761=CARTESIAN_POINT('Ctrl Pts',(-1.32190228759372,50.065,0.616162032086531));
#48762=CARTESIAN_POINT('Ctrl Pts',(-1.33112168336828,50.065,0.588379227984466));
#48763=CARTESIAN_POINT('Ctrl Pts',(-1.34927016508087,50.065,0.533688473351472));
#48764=CARTESIAN_POINT('Ctrl Pts',(-1.36383020120747,50.065,0.477818733970761));
#48765=CARTESIAN_POINT('Ctrl Pts',(-1.37486275654977,50.065,0.421110295908625));
#48766=CARTESIAN_POINT('Ctrl Pts',(-1.38091979747305,50.065,0.389976499668264));
#48767=CARTESIAN_POINT('Ctrl Pts',(-1.38591268206054,50.065,0.358589878940197));
#48768=CARTESIAN_POINT('Ctrl Pts',(-1.38984515858309,50.065,0.327007742108425));
#48769=CARTESIAN_POINT('Ctrl Pts',(-1.39224930977373,50.065,0.307699748422531));
#48770=CARTESIAN_POINT('Ctrl Pts',(-1.3942544329935,50.065,0.288338607708039));
#48771=CARTESIAN_POINT('Ctrl Pts',(-1.3958626601646,50.065,0.268947491632431));
#48772=CARTESIAN_POINT('Ctrl Pts',(-1.40061569214788,50.065,0.211638053914574));
#48773=CARTESIAN_POINT('Ctrl Pts',(-1.40190929233838,50.065,0.154037716185528));
#48774=CARTESIAN_POINT('Ctrl Pts',(-1.39979622763592,50.065,0.0964884123102473));
#48775=CARTESIAN_POINT('Ctrl Pts',(-1.39799633646646,50.065,0.0474683876358261));
#48776=CARTESIAN_POINT('Ctrl Pts',(-1.39372374270588,50.065,-0.00151496550527628));
#48777=CARTESIAN_POINT('Ctrl Pts',(-1.38698332842043,50.065,-0.0502392570618477));
#48778=CARTESIAN_POINT('Ctrl Pts',(-1.38548901145288,50.065,-0.061041194824286));
#48779=CARTESIAN_POINT('Ctrl Pts',(-1.38387401566659,50.065,-0.0718248289893012));
#48780=CARTESIAN_POINT('Ctrl Pts',(-1.38213998134003,50.065,-0.0825802196834237));
#48781=CARTESIAN_POINT('Ctrl Pts',(-1.37319554758143,50.065,-0.138058290756452));
#48782=CARTESIAN_POINT('Ctrl Pts',(-1.36107927502691,50.065,-0.192849000747329));
#48783=CARTESIAN_POINT('Ctrl Pts',(-1.34584240689984,50.065,-0.246634504257576));
#48784=CARTESIAN_POINT('Ctrl Pts',(-1.3309686912773,50.065,-0.299138094703773));
#48785=CARTESIAN_POINT('Ctrl Pts',(-1.31312085741118,50.065,-0.350684738983978));
#48786=CARTESIAN_POINT('Ctrl Pts',(-1.29230435568534,50.065,-0.400954342832866));
#48787=CARTESIAN_POINT('Ctrl Pts',(-1.28027653029496,50.065,-0.430000242355331));
#48788=CARTESIAN_POINT('Ctrl Pts',(-1.26725685158702,50.065,-0.458619267214444));
#48789=CARTESIAN_POINT('Ctrl Pts',(-1.25324064993564,50.065,-0.486744051974305));
#48790=CARTESIAN_POINT('Ctrl Pts',(-1.24638872355449,50.065,-0.500493066111903));
#48791=CARTESIAN_POINT('Ctrl Pts',(-1.23929858571003,50.065,-0.514123894689191));
#48792=CARTESIAN_POINT('Ctrl Pts',(-1.23196935359747,50.065,-0.527628224413549));
#48793=CARTESIAN_POINT('Ctrl Pts',(-1.22699450677309,50.065,-0.536794528715686));
#48794=CARTESIAN_POINT('Ctrl Pts',(-1.2219086199582,50.065,-0.545904071351034));
#48795=CARTESIAN_POINT('Ctrl Pts',(-1.21671412257452,50.065,-0.554949372359807));
#48796=CARTESIAN_POINT('Ctrl Pts',(-1.19038939303419,50.065,-0.600789245802538));
#48797=CARTESIAN_POINT('Ctrl Pts',(-1.16138549452255,50.065,-0.644797644261427));
#48798=CARTESIAN_POINT('Ctrl Pts',(-1.12972143997519,50.065,-0.686686087702281));
#48799=CARTESIAN_POINT('Ctrl Pts',(-1.1202930926426,50.065,-0.699158867945605));
#48800=CARTESIAN_POINT('Ctrl Pts',(-1.11062862879451,50.065,-0.711443459549966));
#48801=CARTESIAN_POINT('Ctrl Pts',(-1.10072790598129,50.065,-0.723531608836915));
#48802=CARTESIAN_POINT('Ctrl Pts',(-1.06670404828826,50.065,-0.765072562853135));
#48803=CARTESIAN_POINT('Ctrl Pts',(-1.02989193273851,50.065,-0.804297171032527));
#48804=CARTESIAN_POINT('Ctrl Pts',(-0.990590001990912,50.065,-0.841070267115875));
#48805=CARTESIAN_POINT('Ctrl Pts',(-0.971180658196642,50.065,-0.85923074042303));
#48806=CARTESIAN_POINT('Ctrl Pts',(-0.951163683276724,50.065,-0.876792598798188));
#48807=CARTESIAN_POINT('Ctrl Pts',(-0.930573455824569,50.065,-0.89373515421317));
#48808=CARTESIAN_POINT('Ctrl Pts',(-0.916787514647906,50.065,-0.905078840089203));
#48809=CARTESIAN_POINT('Ctrl Pts',(-0.902744577782523,50.065,-0.916144842788307));
#48810=CARTESIAN_POINT('Ctrl Pts',(-0.888454863816197,50.065,-0.926926174066913));
#48811=CARTESIAN_POINT('Ctrl Pts',(-0.880246416042113,50.065,-0.933119299761667));
#48812=CARTESIAN_POINT('Ctrl Pts',(-0.871963127969767,50.065,-0.939213453383781));
#48813=CARTESIAN_POINT('Ctrl Pts',(-0.863611899391003,50.065,-0.945204552503321));
#48814=CARTESIAN_POINT('Ctrl Pts',(-0.82097856900588,50.065,-0.975789334817011));
#48815=CARTESIAN_POINT('Ctrl Pts',(-0.776538365170856,50.065,-1.00372098297481));
#48816=CARTESIAN_POINT('Ctrl Pts',(-0.730581585765392,50.065,-1.02889132098778));
#48817=CARTESIAN_POINT('Ctrl Pts',(-0.6849361843158,50.065,-1.05389111858212));
#48818=CARTESIAN_POINT('Ctrl Pts',(-0.637793529996918,50.065,-1.07616713862166));
#48819=CARTESIAN_POINT('Ctrl Pts',(-0.5894257667048,50.065,-1.09556439483884));
#48820=CARTESIAN_POINT('Ctrl Pts',(-0.564948289877972,50.065,-1.10538076543867));
#48821=CARTESIAN_POINT('Ctrl Pts',(-0.540156966365709,50.065,-1.11445906184859));
#48822=CARTESIAN_POINT('Ctrl Pts',(-0.515087268773155,50.065,-1.12277406719407));
#48823=CARTESIAN_POINT('Ctrl Pts',(-0.496757115239239,50.065,-1.12885373066249));
#48824=CARTESIAN_POINT('Ctrl Pts',(-0.478278145159383,50.065,-1.134525262181));
#48825=CARTESIAN_POINT('Ctrl Pts',(-0.459664493506921,50.065,-1.13977758010901));
#48826=CARTESIAN_POINT('Ctrl Pts',(-0.45066760368625,50.065,-1.14231628270127));
#48827=CARTESIAN_POINT('Ctrl Pts',(-0.441640205098046,50.065,-1.14475666360343));
#48828=CARTESIAN_POINT('Ctrl Pts',(-0.432596391441415,50.065,-1.14709452097211));
#48829=CARTESIAN_POINT('Ctrl Pts',(-0.383773881833472,50.065,-1.15971530996425));
#48830=CARTESIAN_POINT('Ctrl Pts',(-0.334376697505691,50.065,-1.16938014447876));
#48831=CARTESIAN_POINT('Ctrl Pts',(-0.284657998630276,50.065,-1.17596097943796));
#48832=CARTESIAN_POINT('Ctrl Pts',(-0.23594412541215,50.065,-1.18240881429936));
#48833=CARTESIAN_POINT('Ctrl Pts',(-0.186920658325916,50.065,-1.18589607879924));
#48834=CARTESIAN_POINT('Ctrl Pts',(-0.137832125061594,50.065,-1.18625310484368));
#48835=CARTESIAN_POINT('Ctrl Pts',(-0.088743591797191,50.065,-1.18661013088813));
#48836=CARTESIAN_POINT('Ctrl Pts',(-0.0395890858340499,50.065,-1.18383710324689));
#48837=CARTESIAN_POINT('Ctrl Pts',(0.009366630370399,50.065,-1.17771275306651));
#48838=CARTESIAN_POINT('Ctrl Pts',(1.11912387040083,50.065,-0.3729656372709));
#48839=CARTESIAN_POINT('Ctrl Pts',(1.13246075041995,50.065,-0.344966336154387));
#48840=CARTESIAN_POINT('Ctrl Pts',(1.14459340453453,50.065,-0.316466733140529));
#48841=CARTESIAN_POINT('Ctrl Pts',(1.15546879160855,50.065,-0.28752483843055));
#48842=CARTESIAN_POINT('Ctrl Pts',(1.17244188610288,50.065,-0.242355548324976));
#48843=CARTESIAN_POINT('Ctrl Pts',(1.18635529783476,50.065,-0.196110283010327));
#48844=CARTESIAN_POINT('Ctrl Pts',(1.19732570794754,50.065,-0.149071507418727));
#48845=CARTESIAN_POINT('Ctrl Pts',(1.20207169098707,50.065,-0.128721745754101));
#48846=CARTESIAN_POINT('Ctrl Pts',(1.20626631636867,50.065,-0.108223099821439));
#48847=CARTESIAN_POINT('Ctrl Pts',(1.20991649016097,50.065,-0.0875970128177899));
#48848=CARTESIAN_POINT('Ctrl Pts',(1.21236509669315,50.065,-0.0737606383752849));
#48849=CARTESIAN_POINT('Ctrl Pts',(1.21456884754754,50.065,-0.059864243936097));
#48850=CARTESIAN_POINT('Ctrl Pts',(1.21652661323577,50.065,-0.0459384094572504));
#48851=CARTESIAN_POINT('Ctrl Pts',(1.2235769855708,50.065,0.0042117789653206));
#48852=CARTESIAN_POINT('Ctrl Pts',(1.22745360466983,50.065,0.0548056738949035));
#48853=CARTESIAN_POINT('Ctrl Pts',(1.22828254246297,50.065,0.105533114130644));
#48854=CARTESIAN_POINT('Ctrl Pts',(1.22886776554746,50.065,0.141346258721905));
#48855=CARTESIAN_POINT('Ctrl Pts',(1.22793295114377,50.065,0.177226698754145));
#48856=CARTESIAN_POINT('Ctrl Pts',(1.22550808937998,50.065,0.213071201673675));
#48857=CARTESIAN_POINT('Ctrl Pts',(1.22464231733817,50.065,0.225869114092314));
#48858=CARTESIAN_POINT('Ctrl Pts',(1.22358648781239,50.065,0.238662474148506));
#48859=CARTESIAN_POINT('Ctrl Pts',(1.22234159897063,50.065,0.251446654317747));
#48860=CARTESIAN_POINT('Ctrl Pts',(1.22143521697024,50.065,0.260754594437777));
#48861=CARTESIAN_POINT('Ctrl Pts',(1.22042868456239,50.065,0.270056192665202));
#48862=CARTESIAN_POINT('Ctrl Pts',(1.21932376301989,50.065,0.27934010984953));
#48863=CARTESIAN_POINT('Ctrl Pts',(1.21304427883545,50.065,0.332102418200232));
#48864=CARTESIAN_POINT('Ctrl Pts',(1.20358324825889,50.065,0.384376692221464));
#48865=CARTESIAN_POINT('Ctrl Pts',(1.19107048812719,50.065,0.435835777877265));
#48866=CARTESIAN_POINT('Ctrl Pts',(1.17861838364559,50.065,0.48704541542878));
#48867=CARTESIAN_POINT('Ctrl Pts',(1.16314397006523,50.065,0.537448933599227));
#48868=CARTESIAN_POINT('Ctrl Pts',(1.14472492208604,50.065,0.586733910875349));
#48869=CARTESIAN_POINT('Ctrl Pts',(1.13394477086779,50.065,0.615579023197392));
#48870=CARTESIAN_POINT('Ctrl Pts',(1.12215501838417,50.065,0.64404108706711));
#48871=CARTESIAN_POINT('Ctrl Pts',(1.10936337857097,50.065,0.672056579431857));
#48872=CARTESIAN_POINT('Ctrl Pts',(1.10160261146699,50.065,0.689053752172891));
#48873=CARTESIAN_POINT('Ctrl Pts',(1.09347294523412,50.065,0.70588652224452));
#48874=CARTESIAN_POINT('Ctrl Pts',(1.08497507156082,50.065,0.722540339201735));
#48875=CARTESIAN_POINT('Ctrl Pts',(1.08052819384105,50.065,0.731255164865588));
#48876=CARTESIAN_POINT('Ctrl Pts',(1.07598037774297,50.065,0.739920924916033));
#48877=CARTESIAN_POINT('Ctrl Pts',(1.07133886425922,50.065,0.748522809552601));
#48878=CARTESIAN_POINT('Ctrl Pts',(1.04531350200145,50.065,0.796754310882876));
#48879=CARTESIAN_POINT('Ctrl Pts',(1.01629564612237,50.065,0.843079360691641));
#48880=CARTESIAN_POINT('Ctrl Pts',(0.984386029779273,50.065,0.887164229561829));
#48881=CARTESIAN_POINT('Ctrl Pts',(0.979086611727012,50.065,0.894485663558722));
#48882=CARTESIAN_POINT('Ctrl Pts',(0.97370731930311,50.065,0.901745301457201));
#48883=CARTESIAN_POINT('Ctrl Pts',(0.968248475848336,50.065,0.908941595055685));
#48884=CARTESIAN_POINT('Ctrl Pts',(0.936337800817732,50.065,0.951008854970467));
#48885=CARTESIAN_POINT('Ctrl Pts',(0.901712641810621,50.065,0.990913516768476));
#48886=CARTESIAN_POINT('Ctrl Pts',(0.864670234321161,50.065,1.02859685862274));
#48887=CARTESIAN_POINT('Ctrl Pts',(0.845706643529314,50.065,1.04788857109572));
#48888=CARTESIAN_POINT('Ctrl Pts',(0.826108741599738,50.065,1.06659771666816));
#48889=CARTESIAN_POINT('Ctrl Pts',(0.805912002498264,50.065,1.08471359677496));
#48890=CARTESIAN_POINT('Ctrl Pts',(0.793586884256897,50.065,1.09576886481803));
#48891=CARTESIAN_POINT('Ctrl Pts',(0.781038699666901,50.065,1.10660315596534));
#48892=CARTESIAN_POINT('Ctrl Pts',(0.768275050659485,50.065,1.11721363233496));
#48893=CARTESIAN_POINT('Ctrl Pts',(0.760318925263968,50.065,1.12382759362878));
#48894=CARTESIAN_POINT('Ctrl Pts',(0.7522775593948,50.065,1.13035566915275));
#48895=CARTESIAN_POINT('Ctrl Pts',(0.744166470702853,50.065,1.13678655984908));
#48896=CARTESIAN_POINT('Ctrl Pts',(0.70143902438249,50.065,1.17066308955491));
#48897=CARTESIAN_POINT('Ctrl Pts',(0.656704573419184,50.065,1.2019097711863));
#48898=CARTESIAN_POINT('Ctrl Pts',(0.610290795174932,50.065,1.23047751400324));
#48899=CARTESIAN_POINT('Ctrl Pts',(0.562526701200975,50.065,1.25987637796452));
#48900=CARTESIAN_POINT('Ctrl Pts',(0.512983462755402,50.065,1.28643883982959));
#48901=CARTESIAN_POINT('Ctrl Pts',(0.46197321398113,50.065,1.31007946992396));
#48902=CARTESIAN_POINT('Ctrl Pts',(0.433134381054957,50.065,1.32344478763841));
#48903=CARTESIAN_POINT('Ctrl Pts',(0.40382590289864,50.065,1.33587558469587));
#48904=CARTESIAN_POINT('Ctrl Pts',(0.374099449030773,50.065,1.34735081798353));
#48905=CARTESIAN_POINT('Ctrl Pts',(0.355628125637758,50.065,1.35448125964363));
#48906=CARTESIAN_POINT('Ctrl Pts',(0.336995357365496,50.065,1.3612426655871));
#48907=CARTESIAN_POINT('Ctrl Pts',(0.318213056572565,50.065,1.36762909032308));
#48908=CARTESIAN_POINT('Ctrl Pts',(0.308740505021669,50.065,1.37084998100119));
#48909=CARTESIAN_POINT('Ctrl Pts',(0.299229914316878,50.065,1.37397548289385));
#48910=CARTESIAN_POINT('Ctrl Pts',(0.289682784609941,50.065,1.37700476219547));
#48911=CARTESIAN_POINT('Ctrl Pts',(0.279575173142051,50.065,1.38021188089485));
#48912=CARTESIAN_POINT('Ctrl Pts',(0.2694357466268,50.065,1.38330822235196));
#48913=CARTESIAN_POINT('Ctrl Pts',(0.259269706426227,50.065,1.38629245527359));
#48914=CARTESIAN_POINT('Ctrl Pts',(0.203372665229807,50.065,1.40270098674391));
#48915=CARTESIAN_POINT('Ctrl Pts',(0.146643819123119,50.065,1.41573293027852));
#48916=CARTESIAN_POINT('Ctrl Pts',(0.089415544266844,50.065,1.42530658648151));
#48917=CARTESIAN_POINT('Ctrl Pts',(0.0313884653490651,50.065,1.43501387375197));
#48918=CARTESIAN_POINT('Ctrl Pts',(-0.0271531028235179,50.065,1.44116635899906));
#48919=CARTESIAN_POINT('Ctrl Pts',(-0.0858909126126426,50.065,1.44363247257722));
#48920=CARTESIAN_POINT('Ctrl Pts',(-0.144628722401879,50.065,1.44609858615538));
#48921=CARTESIAN_POINT('Ctrl Pts',(-0.203563913133846,50.065,1.44487896824704));
#48922=CARTESIAN_POINT('Ctrl Pts',(-0.262389908308771,50.065,1.43978602091342));
#48923=CARTESIAN_POINT('Origin',(0.,50.065,0.));
#48924=CARTESIAN_POINT('Ctrl Pts',(-0.509296898212844,55.7812034156616,
1.05958297275613));
#48925=CARTESIAN_POINT('Ctrl Pts',(-0.861591212604499,55.7547451849235,
0.890249936843907));
#48926=CARTESIAN_POINT('Ctrl Pts',(-1.37785557857217,55.7018287234474,0.175325859793372));
#48927=CARTESIAN_POINT('Ctrl Pts',(-0.89405509938618,55.6224540312332,-1.06476771329504));
#48928=CARTESIAN_POINT('Ctrl Pts',(0.409241656719022,55.543079339019,-1.32750887748838));
#48929=CARTESIAN_POINT('Ctrl Pts',(1.33736108858238,55.4637046468048,-0.376885391722574));
#48930=CARTESIAN_POINT('Ctrl Pts',(1.04199119975101,55.3843299545907,0.919363910817131));
#48931=CARTESIAN_POINT('Ctrl Pts',(-0.20709067843855,55.3049552623765,1.3739204743444));
#48932=CARTESIAN_POINT('Ctrl Pts',(-1.26657263663979,55.2255805701623,0.57137806271837));
#48933=CARTESIAN_POINT('Ctrl Pts',(-1.16704611942123,55.1462058779482,-0.754135090264633));
#48934=CARTESIAN_POINT('Ctrl Pts',(0.00047956154262669,55.0668311857339,
-1.38948211737794));
#48935=CARTESIAN_POINT('Ctrl Pts',(1.16755463529987,54.9874564935198,-0.753324638459543));
#48936=CARTESIAN_POINT('Ctrl Pts',(1.26619427179722,54.9080818013055,0.572220836148192));
#48937=CARTESIAN_POINT('Ctrl Pts',(0.206123279084574,54.8287071090914,1.37411455837363));
#48938=CARTESIAN_POINT('Ctrl Pts',(-1.04257172449213,54.7493324168772,0.91854502704819));
#48939=CARTESIAN_POINT('Ctrl Pts',(-1.33719926070647,54.669957724663,-0.377596321548186));
#48940=CARTESIAN_POINT('Ctrl Pts',(-0.40814140684798,54.5905830324488,-1.32819448115672));
#48941=CARTESIAN_POINT('Ctrl Pts',(0.894410699853024,54.5112083402347,-1.06334845704124));
#48942=CARTESIAN_POINT('Ctrl Pts',(1.37847835230742,54.4318336480205,0.174579051125748));
#48943=CARTESIAN_POINT('Ctrl Pts',(0.601086036540525,54.3524589558063,1.25274733591148));
#48944=CARTESIAN_POINT('Ctrl Pts',(-0.726366352456438,54.2730842635921,
1.18451352739661));
#48945=CARTESIAN_POINT('Ctrl Pts',(-1.38911333142688,54.193709571378,0.032319008359879));
#48946=CARTESIAN_POINT('Ctrl Pts',(-0.780668207941864,54.1143348791637,
-1.14945095732061));
#48947=CARTESIAN_POINT('Ctrl Pts',(0.542174529980675,54.0349601869497,-1.27934637292781));
#48948=CARTESIAN_POINT('Ctrl Pts',(1.36886770346268,53.9555854947353,-0.238498577598694));
#48949=CARTESIAN_POINT('Ctrl Pts',(0.942895765841905,53.8762108025213,1.02060175121614));
#48950=CARTESIAN_POINT('Ctrl Pts',(-0.345929919276582,53.796836110307,1.34573877552148));
#48951=CARTESIAN_POINT('Ctrl Pts',(-1.31819152809999,53.717461418093,0.439376212287943));
#48952=CARTESIAN_POINT('Ctrl Pts',(-1.08416232315526,53.6380867258786,-0.869064104425588));
#48953=CARTESIAN_POINT('Ctrl Pts',(0.141995129440038,53.5587120336646,-1.38221479659209));
#48954=CARTESIAN_POINT('Ctrl Pts',(1.2382113583717,53.4793373414503,-0.630486314404458));
#48955=CARTESIAN_POINT('Ctrl Pts',(1.2013274610036,53.3999626492361,0.698206768858064));
#48956=CARTESIAN_POINT('Ctrl Pts',(0.0650962764719148,53.320587957022,1.38796355696017));
#48957=CARTESIAN_POINT('Ctrl Pts',(-1.13070518949629,53.2412132648078,0.807580420204971));
#48958=CARTESIAN_POINT('Ctrl Pts',(-1.29178654540564,53.1618385725937,-0.511827980634577));
#48959=CARTESIAN_POINT('Ctrl Pts',(-0.270740562688289,53.0824638803794,
-1.36285725898538));
#48960=CARTESIAN_POINT('Ctrl Pts',(0.99806293226542,53.0030891881654,-0.966721647575289));
#48961=CARTESIAN_POINT('Ctrl Pts',(1.3535286299656,52.923714495951,0.314071024636275));
#48962=CARTESIAN_POINT('Ctrl Pts',(0.470366163602632,52.844339803737,1.30745402702759));
#48963=CARTESIAN_POINT('Ctrl Pts',(-0.843233284116505,52.7649651115227,
1.10437221497646));
#48964=CARTESIAN_POINT('Ctrl Pts',(-1.38518116018734,52.6855904193086,-0.109332127545164));
#48965=CARTESIAN_POINT('Ctrl Pts',(-0.659535311713787,52.6062157270943,
-1.22298550001824));
#48966=CARTESIAN_POINT('Ctrl Pts',(0.669658178237574,52.5268410348802,-1.21747208796736));
#48967=CARTESIAN_POINT('Ctrl Pts',(1.38604048598882,52.447466342666,-0.0978372722456281));
#48968=CARTESIAN_POINT('Ctrl Pts',(0.834042691206619,52.3680916504517,1.11132945155648));
#48969=CARTESIAN_POINT('Ctrl Pts',(-0.481196267839791,52.2887169582377,
1.30350700516717));
#48970=CARTESIAN_POINT('Ctrl Pts',(-1.35608750414732,52.2093422660234,0.302831705153106));
#48971=CARTESIAN_POINT('Ctrl Pts',(-0.99000892405737,52.1299675738093,-0.974968046125547));
#48972=CARTESIAN_POINT('Ctrl Pts',(0.282037146610221,52.0505928815951,-1.36056437147411));
#48973=CARTESIAN_POINT('Ctrl Pts',(1.29598808285279,51.971218189381,-0.501094051981872));
#48974=CARTESIAN_POINT('Ctrl Pts',(1.12396681059968,51.8918434971667,0.816932659262804));
#48975=CARTESIAN_POINT('Ctrl Pts',(-0.0766082126106224,51.8124688049526,
1.38737577629275));
#48976=CARTESIAN_POINT('Ctrl Pts',(-1.20707825824582,51.7330941127383,0.688216850016528));
#48977=CARTESIAN_POINT('Ctrl Pts',(-1.23293840873169,51.6537194205242,-0.640736487273394));
#48978=CARTESIAN_POINT('Ctrl Pts',(-0.130523751273304,51.57434472831,-1.38334519369534));
#48979=CARTESIAN_POINT('Ctrl Pts',(1.09133452682926,51.4949700360959,-0.860040267375685));
#48980=CARTESIAN_POINT('Ctrl Pts',(1.3145012484704,51.4155953438816,0.450296436408177));
#48981=CARTESIAN_POINT('Ctrl Pts',(0.334754072362915,51.3362206516676,1.3485622537132));
#48982=CARTESIAN_POINT('Ctrl Pts',(-0.951329854768783,51.2568459594532,
1.01274453599346));
#48983=CARTESIAN_POINT('Ctrl Pts',(-1.36684228725746,51.1774712672391,-0.249845965837834));
#48984=CARTESIAN_POINT('Ctrl Pts',(-0.531542350422215,51.098096575025,-1.28380041172025));
#48985=CARTESIAN_POINT('Ctrl Pts',(0.790176083470376,51.0187218828107,-1.14293454879374));
#48986=CARTESIAN_POINT('Ctrl Pts',(1.38879899296093,50.9393471905966,0.0438403513319658));
#48987=CARTESIAN_POINT('Ctrl Pts',(0.716511864201961,50.8599724983823,1.19050098100684));
#48988=CARTESIAN_POINT('Ctrl Pts',(-0.611451749480356,50.7805978061683,
1.24771292473461));
#48989=CARTESIAN_POINT('Ctrl Pts',(-1.3798910848444,50.701223113954,0.163147090662219));
#48990=CARTESIAN_POINT('Ctrl Pts',(-0.885535284470352,50.6218484217398,
-1.07075038846525));
#48991=CARTESIAN_POINT('Ctrl Pts',(0.419099779724909,50.5424737295257,-1.32472615794866));
#48992=CARTESIAN_POINT('Ctrl Pts',(1.34037590341986,50.4630990373115,-0.366562543644245));
#48993=CARTESIAN_POINT('Ctrl Pts',(1.03473860200598,50.3837243450974,0.92730432182043));
#48994=CARTESIAN_POINT('Ctrl Pts',(-0.217166894820808,50.3043496528831,
1.3720776556735));
#48995=CARTESIAN_POINT('Ctrl Pts',(-1.27158730416588,50.224974960669,0.562254863827906));
#48996=CARTESIAN_POINT('Ctrl Pts',(-1.15984632322935,50.1455937665709,-0.76428168828827));
#48997=CARTESIAN_POINT('Ctrl Pts',(-0.381323777793448,50.092670803211,-1.17880055994548));
#48998=CARTESIAN_POINT('Ctrl Pts',(0.00963790343894936,50.0662060705889,
-1.17558773000307));
#48999=CARTESIAN_POINT('Ctrl Pts',(-0.551142003322691,55.7254357270455,
1.1466409560723));
#49000=CARTESIAN_POINT('Ctrl Pts',(-0.932381698428526,55.6989774963075,
0.9633950950257));
#49001=CARTESIAN_POINT('Ctrl Pts',(-1.49106363405782,55.6460610348314,0.189731070304719));
#49002=CARTESIAN_POINT('Ctrl Pts',(-0.967512899225719,55.5666863426171,
-1.15225168784261));
#49003=CARTESIAN_POINT('Ctrl Pts',(0.442865973302976,55.4873116504031,-1.43658032227372));
#49004=CARTESIAN_POINT('Ctrl Pts',(1.44724201563678,55.4079369581888,-0.407851236765698));
#49005=CARTESIAN_POINT('Ctrl Pts',(1.1276037990622,55.3285622659747,0.994901145811772));
#49006=CARTESIAN_POINT('Ctrl Pts',(-0.22410576578139,55.2491875737605,1.48680521183891));
#49007=CARTESIAN_POINT('Ctrl Pts',(-1.37063740769069,55.1698128815463,0.618323911349722));
#49008=CARTESIAN_POINT('Ctrl Pts',(-1.26293354325317,55.0904381893321,-0.816096712708995));
#49009=CARTESIAN_POINT('Ctrl Pts',(0.000518963516653217,55.0110634971179,
-1.50364543832878));
#49010=CARTESIAN_POINT('Ctrl Pts',(1.2634838400664,54.9316888049038,-0.815219672159533));
#49011=CARTESIAN_POINT('Ctrl Pts',(1.37022795544771,54.8523141126896,0.619235929149326));
#49012=CARTESIAN_POINT('Ctrl Pts',(0.223058882480454,54.7729394204754,1.48701524229669));
#49013=CARTESIAN_POINT('Ctrl Pts',(-1.12823202116588,54.6935647282612,0.994014980507249));
#49014=CARTESIAN_POINT('Ctrl Pts',(-1.44706689157843,54.614190036047,-0.408620578361293));
#49015=CARTESIAN_POINT('Ctrl Pts',(-0.441675324154704,54.5348153438328,
-1.43732225685171));
#49016=CARTESIAN_POINT('Ctrl Pts',(0.967897716715009,54.4554406516187,-1.15071582195045));
#49017=CARTESIAN_POINT('Ctrl Pts',(1.49173757643851,54.3760659594045,0.188922901971819));
#49018=CARTESIAN_POINT('Ctrl Pts',(0.650472766495819,54.2966912671903,1.3556761857263));
#49019=CARTESIAN_POINT('Ctrl Pts',(-0.786046426050945,54.2173165749761,
1.2818361170921));
#49020=CARTESIAN_POINT('Ctrl Pts',(-1.50324635200296,54.1379418827619,0.0349744188024213));
#49021=CARTESIAN_POINT('Ctrl Pts',(-0.844809857600208,54.0585671905478,
-1.24389271869101));
#49022=CARTESIAN_POINT('Ctrl Pts',(0.586720943427397,53.9791924983336,-1.38446066605414));
#49023=CARTESIAN_POINT('Ctrl Pts',(1.48133729268241,53.8998178061194,-0.258094216376765));
#49024=CARTESIAN_POINT('Ctrl Pts',(1.02036643681545,53.8204431139052,1.10445694001623));
#49025=CARTESIAN_POINT('Ctrl Pts',(-0.374352385393229,53.741068421691,1.4563080342578));
#49026=CARTESIAN_POINT('Ctrl Pts',(-1.42649743618979,53.6616937294769,0.47547645921754));
#49027=CARTESIAN_POINT('Ctrl Pts',(-1.17323980728636,53.5823190372627,-0.940468581704944));
#49028=CARTESIAN_POINT('Ctrl Pts',(0.153661803903112,53.5029443450485,-1.49578101631727));
#49029=CARTESIAN_POINT('Ctrl Pts',(1.33994589596871,53.4235696528344,-0.682288644615303));
#49030=CARTESIAN_POINT('Ctrl Pts',(1.3000315254765,53.3441949606201,0.75557318073647));
#49031=CARTESIAN_POINT('Ctrl Pts',(0.0704447491227194,53.264820268406,1.50200210919453));
#49032=CARTESIAN_POINT('Ctrl Pts',(-1.22360675176528,53.1854455761918,0.873933244435241));
#49033=CARTESIAN_POINT('Ctrl Pts',(-1.39792295417167,53.1060708839776,-0.553881045797489));
#49034=CARTESIAN_POINT('Ctrl Pts',(-0.292985283484647,53.0266961917634,
-1.47483301507595));
#49035=CARTESIAN_POINT('Ctrl Pts',(1.08006627541054,52.9473214995492,-1.04614991249642));
#49036=CARTESIAN_POINT('Ctrl Pts',(1.46473792259796,52.8679468073351,0.339875884402707));
#49037=CARTESIAN_POINT('Ctrl Pts',(0.509012622328653,52.7885721151209,1.41487771521272));
#49038=CARTESIAN_POINT('Ctrl Pts',(-0.912515436687621,52.7091974229067,
1.19511019429316));
#49039=CARTESIAN_POINT('Ctrl Pts',(-1.4989911037539,52.6298227306925,-0.118315128197754));
#49040=CARTESIAN_POINT('Ctrl Pts',(-0.713724380092507,52.5504480384784,
-1.32346904306683));
#49041=CARTESIAN_POINT('Ctrl Pts',(0.72467896661141,52.4710733462642,-1.31750263531229));
#49042=CARTESIAN_POINT('Ctrl Pts',(1.49992103390936,52.39169865405,-0.105875826878788));
#49043=CARTESIAN_POINT('Ctrl Pts',(0.902569721711059,52.3123239618358,1.20263905480605));
#49044=CARTESIAN_POINT('Ctrl Pts',(-0.520732554977762,52.2329492696216,
1.41060639617868));
#49045=CARTESIAN_POINT('Ctrl Pts',(-1.46750704027315,52.1535745774075,0.327713114360973));
#49046=CARTESIAN_POINT('Ctrl Pts',(-1.0713505297735,52.0741998851933,-1.05507385574668));
#49047=CARTESIAN_POINT('Ctrl Pts',(0.305210022954444,51.9948251929791,-1.47235173820035));
#49048=CARTESIAN_POINT('Ctrl Pts',(1.40246970042868,51.9154505007649,-0.542265190759049));
#49049=CARTESIAN_POINT('Ctrl Pts',(1.21631473082964,51.8360758085508,0.884053886810973));
#49050=CARTESIAN_POINT('Ctrl Pts',(-0.0829025346852592,51.7567011163365,
1.50136603499951));
#49051=CARTESIAN_POINT('Ctrl Pts',(-1.30625482258257,51.6773264241224,0.744762465213426));
#49052=CARTESIAN_POINT('Ctrl Pts',(-1.33423970761725,51.5979517319082,-0.693380997286618));
#49053=CARTESIAN_POINT('Ctrl Pts',(-0.141247908656813,51.518577039694,-1.49700428966964));
#49054=CARTESIAN_POINT('Ctrl Pts',(1.18100129712657,51.4392023474798,-0.93070332366629));
#49055=CARTESIAN_POINT('Ctrl Pts',(1.42250395396948,51.3598276552657,0.487293916224389));
#49056=CARTESIAN_POINT('Ctrl Pts',(0.36225830298583,51.2804529630515,1.45936349646929));
#49057=CARTESIAN_POINT('Ctrl Pts',(-1.02949349155242,51.2010782708373,1.09595415636771));
#49058=CARTESIAN_POINT('Ctrl Pts',(-1.47914546322335,51.1217035786231,-0.270373934373359));
#49059=CARTESIAN_POINT('Ctrl Pts',(-0.575215197442902,51.042328886409,-1.38928065979757));
#49060=CARTESIAN_POINT('Ctrl Pts',(0.855098923927749,50.9629541941947,-1.23684090576505));
#49061=CARTESIAN_POINT('Ctrl Pts',(1.50290618670359,50.8835795019806,0.0474423840872669));
#49062=CARTESIAN_POINT('Ctrl Pts',(0.775382268430225,50.8042048097663,1.28831551484441));
#49063=CARTESIAN_POINT('Ctrl Pts',(-0.66169015229881,50.7248301175523,1.35022813475386));
#49064=CARTESIAN_POINT('Ctrl Pts',(-1.49326638260898,50.645455425338,0.176551663085664));
#49065=CARTESIAN_POINT('Ctrl Pts',(-0.958293075038441,50.5660807331238,
-1.15872591454633));
#49066=CARTESIAN_POINT('Ctrl Pts',(0.453534064315373,50.4867060409097,-1.43356896754687));
#49067=CARTESIAN_POINT('Ctrl Pts',(1.4505045351907,50.4073313486955,-0.39668023770827));
#49068=CARTESIAN_POINT('Ctrl Pts',(1.1197553097733,50.3279566564813,1.00349396081402));
#49069=CARTESIAN_POINT('Ctrl Pts',(-0.235009869266641,50.2485819642671,
1.48481098258362));
#49070=CARTESIAN_POINT('Ctrl Pts',(-1.3760640928247,50.169207272053,0.60845112765352));
#49071=CARTESIAN_POINT('Ctrl Pts',(-1.2551421938249,50.0898260779548,-0.827076980567057));
#49072=CARTESIAN_POINT('Ctrl Pts',(-0.41265429172088,50.0369031145949,-1.27565375796722));
#49073=CARTESIAN_POINT('Ctrl Pts',(0.0104297776558427,50.0104383819729,
-1.27217695389282));
#49074=CARTESIAN_POINT('Ctrl Pts',(-0.592987108432538,55.6696680384294,
1.23369893938847));
#49075=CARTESIAN_POINT('Ctrl Pts',(-1.00317218425256,55.6432098076914,1.03654025320749));
#49076=CARTESIAN_POINT('Ctrl Pts',(-1.60427168954347,55.5902933462152,0.204136280816067));
#49077=CARTESIAN_POINT('Ctrl Pts',(-1.04097069906526,55.5109186540011,-1.23973566239017));
#49078=CARTESIAN_POINT('Ctrl Pts',(0.476490289886929,55.4315439617868,-1.54565176705905));
#49079=CARTESIAN_POINT('Ctrl Pts',(1.55712294269118,55.3521692695727,-0.43881708180882));
#49080=CARTESIAN_POINT('Ctrl Pts',(1.21321639837339,55.2727945773585,1.07043838080641));
#49081=CARTESIAN_POINT('Ctrl Pts',(-0.241120853124227,55.1934198851444,
1.59968994933341));
#49082=CARTESIAN_POINT('Ctrl Pts',(-1.4747021787416,55.1140451929302,0.665269759981073));
#49083=CARTESIAN_POINT('Ctrl Pts',(-1.35882096708512,55.034670500716,-0.878058335153355));
#49084=CARTESIAN_POINT('Ctrl Pts',(0.000558365490677323,54.9552958085018,
-1.61780875927963));
#49085=CARTESIAN_POINT('Ctrl Pts',(1.35941304483292,54.8759211162877,-0.877114705859523));
#49086=CARTESIAN_POINT('Ctrl Pts',(1.47426163909818,54.7965464240734,0.666251022150459));
#49087=CARTESIAN_POINT('Ctrl Pts',(0.239994485876334,54.7171717318593,1.59991592621975));
#49088=CARTESIAN_POINT('Ctrl Pts',(-1.21389231783962,54.637797039645,1.06948493396631));
#49089=CARTESIAN_POINT('Ctrl Pts',(-1.55693452245038,54.558422347431,-0.4396448351744));
#49090=CARTESIAN_POINT('Ctrl Pts',(-0.475209241461426,54.4790476552166,
-1.5464500325467));
#49091=CARTESIAN_POINT('Ctrl Pts',(1.041384733577,54.3996729630026,-1.23808318685966));
#49092=CARTESIAN_POINT('Ctrl Pts',(1.6049968005696,54.3202982707883,0.203266752817891));
#49093=CARTESIAN_POINT('Ctrl Pts',(0.699859496451111,54.2409235785742,1.45860503554111));
#49094=CARTESIAN_POINT('Ctrl Pts',(-0.845726499645454,54.16154888636,1.3791587067876));
#49095=CARTESIAN_POINT('Ctrl Pts',(-1.61737937257903,54.0821741941458,0.0376298292449642));
#49096=CARTESIAN_POINT('Ctrl Pts',(-0.908951507258555,54.0027995019317,
-1.3383344800614));
#49097=CARTESIAN_POINT('Ctrl Pts',(0.63126735687412,53.9234248097175,-1.48957495918046));
#49098=CARTESIAN_POINT('Ctrl Pts',(1.59380688190213,53.8440501175034,-0.277689855154838));
#49099=CARTESIAN_POINT('Ctrl Pts',(1.09783710778899,53.7646754252891,1.18831212881632));
#49100=CARTESIAN_POINT('Ctrl Pts',(-0.402774851509876,53.6853007330749,
1.56687729299412));
#49101=CARTESIAN_POINT('Ctrl Pts',(-1.53480334427959,53.6059260408607,0.511576706147138));
#49102=CARTESIAN_POINT('Ctrl Pts',(-1.26231729141747,53.5265513486466,-1.0118730589843));
#49103=CARTESIAN_POINT('Ctrl Pts',(0.165328478366184,53.4471766564323,-1.60934723604244));
#49104=CARTESIAN_POINT('Ctrl Pts',(1.44168043356572,53.3678019642183,-0.734090974826148));
#49105=CARTESIAN_POINT('Ctrl Pts',(1.3987355899494,53.288427272004,0.812939592614877));
#49106=CARTESIAN_POINT('Ctrl Pts',(0.075793221773523,53.2090525797899,1.61604066142889));
#49107=CARTESIAN_POINT('Ctrl Pts',(-1.31650831403428,53.1296778875756,0.94028606866551));
#49108=CARTESIAN_POINT('Ctrl Pts',(-1.50405936293771,53.0503031953615,-0.595934110960401));
#49109=CARTESIAN_POINT('Ctrl Pts',(-0.315230004281003,52.9709285031473,
-1.58680877116654));
#49110=CARTESIAN_POINT('Ctrl Pts',(1.16206961855566,52.8915538109331,-1.12557817741755));
#49111=CARTESIAN_POINT('Ctrl Pts',(1.57594721523033,52.8121791187189,0.365680744169135));
#49112=CARTESIAN_POINT('Ctrl Pts',(0.547659081054675,52.7328044265048,1.52230140339784));
#49113=CARTESIAN_POINT('Ctrl Pts',(-0.981797589258738,52.6534297342906,
1.28584817360984));
#49114=CARTESIAN_POINT('Ctrl Pts',(-1.61280104732045,52.5740550420764,-0.127298128850341));
#49115=CARTESIAN_POINT('Ctrl Pts',(-0.767913448471228,52.4946803498622,
-1.42395258611544));
#49116=CARTESIAN_POINT('Ctrl Pts',(0.779699754985248,52.4153056576481,-1.41753318265721));
#49117=CARTESIAN_POINT('Ctrl Pts',(1.61380158182991,52.3359309654339,-0.113914381511949));
#49118=CARTESIAN_POINT('Ctrl Pts',(0.971096752215498,52.2565562732197,1.29394865805562));
#49119=CARTESIAN_POINT('Ctrl Pts',(-0.560268842115734,52.1771815810055,
1.51770578719019));
#49120=CARTESIAN_POINT('Ctrl Pts',(-1.57892657639899,52.0978068887914,0.352594523568839));
#49121=CARTESIAN_POINT('Ctrl Pts',(-1.15269213548962,52.0184321965771,-1.1351796653678));
#49122=CARTESIAN_POINT('Ctrl Pts',(0.328382899298671,51.939057504363,-1.58413910492659));
#49123=CARTESIAN_POINT('Ctrl Pts',(1.50895131800458,51.8596828121488,-0.583436329536225));
#49124=CARTESIAN_POINT('Ctrl Pts',(1.30866265105961,51.7803081199346,0.951175114359142));
#49125=CARTESIAN_POINT('Ctrl Pts',(-0.0891968567598987,51.7009334277205,
1.61535629370628));
#49126=CARTESIAN_POINT('Ctrl Pts',(-1.40543138691931,51.6215587355062,0.801308080410322));
#49127=CARTESIAN_POINT('Ctrl Pts',(-1.43554100650283,51.5421840432921,-0.746025507299841));
#49128=CARTESIAN_POINT('Ctrl Pts',(-0.151972066040321,51.4628093510779,
-1.61066338564395));
#49129=CARTESIAN_POINT('Ctrl Pts',(1.27066806742387,51.3834346588637,-1.00136637995689));
#49130=CARTESIAN_POINT('Ctrl Pts',(1.53050665946856,51.3040599666495,0.5242913960406));
#49131=CARTESIAN_POINT('Ctrl Pts',(0.389762533608743,51.2246852744354,1.57016473922538));
#49132=CARTESIAN_POINT('Ctrl Pts',(-1.10765712833604,51.1453105822212,1.17916377674197));
#49133=CARTESIAN_POINT('Ctrl Pts',(-1.59144863918925,51.065935890007,-0.290901902908883));
#49134=CARTESIAN_POINT('Ctrl Pts',(-0.618888044463587,50.9865611977928,
-1.49476090787491));
#49135=CARTESIAN_POINT('Ctrl Pts',(0.92002176438512,50.9071865055787,-1.33074726273637));
#49136=CARTESIAN_POINT('Ctrl Pts',(1.61701338044625,50.8278118133645,0.0510444168425675));
#49137=CARTESIAN_POINT('Ctrl Pts',(0.834252672658487,50.7484371211503,1.38613004868199));
#49138=CARTESIAN_POINT('Ctrl Pts',(-0.711928555117263,50.6690624289361,
1.45274334477311));
#49139=CARTESIAN_POINT('Ctrl Pts',(-1.60664168037358,50.589687736722,0.189956235509111));
#49140=CARTESIAN_POINT('Ctrl Pts',(-1.03105086560653,50.5103130445077,-1.24670144062743));
#49141=CARTESIAN_POINT('Ctrl Pts',(0.487968348905836,50.4309383522937,-1.54241177714507));
#49142=CARTESIAN_POINT('Ctrl Pts',(1.56063316696155,50.3515636600793,-0.426797931772294));
#49143=CARTESIAN_POINT('Ctrl Pts',(1.20477201754063,50.2721889678652,1.07968359980762));
#49144=CARTESIAN_POINT('Ctrl Pts',(-0.252852843712473,50.192814275651,1.59754430949374));
#49145=CARTESIAN_POINT('Ctrl Pts',(-1.48054088148351,50.1134395834369,0.654647391479134));
#49146=CARTESIAN_POINT('Ctrl Pts',(-1.35043806442046,50.0340583893389,-0.889872272845844));
#49147=CARTESIAN_POINT('Ctrl Pts',(-0.443984805648313,49.9811354259788,
-1.37250695598898));
#49148=CARTESIAN_POINT('Ctrl Pts',(0.011221651872736,49.9546706933568,-1.36876617778256));
#49149=CARTESIAN_POINT('Ctrl Pts',(-0.634832213542385,55.6139003498134,
1.32075692270464));
#49150=CARTESIAN_POINT('Ctrl Pts',(-1.07396267007658,55.5874421190754,1.10968541138929));
#49151=CARTESIAN_POINT('Ctrl Pts',(-1.71747974502912,55.5345256575993,0.218541491327414));
#49152=CARTESIAN_POINT('Ctrl Pts',(-1.11442849890479,55.455150965385,-1.32721963693774));
#49153=CARTESIAN_POINT('Ctrl Pts',(0.510114606470883,55.3757762731709,-1.65472321184439));
#49154=CARTESIAN_POINT('Ctrl Pts',(1.66700386974557,55.2964015809567,-0.469782926851943));
#49155=CARTESIAN_POINT('Ctrl Pts',(1.29882899768456,55.2170268887425,1.14597561580105));
#49156=CARTESIAN_POINT('Ctrl Pts',(-0.258135940467066,55.1376521965284,
1.71257468682791));
#49157=CARTESIAN_POINT('Ctrl Pts',(-1.57876694979249,55.0582775043141,0.712215608612426));
#49158=CARTESIAN_POINT('Ctrl Pts',(-1.45470839091706,54.9789028121001,-0.940019957597718));
#49159=CARTESIAN_POINT('Ctrl Pts',(0.000597767464702774,54.8995281198857,
-1.73197208023047));
#49160=CARTESIAN_POINT('Ctrl Pts',(1.45534224959945,54.8201534276717,-0.939009739559512));
#49161=CARTESIAN_POINT('Ctrl Pts',(1.57829532274867,54.7407787354574,0.713266115151591));
#49162=CARTESIAN_POINT('Ctrl Pts',(0.256930089272216,54.6614040432433,1.71281661014281));
#49163=CARTESIAN_POINT('Ctrl Pts',(-1.29955261451337,54.582029351029,1.14495488742536));
#49164=CARTESIAN_POINT('Ctrl Pts',(-1.66680215332233,54.5026546588149,-0.470669091987506));
#49165=CARTESIAN_POINT('Ctrl Pts',(-0.50874315876815,54.4232799666007,-1.65557780824169));
#49166=CARTESIAN_POINT('Ctrl Pts',(1.11487175043898,54.3439052743866,-1.32545055176888));
#49167=CARTESIAN_POINT('Ctrl Pts',(1.7182560247007,54.2645305821723,0.217610603663962));
#49168=CARTESIAN_POINT('Ctrl Pts',(0.749246226406404,54.1851558899582,1.56153388535592));
#49169=CARTESIAN_POINT('Ctrl Pts',(-0.90540657323996,54.105781197744,1.47648129648309));
#49170=CARTESIAN_POINT('Ctrl Pts',(-1.73151239315509,54.0264065055298,0.0402852396875059));
#49171=CARTESIAN_POINT('Ctrl Pts',(-0.973093156916901,53.9470318133156,
-1.4327762414318));
#49172=CARTESIAN_POINT('Ctrl Pts',(0.675813770320844,53.8676571211015,-1.59468925230679));
#49173=CARTESIAN_POINT('Ctrl Pts',(1.70627647112185,53.7882824288872,-0.297285493932909));
#49174=CARTESIAN_POINT('Ctrl Pts',(1.17530777876252,53.7089077366732,1.27216731761641));
#49175=CARTESIAN_POINT('Ctrl Pts',(-0.431197317626523,53.6295330444589,
1.67744655173045));
#49176=CARTESIAN_POINT('Ctrl Pts',(-1.64310925236939,53.5501583522448,0.547676953076732));
#49177=CARTESIAN_POINT('Ctrl Pts',(-1.35139477554857,53.4707836600306,-1.08327753626366));
#49178=CARTESIAN_POINT('Ctrl Pts',(0.176995152829257,53.3914089678163,-1.72291345576761));
#49179=CARTESIAN_POINT('Ctrl Pts',(1.54341497116274,53.3120342756023,-0.785893305036992));
#49180=CARTESIAN_POINT('Ctrl Pts',(1.4974396544223,53.2326595833879,0.870306004493283));
#49181=CARTESIAN_POINT('Ctrl Pts',(0.0811416944243273,53.1532848911739,
1.73007921366326));
#49182=CARTESIAN_POINT('Ctrl Pts',(-1.40940987630327,53.0739101989596,1.00663889289578));
#49183=CARTESIAN_POINT('Ctrl Pts',(-1.61019577170375,52.9945355067455,-0.637987176123315));
#49184=CARTESIAN_POINT('Ctrl Pts',(-0.337474725077362,52.9151608145313,
-1.69878452725711));
#49185=CARTESIAN_POINT('Ctrl Pts',(1.24407296170078,52.8357861223171,-1.20500644233868));
#49186=CARTESIAN_POINT('Ctrl Pts',(1.68715650786268,52.7564114301029,0.391485603935567));
#49187=CARTESIAN_POINT('Ctrl Pts',(0.586305539780697,52.6770367378888,1.62972509158297));
#49188=CARTESIAN_POINT('Ctrl Pts',(-1.05107974182985,52.5976620456745,1.37658615292654));
#49189=CARTESIAN_POINT('Ctrl Pts',(-1.72661099088702,52.5182873534605,-0.13628112950293));
#49190=CARTESIAN_POINT('Ctrl Pts',(-0.822102516849947,52.4389126612462,
-1.52443612916404));
#49191=CARTESIAN_POINT('Ctrl Pts',(0.834720543359083,52.3595379690321,-1.51756373000215));
#49192=CARTESIAN_POINT('Ctrl Pts',(1.72768212975045,52.2801632768178,-0.121952936145109));
#49193=CARTESIAN_POINT('Ctrl Pts',(1.03962378271994,52.2007885846037,1.3852582613052));
#49194=CARTESIAN_POINT('Ctrl Pts',(-0.599805129253705,52.1214138923895,
1.62480517820171));
#49195=CARTESIAN_POINT('Ctrl Pts',(-1.69034611252483,52.0420392001754,0.377475932776706));
#49196=CARTESIAN_POINT('Ctrl Pts',(-1.23403374120574,51.9626645079611,-1.21528547498893));
#49197=CARTESIAN_POINT('Ctrl Pts',(0.351555775642897,51.883289815747,-1.69592647165283));
#49198=CARTESIAN_POINT('Ctrl Pts',(1.61543293558047,51.8039151235328,-0.624607468313401));
#49199=CARTESIAN_POINT('Ctrl Pts',(1.40101057128958,51.7245404313186,1.01829634190731));
#49200=CARTESIAN_POINT('Ctrl Pts',(-0.0954911788345371,51.6451657391045,
1.72934655241303));
#49201=CARTESIAN_POINT('Ctrl Pts',(-1.50460795125606,51.5657910468902,0.857853695607218));
#49202=CARTESIAN_POINT('Ctrl Pts',(-1.53684230538839,51.4864163546762,-0.798670017313065));
#49203=CARTESIAN_POINT('Ctrl Pts',(-0.162696223423829,51.4070416624618,
-1.72432248161826));
#49204=CARTESIAN_POINT('Ctrl Pts',(1.36033483772117,51.3276669702478,-1.0720294362475));
#49205=CARTESIAN_POINT('Ctrl Pts',(1.63850936496764,51.2482922780335,0.561288875856811));
#49206=CARTESIAN_POINT('Ctrl Pts',(0.417266764231657,51.1689175858195,1.68096598198148));
#49207=CARTESIAN_POINT('Ctrl Pts',(-1.18582076511967,51.0895428936051,1.26237339711622));
#49208=CARTESIAN_POINT('Ctrl Pts',(-1.70375181515514,51.010168201391,-0.311429871444408));
#49209=CARTESIAN_POINT('Ctrl Pts',(-0.662560891484271,50.9307935091768,
-1.60024115595223));
#49210=CARTESIAN_POINT('Ctrl Pts',(0.98494460484249,50.8514188169627,-1.42465361970768));
#49211=CARTESIAN_POINT('Ctrl Pts',(1.73112057418891,50.7720441247485,0.054646449597867));
#49212=CARTESIAN_POINT('Ctrl Pts',(0.893123076886749,50.6926694325343,1.48394458251956));
#49213=CARTESIAN_POINT('Ctrl Pts',(-0.762166957935716,50.6132947403201,
1.55525855479236));
#49214=CARTESIAN_POINT('Ctrl Pts',(-1.72001697813816,50.5339200481059,0.203360807932558));
#49215=CARTESIAN_POINT('Ctrl Pts',(-1.10380865617462,50.4545453558917,-1.33467696670851));
#49216=CARTESIAN_POINT('Ctrl Pts',(0.5224026334963,50.3751706636775,-1.65125458674327));
#49217=CARTESIAN_POINT('Ctrl Pts',(1.67076179873239,50.2957959714634,-0.456915625836322));
#49218=CARTESIAN_POINT('Ctrl Pts',(1.28978872530794,50.2164212792492,1.15587323880121));
#49219=CARTESIAN_POINT('Ctrl Pts',(-0.270695818158305,50.137046587035,1.71027763640386));
#49220=CARTESIAN_POINT('Ctrl Pts',(-1.58501767014233,50.0576718948208,0.700843655304749));
#49221=CARTESIAN_POINT('Ctrl Pts',(-1.44573393501602,49.9782907007227,-0.952667565124631));
#49222=CARTESIAN_POINT('Ctrl Pts',(-0.475315319575745,49.9253677373627,
-1.46936015401072));
#49223=CARTESIAN_POINT('Ctrl Pts',(0.0120135260896293,49.8989030047408,
-1.4653554016723));
#49224=CARTESIAN_POINT('Ctrl Pts',(-1.28852825769066,50.065,0.693921594369763));
#49225=CARTESIAN_POINT('Ctrl Pts',(-1.29259187868739,50.065,0.686211757365716));
#49226=CARTESIAN_POINT('Ctrl Pts',(-1.29665549968411,50.065,0.67850192036167));
#49227=CARTESIAN_POINT('Ctrl Pts',(-1.30071912068084,50.065,0.670792083357623));
#49228=CARTESIAN_POINT('Ctrl Pts',(-0.686166456961371,55.615,-0.959540123316451));
#49229=CARTESIAN_POINT('Ctrl Pts',(-0.713413796911466,55.615,-0.944727431681135));
#49230=CARTESIAN_POINT('Ctrl Pts',(-0.739980968402287,55.615,-0.928802159412089));
#49231=CARTESIAN_POINT('Ctrl Pts',(-0.765790962793899,55.615,-0.911780060719286));
#49232=CARTESIAN_POINT('Ctrl Pts',(-0.806300133279505,55.615,-0.885063623376951));
#49233=CARTESIAN_POINT('Ctrl Pts',(-0.844945527882661,55.615,-0.85564803640011));
#49234=CARTESIAN_POINT('Ctrl Pts',(-0.881654237249992,55.615,-0.823835334333387));
#49235=CARTESIAN_POINT('Ctrl Pts',(-0.897239265429731,55.615,-0.810328952149743));
#49236=CARTESIAN_POINT('Ctrl Pts',(-0.91247497671016,55.615,-0.7963898664341));
#49237=CARTESIAN_POINT('Ctrl Pts',(-0.927354620595185,55.615,-0.782038646482574));
#49238=CARTESIAN_POINT('Ctrl Pts',(-0.937468429879662,55.615,-0.772284011041641));
#49239=CARTESIAN_POINT('Ctrl Pts',(-0.947419424992027,55.615,-0.762336894601238));
#49240=CARTESIAN_POINT('Ctrl Pts',(-0.957188717566935,55.615,-0.752221373165328));
#49241=CARTESIAN_POINT('Ctrl Pts',(-0.992370133259333,55.615,-0.715793109618777));
#49242=CARTESIAN_POINT('Ctrl Pts',(-1.02524473489684,55.615,-0.677140392748355));
#49243=CARTESIAN_POINT('Ctrl Pts',(-1.05573220817217,55.615,-0.636588252605784));
#49244=CARTESIAN_POINT('Ctrl Pts',(-1.07725611353962,55.615,-0.607958775213741));
#49245=CARTESIAN_POINT('Ctrl Pts',(-1.09758983810779,55.615,-0.578381398104754));
#49246=CARTESIAN_POINT('Ctrl Pts',(-1.11669696564595,55.615,-0.547957266410611));
#49247=CARTESIAN_POINT('Ctrl Pts',(-1.12351935004655,55.615,-0.537094036390431));
#49248=CARTESIAN_POINT('Ctrl Pts',(-1.13018528144804,55.615,-0.526122764219766));
#49249=CARTESIAN_POINT('Ctrl Pts',(-1.13669284706255,55.615,-0.515047781095408));
#49250=CARTESIAN_POINT('Ctrl Pts',(-1.14143068161862,55.615,-0.506984637231359));
#49251=CARTESIAN_POINT('Ctrl Pts',(-1.14608376236126,55.615,-0.49886775743124));
#49252=CARTESIAN_POINT('Ctrl Pts',(-1.15064685006719,55.615,-0.490707349154656));
#49253=CARTESIAN_POINT('Ctrl Pts',(-1.1763516666904,55.615,-0.444738081886885));
#49254=CARTESIAN_POINT('Ctrl Pts',(-1.19924569348006,55.615,-0.397319323655606));
#49255=CARTESIAN_POINT('Ctrl Pts',(-1.21924407138793,55.615,-0.348783334871917));
#49256=CARTESIAN_POINT('Ctrl Pts',(-1.23956435361566,55.615,-0.299466085501526));
#49257=CARTESIAN_POINT('Ctrl Pts',(-1.25689577956724,55.615,-0.24899444005167));
#49258=CARTESIAN_POINT('Ctrl Pts',(-1.27111323015662,55.615,-0.197677848868708));
#49259=CARTESIAN_POINT('Ctrl Pts',(-1.27928931799279,55.615,-0.168167005533828));
#49260=CARTESIAN_POINT('Ctrl Pts',(-1.28643485880816,55.615,-0.13837608268905));
#49261=CARTESIAN_POINT('Ctrl Pts',(-1.29251925576579,55.615,-0.108360072500537));
#49262=CARTESIAN_POINT('Ctrl Pts',(-1.29623123190128,55.615,-0.0900478692898342));
#49263=CARTESIAN_POINT('Ctrl Pts',(-1.29954814897365,55.615,-0.0716518423879908));
#49264=CARTESIAN_POINT('Ctrl Pts',(-1.30246201461502,55.615,-0.0531841690282108));
#49265=CARTESIAN_POINT('Ctrl Pts',(-1.30398684891677,55.615,-0.0435199822473792));
#49266=CARTESIAN_POINT('Ctrl Pts',(-1.30540118376147,55.615,-0.033836160950599));
#49267=CARTESIAN_POINT('Ctrl Pts',(-1.30670217233378,55.615,-0.0241489422268533));
#49268=CARTESIAN_POINT('Ctrl Pts',(-1.31399697767701,55.615,0.0301685025311241));
#49269=CARTESIAN_POINT('Ctrl Pts',(-1.31775021860916,55.615,0.084702533890493));
#49270=CARTESIAN_POINT('Ctrl Pts',(-1.31784722812879,55.615,0.139123948194586));
#49271=CARTESIAN_POINT('Ctrl Pts',(-1.31786333897964,55.615,0.148161981701328));
#49272=CARTESIAN_POINT('Ctrl Pts',(-1.3177785083462,55.615,0.157196969940163));
#49273=CARTESIAN_POINT('Ctrl Pts',(-1.31759208781496,55.615,0.166227470352783));
#49274=CARTESIAN_POINT('Ctrl Pts',(-1.31649771872793,55.615,0.219240410644158));
#49275=CARTESIAN_POINT('Ctrl Pts',(-1.31190679820835,55.615,0.272097989836632));
#49276=CARTESIAN_POINT('Ctrl Pts',(-1.30402779002026,55.615,0.324575174779585));
#49277=CARTESIAN_POINT('Ctrl Pts',(-1.29759318812667,55.615,0.36743206558918));
#49278=CARTESIAN_POINT('Ctrl Pts',(-1.28896443766674,55.615,0.41003571745502));
#49279=CARTESIAN_POINT('Ctrl Pts',(-1.27822940812215,55.615,0.452264473592666));
#49280=CARTESIAN_POINT('Ctrl Pts',(-1.27568035532626,55.615,0.46229177053234));
#49281=CARTESIAN_POINT('Ctrl Pts',(-1.27301185909614,55.615,0.472299687376204));
#49282=CARTESIAN_POINT('Ctrl Pts',(-1.27022983206114,55.615,0.482269961965456));
#49283=CARTESIAN_POINT('Ctrl Pts',(-1.2555747222539,55.615,0.534791187343801));
#49284=CARTESIAN_POINT('Ctrl Pts',(-1.23775012514738,55.615,0.586364505451297));
#49285=CARTESIAN_POINT('Ctrl Pts',(-1.21699228297199,55.615,0.63675759876728));
#49286=CARTESIAN_POINT('Ctrl Pts',(-1.19563053272573,55.615,0.688616778756082));
#49287=CARTESIAN_POINT('Ctrl Pts',(-1.17116222891849,55.615,0.739227014421633));
#49288=CARTESIAN_POINT('Ctrl Pts',(-1.14378967960996,55.615,0.78833572555278));
#49289=CARTESIAN_POINT('Ctrl Pts',(-1.12831450200091,55.615,0.816099527102268));
#49290=CARTESIAN_POINT('Ctrl Pts',(-1.11191007542324,55.615,0.843383335748853));
#49291=CARTESIAN_POINT('Ctrl Pts',(-1.09460583269318,55.615,0.87013975692643));
#49292=CARTESIAN_POINT('Ctrl Pts',(-1.08385338689301,55.615,0.886765562112273));
#49293=CARTESIAN_POINT('Ctrl Pts',(-1.07275341592303,55.615,0.903187706241318));
#49294=CARTESIAN_POINT('Ctrl Pts',(-1.06131206243182,55.615,0.919394377481652));
#49295=CARTESIAN_POINT('Ctrl Pts',(-1.05554179996197,55.615,0.927567951254296));
#49296=CARTESIAN_POINT('Ctrl Pts',(-1.04968469512178,55.615,0.935686712806367));
#49297=CARTESIAN_POINT('Ctrl Pts',(-1.04374147146349,55.615,0.943749105818433));
#49298=CARTESIAN_POINT('Ctrl Pts',(-1.03744933002585,55.615,0.952284829875686));
#49299=CARTESIAN_POINT('Ctrl Pts',(-1.03106633620261,55.615,0.960749633607578));
#49300=CARTESIAN_POINT('Ctrl Pts',(-1.02459591553728,55.615,0.969139382618596));
#49301=CARTESIAN_POINT('Ctrl Pts',(-0.989018945593423,55.615,1.01526959019551));
#49302=CARTESIAN_POINT('Ctrl Pts',(-0.950784323740741,55.615,1.05915700560731));
#49303=CARTESIAN_POINT('Ctrl Pts',(-0.910112926818086,55.615,1.10054016857051));
#49304=CARTESIAN_POINT('Ctrl Pts',(-0.868873824614699,55.615,1.14250097188848));
#49305=CARTESIAN_POINT('Ctrl Pts',(-0.825129032595075,55.615,1.18188829248971));
#49306=CARTESIAN_POINT('Ctrl Pts',(-0.779058684490665,55.615,1.21840862870409));
#49307=CARTESIAN_POINT('Ctrl Pts',(-0.732988336386267,55.615,1.25492896491846));
#49308=CARTESIAN_POINT('Ctrl Pts',(-0.684591886750651,55.615,1.28858350433891));
#49309=CARTESIAN_POINT('Ctrl Pts',(-0.634007094575044,55.615,1.31904027763693));
#49310=CARTESIAN_POINT('Origin',(-3.28582941601228E-17,55.615,0.));
#49311=CARTESIAN_POINT('',(0.658022064252088,55.615,1.30722576969605));
#49312=CARTESIAN_POINT('',(-1.79227059055215E-16,55.615,-1.4635));
#49313=CARTESIAN_POINT('Origin',(0.,55.615,0.));
#49314=CARTESIAN_POINT('Ctrl Pts',(0.658022064252089,55.6150000000001,1.30722576969605));
#49315=CARTESIAN_POINT('Ctrl Pts',(0.68291041760411,55.6150000000001,1.29174709945824));
#49316=CARTESIAN_POINT('Ctrl Pts',(0.70727048796654,55.6150000000001,1.27548020477116));
#49317=CARTESIAN_POINT('Ctrl Pts',(0.731059524014722,55.6150000000001,1.25842242479073));
#49318=CARTESIAN_POINT('Ctrl Pts',(0.778314131695388,55.6150000000001,1.22453880297244));
#49319=CARTESIAN_POINT('Ctrl Pts',(0.823318307788889,55.6150000000001,1.18753622257729));
#49320=CARTESIAN_POINT('Ctrl Pts',(0.865917011406816,55.6150000000001,1.14773425046169));
#49321=CARTESIAN_POINT('Ctrl Pts',(0.888709815422025,55.6150000000001,1.12643786177376));
#49322=CARTESIAN_POINT('Ctrl Pts',(0.910813233033345,55.615,1.10433948889784));
#49323=CARTESIAN_POINT('Ctrl Pts',(0.932198075962424,55.615,1.08148531314));
#49324=CARTESIAN_POINT('Ctrl Pts',(0.941182403063221,55.615,1.07188368121272));
#49325=CARTESIAN_POINT('Ctrl Pts',(0.950034495504371,55.615,1.06215426440287));
#49326=CARTESIAN_POINT('Ctrl Pts',(0.958748320582393,55.615,1.05230580285939));
#49327=CARTESIAN_POINT('Ctrl Pts',(0.996890648209955,55.615,1.00919692203433));
#49328=CARTESIAN_POINT('Ctrl Pts',(1.03241482205307,55.615,0.963779887246079));
#49329=CARTESIAN_POINT('Ctrl Pts',(1.06516729256736,55.615,0.916365584833226));
#49330=CARTESIAN_POINT('Ctrl Pts',(1.08673802125298,55.615,0.885138595323546));
#49331=CARTESIAN_POINT('Ctrl Pts',(1.10710560412785,55.615,0.853044676706417));
#49332=CARTESIAN_POINT('Ctrl Pts',(1.1262143987642,55.615,0.820168902777738));
#49333=CARTESIAN_POINT('Ctrl Pts',(1.13494907220612,55.615,0.805141311823826));
#49334=CARTESIAN_POINT('Ctrl Pts',(1.143420596016,55.615,0.789950335051207));
#49335=CARTESIAN_POINT('Ctrl Pts',(1.15162295132403,55.615,0.7746040391249));
#49336=CARTESIAN_POINT('Ctrl Pts',(1.15676325047072,55.615,0.764986734229843));
#49337=CARTESIAN_POINT('Ctrl Pts',(1.161795159293,55.615,0.755313303870316));
#49338=CARTESIAN_POINT('Ctrl Pts',(1.16671416235182,55.615,0.74559275360192));
#49339=CARTESIAN_POINT('Ctrl Pts',(1.19208713322841,55.615,0.695452667101675));
#49340=CARTESIAN_POINT('Ctrl Pts',(1.21449001188561,55.615,0.64400430683225));
#49341=CARTESIAN_POINT('Ctrl Pts',(1.23377743082302,55.615,0.591534933891794));
#49342=CARTESIAN_POINT('Ctrl Pts',(1.25260516103681,55.615,0.540316095258442));
#49343=CARTESIAN_POINT('Ctrl Pts',(1.26846429964751,55.615,0.488123297443767));
#49344=CARTESIAN_POINT('Ctrl Pts',(1.28117110996631,55.615,0.435218704777426));
#49345=CARTESIAN_POINT('Ctrl Pts',(1.28851312999605,55.615,0.404650326933115));
#49346=CARTESIAN_POINT('Ctrl Pts',(1.29480181489721,55.615,0.373844300548893));
#49347=CARTESIAN_POINT('Ctrl Pts',(1.29999379066505,55.615,0.342852380337404));
#49348=CARTESIAN_POINT('Ctrl Pts',(1.30253195104456,55.615,0.327701603931069));
#49349=CARTESIAN_POINT('Ctrl Pts',(1.30480792213547,55.615,0.312506423403815));
#49350=CARTESIAN_POINT('Ctrl Pts',(1.30681610317096,55.615,0.29727304558529));
#49351=CARTESIAN_POINT('Ctrl Pts',(1.30817917115221,55.615,0.286933275821725));
#49352=CARTESIAN_POINT('Ctrl Pts',(1.30941904387809,55.615,0.276574159451665));
#49353=CARTESIAN_POINT('Ctrl Pts',(1.31053329015515,55.615,0.266203176480421));
#49354=CARTESIAN_POINT('Ctrl Pts',(1.31618011679077,55.615,0.213644649621809));
#49355=CARTESIAN_POINT('Ctrl Pts',(1.31858293691913,55.615,0.160993037389023));
#49356=CARTESIAN_POINT('Ctrl Pts',(1.31758756847756,55.615,0.108492899597445));
#49357=CARTESIAN_POINT('Ctrl Pts',(1.31729118832992,55.615,0.0928604986286303));
#49358=CARTESIAN_POINT('Ctrl Pts',(1.31669317679049,55.615,0.0772415590078096));
#49359=CARTESIAN_POINT('Ctrl Pts',(1.31578856736902,55.615,0.0616426741714474));
#49360=CARTESIAN_POINT('Ctrl Pts',(1.31260574726313,55.615,0.00675882805143094));
#49361=CARTESIAN_POINT('Ctrl Pts',(1.30563135996479,55.615,-0.0478787267712015));
#49362=CARTESIAN_POINT('Ctrl Pts',(1.29503867980794,55.615,-0.101964033927055));
#49363=CARTESIAN_POINT('Ctrl Pts',(1.29017588246939,55.615,-0.126793055836274));
#49364=CARTESIAN_POINT('Ctrl Pts',(1.28454982057433,55.615,-0.151505335923803));
#49365=CARTESIAN_POINT('Ctrl Pts',(1.2781739397107,55.615,-0.176068982586533));
#49366=CARTESIAN_POINT('Ctrl Pts',(1.27368851673344,55.615,-0.193349472530278));
#49367=CARTESIAN_POINT('Ctrl Pts',(1.26883195876927,55.615,-0.210556370160557));
#49368=CARTESIAN_POINT('Ctrl Pts',(1.26360842526702,55.615,-0.227678015327403));
#49369=CARTESIAN_POINT('Ctrl Pts',(1.26060788187359,55.615,-0.237513166048233));
#49370=CARTESIAN_POINT('Ctrl Pts',(1.25748861719013,55.615,-0.247312236830595));
#49371=CARTESIAN_POINT('Ctrl Pts',(1.25425381366423,55.615,-0.257067869314174));
#49372=CARTESIAN_POINT('Ctrl Pts',(1.23770844736276,55.615,-0.306965957915593));
#49373=CARTESIAN_POINT('Ctrl Pts',(1.21813026885531,55.615,-0.355775530682368));
#49374=CARTESIAN_POINT('Ctrl Pts',(1.19569149061526,55.615,-0.403236927123455));
#49375=CARTESIAN_POINT('Ctrl Pts',(1.17340656245797,55.615,-0.450372907461588));
#49376=CARTESIAN_POINT('Ctrl Pts',(1.1482993237225,55.615,-0.496180019253271));
#49377=CARTESIAN_POINT('Ctrl Pts',(1.12049946060564,55.615,-0.540371229951903));
#49378=CARTESIAN_POINT('Ctrl Pts',(1.10656068523074,55.615,-0.562528582197986));
#49379=CARTESIAN_POINT('Ctrl Pts',(1.09194444731789,55.615,-0.584279101420356));
#49380=CARTESIAN_POINT('Ctrl Pts',(1.07666430994254,55.615,-0.605582436250956));
#49381=CARTESIAN_POINT('Ctrl Pts',(1.0654084494325,55.615,-0.621275185560824));
#49382=CARTESIAN_POINT('Ctrl Pts',(1.05379230002795,55.615,-0.636725221388357));
#49383=CARTESIAN_POINT('Ctrl Pts',(1.04182078348874,55.615,-0.651915270109351));
#49384=CARTESIAN_POINT('Ctrl Pts',(1.0360343607354,55.615,-0.659257367767205));
#49385=CARTESIAN_POINT('Ctrl Pts',(1.03016546377772,55.615,-0.666537854073461));
#49386=CARTESIAN_POINT('Ctrl Pts',(1.02422302488534,55.615,-0.673745045559676));
#49387=CARTESIAN_POINT('Ctrl Pts',(0.992143122081392,55.615,-0.712652639992629));
#49388=CARTESIAN_POINT('Ctrl Pts',(0.9578608316653,55.615,-0.749506601960801));
#49389=CARTESIAN_POINT('Ctrl Pts',(0.921505700618096,55.615,-0.784054535932657));
#49390=CARTESIAN_POINT('Ctrl Pts',(0.885885294343576,55.615,-0.817904267967041));
#49391=CARTESIAN_POINT('Ctrl Pts',(0.848274239084723,55.615,-0.849540819064814));
#49392=CARTESIAN_POINT('Ctrl Pts',(0.808770632805465,55.615,-0.878683193575754));
#49393=CARTESIAN_POINT('Ctrl Pts',(0.769267026526212,55.615,-0.90782556808669));
#49394=CARTESIAN_POINT('Ctrl Pts',(0.727870244441854,55.615,-0.934474448336147));
#49395=CARTESIAN_POINT('Ctrl Pts',(0.684664424539371,55.615,-0.958295198918462));
#49396=CARTESIAN_POINT('Origin',(0.,55.615,0.));
#49397=CARTESIAN_POINT('Ctrl Pts',(0.851547439304115,55.7810496121231,-1.19249201555124));
#49398=CARTESIAN_POINT('Ctrl Pts',(1.24813648739576,55.7545848791926,-0.909303082791228));
#49399=CARTESIAN_POINT('Ctrl Pts',(1.72948988737955,55.7016619155239,0.0790533067026992));
#49400=CARTESIAN_POINT('Ctrl Pts',(0.870312231128513,55.6222807211175,1.49856009322968));
#49401=CARTESIAN_POINT('Ctrl Pts',(-0.786234575314587,55.5429060289032,
1.54266863466831));
#49402=CARTESIAN_POINT('Ctrl Pts',(-1.72276977183862,55.4635313366891,0.17699222243158));
#49403=CARTESIAN_POINT('Ctrl Pts',(-1.08304583280362,55.3841566444748,-1.35162590392847));
#49404=CARTESIAN_POINT('Ctrl Pts',(0.54791983081442,55.3047819522607,-1.64286170370572));
#49405=CARTESIAN_POINT('Ctrl Pts',(1.67740951839998,55.2254072600464,-0.43094974572187));
#49406=CARTESIAN_POINT('Ctrl Pts',(1.27191930029928,55.1460325678324,1.17545715863903));
#49407=CARTESIAN_POINT('Ctrl Pts',(-0.297535369309862,55.0666578756181,
1.70612562639131));
#49408=CARTESIAN_POINT('Ctrl Pts',(-1.59470324002085,54.987283183404,0.675534000334254));
#49409=CARTESIAN_POINT('Ctrl Pts',(-1.43254616815791,54.9079084911898,-0.97326276475906));
#49410=CARTESIAN_POINT('Ctrl Pts',(0.0405511939472471,54.8285337989756,
-1.73140800565394));
#49411=CARTESIAN_POINT('Ctrl Pts',(1.47653853778323,54.7491591067614,-0.905128112763759));
#49412=CARTESIAN_POINT('Ctrl Pts',(1.56133067791224,54.6697844145472,0.749446188461003));
#49413=CARTESIAN_POINT('Ctrl Pts',(0.217332522504072,54.590409722333,1.71819333027979));
#49414=CARTESIAN_POINT('Ctrl Pts',(-1.32554873260254,54.5110350301189,1.11460441681919));
#49415=CARTESIAN_POINT('Ctrl Pts',(-1.65540659994225,54.4316603379047,-0.508970916374371));
#49416=CARTESIAN_POINT('Ctrl Pts',(-0.470384583918035,54.3522856456905,
-1.66678150637739));
#49417=CARTESIAN_POINT('Ctrl Pts',(1.14509124923834,54.2729109534763,-1.29930303482708));
#49418=CARTESIAN_POINT('Ctrl Pts',(1.71268214966027,54.1935362612622,0.257181232075015));
#49419=CARTESIAN_POINT('Ctrl Pts',(0.712979749441727,54.114161569048,1.57831625179607));
#49420=CARTESIAN_POINT('Ctrl Pts',(-0.939177851791401,54.0347868768338,
1.45511762067378));
#49421=CARTESIAN_POINT('Ctrl Pts',(-1.73188400837484,53.9554121846196,0.000325675578953457));
#49422=CARTESIAN_POINT('Ctrl Pts',(-0.939725047858023,53.8760374924055,
-1.45476429602388));
#49423=CARTESIAN_POINT('Ctrl Pts',(0.712386103172446,53.7966628001912,-1.57858429118273));
#49424=CARTESIAN_POINT('Ctrl Pts',(1.71258530251459,53.7172881079772,-0.257825339110466));
#49425=CARTESIAN_POINT('Ctrl Pts',(1.1455798323574,53.6379134157629,1.29887226907537));
#49426=CARTESIAN_POINT('Ctrl Pts',(-0.46975768860566,53.5585387235487,1.66695831918764));
#49427=CARTESIAN_POINT('Ctrl Pts',(-1.6552150500525,53.4791640313345,0.509593428052268));
#49428=CARTESIAN_POINT('Ctrl Pts',(-1.32596785837452,53.3997893391204,-1.11410572315841));
#49429=CARTESIAN_POINT('Ctrl Pts',(0.216686347870187,53.3204146469062,-1.71827510908279));
#49430=CARTESIAN_POINT('Ctrl Pts',(1.56104861754719,53.241039954692,-0.75003302426545));
#49431=CARTESIAN_POINT('Ctrl Pts',(1.47687901847619,53.1616652624778,0.904572102498378));
#49432=CARTESIAN_POINT('Ctrl Pts',(0.0412020285017384,53.0822905702637,
1.73139386526713));
#49433=CARTESIAN_POINT('Ctrl Pts',(-1.43217936741558,53.0029158780494,0.97379904671594));
#49434=CARTESIAN_POINT('Ctrl Pts',(-1.5949584892478,52.9235411858353,-0.674929434394221));
#49435=CARTESIAN_POINT('Ctrl Pts',(-0.298174465124138,52.8441664936211,
-1.7060229518338));
#49436=CARTESIAN_POINT('Ctrl Pts',(1.27147212143958,52.7647918014069,-1.17591707540933));
#49437=CARTESIAN_POINT('Ctrl Pts',(1.67758131058698,52.6854171091927,0.430282779347293));
#49438=CARTESIAN_POINT('Ctrl Pts',(0.548518348371223,52.6060424169786,1.64272637567395));
#49439=CARTESIAN_POINT('Ctrl Pts',(-1.08249947446898,52.5266677247644,1.35189393504859));
#49440=CARTESIAN_POINT('Ctrl Pts',(-1.72291073975908,52.4472930325502,-0.176070743280815));
#49441=CARTESIAN_POINT('Ctrl Pts',(-0.78666842036735,52.367918340336,-1.54291124833255));
#49442=CARTESIAN_POINT('Ctrl Pts',(0.869462374029881,52.2885436481219,-1.49781758036796));
#49443=CARTESIAN_POINT('Ctrl Pts',(1.72993908299856,52.2091689559076,-0.082055425117027));
#49444=CARTESIAN_POINT('Ctrl Pts',(1.0073304972326,52.1297942636935,1.40879650525601));
#49445=CARTESIAN_POINT('Ctrl Pts',(-0.637096731444034,52.0504195714793,
1.61044406271855));
#49446=CARTESIAN_POINT('Ctrl Pts',(-1.69851009683004,51.9710448792651,0.338357464117524));
#49447=CARTESIAN_POINT('Ctrl Pts',(-1.2055991615173,51.8916701870509,-1.24336357767062));
#49448=CARTESIAN_POINT('Ctrl Pts',(0.390568141023166,51.8122954948368,-1.68726964487261));
#49449=CARTESIAN_POINT('Ctrl Pts',(1.62932246015966,51.7329208026226,-0.587137662407102));
#49450=CARTESIAN_POINT('Ctrl Pts',(1.37706681435153,51.6535461104084,1.05029011263948));
#49451=CARTESIAN_POINT('Ctrl Pts',(-0.135357051476193,51.5741714181942,
1.72658646294032));
#49452=CARTESIAN_POINT('Ctrl Pts',(-1.52391423268581,51.4947967259801,0.822865516477053));
#49453=CARTESIAN_POINT('Ctrl Pts',(-1.51792167730218,51.4154220337658,-0.833868206866928));
#49454=CARTESIAN_POINT('Ctrl Pts',(-0.122863029744826,51.3360473415517,
-1.72752051345823));
#49455=CARTESIAN_POINT('Ctrl Pts',(1.38462859005561,51.2566726493375,-1.04030063594932));
#49456=CARTESIAN_POINT('Ctrl Pts',(1.62503267349089,51.1772979571234,0.598908912336164));
#49457=CARTESIAN_POINT('Ctrl Pts',(0.378351379082027,51.0979232649091,1.69005123828274));
#49458=CARTESIAN_POINT('Ctrl Pts',(-1.21456118004716,51.018548572695,1.23460893456007));
#49459=CARTESIAN_POINT('Ctrl Pts',(-1.69602012104765,50.9391738804808,-0.350634684781572));
#49460=CARTESIAN_POINT('Ctrl Pts',(-0.62542553811471,50.8597991882666,-1.61501315957936));
#49461=CARTESIAN_POINT('Ctrl Pts',(1.01748710575982,50.7804244960525,-1.40146778009058));
#49462=CARTESIAN_POINT('Ctrl Pts',(1.72931688329718,50.7010498038382,0.0945587405418702));
#49463=CARTESIAN_POINT('Ctrl Pts',(0.858571433328937,50.6216751116241,1.50408625737625));
#49464=CARTESIAN_POINT('Ctrl Pts',(-0.797745172198436,50.5423004194099,
1.53714454711868));
#49465=CARTESIAN_POINT('Ctrl Pts',(-1.72426574129088,50.4629257271957,0.163671969299396));
#49466=CARTESIAN_POINT('Ctrl Pts',(-1.07244305206445,50.3835510349816,-1.35982639834679));
#49467=CARTESIAN_POINT('Ctrl Pts',(0.559899301331203,50.3041763427673,-1.63844563418453));
#49468=CARTESIAN_POINT('Ctrl Pts',(1.68161745751345,50.2248016505532,-0.418674646065943));
#49469=CARTESIAN_POINT('Ctrl Pts',(1.26094450061532,50.145426958339,1.18624560473938));
#49470=CARTESIAN_POINT('Ctrl Pts',(0.216585201145672,50.0925104968629,1.52892814110574));
#49471=CARTESIAN_POINT('Ctrl Pts',(-0.262716677134921,50.0660522661248,
1.44157906696032));
#49472=CARTESIAN_POINT('Ctrl Pts',(0.795430237244947,55.7252976988069,-1.11390647550743));
#49473=CARTESIAN_POINT('Ctrl Pts',(1.16588396190188,55.6988329658764,-0.849379768510902));
#49474=CARTESIAN_POINT('Ctrl Pts',(1.61551604518388,55.6459100022078,0.073843672828042));
#49475=CARTESIAN_POINT('Ctrl Pts',(0.812958424312154,55.5665288078012,1.39980458570529));
#49476=CARTESIAN_POINT('Ctrl Pts',(-0.734421508311664,55.487154115587,1.44100636256662));
#49477=CARTESIAN_POINT('Ctrl Pts',(-1.6092387870391,55.4077794233728,0.165328388039434));
#49478=CARTESIAN_POINT('Ctrl Pts',(-1.01167282522525,55.3284047311586,-1.26255339844229));
#49479=CARTESIAN_POINT('Ctrl Pts',(0.511811768669154,55.2490300389445,-1.53459668178578));
#49480=CARTESIAN_POINT('Ctrl Pts',(1.56686778633048,55.1696553467303,-0.402550043201726));
#49481=CARTESIAN_POINT('Ctrl Pts',(1.18809948112844,55.0902806545161,1.09799422018295));
#49482=CARTESIAN_POINT('Ctrl Pts',(-0.27792770957343,55.010905962302,1.59369149519038));
#49483=CARTESIAN_POINT('Ctrl Pts',(-1.48961187362816,54.9315312700877,0.631016130577541));
#49484=CARTESIAN_POINT('Ctrl Pts',(-1.33814099580097,54.8521565778736,-0.909124490476559));
#49485=CARTESIAN_POINT('Ctrl Pts',(0.0378788595129698,54.7727818856594,
-1.61730775895534));
#49486=CARTESIAN_POINT('Ctrl Pts',(1.37923425660231,54.6934071934452,-0.845479930115339));
#49487=CARTESIAN_POINT('Ctrl Pts',(1.45843857221207,54.614032501231,0.700057485907088));
#49488=CARTESIAN_POINT('Ctrl Pts',(0.203010251639913,54.5346578090168,1.60496393419256));
#49489=CARTESIAN_POINT('Ctrl Pts',(-1.23819471962175,54.4552831168027,1.04115169018566));
#49490=CARTESIAN_POINT('Ctrl Pts',(-1.54631486603372,54.3759084245884,-0.475429598018979));
#49491=CARTESIAN_POINT('Ctrl Pts',(-0.439386115103633,54.2965337323744,
-1.55694016311845));
#49492=CARTESIAN_POINT('Ctrl Pts',(1.06962943226405,54.2171590401601,-1.21367862028938));
#49493=CARTESIAN_POINT('Ctrl Pts',(1.59981594183729,54.137784347946,0.24023292068326));
#49494=CARTESIAN_POINT('Ctrl Pts',(0.665994194889158,54.0584096557318,1.47430479227282));
#49495=CARTESIAN_POINT('Ctrl Pts',(-0.877285782311934,53.9790349635176,
1.35922498361067));
#49496=CARTESIAN_POINT('Ctrl Pts',(-1.61775239297073,53.8996602713034,0.000304213471934397));
#49497=CARTESIAN_POINT('Ctrl Pts',(-0.877796918012653,53.8202855790893,
-1.35889494314889));
#49498=CARTESIAN_POINT('Ctrl Pts',(0.665439670066453,53.740910886875,-1.47455516779282));
#49499=CARTESIAN_POINT('Ctrl Pts',(1.5997254769442,53.661536194661,-0.240834580894265));
#49500=CARTESIAN_POINT('Ctrl Pts',(1.070085817626,53.5821615024466,1.21327624211495));
#49501=CARTESIAN_POINT('Ctrl Pts',(-0.438800532358591,53.5027868102325,
1.55710532391762));
#49502=CARTESIAN_POINT('Ctrl Pts',(-1.54613593933251,53.4234121180183,0.476011086012218));
#49503=CARTESIAN_POINT('Ctrl Pts',(-1.23858622489422,53.3440374258042,-1.04068586056936));
#49504=CARTESIAN_POINT('Ctrl Pts',(0.202406660085762,53.26466273359,-1.60504032375076));
#49505=CARTESIAN_POINT('Ctrl Pts',(1.45817509969987,53.1852880413758,-0.700605649076399));
#49506=CARTESIAN_POINT('Ctrl Pts',(1.37955229952733,53.1059133491616,0.844960561073897));
#49507=CARTESIAN_POINT('Ctrl Pts',(0.0384868038977224,53.0265386569474,
1.61729455042378));
#49508=CARTESIAN_POINT('Ctrl Pts',(-1.33779836732483,52.9471639647332,0.909625431310262));
#49509=CARTESIAN_POINT('Ctrl Pts',(-1.48985030186337,52.8677892725191,-0.630451405693282));
#49510=CARTESIAN_POINT('Ctrl Pts',(-0.278524688804058,52.7884145803049,
-1.59359558691344));
#49511=CARTESIAN_POINT('Ctrl Pts',(1.18768177147418,52.7090398880908,-1.09842382831613));
#49512=CARTESIAN_POINT('Ctrl Pts',(1.56702825736679,52.6296651958765,0.401927030088108));
#49513=CARTESIAN_POINT('Ctrl Pts',(0.512370843760241,52.5502905036624,1.53447027190719));
#49514=CARTESIAN_POINT('Ctrl Pts',(-1.01116247204977,52.4709158114481,1.26280376624051));
#49515=CARTESIAN_POINT('Ctrl Pts',(-1.60937046513623,52.391541119234,-0.164467634609069));
#49516=CARTESIAN_POINT('Ctrl Pts',(-0.734826762860395,52.3121664270198,
-1.44123298792605));
#49517=CARTESIAN_POINT('Ctrl Pts',(0.812164573021694,52.2327917348056,-1.39911100463804));
#49518=CARTESIAN_POINT('Ctrl Pts',(1.61593563869248,52.1534170425915,-0.0766479508427663));
#49519=CARTESIAN_POINT('Ctrl Pts',(0.940947150346172,52.0740423503773,1.31595644198213));
#49520=CARTESIAN_POINT('Ctrl Pts',(-0.595111887899797,51.9946676581631,
1.50431537193601));
#49521=CARTESIAN_POINT('Ctrl Pts',(-1.58657783104664,51.9152929659489,0.316059617508257));
#49522=CARTESIAN_POINT('Ctrl Pts',(-1.12614985707864,51.8359182737347,-1.16142558819327));
#49523=CARTESIAN_POINT('Ctrl Pts',(0.364829596960867,51.7565435815206,-1.5760781278539));
#49524=CARTESIAN_POINT('Ctrl Pts',(1.52194967797967,51.6771688893063,-0.548445134760282));
#49525=CARTESIAN_POINT('Ctrl Pts',(1.28631774612217,51.5977941970922,0.981075715705936));
#49526=CARTESIAN_POINT('Ctrl Pts',(-0.126436985890621,51.5184195048781,
1.61280395718511));
#49527=CARTESIAN_POINT('Ctrl Pts',(-1.42348788064797,51.4390448126638,0.768638460737906));
#49528=CARTESIAN_POINT('Ctrl Pts',(-1.41789023625319,51.3596701204497,-0.77891607091346));
#49529=CARTESIAN_POINT('Ctrl Pts',(-0.114766323504441,51.2802954282355,
-1.6136764535262));
#49530=CARTESIAN_POINT('Ctrl Pts',(1.29338119880216,51.2009207360213,-0.971744548178601));
#49531=CARTESIAN_POINT('Ctrl Pts',(1.51794258938992,51.1215460438071,0.559440656197589));
#49532=CARTESIAN_POINT('Ctrl Pts',(0.353417922871217,51.0421713515929,1.57867641352069));
#49533=CARTESIAN_POINT('Ctrl Pts',(-1.13452127621088,50.9627966593788,1.15324787838522));
#49534=CARTESIAN_POINT('Ctrl Pts',(-1.58425194532859,50.8834219671646,-0.327527766074945));
#49535=CARTESIAN_POINT('Ctrl Pts',(-0.584209829305774,50.8040472749504,
-1.50858336410208));
#49536=CARTESIAN_POINT('Ctrl Pts',(0.950434435678181,50.7246725827362,-1.30911068174848));
#49537=CARTESIAN_POINT('Ctrl Pts',(1.61535444211641,50.6452978905221,0.0883272944655598));
#49538=CARTESIAN_POINT('Ctrl Pts',(0.801991348200938,50.5659231983079,1.4049665741692));
#49539=CARTESIAN_POINT('Ctrl Pts',(-0.745173553808545,50.4865485060937,
1.43584631385136));
#49540=CARTESIAN_POINT('Ctrl Pts',(-1.61063617170777,50.4071738138795,0.152885943120856));
#49541=CARTESIAN_POINT('Ctrl Pts',(-1.00176877054839,50.3277991216654,-1.27021347810388));
#49542=CARTESIAN_POINT('Ctrl Pts',(0.523001788902224,50.2484244294511,-1.53047163241706));
#49543=CARTESIAN_POINT('Ctrl Pts',(1.57079842114053,50.169049737237,-0.391083875868172));
#49544=CARTESIAN_POINT('Ctrl Pts',(1.1778479236539,50.0896750450228,1.10807170482447));
#49545=CARTESIAN_POINT('Ctrl Pts',(0.202312178957201,50.0367585835467,1.42817137117346));
#49546=CARTESIAN_POINT('Ctrl Pts',(-0.245403578445858,50.0103003528086,
1.34657862417702));
#49547=CARTESIAN_POINT('Ctrl Pts',(0.739313035185779,55.6695457854907,-1.03532093546362));
#49548=CARTESIAN_POINT('Ctrl Pts',(1.083631436408,55.6430810525602,-0.789456454230577));
#49549=CARTESIAN_POINT('Ctrl Pts',(1.50154220298821,55.5901580888916,0.0686340389533847));
#49550=CARTESIAN_POINT('Ctrl Pts',(0.755604617495797,55.5107768944851,1.30104907818089));
#49551=CARTESIAN_POINT('Ctrl Pts',(-0.68260844130874,55.4314022022709,1.33934409046493));
#49552=CARTESIAN_POINT('Ctrl Pts',(-1.49570780223958,55.3520275100567,0.153664553647287));
#49553=CARTESIAN_POINT('Ctrl Pts',(-0.94029981764689,55.2726528178425,-1.1734808929561));
#49554=CARTESIAN_POINT('Ctrl Pts',(0.475703706523887,55.1932781256284,-1.42633165986584));
#49555=CARTESIAN_POINT('Ctrl Pts',(1.45632605426098,55.1139034334141,-0.374150340681581));
#49556=CARTESIAN_POINT('Ctrl Pts',(1.10427966195761,55.0345287411999,1.02053128172687));
#49557=CARTESIAN_POINT('Ctrl Pts',(-0.258320049836994,54.9551540489857,
1.48125736398945));
#49558=CARTESIAN_POINT('Ctrl Pts',(-1.38452050723547,54.8757793567716,0.586498260820829));
#49559=CARTESIAN_POINT('Ctrl Pts',(-1.24373582344404,54.7964046645574,-0.844986216194058));
#49560=CARTESIAN_POINT('Ctrl Pts',(0.0352065250786907,54.7170299723433,
-1.50320751225676));
#49561=CARTESIAN_POINT('Ctrl Pts',(1.2819299754214,54.6376552801291,-0.785831747466921));
#49562=CARTESIAN_POINT('Ctrl Pts',(1.3555464665119,54.5582805879149,0.650668783353174));
#49563=CARTESIAN_POINT('Ctrl Pts',(0.188687980775752,54.4789058957007,1.49173453810533));
#49564=CARTESIAN_POINT('Ctrl Pts',(-1.15084070664095,54.3995312034865,0.967698963552123));
#49565=CARTESIAN_POINT('Ctrl Pts',(-1.4372231321252,54.3201565112723,-0.441888279663587));
#49566=CARTESIAN_POINT('Ctrl Pts',(-0.408387646289231,54.2407818190582,
-1.44709881985952));
#49567=CARTESIAN_POINT('Ctrl Pts',(0.994167615289757,54.161407126844,-1.12805420575169));
#49568=CARTESIAN_POINT('Ctrl Pts',(1.48694973401431,54.0820324346299,0.223284609291508));
#49569=CARTESIAN_POINT('Ctrl Pts',(0.619008640336589,54.0026577424155,1.37029333274956));
#49570=CARTESIAN_POINT('Ctrl Pts',(-0.815393712832464,53.9232830502014,
1.26333234654755));
#49571=CARTESIAN_POINT('Ctrl Pts',(-1.5036207775666,53.8439083579873,0.00028275136491501));
#49572=CARTESIAN_POINT('Ctrl Pts',(-0.815868788167283,53.7645336657731,
-1.2630255902739));
#49573=CARTESIAN_POINT('Ctrl Pts',(0.61849323696046,53.6851589735588,-1.37052604440289));
#49574=CARTESIAN_POINT('Ctrl Pts',(1.48686565137381,53.6057842813446,-0.223843822678064));
#49575=CARTESIAN_POINT('Ctrl Pts',(0.994591802894592,53.5264095891306,1.12768021515453));
#49576=CARTESIAN_POINT('Ctrl Pts',(-0.407843376111522,53.4470348969164,
1.4472523286476));
#49577=CARTESIAN_POINT('Ctrl Pts',(-1.43705682861252,53.3676602047021,0.442428743972167));
#49578=CARTESIAN_POINT('Ctrl Pts',(-1.1512045914139,53.2882855124879,-0.967265997980326));
#49579=CARTESIAN_POINT('Ctrl Pts',(0.188126972301334,53.2089108202738,-1.49180553841872));
#49580=CARTESIAN_POINT('Ctrl Pts',(1.35530158185256,53.1295361280597,-0.651178273887347));
#49581=CARTESIAN_POINT('Ctrl Pts',(1.28222558057846,53.0501614358455,0.785349019649418));
#49582=CARTESIAN_POINT('Ctrl Pts',(0.0357715792937075,52.9707867436312,
1.50319523558043));
#49583=CARTESIAN_POINT('Ctrl Pts',(-1.2434173672341,52.8914120514171,0.845451815904586));
#49584=CARTESIAN_POINT('Ctrl Pts',(-1.38474211447894,52.812037359203,-0.585973376992345));
#49585=CARTESIAN_POINT('Ctrl Pts',(-0.25887491248398,52.7326626669888,-1.48116822199308));
#49586=CARTESIAN_POINT('Ctrl Pts',(1.1038914215088,52.6532879747745,-1.02093058122293));
#49587=CARTESIAN_POINT('Ctrl Pts',(1.45647520414661,52.5739132825604,0.37357128082892));
#49588=CARTESIAN_POINT('Ctrl Pts',(0.476223339149259,52.4945385903463,1.42621416814043));
#49589=CARTESIAN_POINT('Ctrl Pts',(-0.939825469630544,52.4151638981321,
1.17371359743243));
#49590=CARTESIAN_POINT('Ctrl Pts',(-1.49583019051336,52.3357892059178,-0.152864525937322));
#49591=CARTESIAN_POINT('Ctrl Pts',(-0.682985105353439,52.2564145137037,
-1.33955472751957));
#49592=CARTESIAN_POINT('Ctrl Pts',(0.754866772013506,52.1770398214895,-1.30040442890812));
#49593=CARTESIAN_POINT('Ctrl Pts',(1.50193219438641,52.0976651292753,-0.0712404765685076));
#49594=CARTESIAN_POINT('Ctrl Pts',(0.874563803459747,52.0182904370612,1.22311637870825));
#49595=CARTESIAN_POINT('Ctrl Pts',(-0.55312704435556,51.938915744847,1.39818668115346));
#49596=CARTESIAN_POINT('Ctrl Pts',(-1.47464556526325,51.8595410526328,0.29376177089899));
#49597=CARTESIAN_POINT('Ctrl Pts',(-1.04670055263997,51.7801663604186,-1.07948759871594));
#49598=CARTESIAN_POINT('Ctrl Pts',(0.339091052898566,51.7007916682045,-1.46488661083518));
#49599=CARTESIAN_POINT('Ctrl Pts',(1.41457689579969,51.6214169759902,-0.509752607113461));
#49600=CARTESIAN_POINT('Ctrl Pts',(1.19556867789281,51.5420422837761,0.911861318772394));
#49601=CARTESIAN_POINT('Ctrl Pts',(-0.117516920305048,51.4626675915619,
1.4990214514299));
#49602=CARTESIAN_POINT('Ctrl Pts',(-1.32306152861013,51.3832928993478,0.714411404998759));
#49603=CARTESIAN_POINT('Ctrl Pts',(-1.3178587952042,51.3039182071334,-0.723963934959992));
#49604=CARTESIAN_POINT('Ctrl Pts',(-0.106669617264056,51.2245435149194,
-1.49983239359417));
#49605=CARTESIAN_POINT('Ctrl Pts',(1.20213380754871,51.1451688227052,-0.90318846040789));
#49606=CARTESIAN_POINT('Ctrl Pts',(1.41085250528894,51.065794130491,0.519972400059012));
#49607=CARTESIAN_POINT('Ctrl Pts',(0.328484466660406,50.9864194382767,1.46730158875865));
#49608=CARTESIAN_POINT('Ctrl Pts',(-1.0544813723746,50.9070447460626,1.07188682221037));
#49609=CARTESIAN_POINT('Ctrl Pts',(-1.47248376960954,50.8276700538485,-0.304420847368318));
#49610=CARTESIAN_POINT('Ctrl Pts',(-0.542994120496838,50.7482953616341,
-1.40215356862481));
#49611=CARTESIAN_POINT('Ctrl Pts',(0.883381765596545,50.6689206694202,-1.2167535834064));
#49612=CARTESIAN_POINT('Ctrl Pts',(1.50139200093565,50.5895459772059,0.0820958483892505));
#49613=CARTESIAN_POINT('Ctrl Pts',(0.745411263072938,50.5101712849918,1.30584689096214));
#49614=CARTESIAN_POINT('Ctrl Pts',(-0.692601935418653,50.4307965927775,
1.33454808058404));
#49615=CARTESIAN_POINT('Ctrl Pts',(-1.49700660212466,50.3514219005633,0.142099916942318));
#49616=CARTESIAN_POINT('Ctrl Pts',(-0.93109448903233,50.2720472083492,-1.18060055786096));
#49617=CARTESIAN_POINT('Ctrl Pts',(0.486104276473247,50.192672516135,-1.4224976306496));
#49618=CARTESIAN_POINT('Ctrl Pts',(1.4599793847676,50.1132978239209,-0.363493105670402));
#49619=CARTESIAN_POINT('Ctrl Pts',(1.09475134669248,50.0339231317067,1.02989780490955));
#49620=CARTESIAN_POINT('Ctrl Pts',(0.188039156768732,49.9810066702304,1.32741460124119));
#49621=CARTESIAN_POINT('Ctrl Pts',(-0.228090479756796,49.9545484394925,
1.2515781813937));
#49622=CARTESIAN_POINT('Ctrl Pts',(0.68319583312661,55.6137938721746,-0.956735395419802));
#49623=CARTESIAN_POINT('Ctrl Pts',(1.00137891091411,55.5873291392441,-0.729533139950251));
#49624=CARTESIAN_POINT('Ctrl Pts',(1.38756836079254,55.5344061755755,0.0634244050787278));
#49625=CARTESIAN_POINT('Ctrl Pts',(0.69825081067944,55.4550249811689,1.20229357065649));
#49626=CARTESIAN_POINT('Ctrl Pts',(-0.630795374305817,55.3756502889546,
1.23768181836324));
#49627=CARTESIAN_POINT('Ctrl Pts',(-1.38217681744006,55.2962755967406,0.14200071925514));
#49628=CARTESIAN_POINT('Ctrl Pts',(-0.868926810068525,55.2169009045263,
-1.08440838746992));
#49629=CARTESIAN_POINT('Ctrl Pts',(0.43959564437862,55.1375262123122,-1.31806663794589));
#49630=CARTESIAN_POINT('Ctrl Pts',(1.34578432219146,55.0581515200979,-0.345750638161437));
#49631=CARTESIAN_POINT('Ctrl Pts',(1.02045984278677,54.9787768278838,0.943068343270797));
#49632=CARTESIAN_POINT('Ctrl Pts',(-0.238712390100558,54.8994021356696,
1.36882323278852));
#49633=CARTESIAN_POINT('Ctrl Pts',(-1.27942914084278,54.8200274434554,0.541980391064116));
#49634=CARTESIAN_POINT('Ctrl Pts',(-1.1493306510871,54.7406527512412,-0.780847941911555));
#49635=CARTESIAN_POINT('Ctrl Pts',(0.0325341906444134,54.661278059027,-1.38910726555817));
#49636=CARTESIAN_POINT('Ctrl Pts',(1.18462569424049,54.5819033668129,-0.726183564818503));
#49637=CARTESIAN_POINT('Ctrl Pts',(1.25265436081173,54.5025286745987,0.601280080799261));
#49638=CARTESIAN_POINT('Ctrl Pts',(0.174365709911593,54.4231539823845,1.3785051420181));
#49639=CARTESIAN_POINT('Ctrl Pts',(-1.06348669366016,54.3437792901703,0.894246236918589));
#49640=CARTESIAN_POINT('Ctrl Pts',(-1.32813139821668,54.2644045979561,-0.408346961308196));
#49641=CARTESIAN_POINT('Ctrl Pts',(-0.377389177474829,54.185029905742,-1.33725747660058));
#49642=CARTESIAN_POINT('Ctrl Pts',(0.918705798315464,54.1056552135278,-1.04242979121399));
#49643=CARTESIAN_POINT('Ctrl Pts',(1.37408352619134,54.0262805213136,0.206336297899756));
#49644=CARTESIAN_POINT('Ctrl Pts',(0.572023085784021,53.9469058290994,1.26628187322631));
#49645=CARTESIAN_POINT('Ctrl Pts',(-0.753501643352997,53.8675311368853,
1.16743970948443));
#49646=CARTESIAN_POINT('Ctrl Pts',(-1.38948916216248,53.7881564446711,0.00026128925789496));
#49647=CARTESIAN_POINT('Ctrl Pts',(-0.753940658321912,53.7087817524569,
-1.16715623739892));
#49648=CARTESIAN_POINT('Ctrl Pts',(0.571546803854467,53.6294070602427,-1.26649692101297));
#49649=CARTESIAN_POINT('Ctrl Pts',(1.3740058258034,53.5500323680285,-0.206853064461862));
#49650=CARTESIAN_POINT('Ctrl Pts',(0.919097788163184,53.4706576758144,1.0420841881941));
#49651=CARTESIAN_POINT('Ctrl Pts',(-0.376886219864453,53.3912829836002,
1.33739933337758));
#49652=CARTESIAN_POINT('Ctrl Pts',(-1.32797771789253,53.311908291386,0.408846401932117));
#49653=CARTESIAN_POINT('Ctrl Pts',(-1.06382295793358,53.2325335991718,-0.893846135391286));
#49654=CARTESIAN_POINT('Ctrl Pts',(0.173847284516908,53.1531589069577,-1.37857075308668));
#49655=CARTESIAN_POINT('Ctrl Pts',(1.25242806400526,53.0737842147435,-0.601750898698296));
#49656=CARTESIAN_POINT('Ctrl Pts',(1.18489886162958,52.9944095225293,0.725737478224937));
#49657=CARTESIAN_POINT('Ctrl Pts',(0.033056354689693,52.9150348303151,1.38909592073708));
#49658=CARTESIAN_POINT('Ctrl Pts',(-1.14903636714335,52.835660138101,0.781278200498908));
#49659=CARTESIAN_POINT('Ctrl Pts',(-1.27963392709449,52.7562854458867,-0.541495348291405));
#49660=CARTESIAN_POINT('Ctrl Pts',(-0.239225136163902,52.6769107536726,
-1.36874085707271));
#49661=CARTESIAN_POINT('Ctrl Pts',(1.0201010715434,52.5975360614583,-0.943437334129717));
#49662=CARTESIAN_POINT('Ctrl Pts',(1.34592215092642,52.5181613692442,0.345215531569735));
#49663=CARTESIAN_POINT('Ctrl Pts',(0.440075834538276,52.43878667703,1.31795806437367));
#49664=CARTESIAN_POINT('Ctrl Pts',(-0.868488467211321,52.3594119848159,
1.08462342862434));
#49665=CARTESIAN_POINT('Ctrl Pts',(-1.38228991589051,52.2800372926017,-0.141261417265575));
#49666=CARTESIAN_POINT('Ctrl Pts',(-0.631143447846485,52.2006626003875,
-1.23787646711307));
#49667=CARTESIAN_POINT('Ctrl Pts',(0.69756897100532,52.1212879081734,-1.2016978531782));
#49668=CARTESIAN_POINT('Ctrl Pts',(1.38792875008033,52.0419132159591,-0.065833002294249));
#49669=CARTESIAN_POINT('Ctrl Pts',(0.808180456573323,51.962538523745,1.13027631543437));
#49670=CARTESIAN_POINT('Ctrl Pts',(-0.511142200811324,51.8831638315307,
1.29205799037093));
#49671=CARTESIAN_POINT('Ctrl Pts',(-1.36271329947986,51.8037891393167,0.271463924289723));
#49672=CARTESIAN_POINT('Ctrl Pts',(-0.967251248201307,51.7244144471024,
-0.9975496092386));
#49673=CARTESIAN_POINT('Ctrl Pts',(0.313352508836268,51.6450397548883,-1.35369509381647));
#49674=CARTESIAN_POINT('Ctrl Pts',(1.30720411361969,51.565665062674,-0.471060079466639));
#49675=CARTESIAN_POINT('Ctrl Pts',(1.10481960966345,51.4862903704599,0.84264692183885));
#49676=CARTESIAN_POINT('Ctrl Pts',(-0.108596854719476,51.4069156782457,
1.38523894567469));
#49677=CARTESIAN_POINT('Ctrl Pts',(-1.22263517657228,51.3275409860315,0.660184349259611));
#49678=CARTESIAN_POINT('Ctrl Pts',(-1.21782735415521,51.2481662938174,-0.669011799006525));
#49679=CARTESIAN_POINT('Ctrl Pts',(-0.0985729110236722,51.1687916016031,
-1.38598833366215));
#49680=CARTESIAN_POINT('Ctrl Pts',(1.11088641629526,51.089416909389,-0.83463237263718));
#49681=CARTESIAN_POINT('Ctrl Pts',(1.30376242118797,51.0100422171748,0.480504143920437));
#49682=CARTESIAN_POINT('Ctrl Pts',(0.303551010449595,50.9306675249606,1.3559267639966));
#49683=CARTESIAN_POINT('Ctrl Pts',(-0.97444146853832,50.8512928327465,0.990525766035526));
#49684=CARTESIAN_POINT('Ctrl Pts',(-1.36071559389048,50.7719181405323,-0.281313928661689));
#49685=CARTESIAN_POINT('Ctrl Pts',(-0.501778411687899,50.6925434483181,
-1.29572377314753));
#49686=CARTESIAN_POINT('Ctrl Pts',(0.816329095514904,50.6131687561039,-1.12439648506431));
#49687=CARTESIAN_POINT('Ctrl Pts',(1.38742955975489,50.5337940638897,0.0758644023129377));
#49688=CARTESIAN_POINT('Ctrl Pts',(0.688831177944937,50.4544193716755,1.20672720775508));
#49689=CARTESIAN_POINT('Ctrl Pts',(-0.640030317028762,50.3750446794614,
1.23324984731672));
#49690=CARTESIAN_POINT('Ctrl Pts',(-1.38337703254154,50.2956699872472,0.131313890763781));
#49691=CARTESIAN_POINT('Ctrl Pts',(-0.860420207516269,50.216295295033,-1.09098763761804));
#49692=CARTESIAN_POINT('Ctrl Pts',(0.449206764044268,50.1369206028188,-1.31452362888213));
#49693=CARTESIAN_POINT('Ctrl Pts',(1.34916034839469,50.0575459106046,-0.335902335472633));
#49694=CARTESIAN_POINT('Ctrl Pts',(1.01165476973106,49.9781712183904,0.951723904994636));
#49695=CARTESIAN_POINT('Ctrl Pts',(0.173766134580262,49.9252547569143,1.22665783130891));
#49696=CARTESIAN_POINT('Ctrl Pts',(-0.210777381067733,49.8987965261763,
1.15657773861039));
#49697=CARTESIAN_POINT('Ctrl Pts',(0.634286466388226,55.615,1.31890595895111));
#49698=CARTESIAN_POINT('Ctrl Pts',(0.642198332342847,55.615,1.31501256253275));
#49699=CARTESIAN_POINT('Ctrl Pts',(0.650110198297467,55.615,1.3111191661144));
#49700=CARTESIAN_POINT('Ctrl Pts',(0.658022064252088,55.615,1.30722576969605));
#49701=CARTESIAN_POINT('Origin',(0.,55.615,0.));
#49702=CARTESIAN_POINT('',(-1.91473527046689E-16,55.715,-1.5635));
#49703=CARTESIAN_POINT('Origin',(0.,55.715,0.));
#49704=CARTESIAN_POINT('Origin',(-1.91473527046689E-16,55.615,-1.5635));
#49705=CARTESIAN_POINT('Origin',(0.,55.715,0.));
#49706=CARTESIAN_POINT('',(-3.12284933782575E-16,55.715,-2.55));
#49707=CARTESIAN_POINT('Origin',(0.,55.715,0.));
#49708=CARTESIAN_POINT('Origin',(0.,49.89,0.));
#49709=CARTESIAN_POINT('',(-1.1135,49.715,1.36364421085058E-16));
#49710=CARTESIAN_POINT('',(-1.2885,49.89,1.57795740070136E-16));
#49711=CARTESIAN_POINT('Origin',(0.,49.715,0.));
#49712=CARTESIAN_POINT('Origin',(0.,49.715,0.));
#49713=CARTESIAN_POINT('Origin',(2.56050015783174,58.715,-0.451485261934019));
#49714=CARTESIAN_POINT('',(2.56050015783174,58.565,-0.451485261934019));
#49715=CARTESIAN_POINT('',(2.69848592069234,58.415,-0.529786500229296));
#49716=CARTESIAN_POINT('Ctrl Pts',(2.56050015783174,58.565,-0.451485261934019));
#49717=CARTESIAN_POINT('Ctrl Pts',(2.62755865940943,58.4923524443611,-0.489538200171299));
#49718=CARTESIAN_POINT('Ctrl Pts',(2.69848592069235,58.415,-0.529786500229297));
#49719=CARTESIAN_POINT('',(2.56050015783174,56.315,-0.451485261934019));
#49720=CARTESIAN_POINT('',(2.56050015783174,58.715,-0.451485261934019));
#49721=CARTESIAN_POINT('',(2.69848592069234,56.315,-0.529786500229296));
#49722=CARTESIAN_POINT('',(2.56050015783174,56.315,-0.451485261934019));
#49723=CARTESIAN_POINT('',(2.69848592069234,55.715,-0.529786500229296));
#49724=CARTESIAN_POINT('Origin',(2.78208190225949,56.315,-0.490556101909078));
#49725=CARTESIAN_POINT('',(2.71694496170969,56.315,-0.425100076500034));
#49726=CARTESIAN_POINT('Origin',(0.,56.315,0.));
#49727=CARTESIAN_POINT('',(3.03144735511394,56.315,-0.372057701402184));
#49728=CARTESIAN_POINT('Origin',(3.03144735511394,58.715,-0.372057701402184));
#49729=CARTESIAN_POINT('',(2.71694496170969,58.415,-0.425100076500034));
#49730=CARTESIAN_POINT('Ctrl Pts',(2.71694496170969,58.415,-0.425100076500033));
#49731=CARTESIAN_POINT('Ctrl Pts',(2.63652940831481,58.4923524443615,-0.438662554994084));
#49732=CARTESIAN_POINT('Ctrl Pts',(2.56050015783174,58.565,-0.451485261934019));
#49733=CARTESIAN_POINT('',(2.71694496170969,55.715,-0.425100076500034));
#49734=CARTESIAN_POINT('Origin',(0.,55.715,0.));
#49735=CARTESIAN_POINT('',(-2.74948631640946,56.315,0.0531506902789203));
#49736=CARTESIAN_POINT('',(-2.75,56.315,3.36777869765522E-16));
#49737=CARTESIAN_POINT('Origin',(0.,56.315,0.));
#49738=CARTESIAN_POINT('',(-2.75,55.915,3.36777869765522E-16));
#49739=CARTESIAN_POINT('',(-2.75,55.715,3.36777869765522E-16));
#49740=CARTESIAN_POINT('',(-3.36777869765522E-16,55.915,-2.75));
#49741=CARTESIAN_POINT('Origin',(0.,55.915,0.));
#49742=CARTESIAN_POINT('Origin',(0.,55.915,0.));
#49743=CARTESIAN_POINT('',(-2.74948631640946,56.315,-0.0531506902789196));
#49744=CARTESIAN_POINT('Origin',(0.,56.315,0.));
#49745=CARTESIAN_POINT('',(-2.74948631640946,58.415,-0.0531506902789196));
#49746=CARTESIAN_POINT('',(-2.74948631640946,55.715,-0.0531506902789196));
#49747=CARTESIAN_POINT('',(-2.71694496170969,58.415,-0.425100076500032));
#49748=CARTESIAN_POINT('Origin',(0.,58.415,0.));
#49749=CARTESIAN_POINT('',(-2.71694496170969,56.315,-0.425100076500032));
#49750=CARTESIAN_POINT('',(-2.71694496170969,55.715,-0.425100076500032));
#49751=CARTESIAN_POINT('',(-2.69848592069234,56.315,-0.529786500229295));
#49752=CARTESIAN_POINT('Origin',(0.,56.315,0.));
#49753=CARTESIAN_POINT('',(-2.69848592069234,58.415,-0.529786500229295));
#49754=CARTESIAN_POINT('',(-2.69848592069234,55.715,-0.529786500229295));
#49755=CARTESIAN_POINT('',(-2.60185060918886,58.415,-0.890434392565551));
#49756=CARTESIAN_POINT('Origin',(0.,58.415,0.));
#49757=CARTESIAN_POINT('',(-2.60185060918886,56.315,-0.890434392565551));
#49758=CARTESIAN_POINT('',(-2.60185060918886,55.715,-0.890434392565551));
#49759=CARTESIAN_POINT('',(-2.56549339577475,56.315,-0.990325015455108));
#49760=CARTESIAN_POINT('Origin',(0.,56.315,0.));
#49761=CARTESIAN_POINT('',(-2.56549339577475,58.415,-0.990325015455107));
#49762=CARTESIAN_POINT('',(-2.56549339577475,55.715,-0.990325015455107));
#49763=CARTESIAN_POINT('',(-2.40770034250775,58.415,-1.32871331019451));
#49764=CARTESIAN_POINT('Origin',(0.,58.415,0.));
#49765=CARTESIAN_POINT('',(-2.40770034250775,56.315,-1.32871331019451));
#49766=CARTESIAN_POINT('',(-2.40770034250775,55.715,-1.32871331019451));
#49767=CARTESIAN_POINT('',(-2.35454965222883,56.315,-1.42077300621495));
#49768=CARTESIAN_POINT('Origin',(0.,56.315,0.));
#49769=CARTESIAN_POINT('',(-2.35454965222883,58.415,-1.42077300621495));
#49770=CARTESIAN_POINT('',(-2.35454965222883,55.715,-1.42077300621495));
#49771=CARTESIAN_POINT('',(-2.14039331927471,58.415,-1.72661994625458));
#49772=CARTESIAN_POINT('Origin',(0.,58.415,0.));
#49773=CARTESIAN_POINT('',(-2.14039331927471,56.315,-1.72661994625458));
#49774=CARTESIAN_POINT('',(-2.14039331927471,55.715,-1.72661994625458));
#49775=CARTESIAN_POINT('',(-2.07206410895956,56.315,-1.80805152812679));
#49776=CARTESIAN_POINT('Origin',(0.,56.315,0.));
#49777=CARTESIAN_POINT('',(-2.07206410895956,58.415,-1.80805152812679));
#49778=CARTESIAN_POINT('',(-2.07206410895956,55.715,-1.80805152812679));
#49779=CARTESIAN_POINT('',(-1.80805152812679,58.415,-2.07206410895956));
#49780=CARTESIAN_POINT('Origin',(0.,58.415,0.));
#49781=CARTESIAN_POINT('',(-1.80805152812679,56.315,-2.07206410895956));
#49782=CARTESIAN_POINT('',(-1.80805152812679,55.715,-2.07206410895956));
#49783=CARTESIAN_POINT('',(-1.72661994625458,56.315,-2.14039331927471));
#49784=CARTESIAN_POINT('Origin',(0.,56.315,0.));
#49785=CARTESIAN_POINT('',(-1.72661994625458,58.415,-2.14039331927471));
#49786=CARTESIAN_POINT('',(-1.72661994625458,55.715,-2.14039331927471));
#49787=CARTESIAN_POINT('',(-1.42077300621496,58.415,-2.35454965222883));
#49788=CARTESIAN_POINT('Origin',(0.,58.415,0.));
#49789=CARTESIAN_POINT('',(-1.42077300621496,56.315,-2.35454965222883));
#49790=CARTESIAN_POINT('',(-1.42077300621496,55.715,-2.35454965222883));
#49791=CARTESIAN_POINT('',(-1.32871331019451,56.315,-2.40770034250775));
#49792=CARTESIAN_POINT('Origin',(0.,56.315,0.));
#49793=CARTESIAN_POINT('',(-1.32871331019451,58.415,-2.40770034250775));
#49794=CARTESIAN_POINT('',(-1.32871331019451,55.715,-2.40770034250775));
#49795=CARTESIAN_POINT('',(-0.99032501545511,58.415,-2.56549339577475));
#49796=CARTESIAN_POINT('Origin',(0.,58.415,0.));
#49797=CARTESIAN_POINT('',(-0.99032501545511,56.315,-2.56549339577475));
#49798=CARTESIAN_POINT('',(-0.99032501545511,55.715,-2.56549339577475));
#49799=CARTESIAN_POINT('',(-0.890434392565553,56.315,-2.60185060918886));
#49800=CARTESIAN_POINT('Origin',(0.,56.315,0.));
#49801=CARTESIAN_POINT('',(-0.890434392565553,58.415,-2.60185060918885));
#49802=CARTESIAN_POINT('',(-0.890434392565553,55.715,-2.60185060918885));
#49803=CARTESIAN_POINT('',(-0.529786500229296,58.415,-2.69848592069234));
#49804=CARTESIAN_POINT('Origin',(0.,58.415,0.));
#49805=CARTESIAN_POINT('',(-0.529786500229296,56.315,-2.69848592069234));
#49806=CARTESIAN_POINT('',(-0.529786500229296,55.715,-2.69848592069234));
#49807=CARTESIAN_POINT('',(-0.425100076500033,56.315,-2.71694496170969));
#49808=CARTESIAN_POINT('Origin',(0.,56.315,0.));
#49809=CARTESIAN_POINT('',(-0.425100076500033,58.415,-2.71694496170969));
#49810=CARTESIAN_POINT('',(-0.425100076500033,55.715,-2.71694496170969));
#49811=CARTESIAN_POINT('',(-0.0531506902789204,58.415,-2.74948631640946));
#49812=CARTESIAN_POINT('Origin',(0.,58.415,0.));
#49813=CARTESIAN_POINT('',(-0.0531506902789204,56.315,-2.74948631640946));
#49814=CARTESIAN_POINT('',(-0.0531506902789204,55.715,-2.74948631640946));
#49815=CARTESIAN_POINT('',(0.0531506902789194,56.315,-2.74948631640946));
#49816=CARTESIAN_POINT('Origin',(0.,56.315,0.));
#49817=CARTESIAN_POINT('',(0.0531506902789194,58.415,-2.74948631640946));
#49818=CARTESIAN_POINT('',(0.0531506902789194,55.715,-2.74948631640946));
#49819=CARTESIAN_POINT('',(0.425100076500032,58.415,-2.71694496170969));
#49820=CARTESIAN_POINT('Origin',(0.,58.415,0.));
#49821=CARTESIAN_POINT('',(0.425100076500032,56.315,-2.71694496170969));
#49822=CARTESIAN_POINT('',(0.425100076500032,55.715,-2.71694496170969));
#49823=CARTESIAN_POINT('',(0.529786500229294,56.315,-2.69848592069234));
#49824=CARTESIAN_POINT('Origin',(0.,56.315,0.));
#49825=CARTESIAN_POINT('',(0.529786500229294,58.415,-2.69848592069234));
#49826=CARTESIAN_POINT('',(0.529786500229294,55.715,-2.69848592069234));
#49827=CARTESIAN_POINT('',(0.890434392565549,58.415,-2.60185060918886));
#49828=CARTESIAN_POINT('Origin',(0.,58.415,0.));
#49829=CARTESIAN_POINT('',(0.890434392565549,56.315,-2.60185060918886));
#49830=CARTESIAN_POINT('',(0.890434392565549,55.715,-2.60185060918886));
#49831=CARTESIAN_POINT('',(0.990325015455106,56.315,-2.56549339577475));
#49832=CARTESIAN_POINT('Origin',(0.,56.315,0.));
#49833=CARTESIAN_POINT('',(0.990325015455106,58.415,-2.56549339577475));
#49834=CARTESIAN_POINT('',(0.990325015455106,55.715,-2.56549339577475));
#49835=CARTESIAN_POINT('',(1.32871331019451,58.415,-2.40770034250775));
#49836=CARTESIAN_POINT('Origin',(0.,58.415,0.));
#49837=CARTESIAN_POINT('',(1.32871331019451,56.315,-2.40770034250775));
#49838=CARTESIAN_POINT('',(1.32871331019451,55.715,-2.40770034250775));
#49839=CARTESIAN_POINT('',(1.42077300621496,56.315,-2.35454965222883));
#49840=CARTESIAN_POINT('Origin',(0.,56.315,0.));
#49841=CARTESIAN_POINT('',(1.42077300621495,58.415,-2.35454965222883));
#49842=CARTESIAN_POINT('',(1.42077300621495,55.715,-2.35454965222883));
#49843=CARTESIAN_POINT('',(1.72661994625458,58.415,-2.14039331927471));
#49844=CARTESIAN_POINT('Origin',(0.,58.415,0.));
#49845=CARTESIAN_POINT('',(1.72661994625458,56.315,-2.14039331927471));
#49846=CARTESIAN_POINT('',(1.72661994625458,55.715,-2.14039331927471));
#49847=CARTESIAN_POINT('',(1.80805152812679,56.315,-2.07206410895956));
#49848=CARTESIAN_POINT('Origin',(0.,56.315,0.));
#49849=CARTESIAN_POINT('',(1.80805152812679,58.415,-2.07206410895956));
#49850=CARTESIAN_POINT('',(1.80805152812679,55.715,-2.07206410895956));
#49851=CARTESIAN_POINT('',(2.07206410895956,58.415,-1.80805152812679));
#49852=CARTESIAN_POINT('Origin',(0.,58.415,0.));
#49853=CARTESIAN_POINT('',(2.07206410895956,56.315,-1.80805152812679));
#49854=CARTESIAN_POINT('',(2.07206410895956,55.715,-1.80805152812679));
#49855=CARTESIAN_POINT('',(2.14039331927471,56.315,-1.72661994625458));
#49856=CARTESIAN_POINT('Origin',(0.,56.315,0.));
#49857=CARTESIAN_POINT('',(2.14039331927471,58.415,-1.72661994625458));
#49858=CARTESIAN_POINT('',(2.14039331927471,55.715,-1.72661994625458));
#49859=CARTESIAN_POINT('',(2.35454965222883,58.415,-1.42077300621496));
#49860=CARTESIAN_POINT('Origin',(0.,58.415,0.));
#49861=CARTESIAN_POINT('',(2.35454965222883,56.315,-1.42077300621496));
#49862=CARTESIAN_POINT('',(2.35454965222883,55.715,-1.42077300621496));
#49863=CARTESIAN_POINT('',(2.40770034250775,56.315,-1.32871331019451));
#49864=CARTESIAN_POINT('Origin',(0.,56.315,0.));
#49865=CARTESIAN_POINT('',(2.40770034250775,58.415,-1.32871331019451));
#49866=CARTESIAN_POINT('',(2.40770034250775,55.715,-1.32871331019451));
#49867=CARTESIAN_POINT('',(2.56549339577475,58.415,-0.99032501545511));
#49868=CARTESIAN_POINT('Origin',(0.,58.415,0.));
#49869=CARTESIAN_POINT('',(2.56549339577475,56.315,-0.99032501545511));
#49870=CARTESIAN_POINT('',(2.56549339577475,55.715,-0.99032501545511));
#49871=CARTESIAN_POINT('',(2.60185060918885,56.315,-0.890434392565553));
#49872=CARTESIAN_POINT('Origin',(0.,56.315,0.));
#49873=CARTESIAN_POINT('',(2.60185060918885,58.415,-0.890434392565553));
#49874=CARTESIAN_POINT('',(2.60185060918885,55.715,-0.890434392565553));
#49875=CARTESIAN_POINT('Origin',(0.,58.415,0.));
#49876=CARTESIAN_POINT('',(2.74948631640946,58.415,-0.0531506902789199));
#49877=CARTESIAN_POINT('Origin',(0.,58.415,0.));
#49878=CARTESIAN_POINT('',(2.74948631640946,56.315,-0.0531506902789199));
#49879=CARTESIAN_POINT('',(2.74948631640946,55.715,-0.0531506902789199));
#49880=CARTESIAN_POINT('',(2.74948631640946,56.315,0.0531506902789197));
#49881=CARTESIAN_POINT('Origin',(0.,56.315,0.));
#49882=CARTESIAN_POINT('',(2.74948631640946,58.415,0.0531506902789197));
#49883=CARTESIAN_POINT('',(2.74948631640946,55.715,0.0531506902789197));
#49884=CARTESIAN_POINT('',(2.71694496170969,58.415,0.425100076500033));
#49885=CARTESIAN_POINT('Origin',(0.,58.415,0.));
#49886=CARTESIAN_POINT('',(2.71694496170969,56.315,0.425100076500033));
#49887=CARTESIAN_POINT('',(2.71694496170969,55.715,0.425100076500033));
#49888=CARTESIAN_POINT('',(2.69848592069234,56.315,0.529786500229295));
#49889=CARTESIAN_POINT('Origin',(0.,56.315,0.));
#49890=CARTESIAN_POINT('',(2.69848592069234,58.415,0.529786500229295));
#49891=CARTESIAN_POINT('',(2.69848592069234,55.715,0.529786500229295));
#49892=CARTESIAN_POINT('',(2.60185060918886,58.415,0.890434392565551));
#49893=CARTESIAN_POINT('Origin',(0.,58.415,0.));
#49894=CARTESIAN_POINT('',(2.60185060918886,56.315,0.890434392565551));
#49895=CARTESIAN_POINT('',(2.60185060918886,55.715,0.890434392565551));
#49896=CARTESIAN_POINT('',(2.56549339577475,56.315,0.990325015455108));
#49897=CARTESIAN_POINT('Origin',(0.,56.315,0.));
#49898=CARTESIAN_POINT('',(2.56549339577475,58.415,0.990325015455108));
#49899=CARTESIAN_POINT('',(2.56549339577475,55.715,0.990325015455108));
#49900=CARTESIAN_POINT('',(2.40770034250775,58.415,1.32871331019451));
#49901=CARTESIAN_POINT('Origin',(0.,58.415,0.));
#49902=CARTESIAN_POINT('',(2.40770034250775,56.315,1.32871331019451));
#49903=CARTESIAN_POINT('',(2.40770034250775,55.715,1.32871331019451));
#49904=CARTESIAN_POINT('',(2.35454965222883,56.315,1.42077300621495));
#49905=CARTESIAN_POINT('Origin',(0.,56.315,0.));
#49906=CARTESIAN_POINT('',(2.35454965222883,58.415,1.42077300621495));
#49907=CARTESIAN_POINT('',(2.35454965222883,55.715,1.42077300621495));
#49908=CARTESIAN_POINT('',(2.14039331927471,58.415,1.72661994625458));
#49909=CARTESIAN_POINT('Origin',(0.,58.415,0.));
#49910=CARTESIAN_POINT('',(2.14039331927471,56.315,1.72661994625458));
#49911=CARTESIAN_POINT('',(2.14039331927471,55.715,1.72661994625458));
#49912=CARTESIAN_POINT('',(2.07206410895956,56.315,1.80805152812679));
#49913=CARTESIAN_POINT('Origin',(0.,56.315,0.));
#49914=CARTESIAN_POINT('',(2.07206410895956,58.415,1.80805152812679));
#49915=CARTESIAN_POINT('',(2.07206410895956,55.715,1.80805152812679));
#49916=CARTESIAN_POINT('',(1.80805152812679,58.415,2.07206410895956));
#49917=CARTESIAN_POINT('Origin',(0.,58.415,0.));
#49918=CARTESIAN_POINT('',(1.80805152812679,56.315,2.07206410895956));
#49919=CARTESIAN_POINT('',(1.80805152812679,55.715,2.07206410895956));
#49920=CARTESIAN_POINT('',(1.72661994625458,56.315,2.14039331927471));
#49921=CARTESIAN_POINT('Origin',(0.,56.315,0.));
#49922=CARTESIAN_POINT('',(1.72661994625458,58.415,2.14039331927471));
#49923=CARTESIAN_POINT('',(1.72661994625458,55.715,2.14039331927471));
#49924=CARTESIAN_POINT('',(1.42077300621495,58.415,2.35454965222883));
#49925=CARTESIAN_POINT('Origin',(0.,58.415,0.));
#49926=CARTESIAN_POINT('',(1.42077300621496,56.315,2.35454965222883));
#49927=CARTESIAN_POINT('',(1.42077300621495,55.715,2.35454965222883));
#49928=CARTESIAN_POINT('',(1.32871331019451,56.315,2.40770034250775));
#49929=CARTESIAN_POINT('Origin',(0.,56.315,0.));
#49930=CARTESIAN_POINT('',(1.32871331019451,58.415,2.40770034250775));
#49931=CARTESIAN_POINT('',(1.32871331019451,55.715,2.40770034250775));
#49932=CARTESIAN_POINT('',(0.990325015455108,58.415,2.56549339577475));
#49933=CARTESIAN_POINT('Origin',(0.,58.415,0.));
#49934=CARTESIAN_POINT('',(0.990325015455108,56.315,2.56549339577475));
#49935=CARTESIAN_POINT('',(0.990325015455108,55.715,2.56549339577475));
#49936=CARTESIAN_POINT('',(0.890434392565551,56.315,2.60185060918886));
#49937=CARTESIAN_POINT('Origin',(0.,56.315,0.));
#49938=CARTESIAN_POINT('',(0.890434392565551,58.415,2.60185060918886));
#49939=CARTESIAN_POINT('',(0.890434392565551,55.715,2.60185060918886));
#49940=CARTESIAN_POINT('',(0.529786500229295,58.415,2.69848592069234));
#49941=CARTESIAN_POINT('Origin',(0.,58.415,0.));
#49942=CARTESIAN_POINT('',(0.529786500229296,56.315,2.69848592069234));
#49943=CARTESIAN_POINT('',(0.529786500229295,55.715,2.69848592069234));
#49944=CARTESIAN_POINT('',(0.425100076500034,56.315,2.71694496170969));
#49945=CARTESIAN_POINT('Origin',(0.,56.315,0.));
#49946=CARTESIAN_POINT('',(0.425100076500033,58.415,2.71694496170969));
#49947=CARTESIAN_POINT('',(0.425100076500033,55.715,2.71694496170969));
#49948=CARTESIAN_POINT('',(0.05315069027892,58.415,2.74948631640946));
#49949=CARTESIAN_POINT('Origin',(0.,58.415,0.));
#49950=CARTESIAN_POINT('',(0.0531506902789201,56.315,2.74948631640946));
#49951=CARTESIAN_POINT('',(0.05315069027892,55.715,2.74948631640946));
#49952=CARTESIAN_POINT('',(-0.0531506902789196,56.315,2.74948631640946));
#49953=CARTESIAN_POINT('Origin',(0.,56.315,0.));
#49954=CARTESIAN_POINT('',(-0.0531506902789199,58.415,2.74948631640946));
#49955=CARTESIAN_POINT('',(-0.0531506902789199,55.715,2.74948631640946));
#49956=CARTESIAN_POINT('',(-0.425100076500033,58.415,2.71694496170969));
#49957=CARTESIAN_POINT('Origin',(0.,58.415,0.));
#49958=CARTESIAN_POINT('',(-0.425100076500033,56.315,2.71694496170969));
#49959=CARTESIAN_POINT('',(-0.425100076500033,55.715,2.71694496170969));
#49960=CARTESIAN_POINT('',(-0.529786500229295,56.315,2.69848592069234));
#49961=CARTESIAN_POINT('Origin',(0.,56.315,0.));
#49962=CARTESIAN_POINT('',(-0.529786500229295,58.415,2.69848592069234));
#49963=CARTESIAN_POINT('',(-0.529786500229295,55.715,2.69848592069234));
#49964=CARTESIAN_POINT('',(-0.890434392565551,58.415,2.60185060918886));
#49965=CARTESIAN_POINT('Origin',(0.,58.415,0.));
#49966=CARTESIAN_POINT('',(-0.890434392565551,56.315,2.60185060918886));
#49967=CARTESIAN_POINT('',(-0.890434392565551,55.715,2.60185060918886));
#49968=CARTESIAN_POINT('',(-0.990325015455108,56.315,2.56549339577475));
#49969=CARTESIAN_POINT('Origin',(0.,56.315,0.));
#49970=CARTESIAN_POINT('',(-0.990325015455108,58.415,2.56549339577475));
#49971=CARTESIAN_POINT('',(-0.990325015455108,55.715,2.56549339577475));
#49972=CARTESIAN_POINT('',(-1.32871331019451,58.415,2.40770034250775));
#49973=CARTESIAN_POINT('Origin',(0.,58.415,0.));
#49974=CARTESIAN_POINT('',(-1.32871331019451,56.315,2.40770034250775));
#49975=CARTESIAN_POINT('',(-1.32871331019451,55.715,2.40770034250775));
#49976=CARTESIAN_POINT('',(-1.42077300621495,56.315,2.35454965222883));
#49977=CARTESIAN_POINT('Origin',(0.,56.315,0.));
#49978=CARTESIAN_POINT('',(-1.42077300621495,58.415,2.35454965222883));
#49979=CARTESIAN_POINT('',(-1.42077300621495,55.715,2.35454965222883));
#49980=CARTESIAN_POINT('',(-1.72661994625458,58.415,2.14039331927471));
#49981=CARTESIAN_POINT('Origin',(0.,58.415,0.));
#49982=CARTESIAN_POINT('',(-1.72661994625458,56.315,2.14039331927471));
#49983=CARTESIAN_POINT('',(-1.72661994625458,55.715,2.14039331927471));
#49984=CARTESIAN_POINT('',(-1.80805152812679,56.315,2.07206410895956));
#49985=CARTESIAN_POINT('Origin',(0.,56.315,0.));
#49986=CARTESIAN_POINT('',(-1.80805152812679,58.415,2.07206410895956));
#49987=CARTESIAN_POINT('',(-1.80805152812679,55.715,2.07206410895956));
#49988=CARTESIAN_POINT('',(-2.07206410895956,58.415,1.80805152812679));
#49989=CARTESIAN_POINT('Origin',(0.,58.415,0.));
#49990=CARTESIAN_POINT('',(-2.07206410895956,56.315,1.80805152812679));
#49991=CARTESIAN_POINT('',(-2.07206410895956,55.715,1.80805152812679));
#49992=CARTESIAN_POINT('',(-2.14039331927471,56.315,1.72661994625458));
#49993=CARTESIAN_POINT('Origin',(0.,56.315,0.));
#49994=CARTESIAN_POINT('',(-2.14039331927471,58.415,1.72661994625458));
#49995=CARTESIAN_POINT('',(-2.14039331927471,55.715,1.72661994625458));
#49996=CARTESIAN_POINT('',(-2.35454965222883,58.415,1.42077300621495));
#49997=CARTESIAN_POINT('Origin',(0.,58.415,0.));
#49998=CARTESIAN_POINT('',(-2.35454965222883,56.315,1.42077300621495));
#49999=CARTESIAN_POINT('',(-2.35454965222883,55.715,1.42077300621495));
#50000=CARTESIAN_POINT('',(-2.40770034250775,56.315,1.32871331019451));
#50001=CARTESIAN_POINT('Origin',(0.,56.315,0.));
#50002=CARTESIAN_POINT('',(-2.40770034250775,58.415,1.32871331019451));
#50003=CARTESIAN_POINT('',(-2.40770034250775,55.715,1.32871331019451));
#50004=CARTESIAN_POINT('',(-2.56549339577475,58.415,0.990325015455108));
#50005=CARTESIAN_POINT('Origin',(0.,58.415,0.));
#50006=CARTESIAN_POINT('',(-2.56549339577475,56.315,0.990325015455108));
#50007=CARTESIAN_POINT('',(-2.56549339577475,55.715,0.990325015455108));
#50008=CARTESIAN_POINT('',(-2.60185060918886,56.315,0.890434392565551));
#50009=CARTESIAN_POINT('Origin',(0.,56.315,0.));
#50010=CARTESIAN_POINT('',(-2.60185060918886,58.415,0.890434392565551));
#50011=CARTESIAN_POINT('',(-2.60185060918886,55.715,0.890434392565551));
#50012=CARTESIAN_POINT('',(-2.69848592069234,58.415,0.529786500229296));
#50013=CARTESIAN_POINT('Origin',(0.,58.415,0.));
#50014=CARTESIAN_POINT('',(-2.69848592069234,56.315,0.529786500229296));
#50015=CARTESIAN_POINT('',(-2.69848592069234,55.715,0.529786500229296));
#50016=CARTESIAN_POINT('',(-2.71694496170969,56.315,0.425100076500034));
#50017=CARTESIAN_POINT('Origin',(0.,56.315,0.));
#50018=CARTESIAN_POINT('',(-2.71694496170969,58.415,0.425100076500034));
#50019=CARTESIAN_POINT('',(-2.71694496170969,55.715,0.425100076500034));
#50020=CARTESIAN_POINT('',(-2.74948631640946,58.415,0.0531506902789201));
#50021=CARTESIAN_POINT('Origin',(0.,58.415,0.));
#50022=CARTESIAN_POINT('',(-2.74948631640946,55.715,0.0531506902789201));
#50023=CARTESIAN_POINT('Origin',(2.44320081404336,58.715,-0.889252372646741));
#50024=CARTESIAN_POINT('',(2.44320081404336,58.565,-0.88925237264674));
#50025=CARTESIAN_POINT('Ctrl Pts',(2.44320081404336,58.565,-0.88925237264674));
#50026=CARTESIAN_POINT('Ctrl Pts',(2.50263272292269,58.4923524443611,-0.938371787843764));
#50027=CARTESIAN_POINT('Ctrl Pts',(2.56549339577475,58.415,-0.990325015455113));
#50028=CARTESIAN_POINT('',(2.44320081404336,56.315,-0.889252372646741));
#50029=CARTESIAN_POINT('',(2.44320081404336,58.715,-0.889252372646741));
#50030=CARTESIAN_POINT('',(2.44320081404336,56.315,-0.889252372646741));
#50031=CARTESIAN_POINT('Origin',(2.65463165372019,56.315,-0.966206904895016));
#50032=CARTESIAN_POINT('',(2.92078571632913,56.315,-0.892810617817547));
#50033=CARTESIAN_POINT('Origin',(2.92078571632913,58.715,-0.892810617817547));
#50034=CARTESIAN_POINT('Ctrl Pts',(2.60185060918886,58.415,-0.890434392565553));
#50035=CARTESIAN_POINT('Ctrl Pts',(2.52030164906794,58.4923524443612,-0.889826812233457));
#50036=CARTESIAN_POINT('Ctrl Pts',(2.44320081404336,58.565,-0.88925237264674));
#50037=CARTESIAN_POINT('Origin',(2.25166604983954,58.715,-1.3));
#50038=CARTESIAN_POINT('',(2.25166604983954,58.565,-1.3));
#50039=CARTESIAN_POINT('Ctrl Pts',(2.25166604983954,58.565,-1.3));
#50040=CARTESIAN_POINT('Ctrl Pts',(2.301665557543,58.4923524443614,-1.3586934235814));
#50041=CARTESIAN_POINT('Ctrl Pts',(2.35454965222884,58.415,-1.42077300621496));
#50042=CARTESIAN_POINT('',(2.25166604983954,56.315,-1.3));
#50043=CARTESIAN_POINT('',(2.25166604983954,58.715,-1.3));
#50044=CARTESIAN_POINT('',(2.25166604983954,56.315,-1.3));
#50045=CARTESIAN_POINT('Origin',(2.44652176569104,56.315,-1.4125));
#50046=CARTESIAN_POINT('',(2.72137748154254,56.315,-1.38643593539449));
#50047=CARTESIAN_POINT('Origin',(2.72137748154254,58.715,-1.38643593539449));
#50048=CARTESIAN_POINT('Ctrl Pts',(2.40770034250776,58.415,-1.32871331019451));
#50049=CARTESIAN_POINT('Ctrl Pts',(2.32749579954827,58.492352444361,-1.31395413205729));
#50050=CARTESIAN_POINT('Ctrl Pts',(2.25166604983954,58.565,-1.3));
#50051=CARTESIAN_POINT('Origin',(1.99171555210934,58.715,-1.671247785185));
#50052=CARTESIAN_POINT('',(1.99171555210934,58.565,-1.671247785185));
#50053=CARTESIAN_POINT('Ctrl Pts',(1.99171555210934,58.565,-1.671247785185));
#50054=CARTESIAN_POINT('Ctrl Pts',(2.03076344889672,58.4923524443611,-1.73773184717601));
#50055=CARTESIAN_POINT('Ctrl Pts',(2.07206410895956,58.415,-1.8080515281268));
#50056=CARTESIAN_POINT('',(1.99171555210934,56.315,-1.671247785185));
#50057=CARTESIAN_POINT('',(1.99171555210934,58.715,-1.671247785185));
#50058=CARTESIAN_POINT('',(1.99171555210934,56.315,-1.671247785185));
#50059=CARTESIAN_POINT('Origin',(2.16407555181111,56.315,-1.81587499736447));
#50060=CARTESIAN_POINT('',(2.43928156906273,56.315,-1.83793509864491));
#50061=CARTESIAN_POINT('Origin',(2.43928156906273,58.715,-1.83793509864491));
#50062=CARTESIAN_POINT('Ctrl Pts',(2.14039331927472,58.415,-1.72661994625458));
#50063=CARTESIAN_POINT('Ctrl Pts',(2.06397016792854,58.4923524443612,-1.69815762047134));
#50064=CARTESIAN_POINT('Ctrl Pts',(1.99171555210934,58.565,-1.671247785185));
#50065=CARTESIAN_POINT('Origin',(1.671247785185,58.715,-1.99171555210934));
#50066=CARTESIAN_POINT('',(1.671247785185,58.565,-1.99171555210934));
#50067=CARTESIAN_POINT('Ctrl Pts',(1.671247785185,58.565,-1.99171555210934));
#50068=CARTESIAN_POINT('Ctrl Pts',(1.69815762047149,58.4923524443608,-2.06397016792894));
#50069=CARTESIAN_POINT('Ctrl Pts',(1.72661994625458,58.415,-2.14039331927472));
#50070=CARTESIAN_POINT('',(1.671247785185,56.315,-1.99171555210934));
#50071=CARTESIAN_POINT('',(1.671247785185,58.715,-1.99171555210934));
#50072=CARTESIAN_POINT('',(1.671247785185,56.315,-1.99171555210934));
#50073=CARTESIAN_POINT('Origin',(1.81587499736447,56.315,-2.16407555181111));
#50074=CARTESIAN_POINT('',(2.08306932044298,56.315,-2.23358953396304));
#50075=CARTESIAN_POINT('Origin',(2.08306932044298,58.715,-2.23358953396304));
#50076=CARTESIAN_POINT('Ctrl Pts',(1.80805152812679,58.415,-2.07206410895956));
#50077=CARTESIAN_POINT('Ctrl Pts',(1.73773184717629,58.4923524443608,-2.03076344889689));
#50078=CARTESIAN_POINT('Ctrl Pts',(1.671247785185,58.565,-1.99171555210934));
#50079=CARTESIAN_POINT('Origin',(1.3,58.715,-2.25166604983954));
#50080=CARTESIAN_POINT('',(1.3,58.565,-2.25166604983954));
#50081=CARTESIAN_POINT('Ctrl Pts',(1.3,58.565,-2.25166604983954));
#50082=CARTESIAN_POINT('Ctrl Pts',(1.31395413205732,58.4923524443609,-2.32749579954839));
#50083=CARTESIAN_POINT('Ctrl Pts',(1.32871331019451,58.415,-2.40770034250776));
#50084=CARTESIAN_POINT('',(1.3,56.315,-2.25166604983954));
#50085=CARTESIAN_POINT('',(1.3,58.715,-2.25166604983954));
#50086=CARTESIAN_POINT('',(1.3,56.315,-2.25166604983954));
#50087=CARTESIAN_POINT('Origin',(1.4125,56.315,-2.44652176569104));
#50088=CARTESIAN_POINT('',(1.66356406460551,56.315,-2.56137748154254));
#50089=CARTESIAN_POINT('Origin',(1.66356406460551,58.715,-2.56137748154254));
#50090=CARTESIAN_POINT('Ctrl Pts',(1.42077300621496,58.415,-2.35454965222884));
#50091=CARTESIAN_POINT('Ctrl Pts',(1.35869342358154,58.4923524443612,-2.30166555754312));
#50092=CARTESIAN_POINT('Ctrl Pts',(1.3,58.565,-2.25166604983954));
#50093=CARTESIAN_POINT('Origin',(0.889252372646737,58.715,-2.44320081404336));
#50094=CARTESIAN_POINT('',(0.889252372646737,58.565,-2.44320081404336));
#50095=CARTESIAN_POINT('Ctrl Pts',(0.889252372646737,58.565,-2.44320081404336));
#50096=CARTESIAN_POINT('Ctrl Pts',(0.889826812233453,58.4923524443614,-2.52030164906772));
#50097=CARTESIAN_POINT('Ctrl Pts',(0.890434392565549,58.415,-2.60185060918886));
#50098=CARTESIAN_POINT('',(0.889252372646737,56.315,-2.44320081404336));
#50099=CARTESIAN_POINT('',(0.889252372646737,58.715,-2.44320081404336));
#50100=CARTESIAN_POINT('',(0.889252372646737,56.315,-2.44320081404336));
#50101=CARTESIAN_POINT('Origin',(0.966206904895013,56.315,-2.65463165372019));
#50102=CARTESIAN_POINT('',(1.19351225646903,56.315,-2.81133927046491));
#50103=CARTESIAN_POINT('Origin',(1.19351225646903,58.715,-2.81133927046491));
#50104=CARTESIAN_POINT('Ctrl Pts',(0.990325015455109,58.415,-2.56549339577475));
#50105=CARTESIAN_POINT('Ctrl Pts',(0.938371787843648,58.4923524443613,-2.50263272292255));
#50106=CARTESIAN_POINT('Ctrl Pts',(0.889252372646737,58.565,-2.44320081404336));
#50107=CARTESIAN_POINT('Origin',(0.451485261934018,58.715,-2.56050015783174));
#50108=CARTESIAN_POINT('',(0.451485261934018,58.565,-2.56050015783174));
#50109=CARTESIAN_POINT('Ctrl Pts',(0.451485261934018,58.565,-2.56050015783174));
#50110=CARTESIAN_POINT('Ctrl Pts',(0.438662554994094,58.4923524443615,-2.63652940831474));
#50111=CARTESIAN_POINT('Ctrl Pts',(0.425100076500031,58.415,-2.71694496170969));
#50112=CARTESIAN_POINT('',(0.451485261934018,56.315,-2.56050015783174));
#50113=CARTESIAN_POINT('',(0.451485261934018,58.715,-2.56050015783174));
#50114=CARTESIAN_POINT('',(0.451485261934018,56.315,-2.56050015783174));
#50115=CARTESIAN_POINT('Origin',(0.490556101909077,56.315,-2.78208190225949));
#50116=CARTESIAN_POINT('',(0.68719618236609,56.315,-2.97587993826053));
#50117=CARTESIAN_POINT('Origin',(0.68719618236609,58.715,-2.97587993826053));
#50118=CARTESIAN_POINT('Ctrl Pts',(0.529786500229297,58.415,-2.69848592069235));
#50119=CARTESIAN_POINT('Ctrl Pts',(0.48953820017136,58.492352444361,-2.62755865940953));
#50120=CARTESIAN_POINT('Ctrl Pts',(0.451485261934018,58.565,-2.56050015783174));
#50121=CARTESIAN_POINT('Origin',(-4.77612251667468E-16,58.715,-2.6));
#50122=CARTESIAN_POINT('',(-4.77612251667468E-16,58.565,-2.6));
#50123=CARTESIAN_POINT('Ctrl Pts',(-4.77612251667468E-16,58.565,-2.6));
#50124=CARTESIAN_POINT('Ctrl Pts',(-0.0258302420049523,58.4923524443611,
-2.67264755563893));
#50125=CARTESIAN_POINT('Ctrl Pts',(-0.053150690278922,58.415,-2.74948631640947));
#50126=CARTESIAN_POINT('',(-4.77612251667468E-16,56.315,-2.6));
#50127=CARTESIAN_POINT('',(-4.77612251667468E-16,58.715,-2.6));
#50128=CARTESIAN_POINT('',(-4.77612251667468E-16,56.315,-2.6));
#50129=CARTESIAN_POINT('Origin',(-5.18944081138691E-16,56.315,-2.825));
#50130=CARTESIAN_POINT('',(0.159999999999999,56.315,-3.05));
#50131=CARTESIAN_POINT('Origin',(0.159999999999999,58.715,-3.05));
#50132=CARTESIAN_POINT('Ctrl Pts',(0.0531506902789212,58.415,-2.74948631640947));
#50133=CARTESIAN_POINT('Ctrl Pts',(0.0258302420049448,58.4923524443611,
-2.67264755563891));
#50134=CARTESIAN_POINT('Ctrl Pts',(-4.77612251667468E-16,58.565,-2.6));
#50135=CARTESIAN_POINT('Origin',(-0.451485261934019,58.715,-2.56050015783174));
#50136=CARTESIAN_POINT('',(-0.451485261934019,58.565,-2.56050015783174));
#50137=CARTESIAN_POINT('Ctrl Pts',(-0.451485261934019,58.565,-2.56050015783174));
#50138=CARTESIAN_POINT('Ctrl Pts',(-0.489538200171262,58.4923524443612,
-2.62755865940936));
#50139=CARTESIAN_POINT('Ctrl Pts',(-0.529786500229298,58.415,-2.69848592069235));
#50140=CARTESIAN_POINT('',(-0.451485261934019,56.315,-2.56050015783174));
#50141=CARTESIAN_POINT('',(-0.451485261934019,58.715,-2.56050015783174));
#50142=CARTESIAN_POINT('',(-0.451485261934019,56.315,-2.56050015783174));
#50143=CARTESIAN_POINT('Origin',(-0.490556101909078,56.315,-2.78208190225949));
#50144=CARTESIAN_POINT('',(-0.372057701402184,56.315,-3.03144735511394));
#50145=CARTESIAN_POINT('Origin',(-0.372057701402184,58.715,-3.03144735511394));
#50146=CARTESIAN_POINT('Ctrl Pts',(-0.425100076500033,58.415,-2.71694496170969));
#50147=CARTESIAN_POINT('Ctrl Pts',(-0.438662554993996,58.4923524443609,
-2.63652940831532));
#50148=CARTESIAN_POINT('Ctrl Pts',(-0.451485261934019,58.565,-2.56050015783174));
#50149=CARTESIAN_POINT('Origin',(-0.88925237264674,58.715,-2.44320081404336));
#50150=CARTESIAN_POINT('',(-0.88925237264674,58.565,-2.44320081404336));
#50151=CARTESIAN_POINT('Ctrl Pts',(-0.889252372646741,58.565,-2.44320081404336));
#50152=CARTESIAN_POINT('Ctrl Pts',(-0.938371787843537,58.4923524443615,
-2.50263272292241));
#50153=CARTESIAN_POINT('Ctrl Pts',(-0.990325015455113,58.415,-2.56549339577475));
#50154=CARTESIAN_POINT('',(-0.88925237264674,56.315,-2.44320081404336));
#50155=CARTESIAN_POINT('',(-0.88925237264674,58.715,-2.44320081404336));
#50156=CARTESIAN_POINT('',(-0.88925237264674,56.315,-2.44320081404336));
#50157=CARTESIAN_POINT('Origin',(-0.966206904895016,56.315,-2.65463165372019));
#50158=CARTESIAN_POINT('',(-0.892810617817546,56.315,-2.92078571632913));
#50159=CARTESIAN_POINT('Origin',(-0.892810617817546,58.715,-2.92078571632913));
#50160=CARTESIAN_POINT('Ctrl Pts',(-0.890434392565553,58.415,-2.60185060918886));
#50161=CARTESIAN_POINT('Ctrl Pts',(-0.88982681223346,58.4923524443608,-2.52030164906832));
#50162=CARTESIAN_POINT('Ctrl Pts',(-0.88925237264674,58.565,-2.44320081404336));
#50163=CARTESIAN_POINT('Origin',(-1.3,58.715,-2.25166604983954));
#50164=CARTESIAN_POINT('',(-1.3,58.565,-2.25166604983954));
#50165=CARTESIAN_POINT('Ctrl Pts',(-1.3,58.565,-2.25166604983954));
#50166=CARTESIAN_POINT('Ctrl Pts',(-1.35869342358187,58.4923524443608,-2.30166555754341));
#50167=CARTESIAN_POINT('Ctrl Pts',(-1.42077300621496,58.415,-2.35454965222884));
#50168=CARTESIAN_POINT('',(-1.3,56.315,-2.25166604983954));
#50169=CARTESIAN_POINT('',(-1.3,58.715,-2.25166604983954));
#50170=CARTESIAN_POINT('',(-1.3,56.315,-2.25166604983954));
#50171=CARTESIAN_POINT('Origin',(-1.4125,56.315,-2.44652176569104));
#50172=CARTESIAN_POINT('',(-1.38643593539449,56.315,-2.72137748154254));
#50173=CARTESIAN_POINT('Origin',(-1.38643593539449,58.715,-2.72137748154254));
#50174=CARTESIAN_POINT('Ctrl Pts',(-1.32871331019451,58.415,-2.40770034250776));
#50175=CARTESIAN_POINT('Ctrl Pts',(-1.31395413205734,58.4923524443608,-2.3274957995485));
#50176=CARTESIAN_POINT('Ctrl Pts',(-1.3,58.565,-2.25166604983954));
#50177=CARTESIAN_POINT('Origin',(-1.671247785185,58.715,-1.99171555210934));
#50178=CARTESIAN_POINT('',(-1.671247785185,58.565,-1.99171555210934));
#50179=CARTESIAN_POINT('Ctrl Pts',(-1.671247785185,58.565,-1.99171555210934));
#50180=CARTESIAN_POINT('Ctrl Pts',(-1.7377318471757,58.4923524443614,-2.03076344889654));
#50181=CARTESIAN_POINT('Ctrl Pts',(-1.8080515281268,58.415,-2.07206410895956));
#50182=CARTESIAN_POINT('',(-1.671247785185,56.315,-1.99171555210934));
#50183=CARTESIAN_POINT('',(-1.671247785185,58.715,-1.99171555210934));
#50184=CARTESIAN_POINT('',(-1.671247785185,56.315,-1.99171555210934));
#50185=CARTESIAN_POINT('Origin',(-1.81587499736447,56.315,-2.16407555181111));
#50186=CARTESIAN_POINT('',(-1.83793509864491,56.315,-2.43928156906273));
#50187=CARTESIAN_POINT('Origin',(-1.83793509864491,58.715,-2.43928156906273));
#50188=CARTESIAN_POINT('Ctrl Pts',(-1.72661994625458,58.415,-2.14039331927472));
#50189=CARTESIAN_POINT('Ctrl Pts',(-1.69815762047141,58.4923524443611,-2.0639701679287));
#50190=CARTESIAN_POINT('Ctrl Pts',(-1.671247785185,58.565,-1.99171555210934));
#50191=CARTESIAN_POINT('Origin',(-1.99171555210934,58.715,-1.671247785185));
#50192=CARTESIAN_POINT('',(-1.99171555210934,58.565,-1.671247785185));
#50193=CARTESIAN_POINT('Ctrl Pts',(-1.99171555210934,58.565,-1.671247785185));
#50194=CARTESIAN_POINT('Ctrl Pts',(-2.06397016792865,58.4923524443611,-1.69815762047139));
#50195=CARTESIAN_POINT('Ctrl Pts',(-2.14039331927472,58.415,-1.72661994625458));
#50196=CARTESIAN_POINT('',(-1.99171555210934,56.315,-1.671247785185));
#50197=CARTESIAN_POINT('',(-1.99171555210934,58.715,-1.671247785185));
#50198=CARTESIAN_POINT('',(-1.99171555210934,56.315,-1.671247785185));
#50199=CARTESIAN_POINT('Origin',(-2.16407555181111,56.315,-1.81587499736447));
#50200=CARTESIAN_POINT('',(-2.23358953396304,56.315,-2.08306932044298));
#50201=CARTESIAN_POINT('Origin',(-2.23358953396304,58.715,-2.08306932044298));
#50202=CARTESIAN_POINT('Ctrl Pts',(-2.07206410895956,58.415,-1.8080515281268));
#50203=CARTESIAN_POINT('Ctrl Pts',(-2.03076344889677,58.492352444361,-1.73773184717609));
#50204=CARTESIAN_POINT('Ctrl Pts',(-1.99171555210934,58.565,-1.671247785185));
#50205=CARTESIAN_POINT('Origin',(-2.25166604983954,58.715,-1.3));
#50206=CARTESIAN_POINT('',(-2.25166604983954,58.565,-1.3));
#50207=CARTESIAN_POINT('Ctrl Pts',(-2.25166604983954,58.565,-1.3));
#50208=CARTESIAN_POINT('Ctrl Pts',(-2.32749579954808,58.4923524443612,-1.31395413205726));
#50209=CARTESIAN_POINT('Ctrl Pts',(-2.40770034250776,58.415,-1.32871331019451));
#50210=CARTESIAN_POINT('',(-2.25166604983954,56.315,-1.3));
#50211=CARTESIAN_POINT('',(-2.25166604983954,58.715,-1.3));
#50212=CARTESIAN_POINT('',(-2.25166604983954,56.315,-1.3));
#50213=CARTESIAN_POINT('Origin',(-2.44652176569104,56.315,-1.4125));
#50214=CARTESIAN_POINT('',(-2.56137748154254,56.315,-1.66356406460551));
#50215=CARTESIAN_POINT('Origin',(-2.56137748154254,58.715,-1.66356406460551));
#50216=CARTESIAN_POINT('Ctrl Pts',(-2.35454965222884,58.415,-1.42077300621496));
#50217=CARTESIAN_POINT('Ctrl Pts',(-2.30166555754322,58.4923524443611,-1.35869342358165));
#50218=CARTESIAN_POINT('Ctrl Pts',(-2.25166604983954,58.565,-1.3));
#50219=CARTESIAN_POINT('Origin',(-2.44320081404336,58.715,-0.889252372646739));
#50220=CARTESIAN_POINT('',(-2.44320081404336,58.565,-0.889252372646739));
#50221=CARTESIAN_POINT('Ctrl Pts',(-2.44320081404336,58.565,-0.889252372646739));
#50222=CARTESIAN_POINT('Ctrl Pts',(-2.52030164906835,58.4923524443608,-0.889826812233458));
#50223=CARTESIAN_POINT('Ctrl Pts',(-2.60185060918886,58.415,-0.890434392565551));
#50224=CARTESIAN_POINT('',(-2.44320081404336,56.315,-0.889252372646739));
#50225=CARTESIAN_POINT('',(-2.44320081404336,58.715,-0.889252372646739));
#50226=CARTESIAN_POINT('',(-2.44320081404336,56.315,-0.889252372646739));
#50227=CARTESIAN_POINT('Origin',(-2.65463165372019,56.315,-0.966206904895014));
#50228=CARTESIAN_POINT('',(-2.81133927046491,56.315,-1.19351225646903));
#50229=CARTESIAN_POINT('Origin',(-2.81133927046491,58.715,-1.19351225646903));
#50230=CARTESIAN_POINT('Ctrl Pts',(-2.56549339577475,58.415,-0.99032501545511));
#50231=CARTESIAN_POINT('Ctrl Pts',(-2.50263272292257,58.4923524443613,-0.938371787843666));
#50232=CARTESIAN_POINT('Ctrl Pts',(-2.44320081404336,58.565,-0.889252372646739));
#50233=CARTESIAN_POINT('Origin',(-2.56050015783174,58.715,-0.451485261934018));
#50234=CARTESIAN_POINT('',(-2.56050015783174,58.565,-0.451485261934018));
#50235=CARTESIAN_POINT('Ctrl Pts',(-2.56050015783174,58.565,-0.451485261934018));
#50236=CARTESIAN_POINT('Ctrl Pts',(-2.63652940831505,58.4923524443612,-0.438662554994041));
#50237=CARTESIAN_POINT('Ctrl Pts',(-2.71694496170969,58.415,-0.425100076500032));
#50238=CARTESIAN_POINT('',(-2.56050015783174,56.315,-0.451485261934018));
#50239=CARTESIAN_POINT('',(-2.56050015783174,58.715,-0.451485261934018));
#50240=CARTESIAN_POINT('',(-2.56050015783174,56.315,-0.451485261934018));
#50241=CARTESIAN_POINT('Origin',(-2.78208190225949,56.315,-0.490556101909077));
#50242=CARTESIAN_POINT('',(-2.97587993826053,56.315,-0.68719618236609));
#50243=CARTESIAN_POINT('Origin',(-2.97587993826053,58.715,-0.68719618236609));
#50244=CARTESIAN_POINT('Ctrl Pts',(-2.69848592069235,58.415,-0.529786500229297));
#50245=CARTESIAN_POINT('Ctrl Pts',(-2.62755865940921,58.4923524443614,-0.489538200171177));
#50246=CARTESIAN_POINT('Ctrl Pts',(-2.56050015783174,58.565,-0.451485261934018));
#50247=CARTESIAN_POINT('Origin',(-2.6,58.715,3.18408167778312E-16));
#50248=CARTESIAN_POINT('',(-2.6,58.565,3.18408167778312E-16));
#50249=CARTESIAN_POINT('Ctrl Pts',(-2.6,58.565,3.18408167778312E-16));
#50250=CARTESIAN_POINT('Ctrl Pts',(-2.67264755563861,58.4923524443614,0.0258302420048414));
#50251=CARTESIAN_POINT('Ctrl Pts',(-2.74948631640947,58.415,0.0531506902789219));
#50252=CARTESIAN_POINT('',(-2.6,56.315,3.18408167778312E-16));
#50253=CARTESIAN_POINT('',(-2.6,58.715,3.18408167778312E-16));
#50254=CARTESIAN_POINT('',(-2.6,56.315,3.18408167778312E-16));
#50255=CARTESIAN_POINT('Origin',(-2.825,56.315,3.45962720759127E-16));
#50256=CARTESIAN_POINT('',(-3.05,56.315,-0.16));
#50257=CARTESIAN_POINT('Origin',(-3.05,58.715,-0.16));
#50258=CARTESIAN_POINT('Ctrl Pts',(-2.74948631640947,58.415,-0.0531506902789213));
#50259=CARTESIAN_POINT('Ctrl Pts',(-2.67264755563921,58.4923524443608,-0.0258302420050519));
#50260=CARTESIAN_POINT('Ctrl Pts',(-2.6,58.565,3.18408167778312E-16));
#50261=CARTESIAN_POINT('Origin',(-2.56050015783174,58.715,0.45148526193402));
#50262=CARTESIAN_POINT('',(-2.56050015783174,58.565,0.45148526193402));
#50263=CARTESIAN_POINT('Ctrl Pts',(-2.56050015783174,58.565,0.45148526193402));
#50264=CARTESIAN_POINT('Ctrl Pts',(-2.62755865940922,58.4923524443614,0.489538200171184));
#50265=CARTESIAN_POINT('Ctrl Pts',(-2.69848592069235,58.415,0.529786500229298));
#50266=CARTESIAN_POINT('',(-2.56050015783174,56.315,0.45148526193402));
#50267=CARTESIAN_POINT('',(-2.56050015783174,58.715,0.45148526193402));
#50268=CARTESIAN_POINT('',(-2.56050015783174,56.315,0.45148526193402));
#50269=CARTESIAN_POINT('Origin',(-2.78208190225949,56.315,0.490556101909079));
#50270=CARTESIAN_POINT('',(-3.03144735511394,56.315,0.372057701402185));
#50271=CARTESIAN_POINT('Origin',(-3.03144735511394,58.715,0.372057701402185));
#50272=CARTESIAN_POINT('Ctrl Pts',(-2.71694496170969,58.415,0.425100076500033));
#50273=CARTESIAN_POINT('Ctrl Pts',(-2.63652940831533,58.4923524443609,0.438662554993998));
#50274=CARTESIAN_POINT('Ctrl Pts',(-2.56050015783174,58.565,0.45148526193402));
#50275=CARTESIAN_POINT('Origin',(-2.44320081404336,58.715,0.889252372646739));
#50276=CARTESIAN_POINT('',(-2.44320081404336,58.565,0.889252372646739));
#50277=CARTESIAN_POINT('Ctrl Pts',(-2.44320081404336,58.565,0.889252372646739));
#50278=CARTESIAN_POINT('Ctrl Pts',(-2.50263272292248,58.4923524443614,0.938371787843588));
#50279=CARTESIAN_POINT('Ctrl Pts',(-2.56549339577475,58.415,0.990325015455111));
#50280=CARTESIAN_POINT('',(-2.44320081404336,56.315,0.889252372646739));
#50281=CARTESIAN_POINT('',(-2.44320081404336,58.715,0.889252372646739));
#50282=CARTESIAN_POINT('',(-2.44320081404336,56.315,0.889252372646739));
#50283=CARTESIAN_POINT('Origin',(-2.65463165372019,56.315,0.966206904895015));
#50284=CARTESIAN_POINT('',(-2.92078571632913,56.315,0.892810617817545));
#50285=CARTESIAN_POINT('Origin',(-2.92078571632913,58.715,0.892810617817545));
#50286=CARTESIAN_POINT('Ctrl Pts',(-2.60185060918886,58.415,0.890434392565552));
#50287=CARTESIAN_POINT('Ctrl Pts',(-2.52030164906805,58.4923524443611,0.889826812233457));
#50288=CARTESIAN_POINT('Ctrl Pts',(-2.44320081404336,58.565,0.889252372646739));
#50289=CARTESIAN_POINT('Origin',(-2.25166604983954,58.715,1.3));
#50290=CARTESIAN_POINT('',(-2.25166604983954,58.565,1.3));
#50291=CARTESIAN_POINT('Ctrl Pts',(-2.25166604983954,58.565,1.3));
#50292=CARTESIAN_POINT('Ctrl Pts',(-2.30166555754319,58.4923524443611,1.35869342358162));
#50293=CARTESIAN_POINT('Ctrl Pts',(-2.35454965222884,58.415,1.42077300621496));
#50294=CARTESIAN_POINT('',(-2.25166604983954,56.315,1.3));
#50295=CARTESIAN_POINT('',(-2.25166604983954,58.715,1.3));
#50296=CARTESIAN_POINT('',(-2.25166604983954,56.315,1.3));
#50297=CARTESIAN_POINT('Origin',(-2.44652176569104,56.315,1.4125));
#50298=CARTESIAN_POINT('',(-2.72137748154254,56.315,1.38643593539449));
#50299=CARTESIAN_POINT('Origin',(-2.72137748154254,58.715,1.38643593539449));
#50300=CARTESIAN_POINT('Ctrl Pts',(-2.40770034250776,58.415,1.32871331019451));
#50301=CARTESIAN_POINT('Ctrl Pts',(-2.32749579954805,58.4923524443612,1.31395413205725));
#50302=CARTESIAN_POINT('Ctrl Pts',(-2.25166604983954,58.565,1.3));
#50303=CARTESIAN_POINT('Origin',(-1.99171555210934,58.715,1.671247785185));
#50304=CARTESIAN_POINT('',(-1.99171555210934,58.565,1.671247785185));
#50305=CARTESIAN_POINT('Ctrl Pts',(-1.99171555210934,58.565,1.671247785185));
#50306=CARTESIAN_POINT('Ctrl Pts',(-2.03076344889688,58.4923524443608,1.73773184717629));
#50307=CARTESIAN_POINT('Ctrl Pts',(-2.07206410895956,58.415,1.8080515281268));
#50308=CARTESIAN_POINT('',(-1.99171555210934,56.315,1.671247785185));
#50309=CARTESIAN_POINT('',(-1.99171555210934,58.715,1.671247785185));
#50310=CARTESIAN_POINT('',(-1.99171555210934,56.315,1.671247785185));
#50311=CARTESIAN_POINT('Origin',(-2.16407555181111,56.315,1.81587499736447));
#50312=CARTESIAN_POINT('',(-2.43928156906273,56.315,1.83793509864491));
#50313=CARTESIAN_POINT('Origin',(-2.43928156906273,58.715,1.83793509864491));
#50314=CARTESIAN_POINT('Ctrl Pts',(-2.14039331927472,58.415,1.72661994625458));
#50315=CARTESIAN_POINT('Ctrl Pts',(-2.06397016792831,58.4923524443615,1.69815762047126));
#50316=CARTESIAN_POINT('Ctrl Pts',(-1.99171555210934,58.565,1.671247785185));
#50317=CARTESIAN_POINT('Origin',(-1.671247785185,58.715,1.99171555210934));
#50318=CARTESIAN_POINT('',(-1.671247785185,58.565,1.99171555210934));
#50319=CARTESIAN_POINT('Ctrl Pts',(-1.671247785185,58.565,1.99171555210934));
#50320=CARTESIAN_POINT('Ctrl Pts',(-1.69815762047144,58.492352444361,2.06397016792879));
#50321=CARTESIAN_POINT('Ctrl Pts',(-1.72661994625458,58.415,2.14039331927472));
#50322=CARTESIAN_POINT('',(-1.671247785185,56.315,1.99171555210934));
#50323=CARTESIAN_POINT('',(-1.671247785185,58.715,1.99171555210934));
#50324=CARTESIAN_POINT('',(-1.671247785185,56.315,1.99171555210934));
#50325=CARTESIAN_POINT('Origin',(-1.81587499736447,56.315,2.16407555181111));
#50326=CARTESIAN_POINT('',(-2.08306932044298,56.315,2.23358953396304));
#50327=CARTESIAN_POINT('Origin',(-2.08306932044298,58.715,2.23358953396304));
#50328=CARTESIAN_POINT('Ctrl Pts',(-1.8080515281268,58.415,2.07206410895956));
#50329=CARTESIAN_POINT('Ctrl Pts',(-1.73773184717619,58.4923524443609,2.03076344889682));
#50330=CARTESIAN_POINT('Ctrl Pts',(-1.671247785185,58.565,1.99171555210934));
#50331=CARTESIAN_POINT('Origin',(-1.3,58.715,2.25166604983954));
#50332=CARTESIAN_POINT('',(-1.3,58.565,2.25166604983954));
#50333=CARTESIAN_POINT('Ctrl Pts',(-1.3,58.565,2.25166604983954));
#50334=CARTESIAN_POINT('Ctrl Pts',(-1.31395413205728,58.4923524443611,2.32749579954818));
#50335=CARTESIAN_POINT('Ctrl Pts',(-1.32871331019451,58.415,2.40770034250776));
#50336=CARTESIAN_POINT('',(-1.3,56.315,2.25166604983954));
#50337=CARTESIAN_POINT('',(-1.3,58.715,2.25166604983954));
#50338=CARTESIAN_POINT('',(-1.3,56.315,2.25166604983954));
#50339=CARTESIAN_POINT('Origin',(-1.4125,56.315,2.44652176569104));
#50340=CARTESIAN_POINT('',(-1.66356406460551,56.315,2.56137748154254));
#50341=CARTESIAN_POINT('Origin',(-1.66356406460551,58.715,2.56137748154254));
#50342=CARTESIAN_POINT('Ctrl Pts',(-1.42077300621496,58.415,2.35454965222884));
#50343=CARTESIAN_POINT('Ctrl Pts',(-1.35869342358169,58.492352444361,2.30166555754325));
#50344=CARTESIAN_POINT('Ctrl Pts',(-1.3,58.565,2.25166604983954));
#50345=CARTESIAN_POINT('Origin',(-0.889252372646739,58.715,2.44320081404336));
#50346=CARTESIAN_POINT('',(-0.889252372646739,58.565,2.44320081404336));
#50347=CARTESIAN_POINT('Ctrl Pts',(-0.889252372646739,58.565,2.44320081404336));
#50348=CARTESIAN_POINT('Ctrl Pts',(-0.889826812233454,58.4923524443614,
2.52030164906776));
#50349=CARTESIAN_POINT('Ctrl Pts',(-0.890434392565551,58.415,2.60185060918886));
#50350=CARTESIAN_POINT('',(-0.889252372646739,56.315,2.44320081404336));
#50351=CARTESIAN_POINT('',(-0.889252372646739,58.715,2.44320081404336));
#50352=CARTESIAN_POINT('',(-0.889252372646739,56.315,2.44320081404336));
#50353=CARTESIAN_POINT('Origin',(-0.966206904895014,56.315,2.65463165372019));
#50354=CARTESIAN_POINT('',(-1.19351225646904,56.315,2.81133927046491));
#50355=CARTESIAN_POINT('Origin',(-1.19351225646904,58.715,2.81133927046491));
#50356=CARTESIAN_POINT('Ctrl Pts',(-0.99032501545511,58.415,2.56549339577475));
#50357=CARTESIAN_POINT('Ctrl Pts',(-0.938371787843834,58.492352444361,2.50263272292277));
#50358=CARTESIAN_POINT('Ctrl Pts',(-0.889252372646739,58.565,2.44320081404336));
#50359=CARTESIAN_POINT('Origin',(-0.451485261934019,58.715,2.56050015783174));
#50360=CARTESIAN_POINT('',(-0.451485261934019,58.565,2.56050015783174));
#50361=CARTESIAN_POINT('Ctrl Pts',(-0.451485261934019,58.565,2.56050015783174));
#50362=CARTESIAN_POINT('Ctrl Pts',(-0.438662554993981,58.4923524443609,
2.63652940831541));
#50363=CARTESIAN_POINT('Ctrl Pts',(-0.425100076500032,58.415,2.71694496170969));
#50364=CARTESIAN_POINT('',(-0.451485261934019,56.315,2.56050015783174));
#50365=CARTESIAN_POINT('',(-0.451485261934019,58.715,2.56050015783174));
#50366=CARTESIAN_POINT('',(-0.451485261934019,56.315,2.56050015783174));
#50367=CARTESIAN_POINT('Origin',(-0.490556101909078,56.315,2.78208190225949));
#50368=CARTESIAN_POINT('',(-0.687196182366091,56.315,2.97587993826053));
#50369=CARTESIAN_POINT('Origin',(-0.687196182366091,58.715,2.97587993826053));
#50370=CARTESIAN_POINT('Ctrl Pts',(-0.529786500229298,58.415,2.69848592069235));
#50371=CARTESIAN_POINT('Ctrl Pts',(-0.489538200171253,58.4923524443612,
2.62755865940935));
#50372=CARTESIAN_POINT('Ctrl Pts',(-0.451485261934019,58.565,2.56050015783174));
#50373=CARTESIAN_POINT('Origin',(1.59204083889156E-16,58.715,2.6));
#50374=CARTESIAN_POINT('',(1.59204083889156E-16,58.565,2.6));
#50375=CARTESIAN_POINT('Ctrl Pts',(1.59204083889156E-16,58.565,2.6));
#50376=CARTESIAN_POINT('Ctrl Pts',(0.0258302420049794,58.492352444361,2.67264755563901));
#50377=CARTESIAN_POINT('Ctrl Pts',(0.0531506902789217,58.415,2.74948631640947));
#50378=CARTESIAN_POINT('',(1.59204083889156E-16,56.315,2.6));
#50379=CARTESIAN_POINT('',(1.59204083889156E-16,58.715,2.6));
#50380=CARTESIAN_POINT('',(1.59204083889156E-16,56.315,2.6));
#50381=CARTESIAN_POINT('Origin',(1.72981360379564E-16,56.315,2.825));
#50382=CARTESIAN_POINT('',(-0.16,56.315,3.05));
#50383=CARTESIAN_POINT('Origin',(-0.16,58.715,3.05));
#50384=CARTESIAN_POINT('Ctrl Pts',(-0.0531506902789213,58.415,2.74948631640947));
#50385=CARTESIAN_POINT('Ctrl Pts',(-0.0258302420049886,58.492352444361,
2.67264755563903));
#50386=CARTESIAN_POINT('Ctrl Pts',(1.59204083889156E-16,58.565,2.6));
#50387=CARTESIAN_POINT('Origin',(0.451485261934019,58.715,2.56050015783174));
#50388=CARTESIAN_POINT('',(0.451485261934019,58.565,2.56050015783174));
#50389=CARTESIAN_POINT('Ctrl Pts',(0.451485261934019,58.565,2.56050015783174));
#50390=CARTESIAN_POINT('Ctrl Pts',(0.489538200171364,58.492352444361,2.62755865940954));
#50391=CARTESIAN_POINT('Ctrl Pts',(0.529786500229298,58.415,2.69848592069235));
#50392=CARTESIAN_POINT('',(0.451485261934019,56.315,2.56050015783174));
#50393=CARTESIAN_POINT('',(0.451485261934019,58.715,2.56050015783174));
#50394=CARTESIAN_POINT('',(0.451485261934019,56.315,2.56050015783174));
#50395=CARTESIAN_POINT('Origin',(0.490556101909078,56.315,2.78208190225949));
#50396=CARTESIAN_POINT('',(0.372057701402184,56.315,3.03144735511394));
#50397=CARTESIAN_POINT('Origin',(0.372057701402184,58.715,3.03144735511394));
#50398=CARTESIAN_POINT('Ctrl Pts',(0.425100076500033,58.415,2.71694496170969));
#50399=CARTESIAN_POINT('Ctrl Pts',(0.438662554994009,58.492352444361,2.63652940831525));
#50400=CARTESIAN_POINT('Ctrl Pts',(0.451485261934019,58.565,2.56050015783174));
#50401=CARTESIAN_POINT('Origin',(0.889252372646739,58.715,2.44320081404336));
#50402=CARTESIAN_POINT('',(0.889252372646739,58.565,2.44320081404336));
#50403=CARTESIAN_POINT('Ctrl Pts',(0.889252372646739,58.565,2.44320081404336));
#50404=CARTESIAN_POINT('Ctrl Pts',(0.938371787844005,58.4923524443608,2.50263272292298));
#50405=CARTESIAN_POINT('Ctrl Pts',(0.990325015455111,58.415,2.56549339577475));
#50406=CARTESIAN_POINT('',(0.889252372646739,56.315,2.44320081404336));
#50407=CARTESIAN_POINT('',(0.889252372646739,58.715,2.44320081404336));
#50408=CARTESIAN_POINT('',(0.889252372646739,56.315,2.44320081404336));
#50409=CARTESIAN_POINT('Origin',(0.966206904895014,56.315,2.65463165372019));
#50410=CARTESIAN_POINT('',(0.892810617817545,56.315,2.92078571632913));
#50411=CARTESIAN_POINT('Origin',(0.892810617817545,58.715,2.92078571632913));
#50412=CARTESIAN_POINT('Ctrl Pts',(0.890434392565551,58.415,2.60185060918886));
#50413=CARTESIAN_POINT('Ctrl Pts',(0.889826812233459,58.4923524443609,2.52030164906829));
#50414=CARTESIAN_POINT('Ctrl Pts',(0.889252372646739,58.565,2.44320081404336));
#50415=CARTESIAN_POINT('Origin',(1.3,58.715,2.25166604983954));
#50416=CARTESIAN_POINT('',(1.3,58.565,2.25166604983954));
#50417=CARTESIAN_POINT('Ctrl Pts',(1.3,58.565,2.25166604983954));
#50418=CARTESIAN_POINT('Ctrl Pts',(1.35869342358162,58.4923524443611,2.30166555754319));
#50419=CARTESIAN_POINT('Ctrl Pts',(1.42077300621496,58.415,2.35454965222884));
#50420=CARTESIAN_POINT('',(1.3,56.315,2.25166604983954));
#50421=CARTESIAN_POINT('',(1.3,58.715,2.25166604983954));
#50422=CARTESIAN_POINT('',(1.3,56.315,2.25166604983954));
#50423=CARTESIAN_POINT('Origin',(1.4125,56.315,2.44652176569104));
#50424=CARTESIAN_POINT('',(1.38643593539449,56.315,2.72137748154254));
#50425=CARTESIAN_POINT('Origin',(1.38643593539449,58.715,2.72137748154254));
#50426=CARTESIAN_POINT('Ctrl Pts',(1.32871331019451,58.415,2.40770034250776));
#50427=CARTESIAN_POINT('Ctrl Pts',(1.31395413205722,58.4923524443614,2.32749579954787));
#50428=CARTESIAN_POINT('Ctrl Pts',(1.3,58.565,2.25166604983954));
#50429=CARTESIAN_POINT('Origin',(1.671247785185,58.715,1.99171555210934));
#50430=CARTESIAN_POINT('',(1.671247785185,58.565,1.99171555210934));
#50431=CARTESIAN_POINT('Ctrl Pts',(1.671247785185,58.565,1.99171555210934));
#50432=CARTESIAN_POINT('Ctrl Pts',(1.73773184717615,58.4923524443609,2.0307634488968));
#50433=CARTESIAN_POINT('Ctrl Pts',(1.8080515281268,58.415,2.07206410895956));
#50434=CARTESIAN_POINT('',(1.671247785185,56.315,1.99171555210934));
#50435=CARTESIAN_POINT('',(1.671247785185,58.715,1.99171555210934));
#50436=CARTESIAN_POINT('',(1.671247785185,56.315,1.99171555210934));
#50437=CARTESIAN_POINT('Origin',(1.81587499736447,56.315,2.16407555181111));
#50438=CARTESIAN_POINT('',(1.83793509864491,56.315,2.43928156906273));
#50439=CARTESIAN_POINT('Origin',(1.83793509864491,58.715,2.43928156906273));
#50440=CARTESIAN_POINT('Ctrl Pts',(1.72661994625458,58.415,2.14039331927472));
#50441=CARTESIAN_POINT('Ctrl Pts',(1.69815762047144,58.492352444361,2.06397016792879));
#50442=CARTESIAN_POINT('Ctrl Pts',(1.671247785185,58.565,1.99171555210934));
#50443=CARTESIAN_POINT('Origin',(1.99171555210934,58.715,1.671247785185));
#50444=CARTESIAN_POINT('',(1.99171555210934,58.565,1.671247785185));
#50445=CARTESIAN_POINT('Ctrl Pts',(1.99171555210934,58.565,1.671247785185));
#50446=CARTESIAN_POINT('Ctrl Pts',(2.06397016792865,58.4923524443611,1.69815762047139));
#50447=CARTESIAN_POINT('Ctrl Pts',(2.14039331927472,58.415,1.72661994625458));
#50448=CARTESIAN_POINT('',(1.99171555210934,56.315,1.671247785185));
#50449=CARTESIAN_POINT('',(1.99171555210934,58.715,1.671247785185));
#50450=CARTESIAN_POINT('',(1.99171555210934,56.315,1.671247785185));
#50451=CARTESIAN_POINT('Origin',(2.16407555181111,56.315,1.81587499736447));
#50452=CARTESIAN_POINT('',(2.23358953396304,56.315,2.08306932044298));
#50453=CARTESIAN_POINT('Origin',(2.23358953396304,58.715,2.08306932044298));
#50454=CARTESIAN_POINT('Ctrl Pts',(2.07206410895956,58.415,1.8080515281268));
#50455=CARTESIAN_POINT('Ctrl Pts',(2.03076344889677,58.492352444361,1.73773184717609));
#50456=CARTESIAN_POINT('Ctrl Pts',(1.99171555210934,58.565,1.671247785185));
#50457=CARTESIAN_POINT('Origin',(2.25166604983954,58.715,1.3));
#50458=CARTESIAN_POINT('',(2.25166604983954,58.565,1.3));
#50459=CARTESIAN_POINT('Ctrl Pts',(2.25166604983954,58.565,1.3));
#50460=CARTESIAN_POINT('Ctrl Pts',(2.32749579954822,58.492352444361,1.31395413205728));
#50461=CARTESIAN_POINT('Ctrl Pts',(2.40770034250776,58.415,1.32871331019451));
#50462=CARTESIAN_POINT('',(2.25166604983954,56.315,1.3));
#50463=CARTESIAN_POINT('',(2.25166604983954,58.715,1.3));
#50464=CARTESIAN_POINT('',(2.25166604983954,56.315,1.3));
#50465=CARTESIAN_POINT('Origin',(2.44652176569104,56.315,1.4125));
#50466=CARTESIAN_POINT('',(2.56137748154254,56.315,1.66356406460551));
#50467=CARTESIAN_POINT('Origin',(2.56137748154254,58.715,1.66356406460551));
#50468=CARTESIAN_POINT('Ctrl Pts',(2.35454965222884,58.415,1.42077300621496));
#50469=CARTESIAN_POINT('Ctrl Pts',(2.30166555754331,58.4923524443609,1.35869342358176));
#50470=CARTESIAN_POINT('Ctrl Pts',(2.25166604983954,58.565,1.3));
#50471=CARTESIAN_POINT('Origin',(2.44320081404336,58.715,0.889252372646739));
#50472=CARTESIAN_POINT('',(2.44320081404336,58.565,0.889252372646739));
#50473=CARTESIAN_POINT('Ctrl Pts',(2.44320081404336,58.565,0.889252372646739));
#50474=CARTESIAN_POINT('Ctrl Pts',(2.52030164906804,58.4923524443611,0.889826812233456));
#50475=CARTESIAN_POINT('Ctrl Pts',(2.60185060918886,58.415,0.890434392565551));
#50476=CARTESIAN_POINT('',(2.44320081404336,56.315,0.889252372646739));
#50477=CARTESIAN_POINT('',(2.44320081404336,58.715,0.889252372646739));
#50478=CARTESIAN_POINT('',(2.44320081404336,56.315,0.889252372646739));
#50479=CARTESIAN_POINT('Origin',(2.65463165372019,56.315,0.966206904895014));
#50480=CARTESIAN_POINT('',(2.81133927046491,56.315,1.19351225646904));
#50481=CARTESIAN_POINT('Origin',(2.81133927046491,58.715,1.19351225646904));
#50482=CARTESIAN_POINT('Ctrl Pts',(2.56549339577475,58.415,0.99032501545511));
#50483=CARTESIAN_POINT('Ctrl Pts',(2.50263272292278,58.492352444361,0.93837178784384));
#50484=CARTESIAN_POINT('Ctrl Pts',(2.44320081404336,58.565,0.889252372646739));
#50485=CARTESIAN_POINT('Origin',(2.56050015783174,58.715,0.451485261934019));
#50486=CARTESIAN_POINT('',(2.56050015783174,58.565,0.451485261934019));
#50487=CARTESIAN_POINT('Ctrl Pts',(2.56050015783174,58.565,0.451485261934019));
#50488=CARTESIAN_POINT('Ctrl Pts',(2.63652940831479,58.4923524443615,0.438662554994086));
#50489=CARTESIAN_POINT('Ctrl Pts',(2.71694496170969,58.415,0.425100076500033));
#50490=CARTESIAN_POINT('',(2.56050015783174,56.315,0.451485261934019));
#50491=CARTESIAN_POINT('',(2.56050015783174,58.715,0.451485261934019));
#50492=CARTESIAN_POINT('',(2.56050015783174,56.315,0.451485261934019));
#50493=CARTESIAN_POINT('Origin',(2.78208190225949,56.315,0.490556101909078));
#50494=CARTESIAN_POINT('',(2.97587993826053,56.315,0.687196182366091));
#50495=CARTESIAN_POINT('Origin',(2.97587993826053,58.715,0.687196182366091));
#50496=CARTESIAN_POINT('Ctrl Pts',(2.69848592069235,58.415,0.529786500229298));
#50497=CARTESIAN_POINT('Ctrl Pts',(2.62755865940969,58.4923524443609,0.489538200171446));
#50498=CARTESIAN_POINT('Ctrl Pts',(2.56050015783174,58.565,0.451485261934019));
#50499=CARTESIAN_POINT('Origin',(2.6,58.715,0.));
#50500=CARTESIAN_POINT('',(2.6,58.565,0.));
#50501=CARTESIAN_POINT('Ctrl Pts',(2.6,58.565,0.));
#50502=CARTESIAN_POINT('Ctrl Pts',(2.67264755563906,58.4923524443609,-0.0258302420049978));
#50503=CARTESIAN_POINT('Ctrl Pts',(2.74948631640947,58.415,-0.0531506902789213));
#50504=CARTESIAN_POINT('',(2.6,56.315,0.));
#50505=CARTESIAN_POINT('',(2.6,58.715,0.));
#50506=CARTESIAN_POINT('',(2.6,56.315,0.));
#50507=CARTESIAN_POINT('Origin',(2.825,56.315,0.));
#50508=CARTESIAN_POINT('',(3.05,56.315,0.16));
#50509=CARTESIAN_POINT('Origin',(3.05,58.715,0.16));
#50510=CARTESIAN_POINT('Ctrl Pts',(2.74948631640947,58.415,0.0531506902789213));
#50511=CARTESIAN_POINT('Ctrl Pts',(2.67264755563908,58.4923524443609,0.0258302420050066));
#50512=CARTESIAN_POINT('Ctrl Pts',(2.6,58.565,0.));
#50513=CARTESIAN_POINT('Origin',(0.,55.915,0.));
#50514=CARTESIAN_POINT('Origin',(-3.12284933782575E-16,55.915,-2.55));
#50515=CARTESIAN_POINT('Origin',(0.,58.565,0.));
#50516=CARTESIAN_POINT('',(-2.45,58.715,-3.00038465791102E-16));
#50517=CARTESIAN_POINT('',(-2.6,58.565,-3.18408167778312E-16));
#50518=CARTESIAN_POINT('Origin',(0.,58.715,0.));
#50519=CARTESIAN_POINT('Origin',(0.,58.715,0.));
#50520=CARTESIAN_POINT('',(-1.59337567297407,58.715,-1.95132241774696E-16));
#50521=CARTESIAN_POINT('Origin',(0.,58.715,0.));
#50522=CARTESIAN_POINT('Origin',(0.,58.615,0.));
#50523=CARTESIAN_POINT('',(-1.39034491479519,58.515,-0.0918519675297062));
#50524=CARTESIAN_POINT('',(-1.44337567297406,58.565,1.76762539787484E-16));
#50525=CARTESIAN_POINT('Ctrl Pts',(-1.39034491479519,58.515,-0.0918519675297066));
#50526=CARTESIAN_POINT('Ctrl Pts',(-1.41639293922685,58.5380172662528,-0.0467354657772785));
#50527=CARTESIAN_POINT('Ctrl Pts',(-1.44337567297406,58.565,1.76762539787484E-16));
#50528=CARTESIAN_POINT('',(-0.774718594665906,58.515,-1.15814803247029));
#50529=CARTESIAN_POINT('Origin',(0.,58.515,0.));
#50530=CARTESIAN_POINT('',(-0.721687836487033,58.565,-1.25));
#50531=CARTESIAN_POINT('Ctrl Pts',(-0.721687836487033,58.565,-1.25));
#50532=CARTESIAN_POINT('Ctrl Pts',(-0.748670570234245,58.5380172662528,
-1.20326453422273));
#50533=CARTESIAN_POINT('Ctrl Pts',(-0.774718594665906,58.515,-1.15814803247029));
#50534=CARTESIAN_POINT('',(-0.615626320129288,58.515,-1.25));
#50535=CARTESIAN_POINT('Ctrl Pts',(-0.615626320129287,58.515,-1.25));
#50536=CARTESIAN_POINT('Ctrl Pts',(-0.667722368992606,58.5380172662528,
-1.25));
#50537=CARTESIAN_POINT('Ctrl Pts',(-0.721687836487033,58.565,-1.25));
#50538=CARTESIAN_POINT('',(0.615626320129287,58.515,-1.25));
#50539=CARTESIAN_POINT('Origin',(0.,58.515,0.));
#50540=CARTESIAN_POINT('',(0.721687836487032,58.565,-1.25));
#50541=CARTESIAN_POINT('Ctrl Pts',(0.721687836487032,58.565,-1.25));
#50542=CARTESIAN_POINT('Ctrl Pts',(0.667722368992606,58.5380172662528,-1.25));
#50543=CARTESIAN_POINT('Ctrl Pts',(0.615626320129287,58.515,-1.25));
#50544=CARTESIAN_POINT('',(0.774718594665905,58.515,-1.15814803247029));
#50545=CARTESIAN_POINT('Ctrl Pts',(0.774718594665906,58.515,-1.15814803247029));
#50546=CARTESIAN_POINT('Ctrl Pts',(0.748670570234245,58.5380172662528,-1.20326453422273));
#50547=CARTESIAN_POINT('Ctrl Pts',(0.721687836487032,58.565,-1.25));
#50548=CARTESIAN_POINT('',(1.39034491479519,58.515,-0.0918519675297066));
#50549=CARTESIAN_POINT('Origin',(0.,58.515,0.));
#50550=CARTESIAN_POINT('',(1.44337567297406,58.565,0.));
#50551=CARTESIAN_POINT('Ctrl Pts',(1.44337567297406,58.565,0.));
#50552=CARTESIAN_POINT('Ctrl Pts',(1.41639293922685,58.5380172662528,-0.0467354657772708));
#50553=CARTESIAN_POINT('Ctrl Pts',(1.39034491479519,58.515,-0.0918519675297073));
#50554=CARTESIAN_POINT('',(1.39034491479519,58.515,0.0918519675297068));
#50555=CARTESIAN_POINT('Ctrl Pts',(1.39034491479519,58.515,0.0918519675297077));
#50556=CARTESIAN_POINT('Ctrl Pts',(1.41639293922685,58.5380172662528,0.0467354657772747));
#50557=CARTESIAN_POINT('Ctrl Pts',(1.44337567297406,58.565,0.));
#50558=CARTESIAN_POINT('',(0.774718594665905,58.515,1.15814803247029));
#50559=CARTESIAN_POINT('Origin',(0.,58.515,0.));
#50560=CARTESIAN_POINT('',(0.721687836487032,58.565,1.25));
#50561=CARTESIAN_POINT('Ctrl Pts',(0.721687836487032,58.565,1.25));
#50562=CARTESIAN_POINT('Ctrl Pts',(0.748670570234242,58.5380172662528,1.20326453422273));
#50563=CARTESIAN_POINT('Ctrl Pts',(0.774718594665906,58.515,1.15814803247029));
#50564=CARTESIAN_POINT('',(0.615626320129287,58.515,1.25));
#50565=CARTESIAN_POINT('Ctrl Pts',(0.615626320129287,58.515,1.25));
#50566=CARTESIAN_POINT('Ctrl Pts',(0.667722368992607,58.5380172662528,1.25));
#50567=CARTESIAN_POINT('Ctrl Pts',(0.721687836487032,58.565,1.25));
#50568=CARTESIAN_POINT('',(-0.615626320129287,58.515,1.25));
#50569=CARTESIAN_POINT('Origin',(0.,58.515,0.));
#50570=CARTESIAN_POINT('',(-0.721687836487032,58.565,1.25));
#50571=CARTESIAN_POINT('Ctrl Pts',(-0.721687836487032,58.565,1.25));
#50572=CARTESIAN_POINT('Ctrl Pts',(-0.667722368992609,58.5380172662528,
1.25));
#50573=CARTESIAN_POINT('Ctrl Pts',(-0.615626320129286,58.515,1.25));
#50574=CARTESIAN_POINT('',(-0.774718594665904,58.515,1.15814803247029));
#50575=CARTESIAN_POINT('Ctrl Pts',(-0.774718594665905,58.515,1.15814803247029));
#50576=CARTESIAN_POINT('Ctrl Pts',(-0.748670570234242,58.5380172662528,
1.20326453422273));
#50577=CARTESIAN_POINT('Ctrl Pts',(-0.721687836487032,58.565,1.25));
#50578=CARTESIAN_POINT('',(-1.39034491479519,58.515,0.0918519675297067));
#50579=CARTESIAN_POINT('Origin',(0.,58.515,0.));
#50580=CARTESIAN_POINT('Ctrl Pts',(-1.44337567297406,58.565,1.76762539787484E-16));
#50581=CARTESIAN_POINT('Ctrl Pts',(-1.41639293922685,58.5380172662528,0.0467354657772748));
#50582=CARTESIAN_POINT('Ctrl Pts',(-1.39034491479519,58.515,0.0918519675297071));
#50583=CARTESIAN_POINT('',(-1.49337567297406,58.615,1.82885773783221E-16));
#50584=CARTESIAN_POINT('Origin',(0.,58.615,0.));
#50585=CARTESIAN_POINT('',(0.615626320129287,58.715,-1.25));
#50586=CARTESIAN_POINT('',(0.615626320129287,58.615,-1.25));
#50587=CARTESIAN_POINT('',(-0.615626320129288,58.715,-1.25));
#50588=CARTESIAN_POINT('',(-0.615626320129288,58.615,-1.25));
#50589=CARTESIAN_POINT('Origin',(0.,58.715,0.));
#50590=CARTESIAN_POINT('Origin',(0.,58.615,0.));
#50591=CARTESIAN_POINT('',(1.39034491479519,58.715,-0.0918519675297066));
#50592=CARTESIAN_POINT('',(1.39034491479519,58.615,-0.0918519675297066));
#50593=CARTESIAN_POINT('',(0.774718594665905,58.715,-1.15814803247029));
#50594=CARTESIAN_POINT('',(0.774718594665905,58.615,-1.15814803247029));
#50595=CARTESIAN_POINT('Origin',(0.,58.715,0.));
#50596=CARTESIAN_POINT('Origin',(0.,58.615,0.));
#50597=CARTESIAN_POINT('',(-1.39034491479519,58.715,-0.0918519675297062));
#50598=CARTESIAN_POINT('',(-1.39034491479519,58.615,-0.0918519675297062));
#50599=CARTESIAN_POINT('',(-0.774718594665906,58.715,-1.15814803247029));
#50600=CARTESIAN_POINT('Origin',(0.,58.715,0.));
#50601=CARTESIAN_POINT('',(-0.774718594665906,58.615,-1.15814803247029));
#50602=CARTESIAN_POINT('Origin',(0.,58.615,0.));
#50603=CARTESIAN_POINT('',(0.774718594665905,58.715,1.15814803247029));
#50604=CARTESIAN_POINT('',(0.774718594665905,58.615,1.15814803247029));
#50605=CARTESIAN_POINT('',(1.39034491479519,58.715,0.0918519675297068));
#50606=CARTESIAN_POINT('',(1.39034491479519,58.615,0.0918519675297068));
#50607=CARTESIAN_POINT('Origin',(0.,58.715,0.));
#50608=CARTESIAN_POINT('Origin',(0.,58.615,0.));
#50609=CARTESIAN_POINT('',(-0.774718594665904,58.715,1.15814803247029));
#50610=CARTESIAN_POINT('',(-0.774718594665904,58.615,1.15814803247029));
#50611=CARTESIAN_POINT('',(-1.39034491479519,58.715,0.0918519675297067));
#50612=CARTESIAN_POINT('Origin',(0.,58.715,0.));
#50613=CARTESIAN_POINT('',(-1.39034491479519,58.615,0.0918519675297067));
#50614=CARTESIAN_POINT('Origin',(0.,58.615,0.));
#50615=CARTESIAN_POINT('',(0.615626320129287,58.715,1.25));
#50616=CARTESIAN_POINT('',(0.615626320129287,58.615,1.25));
#50617=CARTESIAN_POINT('',(-0.615626320129287,58.715,1.25));
#50618=CARTESIAN_POINT('Origin',(0.,58.715,0.));
#50619=CARTESIAN_POINT('',(-0.615626320129287,58.615,1.25));
#50620=CARTESIAN_POINT('Origin',(1.44337567297406,58.715,0.));
#50621=CARTESIAN_POINT('',(1.26295371385231,58.715,0.3125));
#50622=CARTESIAN_POINT('',(1.44337567297406,57.415,0.));
#50623=CARTESIAN_POINT('',(1.44337567297406,58.715,0.));
#50624=CARTESIAN_POINT('',(0.721687836487032,57.415,1.25));
#50625=CARTESIAN_POINT('',(1.44337567297406,57.415,0.));
#50626=CARTESIAN_POINT('',(0.721687836487032,58.715,1.25));
#50627=CARTESIAN_POINT('Origin',(0.721687836487032,58.715,-1.25));
#50628=CARTESIAN_POINT('',(0.902109795608791,58.715,-0.9375));
#50629=CARTESIAN_POINT('',(0.721687836487032,57.415,-1.25));
#50630=CARTESIAN_POINT('',(0.721687836487032,58.715,-1.25));
#50631=CARTESIAN_POINT('',(0.721687836487032,57.415,-1.25));
#50632=CARTESIAN_POINT('Origin',(-0.721687836487033,58.715,-1.25));
#50633=CARTESIAN_POINT('',(-0.360843918243517,58.715,-1.25));
#50634=CARTESIAN_POINT('',(-0.721687836487033,57.415,-1.25));
#50635=CARTESIAN_POINT('',(-0.721687836487033,58.715,-1.25));
#50636=CARTESIAN_POINT('',(-0.721687836487033,57.415,-1.25));
#50637=CARTESIAN_POINT('Origin',(0.,58.715,0.));
#50638=CARTESIAN_POINT('Origin',(0.,58.715,0.));
#50639=CARTESIAN_POINT('Origin',(0.,58.715,0.));
#50640=CARTESIAN_POINT('',(-1.26295371385231,58.715,-0.3125));
#50641=CARTESIAN_POINT('Origin',(0.,58.715,0.));
#50642=CARTESIAN_POINT('Origin',(0.,58.715,0.));
#50643=CARTESIAN_POINT('',(-0.90210979560879,58.715,0.9375));
#50644=CARTESIAN_POINT('Origin',(0.,58.715,0.));
#50645=CARTESIAN_POINT('',(0.360843918243516,58.715,1.25));
#50646=CARTESIAN_POINT('Origin',(1.44337567297406,57.415,0.));
#50647=CARTESIAN_POINT('',(-1.44337567297406,57.415,1.38777878078145E-16));
#50648=CARTESIAN_POINT('',(-1.44337567297406,57.415,1.76762539787484E-16));
#50649=CARTESIAN_POINT('Origin',(0.,57.415,0.));
#50650=CARTESIAN_POINT('Origin',(1.44337567297406,57.415,0.));
#50651=CARTESIAN_POINT('Origin',(0.,57.415,0.));
#50652=CARTESIAN_POINT('Origin',(1.44337567297406,57.415,0.));
#50653=CARTESIAN_POINT('Origin',(0.,57.415,0.));
#50654=CARTESIAN_POINT('Origin',(1.44337567297406,57.415,0.));
#50655=CARTESIAN_POINT('Origin',(0.,57.415,0.));
#50656=CARTESIAN_POINT('Origin',(1.44337567297406,57.415,0.));
#50657=CARTESIAN_POINT('',(-0.721687836487032,57.415,1.25));
#50658=CARTESIAN_POINT('',(0.721687836487032,57.415,1.25));
#50659=CARTESIAN_POINT('Origin',(0.,57.415,0.));
#50660=CARTESIAN_POINT('Origin',(1.44337567297406,57.415,0.));
#50661=CARTESIAN_POINT('',(-0.721687836487032,57.415,1.25));
#50662=CARTESIAN_POINT('Origin',(0.,57.415,0.));
#50663=CARTESIAN_POINT('Origin',(0.,57.415,0.));
#50664=CARTESIAN_POINT('',(0.,56.5477323996475,0.));
#50665=CARTESIAN_POINT('',(-1.44337567297406,57.415,1.76762539787484E-16));
#50666=CARTESIAN_POINT('Origin',(-1.44337567297406,58.715,1.76762539787484E-16));
#50667=CARTESIAN_POINT('',(-1.44337567297406,58.715,1.76762539787484E-16));
#50668=CARTESIAN_POINT('Origin',(-0.721687836487032,58.715,1.25));
#50669=CARTESIAN_POINT('',(-0.721687836487032,58.715,1.25));
#50670=CARTESIAN_POINT('Origin',(0.721687836487032,58.715,1.25));
#50671=CARTESIAN_POINT('',(0.,0.,0.));
#50672=CARTESIAN_POINT('Origin',(97.79,63.745,12.066));
#50673=CARTESIAN_POINT('',(96.012,63.645,12.066));
#50674=CARTESIAN_POINT('Origin',(97.79,63.645,12.066));
#50675=CARTESIAN_POINT('',(95.812,63.845,12.066));
#50676=CARTESIAN_POINT('',(95.912,63.745,12.066));
#50677=CARTESIAN_POINT('Origin',(97.79,63.845,12.066));
#50678=CARTESIAN_POINT('Origin',(0.,63.845,12.066));
#50679=CARTESIAN_POINT('',(97.79,63.845,16.5785));
#50680=CARTESIAN_POINT('',(-97.79,63.845,16.5785));
#50681=CARTESIAN_POINT('',(-48.895,63.845,16.5785));
#50682=CARTESIAN_POINT('',(97.79,63.845,7.5535));
#50683=CARTESIAN_POINT('Origin',(97.79,63.845,12.066));
#50684=CARTESIAN_POINT('',(-97.79,63.845,7.5535));
#50685=CARTESIAN_POINT('',(48.895,63.845,7.5535));
#50686=CARTESIAN_POINT('Origin',(-97.79,63.845,12.066));
#50687=CARTESIAN_POINT('',(76.254,63.845,12.066));
#50688=CARTESIAN_POINT('Origin',(78.232,63.845,12.066));
#50689=CARTESIAN_POINT('',(37.138,63.845,12.066));
#50690=CARTESIAN_POINT('Origin',(39.116,63.845,12.066));
#50691=CARTESIAN_POINT('',(-99.768,63.845,12.066));
#50692=CARTESIAN_POINT('Origin',(-97.79,63.845,12.066));
#50693=CARTESIAN_POINT('',(-31.315,63.845,12.066));
#50694=CARTESIAN_POINT('Origin',(-29.337,63.845,12.066));
#50695=CARTESIAN_POINT('',(-70.431,63.845,12.066));
#50696=CARTESIAN_POINT('Origin',(-68.453,63.845,12.066));
#50697=CARTESIAN_POINT('',(-80.21,63.845,12.066));
#50698=CARTESIAN_POINT('Origin',(-78.232,63.845,12.066));
#50699=CARTESIAN_POINT('',(-41.094,63.845,12.066));
#50700=CARTESIAN_POINT('Origin',(-39.116,63.845,12.066));
#50701=CARTESIAN_POINT('',(-1.978,63.845,12.066));
#50702=CARTESIAN_POINT('Origin',(0.,63.845,12.066));
#50703=CARTESIAN_POINT('',(27.359,63.845,12.066));
#50704=CARTESIAN_POINT('Origin',(29.337,63.845,12.066));
#50705=CARTESIAN_POINT('',(66.475,63.845,12.066));
#50706=CARTESIAN_POINT('Origin',(68.453,63.845,12.066));
#50707=CARTESIAN_POINT('',(86.033,63.845,12.066));
#50708=CARTESIAN_POINT('Origin',(88.011,63.845,12.066));
#50709=CARTESIAN_POINT('',(46.917,63.845,12.066));
#50710=CARTESIAN_POINT('Origin',(48.895,63.845,12.066));
#50711=CARTESIAN_POINT('',(7.801,63.845,12.066));
#50712=CARTESIAN_POINT('Origin',(9.779,63.845,12.066));
#50713=CARTESIAN_POINT('',(-21.536,63.845,12.066));
#50714=CARTESIAN_POINT('Origin',(-19.558,63.845,12.066));
#50715=CARTESIAN_POINT('',(-60.652,63.845,12.066));
#50716=CARTESIAN_POINT('Origin',(-58.674,63.845,12.066));
#50717=CARTESIAN_POINT('',(-89.989,63.845,12.066));
#50718=CARTESIAN_POINT('Origin',(-88.011,63.845,12.066));
#50719=CARTESIAN_POINT('',(-50.873,63.845,12.066));
#50720=CARTESIAN_POINT('Origin',(-48.895,63.845,12.066));
#50721=CARTESIAN_POINT('',(-11.757,63.845,12.066));
#50722=CARTESIAN_POINT('Origin',(-9.779,63.845,12.066));
#50723=CARTESIAN_POINT('',(17.58,63.845,12.066));
#50724=CARTESIAN_POINT('Origin',(19.558,63.845,12.066));
#50725=CARTESIAN_POINT('',(56.696,63.845,12.066));
#50726=CARTESIAN_POINT('Origin',(58.674,63.845,12.066));
#50727=CARTESIAN_POINT('Origin',(97.79,63.845,12.066));
#50728=CARTESIAN_POINT('',(96.012,57.495,12.066));
#50729=CARTESIAN_POINT('',(96.012,63.845,12.066));
#50730=CARTESIAN_POINT('Origin',(97.79,57.495,12.066));
#50731=CARTESIAN_POINT('Origin',(78.232,63.745,12.066));
#50732=CARTESIAN_POINT('',(76.454,63.645,12.066));
#50733=CARTESIAN_POINT('Origin',(78.232,63.645,12.066));
#50734=CARTESIAN_POINT('',(76.354,63.745,12.066));
#50735=CARTESIAN_POINT('Origin',(78.232,63.845,12.066));
#50736=CARTESIAN_POINT('',(76.454,57.495,12.066));
#50737=CARTESIAN_POINT('',(76.454,63.845,12.066));
#50738=CARTESIAN_POINT('Origin',(78.232,57.495,12.066));
#50739=CARTESIAN_POINT('Origin',(58.674,63.745,12.066));
#50740=CARTESIAN_POINT('',(56.896,63.645,12.066));
#50741=CARTESIAN_POINT('Origin',(58.674,63.645,12.066));
#50742=CARTESIAN_POINT('',(56.796,63.745,12.066));
#50743=CARTESIAN_POINT('Origin',(58.674,63.845,12.066));
#50744=CARTESIAN_POINT('',(56.896,57.495,12.066));
#50745=CARTESIAN_POINT('',(56.896,63.845,12.066));
#50746=CARTESIAN_POINT('Origin',(58.674,57.495,12.066));
#50747=CARTESIAN_POINT('Origin',(39.116,63.745,12.066));
#50748=CARTESIAN_POINT('',(37.338,63.645,12.066));
#50749=CARTESIAN_POINT('Origin',(39.116,63.645,12.066));
#50750=CARTESIAN_POINT('',(37.238,63.745,12.066));
#50751=CARTESIAN_POINT('Origin',(39.116,63.845,12.066));
#50752=CARTESIAN_POINT('',(37.338,57.495,12.066));
#50753=CARTESIAN_POINT('',(37.338,63.845,12.066));
#50754=CARTESIAN_POINT('Origin',(39.116,57.495,12.066));
#50755=CARTESIAN_POINT('Origin',(19.558,63.745,12.066));
#50756=CARTESIAN_POINT('',(17.78,63.645,12.066));
#50757=CARTESIAN_POINT('Origin',(19.558,63.645,12.066));
#50758=CARTESIAN_POINT('',(17.68,63.745,12.066));
#50759=CARTESIAN_POINT('Origin',(19.558,63.845,12.066));
#50760=CARTESIAN_POINT('',(17.78,57.495,12.066));
#50761=CARTESIAN_POINT('',(17.78,63.845,12.066));
#50762=CARTESIAN_POINT('Origin',(19.558,57.495,12.066));
#50763=CARTESIAN_POINT('Origin',(-97.79,63.745,12.066));
#50764=CARTESIAN_POINT('',(-99.568,63.645,12.066));
#50765=CARTESIAN_POINT('Origin',(-97.79,63.645,12.066));
#50766=CARTESIAN_POINT('',(-99.668,63.745,12.066));
#50767=CARTESIAN_POINT('Origin',(-97.79,63.845,12.066));
#50768=CARTESIAN_POINT('',(-99.568,57.495,12.066));
#50769=CARTESIAN_POINT('',(-99.568,63.845,12.066));
#50770=CARTESIAN_POINT('Origin',(-97.79,57.495,12.066));
#50771=CARTESIAN_POINT('Origin',(-9.779,63.745,12.066));
#50772=CARTESIAN_POINT('',(-11.557,63.645,12.066));
#50773=CARTESIAN_POINT('Origin',(-9.779,63.645,12.066));
#50774=CARTESIAN_POINT('',(-11.657,63.745,12.066));
#50775=CARTESIAN_POINT('Origin',(-9.779,63.845,12.066));
#50776=CARTESIAN_POINT('',(-11.557,57.495,12.066));
#50777=CARTESIAN_POINT('',(-11.557,63.845,12.066));
#50778=CARTESIAN_POINT('Origin',(-9.779,57.495,12.066));
#50779=CARTESIAN_POINT('Origin',(-29.337,63.745,12.066));
#50780=CARTESIAN_POINT('',(-31.115,63.645,12.066));
#50781=CARTESIAN_POINT('Origin',(-29.337,63.645,12.066));
#50782=CARTESIAN_POINT('',(-31.215,63.745,12.066));
#50783=CARTESIAN_POINT('Origin',(-29.337,63.845,12.066));
#50784=CARTESIAN_POINT('',(-31.115,57.495,12.066));
#50785=CARTESIAN_POINT('',(-31.115,63.845,12.066));
#50786=CARTESIAN_POINT('Origin',(-29.337,57.495,12.066));
#50787=CARTESIAN_POINT('Origin',(-48.895,63.745,12.066));
#50788=CARTESIAN_POINT('',(-50.673,63.645,12.066));
#50789=CARTESIAN_POINT('Origin',(-48.895,63.645,12.066));
#50790=CARTESIAN_POINT('',(-50.773,63.745,12.066));
#50791=CARTESIAN_POINT('Origin',(-48.895,63.845,12.066));
#50792=CARTESIAN_POINT('',(-50.673,57.495,12.066));
#50793=CARTESIAN_POINT('',(-50.673,63.845,12.066));
#50794=CARTESIAN_POINT('Origin',(-48.895,57.495,12.066));
#50795=CARTESIAN_POINT('Origin',(-68.453,63.745,12.066));
#50796=CARTESIAN_POINT('',(-70.231,63.645,12.066));
#50797=CARTESIAN_POINT('Origin',(-68.453,63.645,12.066));
#50798=CARTESIAN_POINT('',(-70.331,63.745,12.066));
#50799=CARTESIAN_POINT('Origin',(-68.453,63.845,12.066));
#50800=CARTESIAN_POINT('',(-70.231,57.495,12.066));
#50801=CARTESIAN_POINT('',(-70.231,63.845,12.066));
#50802=CARTESIAN_POINT('Origin',(-68.453,57.495,12.066));
#50803=CARTESIAN_POINT('Origin',(-88.011,63.745,12.066));
#50804=CARTESIAN_POINT('',(-89.789,63.645,12.066));
#50805=CARTESIAN_POINT('Origin',(-88.011,63.645,12.066));
#50806=CARTESIAN_POINT('',(-89.889,63.745,12.066));
#50807=CARTESIAN_POINT('Origin',(-88.011,63.845,12.066));
#50808=CARTESIAN_POINT('',(-89.789,57.495,12.066));
#50809=CARTESIAN_POINT('',(-89.789,63.845,12.066));
#50810=CARTESIAN_POINT('Origin',(-88.011,57.495,12.066));
#50811=CARTESIAN_POINT('Origin',(-78.232,63.745,12.066));
#50812=CARTESIAN_POINT('',(-80.01,63.645,12.066));
#50813=CARTESIAN_POINT('Origin',(-78.232,63.645,12.066));
#50814=CARTESIAN_POINT('',(-80.11,63.745,12.066));
#50815=CARTESIAN_POINT('Origin',(-78.232,63.845,12.066));
#50816=CARTESIAN_POINT('',(-80.01,57.495,12.066));
#50817=CARTESIAN_POINT('',(-80.01,63.845,12.066));
#50818=CARTESIAN_POINT('Origin',(-78.232,57.495,12.066));
#50819=CARTESIAN_POINT('Origin',(-58.674,63.745,12.066));
#50820=CARTESIAN_POINT('',(-60.452,63.645,12.066));
#50821=CARTESIAN_POINT('Origin',(-58.674,63.645,12.066));
#50822=CARTESIAN_POINT('',(-60.552,63.745,12.066));
#50823=CARTESIAN_POINT('Origin',(-58.674,63.845,12.066));
#50824=CARTESIAN_POINT('',(-60.452,57.495,12.066));
#50825=CARTESIAN_POINT('',(-60.452,63.845,12.066));
#50826=CARTESIAN_POINT('Origin',(-58.674,57.495,12.066));
#50827=CARTESIAN_POINT('Origin',(-39.116,63.745,12.066));
#50828=CARTESIAN_POINT('',(-40.894,63.645,12.066));
#50829=CARTESIAN_POINT('Origin',(-39.116,63.645,12.066));
#50830=CARTESIAN_POINT('',(-40.994,63.745,12.066));
#50831=CARTESIAN_POINT('Origin',(-39.116,63.845,12.066));
#50832=CARTESIAN_POINT('',(-40.894,57.495,12.066));
#50833=CARTESIAN_POINT('',(-40.894,63.845,12.066));
#50834=CARTESIAN_POINT('Origin',(-39.116,57.495,12.066));
#50835=CARTESIAN_POINT('Origin',(-19.558,63.745,12.066));
#50836=CARTESIAN_POINT('',(-21.336,63.645,12.066));
#50837=CARTESIAN_POINT('Origin',(-19.558,63.645,12.066));
#50838=CARTESIAN_POINT('',(-21.436,63.745,12.066));
#50839=CARTESIAN_POINT('Origin',(-19.558,63.845,12.066));
#50840=CARTESIAN_POINT('',(-21.336,57.495,12.066));
#50841=CARTESIAN_POINT('',(-21.336,63.845,12.066));
#50842=CARTESIAN_POINT('Origin',(-19.558,57.495,12.066));
#50843=CARTESIAN_POINT('Origin',(0.,63.745,12.066));
#50844=CARTESIAN_POINT('',(-1.778,63.645,12.066));
#50845=CARTESIAN_POINT('Origin',(0.,63.645,12.066));
#50846=CARTESIAN_POINT('',(-1.878,63.745,12.066));
#50847=CARTESIAN_POINT('Origin',(0.,63.845,12.066));
#50848=CARTESIAN_POINT('',(-1.778,57.495,12.066));
#50849=CARTESIAN_POINT('',(-1.778,63.845,12.066));
#50850=CARTESIAN_POINT('Origin',(0.,57.495,12.066));
#50851=CARTESIAN_POINT('Origin',(9.779,63.745,12.066));
#50852=CARTESIAN_POINT('',(8.001,63.645,12.066));
#50853=CARTESIAN_POINT('Origin',(9.779,63.645,12.066));
#50854=CARTESIAN_POINT('',(7.901,63.745,12.066));
#50855=CARTESIAN_POINT('Origin',(9.779,63.845,12.066));
#50856=CARTESIAN_POINT('',(8.001,57.495,12.066));
#50857=CARTESIAN_POINT('',(8.001,63.845,12.066));
#50858=CARTESIAN_POINT('Origin',(9.779,57.495,12.066));
#50859=CARTESIAN_POINT('Origin',(29.337,63.745,12.066));
#50860=CARTESIAN_POINT('',(27.559,63.645,12.066));
#50861=CARTESIAN_POINT('Origin',(29.337,63.645,12.066));
#50862=CARTESIAN_POINT('',(27.459,63.745,12.066));
#50863=CARTESIAN_POINT('Origin',(29.337,63.845,12.066));
#50864=CARTESIAN_POINT('',(27.559,57.495,12.066));
#50865=CARTESIAN_POINT('',(27.559,63.845,12.066));
#50866=CARTESIAN_POINT('Origin',(29.337,57.495,12.066));
#50867=CARTESIAN_POINT('Origin',(48.895,63.745,12.066));
#50868=CARTESIAN_POINT('',(47.117,63.645,12.066));
#50869=CARTESIAN_POINT('Origin',(48.895,63.645,12.066));
#50870=CARTESIAN_POINT('',(47.017,63.745,12.066));
#50871=CARTESIAN_POINT('Origin',(48.895,63.845,12.066));
#50872=CARTESIAN_POINT('',(47.117,57.495,12.066));
#50873=CARTESIAN_POINT('',(47.117,63.845,12.066));
#50874=CARTESIAN_POINT('Origin',(48.895,57.495,12.066));
#50875=CARTESIAN_POINT('Origin',(68.453,63.745,12.066));
#50876=CARTESIAN_POINT('',(66.675,63.645,12.066));
#50877=CARTESIAN_POINT('Origin',(68.453,63.645,12.066));
#50878=CARTESIAN_POINT('',(66.575,63.745,12.066));
#50879=CARTESIAN_POINT('Origin',(68.453,63.845,12.066));
#50880=CARTESIAN_POINT('',(66.675,57.495,12.066));
#50881=CARTESIAN_POINT('',(66.675,63.845,12.066));
#50882=CARTESIAN_POINT('Origin',(68.453,57.495,12.066));
#50883=CARTESIAN_POINT('Origin',(88.011,63.745,12.066));
#50884=CARTESIAN_POINT('',(86.233,63.645,12.066));
#50885=CARTESIAN_POINT('Origin',(88.011,63.645,12.066));
#50886=CARTESIAN_POINT('',(86.133,63.745,12.066));
#50887=CARTESIAN_POINT('Origin',(88.011,63.845,12.066));
#50888=CARTESIAN_POINT('',(86.233,57.495,12.066));
#50889=CARTESIAN_POINT('',(86.233,63.845,12.066));
#50890=CARTESIAN_POINT('Origin',(88.011,57.495,12.066));
#50891=CARTESIAN_POINT('Origin',(-48.895,63.72,16.7035));
#50892=CARTESIAN_POINT('',(97.79,63.595,16.8285));
#50893=CARTESIAN_POINT('',(97.79,63.595,16.8285));
#50894=CARTESIAN_POINT('',(-97.79,63.595,16.8285));
#50895=CARTESIAN_POINT('',(-97.79,63.845,16.5785));
#50896=CARTESIAN_POINT('',(-48.895,63.595,16.8285));
#50897=CARTESIAN_POINT('Origin',(97.79,63.72,12.066));
#50898=CARTESIAN_POINT('',(97.79,63.595,7.3035));
#50899=CARTESIAN_POINT('',(97.79,63.595,7.3035));
#50900=CARTESIAN_POINT('Origin',(97.79,63.595,12.066));
#50901=CARTESIAN_POINT('Origin',(48.895,63.72,7.4285));
#50902=CARTESIAN_POINT('',(-97.79,63.595,7.3035));
#50903=CARTESIAN_POINT('',(-97.79,63.595,7.3035));
#50904=CARTESIAN_POINT('',(48.895,63.595,7.3035));
#50905=CARTESIAN_POINT('Origin',(-97.79,63.72,12.066));
#50906=CARTESIAN_POINT('Origin',(-97.79,63.595,12.066));
#50907=CARTESIAN_POINT('Origin',(97.79,57.495,12.066));
#50908=CARTESIAN_POINT('',(97.79,57.745,16.8285));
#50909=CARTESIAN_POINT('',(97.79,57.495,16.8285));
#50910=CARTESIAN_POINT('',(97.79,57.745,7.3035));
#50911=CARTESIAN_POINT('Origin',(97.79,57.745,12.066));
#50912=CARTESIAN_POINT('',(97.79,57.495,7.3035));
#50913=CARTESIAN_POINT('Origin',(-97.79,57.495,16.8285));
#50914=CARTESIAN_POINT('',(-97.79,57.745,16.8285));
#50915=CARTESIAN_POINT('',(-97.79,57.495,16.8285));
#50916=CARTESIAN_POINT('',(-48.895,57.745,16.8285));
#50917=CARTESIAN_POINT('Origin',(-48.895,57.62,16.7035));
#50918=CARTESIAN_POINT('',(-97.79,57.495,16.5785));
#50919=CARTESIAN_POINT('',(-97.79,57.745,16.8285));
#50920=CARTESIAN_POINT('',(97.79,57.495,16.5785));
#50921=CARTESIAN_POINT('',(-48.895,57.495,16.5785));
#50922=CARTESIAN_POINT('',(97.79,57.495,16.5785));
#50923=CARTESIAN_POINT('Origin',(-97.79,57.62,12.066));
#50924=CARTESIAN_POINT('',(-97.79,57.745,7.3035));
#50925=CARTESIAN_POINT('Origin',(-97.79,57.745,12.066));
#50926=CARTESIAN_POINT('',(-97.79,57.495,7.5535));
#50927=CARTESIAN_POINT('',(-97.79,57.745,7.3035));
#50928=CARTESIAN_POINT('Origin',(-97.79,57.495,12.066));
#50929=CARTESIAN_POINT('Origin',(48.895,57.62,7.4285));
#50930=CARTESIAN_POINT('',(97.79,57.495,7.5535));
#50931=CARTESIAN_POINT('',(97.79,57.745,7.3035));
#50932=CARTESIAN_POINT('',(48.895,57.495,7.5535));
#50933=CARTESIAN_POINT('',(48.895,57.745,7.3035));
#50934=CARTESIAN_POINT('Origin',(97.79,57.62,12.066));
#50935=CARTESIAN_POINT('Origin',(97.79,57.495,12.066));
#50936=CARTESIAN_POINT('Origin',(-97.79,57.495,12.066));
#50937=CARTESIAN_POINT('',(-97.79,57.495,7.3035));
#50938=CARTESIAN_POINT('Origin',(0.,57.495,12.066));
#50939=CARTESIAN_POINT('Origin',(97.79,57.495,7.3035));
#50940=CARTESIAN_POINT('',(0.,0.,0.));
#50941=CARTESIAN_POINT('Origin',(-43.4930033668588,57.395,7.4035));
#50942=CARTESIAN_POINT('',(-87.0588007805708,57.495,7.5035));
#50943=CARTESIAN_POINT('',(-86.9860067337175,57.295,7.3035));
#50944=CARTESIAN_POINT('',(-85.229357070045,52.4686447151669,2.47714471516705));
#50945=CARTESIAN_POINT('',(-88.011,57.295,7.3035));
#50946=CARTESIAN_POINT('',(-43.4930033668588,57.295,7.3035));
#50947=CARTESIAN_POINT('',(-88.011,57.495,7.5035));
#50948=CARTESIAN_POINT('',(-88.011,57.295,7.3035));
#50949=CARTESIAN_POINT('',(-43.4930033668588,57.495,7.5035));
#50950=CARTESIAN_POINT('Origin',(-88.011,57.395,12.066));
#50951=CARTESIAN_POINT('',(-88.011,57.295,16.8285));
#50952=CARTESIAN_POINT('',(-88.011,57.495,16.6285));
#50953=CARTESIAN_POINT('',(-88.011,57.295,16.8285));
#50954=CARTESIAN_POINT('Origin',(-88.011,57.495,12.066));
#50955=CARTESIAN_POINT('Origin',(-88.011,57.295,12.066));
#50956=CARTESIAN_POINT('Origin',(-44.0055,57.395,16.7285));
#50957=CARTESIAN_POINT('',(88.011,57.295,16.8285));
#50958=CARTESIAN_POINT('',(88.011,57.495,16.6285));
#50959=CARTESIAN_POINT('',(88.011,57.295,16.8285));
#50960=CARTESIAN_POINT('',(-44.0055,57.495,16.6285));
#50961=CARTESIAN_POINT('',(-44.0055,57.295,16.8285));
#50962=CARTESIAN_POINT('Origin',(88.011,57.395,12.066));
#50963=CARTESIAN_POINT('',(88.011,57.295,7.3035));
#50964=CARTESIAN_POINT('',(88.011,57.495,7.5035));
#50965=CARTESIAN_POINT('',(88.011,57.295,7.3035));
#50966=CARTESIAN_POINT('Origin',(88.011,57.495,12.066));
#50967=CARTESIAN_POINT('Origin',(88.011,57.295,12.066));
#50968=CARTESIAN_POINT('Origin',(44.0055,57.395,7.4035));
#50969=CARTESIAN_POINT('',(86.9860067337175,57.295,7.3035));
#50970=CARTESIAN_POINT('',(87.0588007805708,57.495,7.5035));
#50971=CARTESIAN_POINT('',(85.4141633601712,52.9763958242619,2.98489582426201));
#50972=CARTESIAN_POINT('',(44.0055,57.495,7.5035));
#50973=CARTESIAN_POINT('',(44.0055,57.295,7.3035));
#50974=CARTESIAN_POINT('Origin',(88.011,54.32,7.3035));
#50975=CARTESIAN_POINT('',(88.011,54.52,7.3035));
#50976=CARTESIAN_POINT('',(88.011,54.32,7.3035));
#50977=CARTESIAN_POINT('',(86.9860067337175,54.52,7.3035));
#50978=CARTESIAN_POINT('',(44.0055,54.52,7.3035));
#50979=CARTESIAN_POINT('',(86.9860067337175,54.32,7.3035));
#50980=CARTESIAN_POINT('Origin',(88.011,54.32,12.066));
#50981=CARTESIAN_POINT('',(88.011,54.52,16.8285));
#50982=CARTESIAN_POINT('',(88.011,54.32,16.8285));
#50983=CARTESIAN_POINT('Origin',(88.011,54.52,12.066));
#50984=CARTESIAN_POINT('Origin',(-88.011,54.32,16.8285));
#50985=CARTESIAN_POINT('',(-88.011,54.52,16.8285));
#50986=CARTESIAN_POINT('',(-88.011,54.32,16.8285));
#50987=CARTESIAN_POINT('',(-44.0055,54.52,16.8285));
#50988=CARTESIAN_POINT('Origin',(-88.011,54.32,12.066));
#50989=CARTESIAN_POINT('',(-88.011,54.52,7.3035));
#50990=CARTESIAN_POINT('',(-88.011,54.32,7.3035));
#50991=CARTESIAN_POINT('Origin',(-88.011,54.52,12.066));
#50992=CARTESIAN_POINT('Origin',(-86.9860067337175,54.32,7.3035));
#50993=CARTESIAN_POINT('',(-86.9860067337175,54.52,7.3035));
#50994=CARTESIAN_POINT('',(-86.9860067337175,54.32,7.3035));
#50995=CARTESIAN_POINT('',(-43.4930033668588,54.52,7.3035));
#50996=CARTESIAN_POINT('Origin',(44.0055,54.42,7.4035));
#50997=CARTESIAN_POINT('',(87.0588007805708,54.32,7.5035));
#50998=CARTESIAN_POINT('',(85.6851174993985,58.0941637965031,3.72933620349686));
#50999=CARTESIAN_POINT('',(88.011,54.32,7.5035));
#51000=CARTESIAN_POINT('',(88.011,54.52,7.3035));
#51001=CARTESIAN_POINT('',(44.0055,54.32,7.5035));
#51002=CARTESIAN_POINT('Origin',(88.011,54.42,12.066));
#51003=CARTESIAN_POINT('',(88.011,54.32,16.6285));
#51004=CARTESIAN_POINT('',(88.011,54.52,16.8285));
#51005=CARTESIAN_POINT('Origin',(88.011,54.32,12.066));
#51006=CARTESIAN_POINT('Origin',(-44.0055,54.42,16.7285));
#51007=CARTESIAN_POINT('',(-88.011,54.32,16.6285));
#51008=CARTESIAN_POINT('',(-88.011,54.52,16.8285));
#51009=CARTESIAN_POINT('',(-44.0055,54.32,16.6285));
#51010=CARTESIAN_POINT('Origin',(-88.011,54.42,12.066));
#51011=CARTESIAN_POINT('',(-88.011,54.32,7.5035));
#51012=CARTESIAN_POINT('',(-88.011,54.52,7.3035));
#51013=CARTESIAN_POINT('Origin',(-88.011,54.32,12.066));
#51014=CARTESIAN_POINT('Origin',(-43.4930033668588,54.42,7.4035));
#51015=CARTESIAN_POINT('',(-87.0588007805708,54.32,7.5035));
#51016=CARTESIAN_POINT('',(-85.5003112092723,58.601914905598,3.22158509440188));
#51017=CARTESIAN_POINT('',(-43.4930033668588,54.32,7.5035));
#51018=CARTESIAN_POINT('Origin',(68.453,57.495,12.066));
#51019=CARTESIAN_POINT('',(66.675,57.495,12.066));
#51020=CARTESIAN_POINT('Origin',(68.453,57.495,12.066));
#51021=CARTESIAN_POINT('',(66.675,54.32,12.066));
#51022=CARTESIAN_POINT('',(66.675,57.495,12.066));
#51023=CARTESIAN_POINT('Origin',(68.453,54.32,12.066));
#51024=CARTESIAN_POINT('Origin',(29.337,57.495,12.066));
#51025=CARTESIAN_POINT('',(27.559,57.495,12.066));
#51026=CARTESIAN_POINT('Origin',(29.337,57.495,12.066));
#51027=CARTESIAN_POINT('',(27.559,54.32,12.066));
#51028=CARTESIAN_POINT('',(27.559,57.495,12.066));
#51029=CARTESIAN_POINT('Origin',(29.337,54.32,12.066));
#51030=CARTESIAN_POINT('Origin',(-88.011,57.495,12.066));
#51031=CARTESIAN_POINT('',(-89.789,57.495,12.066));
#51032=CARTESIAN_POINT('Origin',(-88.011,57.495,12.066));
#51033=CARTESIAN_POINT('',(-89.789,54.32,12.066));
#51034=CARTESIAN_POINT('',(-89.789,57.495,12.066));
#51035=CARTESIAN_POINT('Origin',(-88.011,54.32,12.066));
#51036=CARTESIAN_POINT('Origin',(-29.337,57.495,12.066));
#51037=CARTESIAN_POINT('',(-31.115,57.495,12.066));
#51038=CARTESIAN_POINT('Origin',(-29.337,57.495,12.066));
#51039=CARTESIAN_POINT('',(-31.115,54.32,12.066));
#51040=CARTESIAN_POINT('',(-31.115,57.495,12.066));
#51041=CARTESIAN_POINT('Origin',(-29.337,54.32,12.066));
#51042=CARTESIAN_POINT('Origin',(-68.453,57.495,12.066));
#51043=CARTESIAN_POINT('',(-70.231,57.495,12.066));
#51044=CARTESIAN_POINT('Origin',(-68.453,57.495,12.066));
#51045=CARTESIAN_POINT('',(-70.231,54.32,12.066));
#51046=CARTESIAN_POINT('',(-70.231,57.495,12.066));
#51047=CARTESIAN_POINT('Origin',(-68.453,54.32,12.066));
#51048=CARTESIAN_POINT('Origin',(-48.895,57.495,12.066));
#51049=CARTESIAN_POINT('',(-50.673,57.495,12.066));
#51050=CARTESIAN_POINT('Origin',(-48.895,57.495,12.066));
#51051=CARTESIAN_POINT('',(-50.673,54.32,12.066));
#51052=CARTESIAN_POINT('',(-50.673,57.495,12.066));
#51053=CARTESIAN_POINT('Origin',(-48.895,54.32,12.066));
#51054=CARTESIAN_POINT('Origin',(-9.779,57.495,12.066));
#51055=CARTESIAN_POINT('',(-11.557,57.495,12.066));
#51056=CARTESIAN_POINT('Origin',(-9.779,57.495,12.066));
#51057=CARTESIAN_POINT('',(-11.557,54.32,12.066));
#51058=CARTESIAN_POINT('',(-11.557,57.495,12.066));
#51059=CARTESIAN_POINT('Origin',(-9.779,54.32,12.066));
#51060=CARTESIAN_POINT('Origin',(9.779,57.495,12.066));
#51061=CARTESIAN_POINT('',(8.001,57.495,12.066));
#51062=CARTESIAN_POINT('Origin',(9.779,57.495,12.066));
#51063=CARTESIAN_POINT('',(8.001,54.32,12.066));
#51064=CARTESIAN_POINT('',(8.001,57.495,12.066));
#51065=CARTESIAN_POINT('Origin',(9.779,54.32,12.066));
#51066=CARTESIAN_POINT('Origin',(48.895,57.495,12.066));
#51067=CARTESIAN_POINT('',(47.117,57.495,12.066));
#51068=CARTESIAN_POINT('Origin',(48.895,57.495,12.066));
#51069=CARTESIAN_POINT('',(47.117,54.32,12.066));
#51070=CARTESIAN_POINT('',(47.117,57.495,12.066));
#51071=CARTESIAN_POINT('Origin',(48.895,54.32,12.066));
#51072=CARTESIAN_POINT('Origin',(88.011,57.495,12.066));
#51073=CARTESIAN_POINT('',(86.233,57.495,12.066));
#51074=CARTESIAN_POINT('Origin',(88.011,57.495,12.066));
#51075=CARTESIAN_POINT('',(86.233,54.32,12.066));
#51076=CARTESIAN_POINT('',(86.233,57.495,12.066));
#51077=CARTESIAN_POINT('Origin',(88.011,54.32,12.066));
#51078=CARTESIAN_POINT('Origin',(-86.3499687493374,54.32,5.556));
#51079=CARTESIAN_POINT('',(-86.3499687493374,54.32,5.556));
#51080=CARTESIAN_POINT('',(-86.9860067337175,54.32,7.3035));
#51081=CARTESIAN_POINT('',(-86.3499687493374,57.495,5.556));
#51082=CARTESIAN_POINT('',(-86.9860067337175,57.495,7.3035));
#51083=CARTESIAN_POINT('',(-86.3499687493374,54.32,5.556));
#51084=CARTESIAN_POINT('Origin',(-85.7111338969586,54.32,5.556));
#51085=CARTESIAN_POINT('',(-85.7111338969586,54.32,5.556));
#51086=CARTESIAN_POINT('',(-86.3499687493374,54.32,5.556));
#51087=CARTESIAN_POINT('',(-85.7111338969586,57.495,5.556));
#51088=CARTESIAN_POINT('',(-86.3499687493374,57.495,5.556));
#51089=CARTESIAN_POINT('',(-85.7111338969586,54.32,5.556));
#51090=CARTESIAN_POINT('Origin',(-85.0750959125784,54.32,7.3035));
#51091=CARTESIAN_POINT('',(-85.0750959125784,54.32,7.3035));
#51092=CARTESIAN_POINT('',(-85.7111338969586,54.32,5.556));
#51093=CARTESIAN_POINT('',(-85.0750959125784,57.495,7.3035));
#51094=CARTESIAN_POINT('',(-85.7111338969586,57.495,5.556));
#51095=CARTESIAN_POINT('',(-85.0750959125784,54.32,7.3035));
#51096=CARTESIAN_POINT('Origin',(-84.4923675649306,54.32,7.3035));
#51097=CARTESIAN_POINT('',(-84.4923675649306,54.32,7.3035));
#51098=CARTESIAN_POINT('',(-85.0750959125784,54.32,7.3035));
#51099=CARTESIAN_POINT('',(-84.4923675649306,57.495,7.3035));
#51100=CARTESIAN_POINT('',(-85.0750959125784,57.495,7.3035));
#51101=CARTESIAN_POINT('',(-84.4923675649306,54.32,7.3035));
#51102=CARTESIAN_POINT('Origin',(-83.8563295805504,54.32,5.556));
#51103=CARTESIAN_POINT('',(-83.8563295805504,54.32,5.556));
#51104=CARTESIAN_POINT('',(-84.4923675649306,54.32,7.3035));
#51105=CARTESIAN_POINT('',(-83.8563295805504,57.495,5.556));
#51106=CARTESIAN_POINT('',(-84.4923675649306,57.495,7.3035));
#51107=CARTESIAN_POINT('',(-83.8563295805504,54.32,5.556));
#51108=CARTESIAN_POINT('Origin',(-83.2174947281717,54.32,5.556));
#51109=CARTESIAN_POINT('',(-83.2174947281717,54.32,5.556));
#51110=CARTESIAN_POINT('',(-83.8563295805504,54.32,5.556));
#51111=CARTESIAN_POINT('',(-83.2174947281717,57.495,5.556));
#51112=CARTESIAN_POINT('',(-83.8563295805504,57.495,5.556));
#51113=CARTESIAN_POINT('',(-83.2174947281717,54.32,5.556));
#51114=CARTESIAN_POINT('Origin',(-82.5814567437915,54.32,7.3035));
#51115=CARTESIAN_POINT('',(-82.5814567437915,54.32,7.3035));
#51116=CARTESIAN_POINT('',(-83.2174947281717,54.32,5.556));
#51117=CARTESIAN_POINT('',(-82.5814567437915,57.495,7.3035));
#51118=CARTESIAN_POINT('',(-83.2174947281717,57.495,5.556));
#51119=CARTESIAN_POINT('',(-82.5814567437915,54.32,7.3035));
#51120=CARTESIAN_POINT('Origin',(-81.9987283961437,54.32,7.3035));
#51121=CARTESIAN_POINT('',(-81.9987283961437,54.32,7.3035));
#51122=CARTESIAN_POINT('',(-82.5814567437915,54.32,7.3035));
#51123=CARTESIAN_POINT('',(-81.9987283961437,57.495,7.3035));
#51124=CARTESIAN_POINT('',(-82.5814567437915,57.495,7.3035));
#51125=CARTESIAN_POINT('',(-81.9987283961437,54.32,7.3035));
#51126=CARTESIAN_POINT('Origin',(-81.3626904117636,54.32,5.556));
#51127=CARTESIAN_POINT('',(-81.3626904117636,54.32,5.556));
#51128=CARTESIAN_POINT('',(-81.9987283961437,54.32,7.3035));
#51129=CARTESIAN_POINT('',(-81.3626904117636,57.495,5.556));
#51130=CARTESIAN_POINT('',(-81.9987283961437,57.495,7.3035));
#51131=CARTESIAN_POINT('',(-81.3626904117636,54.32,5.556));
#51132=CARTESIAN_POINT('Origin',(-80.7238555593848,54.32,5.556));
#51133=CARTESIAN_POINT('',(-80.7238555593848,54.32,5.556));
#51134=CARTESIAN_POINT('',(-81.3626904117636,54.32,5.556));
#51135=CARTESIAN_POINT('',(-80.7238555593848,57.495,5.556));
#51136=CARTESIAN_POINT('',(-81.3626904117636,57.495,5.556));
#51137=CARTESIAN_POINT('',(-80.7238555593848,54.32,5.556));
#51138=CARTESIAN_POINT('Origin',(-80.0878175750046,54.32,7.3035));
#51139=CARTESIAN_POINT('',(-80.0878175750046,54.32,7.3035));
#51140=CARTESIAN_POINT('',(-80.7238555593848,54.32,5.556));
#51141=CARTESIAN_POINT('',(-80.0878175750046,57.495,7.3035));
#51142=CARTESIAN_POINT('',(-80.7238555593848,57.495,5.556));
#51143=CARTESIAN_POINT('',(-80.0878175750046,54.32,7.3035));
#51144=CARTESIAN_POINT('Origin',(-79.5050892273568,54.32,7.3035));
#51145=CARTESIAN_POINT('',(-79.5050892273568,54.32,7.3035));
#51146=CARTESIAN_POINT('',(-80.0878175750046,54.32,7.3035));
#51147=CARTESIAN_POINT('',(-79.5050892273568,57.495,7.3035));
#51148=CARTESIAN_POINT('',(-80.0878175750046,57.495,7.3035));
#51149=CARTESIAN_POINT('',(-79.5050892273568,54.32,7.3035));
#51150=CARTESIAN_POINT('Origin',(-78.8690512429767,54.32,5.556));
#51151=CARTESIAN_POINT('',(-78.8690512429767,54.32,5.556));
#51152=CARTESIAN_POINT('',(-79.5050892273568,54.32,7.3035));
#51153=CARTESIAN_POINT('',(-78.8690512429767,57.495,5.556));
#51154=CARTESIAN_POINT('',(-79.5050892273568,57.495,7.3035));
#51155=CARTESIAN_POINT('',(-78.8690512429767,54.32,5.556));
#51156=CARTESIAN_POINT('Origin',(-78.2302163905979,54.32,5.556));
#51157=CARTESIAN_POINT('',(-78.2302163905979,54.32,5.556));
#51158=CARTESIAN_POINT('',(-78.8690512429767,54.32,5.556));
#51159=CARTESIAN_POINT('',(-78.2302163905979,57.495,5.556));
#51160=CARTESIAN_POINT('',(-78.8690512429767,57.495,5.556));
#51161=CARTESIAN_POINT('',(-78.2302163905979,54.32,5.556));
#51162=CARTESIAN_POINT('Origin',(-77.5941784062178,54.32,7.3035));
#51163=CARTESIAN_POINT('',(-77.5941784062178,54.32,7.3035));
#51164=CARTESIAN_POINT('',(-78.2302163905979,54.32,5.556));
#51165=CARTESIAN_POINT('',(-77.5941784062178,57.495,7.3035));
#51166=CARTESIAN_POINT('',(-78.2302163905979,57.495,5.556));
#51167=CARTESIAN_POINT('',(-77.5941784062178,54.32,7.3035));
#51168=CARTESIAN_POINT('Origin',(-77.0114500585699,54.32,7.3035));
#51169=CARTESIAN_POINT('',(-77.0114500585699,54.32,7.3035));
#51170=CARTESIAN_POINT('',(-77.5941784062178,54.32,7.3035));
#51171=CARTESIAN_POINT('',(-77.0114500585699,57.495,7.3035));
#51172=CARTESIAN_POINT('',(-77.5941784062178,57.495,7.3035));
#51173=CARTESIAN_POINT('',(-77.0114500585699,54.32,7.3035));
#51174=CARTESIAN_POINT('Origin',(-76.3754120741898,54.32,5.556));
#51175=CARTESIAN_POINT('',(-76.3754120741898,54.32,5.556));
#51176=CARTESIAN_POINT('',(-77.0114500585699,54.32,7.3035));
#51177=CARTESIAN_POINT('',(-76.3754120741898,57.495,5.556));
#51178=CARTESIAN_POINT('',(-77.0114500585699,57.495,7.3035));
#51179=CARTESIAN_POINT('',(-76.3754120741898,54.32,5.556));
#51180=CARTESIAN_POINT('Origin',(-75.736577221811,54.32,5.556));
#51181=CARTESIAN_POINT('',(-75.736577221811,54.32,5.556));
#51182=CARTESIAN_POINT('',(-76.3754120741898,54.32,5.556));
#51183=CARTESIAN_POINT('',(-75.736577221811,57.495,5.556));
#51184=CARTESIAN_POINT('',(-76.3754120741898,57.495,5.556));
#51185=CARTESIAN_POINT('',(-75.736577221811,54.32,5.556));
#51186=CARTESIAN_POINT('Origin',(-75.1005392374309,54.32,7.3035));
#51187=CARTESIAN_POINT('',(-75.1005392374309,54.32,7.3035));
#51188=CARTESIAN_POINT('',(-75.736577221811,54.32,5.556));
#51189=CARTESIAN_POINT('',(-75.1005392374309,57.495,7.3035));
#51190=CARTESIAN_POINT('',(-75.736577221811,57.495,5.556));
#51191=CARTESIAN_POINT('',(-75.1005392374309,54.32,7.3035));
#51192=CARTESIAN_POINT('Origin',(-74.517810889783,54.32,7.3035));
#51193=CARTESIAN_POINT('',(-74.517810889783,54.32,7.3035));
#51194=CARTESIAN_POINT('',(-75.1005392374309,54.32,7.3035));
#51195=CARTESIAN_POINT('',(-74.517810889783,57.495,7.3035));
#51196=CARTESIAN_POINT('',(-75.1005392374309,57.495,7.3035));
#51197=CARTESIAN_POINT('',(-74.517810889783,54.32,7.3035));
#51198=CARTESIAN_POINT('Origin',(-73.8817729054029,54.32,5.556));
#51199=CARTESIAN_POINT('',(-73.8817729054029,54.32,5.556));
#51200=CARTESIAN_POINT('',(-74.517810889783,54.32,7.3035));
#51201=CARTESIAN_POINT('',(-73.8817729054029,57.495,5.556));
#51202=CARTESIAN_POINT('',(-74.517810889783,57.495,7.3035));
#51203=CARTESIAN_POINT('',(-73.8817729054029,54.32,5.556));
#51204=CARTESIAN_POINT('Origin',(-73.2429380530241,54.32,5.556));
#51205=CARTESIAN_POINT('',(-73.2429380530241,54.32,5.556));
#51206=CARTESIAN_POINT('',(-73.8817729054029,54.32,5.556));
#51207=CARTESIAN_POINT('',(-73.2429380530241,57.495,5.556));
#51208=CARTESIAN_POINT('',(-73.8817729054029,57.495,5.556));
#51209=CARTESIAN_POINT('',(-73.2429380530241,54.32,5.556));
#51210=CARTESIAN_POINT('Origin',(-72.606900068644,54.32,7.3035));
#51211=CARTESIAN_POINT('',(-72.606900068644,54.32,7.3035));
#51212=CARTESIAN_POINT('',(-73.2429380530241,54.32,5.556));
#51213=CARTESIAN_POINT('',(-72.606900068644,57.495,7.3035));
#51214=CARTESIAN_POINT('',(-73.2429380530241,57.495,5.556));
#51215=CARTESIAN_POINT('',(-72.606900068644,54.32,7.3035));
#51216=CARTESIAN_POINT('Origin',(-72.0241717209961,54.32,7.3035));
#51217=CARTESIAN_POINT('',(-72.0241717209961,54.32,7.3035));
#51218=CARTESIAN_POINT('',(-72.606900068644,54.32,7.3035));
#51219=CARTESIAN_POINT('',(-72.0241717209961,57.495,7.3035));
#51220=CARTESIAN_POINT('',(-72.606900068644,57.495,7.3035));
#51221=CARTESIAN_POINT('',(-72.0241717209961,54.32,7.3035));
#51222=CARTESIAN_POINT('Origin',(-71.388133736616,54.32,5.556));
#51223=CARTESIAN_POINT('',(-71.388133736616,54.32,5.556));
#51224=CARTESIAN_POINT('',(-72.0241717209961,54.32,7.3035));
#51225=CARTESIAN_POINT('',(-71.388133736616,57.495,5.556));
#51226=CARTESIAN_POINT('',(-72.0241717209961,57.495,7.3035));
#51227=CARTESIAN_POINT('',(-71.388133736616,54.32,5.556));
#51228=CARTESIAN_POINT('Origin',(-70.7492988842372,54.32,5.556));
#51229=CARTESIAN_POINT('',(-70.7492988842372,54.32,5.556));
#51230=CARTESIAN_POINT('',(-71.388133736616,54.32,5.556));
#51231=CARTESIAN_POINT('',(-70.7492988842372,57.495,5.556));
#51232=CARTESIAN_POINT('',(-71.388133736616,57.495,5.556));
#51233=CARTESIAN_POINT('',(-70.7492988842372,54.32,5.556));
#51234=CARTESIAN_POINT('Origin',(-70.1132608998571,54.32,7.3035));
#51235=CARTESIAN_POINT('',(-70.1132608998571,54.32,7.3035));
#51236=CARTESIAN_POINT('',(-70.7492988842372,54.32,5.556));
#51237=CARTESIAN_POINT('',(-70.1132608998571,57.495,7.3035));
#51238=CARTESIAN_POINT('',(-70.7492988842372,57.495,5.556));
#51239=CARTESIAN_POINT('',(-70.1132608998571,54.32,7.3035));
#51240=CARTESIAN_POINT('Origin',(-69.5305325522092,54.32,7.3035));
#51241=CARTESIAN_POINT('',(-69.5305325522092,54.32,7.3035));
#51242=CARTESIAN_POINT('',(-70.1132608998571,54.32,7.3035));
#51243=CARTESIAN_POINT('',(-69.5305325522092,57.495,7.3035));
#51244=CARTESIAN_POINT('',(-70.1132608998571,57.495,7.3035));
#51245=CARTESIAN_POINT('',(-69.5305325522092,54.32,7.3035));
#51246=CARTESIAN_POINT('Origin',(-68.8944945678291,54.32,5.556));
#51247=CARTESIAN_POINT('',(-68.8944945678291,54.32,5.556));
#51248=CARTESIAN_POINT('',(-69.5305325522092,54.32,7.3035));
#51249=CARTESIAN_POINT('',(-68.8944945678291,57.495,5.556));
#51250=CARTESIAN_POINT('',(-69.5305325522092,57.495,7.3035));
#51251=CARTESIAN_POINT('',(-68.8944945678291,54.32,5.556));
#51252=CARTESIAN_POINT('Origin',(-68.2556597154503,54.32,5.556));
#51253=CARTESIAN_POINT('',(-68.2556597154503,54.32,5.556));
#51254=CARTESIAN_POINT('',(-68.8944945678291,54.32,5.556));
#51255=CARTESIAN_POINT('',(-68.2556597154503,57.495,5.556));
#51256=CARTESIAN_POINT('',(-68.8944945678291,57.495,5.556));
#51257=CARTESIAN_POINT('',(-68.2556597154503,54.32,5.556));
#51258=CARTESIAN_POINT('Origin',(-67.6196217310702,54.32,7.3035));
#51259=CARTESIAN_POINT('',(-67.6196217310702,54.32,7.3035));
#51260=CARTESIAN_POINT('',(-68.2556597154503,54.32,5.556));
#51261=CARTESIAN_POINT('',(-67.6196217310702,57.495,7.3035));
#51262=CARTESIAN_POINT('',(-68.2556597154503,57.495,5.556));
#51263=CARTESIAN_POINT('',(-67.6196217310702,54.32,7.3035));
#51264=CARTESIAN_POINT('Origin',(-67.0368933834223,54.32,7.3035));
#51265=CARTESIAN_POINT('',(-67.0368933834223,54.32,7.3035));
#51266=CARTESIAN_POINT('',(-67.6196217310702,54.32,7.3035));
#51267=CARTESIAN_POINT('',(-67.0368933834223,57.495,7.3035));
#51268=CARTESIAN_POINT('',(-67.6196217310702,57.495,7.3035));
#51269=CARTESIAN_POINT('',(-67.0368933834223,54.32,7.3035));
#51270=CARTESIAN_POINT('Origin',(-66.4008553990422,54.32,5.556));
#51271=CARTESIAN_POINT('',(-66.4008553990422,54.32,5.556));
#51272=CARTESIAN_POINT('',(-67.0368933834223,54.32,7.3035));
#51273=CARTESIAN_POINT('',(-66.4008553990422,57.495,5.556));
#51274=CARTESIAN_POINT('',(-67.0368933834223,57.495,7.3035));
#51275=CARTESIAN_POINT('',(-66.4008553990422,54.32,5.556));
#51276=CARTESIAN_POINT('Origin',(-65.7620205466634,54.32,5.556));
#51277=CARTESIAN_POINT('',(-65.7620205466634,54.32,5.556));
#51278=CARTESIAN_POINT('',(-66.4008553990422,54.32,5.556));
#51279=CARTESIAN_POINT('',(-65.7620205466634,57.495,5.556));
#51280=CARTESIAN_POINT('',(-66.4008553990422,57.495,5.556));
#51281=CARTESIAN_POINT('',(-65.7620205466634,54.32,5.556));
#51282=CARTESIAN_POINT('Origin',(-65.1259825622833,54.32,7.3035));
#51283=CARTESIAN_POINT('',(-65.1259825622833,54.32,7.3035));
#51284=CARTESIAN_POINT('',(-65.7620205466634,54.32,5.556));
#51285=CARTESIAN_POINT('',(-65.1259825622833,57.495,7.3035));
#51286=CARTESIAN_POINT('',(-65.7620205466634,57.495,5.556));
#51287=CARTESIAN_POINT('',(-65.1259825622833,54.32,7.3035));
#51288=CARTESIAN_POINT('Origin',(-64.5432542146355,54.32,7.3035));
#51289=CARTESIAN_POINT('',(-64.5432542146355,54.32,7.3035));
#51290=CARTESIAN_POINT('',(-65.1259825622833,54.32,7.3035));
#51291=CARTESIAN_POINT('',(-64.5432542146355,57.495,7.3035));
#51292=CARTESIAN_POINT('',(-65.1259825622833,57.495,7.3035));
#51293=CARTESIAN_POINT('',(-64.5432542146355,54.32,7.3035));
#51294=CARTESIAN_POINT('Origin',(-63.9072162302553,54.32,5.556));
#51295=CARTESIAN_POINT('',(-63.9072162302553,54.32,5.556));
#51296=CARTESIAN_POINT('',(-64.5432542146355,54.32,7.3035));
#51297=CARTESIAN_POINT('',(-63.9072162302553,57.495,5.556));
#51298=CARTESIAN_POINT('',(-64.5432542146355,57.495,7.3035));
#51299=CARTESIAN_POINT('',(-63.9072162302553,54.32,5.556));
#51300=CARTESIAN_POINT('Origin',(-63.2683813778765,54.32,5.556));
#51301=CARTESIAN_POINT('',(-63.2683813778765,54.32,5.556));
#51302=CARTESIAN_POINT('',(-63.9072162302553,54.32,5.556));
#51303=CARTESIAN_POINT('',(-63.2683813778765,57.495,5.556));
#51304=CARTESIAN_POINT('',(-63.9072162302553,57.495,5.556));
#51305=CARTESIAN_POINT('',(-63.2683813778765,54.32,5.556));
#51306=CARTESIAN_POINT('Origin',(-62.6323433934964,54.32,7.3035));
#51307=CARTESIAN_POINT('',(-62.6323433934964,54.32,7.3035));
#51308=CARTESIAN_POINT('',(-63.2683813778765,54.32,5.556));
#51309=CARTESIAN_POINT('',(-62.6323433934964,57.495,7.3035));
#51310=CARTESIAN_POINT('',(-63.2683813778765,57.495,5.556));
#51311=CARTESIAN_POINT('',(-62.6323433934964,54.32,7.3035));
#51312=CARTESIAN_POINT('Origin',(-62.0496150458486,54.32,7.3035));
#51313=CARTESIAN_POINT('',(-62.0496150458486,54.32,7.3035));
#51314=CARTESIAN_POINT('',(-62.6323433934964,54.32,7.3035));
#51315=CARTESIAN_POINT('',(-62.0496150458486,57.495,7.3035));
#51316=CARTESIAN_POINT('',(-62.6323433934964,57.495,7.3035));
#51317=CARTESIAN_POINT('',(-62.0496150458486,54.32,7.3035));
#51318=CARTESIAN_POINT('Origin',(-61.4135770614684,54.32,5.556));
#51319=CARTESIAN_POINT('',(-61.4135770614684,54.32,5.556));
#51320=CARTESIAN_POINT('',(-62.0496150458486,54.32,7.3035));
#51321=CARTESIAN_POINT('',(-61.4135770614684,57.495,5.556));
#51322=CARTESIAN_POINT('',(-62.0496150458486,57.495,7.3035));
#51323=CARTESIAN_POINT('',(-61.4135770614684,54.32,5.556));
#51324=CARTESIAN_POINT('Origin',(-60.7747422090896,54.32,5.556));
#51325=CARTESIAN_POINT('',(-60.7747422090896,54.32,5.556));
#51326=CARTESIAN_POINT('',(-61.4135770614684,54.32,5.556));
#51327=CARTESIAN_POINT('',(-60.7747422090896,57.495,5.556));
#51328=CARTESIAN_POINT('',(-61.4135770614684,57.495,5.556));
#51329=CARTESIAN_POINT('',(-60.7747422090896,54.32,5.556));
#51330=CARTESIAN_POINT('Origin',(-60.1387042247095,54.32,7.3035));
#51331=CARTESIAN_POINT('',(-60.1387042247095,54.32,7.3035));
#51332=CARTESIAN_POINT('',(-60.7747422090896,54.32,5.556));
#51333=CARTESIAN_POINT('',(-60.1387042247095,57.495,7.3035));
#51334=CARTESIAN_POINT('',(-60.7747422090896,57.495,5.556));
#51335=CARTESIAN_POINT('',(-60.1387042247095,54.32,7.3035));
#51336=CARTESIAN_POINT('Origin',(-59.5559758770617,54.32,7.3035));
#51337=CARTESIAN_POINT('',(-59.5559758770617,54.32,7.3035));
#51338=CARTESIAN_POINT('',(-60.1387042247095,54.32,7.3035));
#51339=CARTESIAN_POINT('',(-59.5559758770617,57.495,7.3035));
#51340=CARTESIAN_POINT('',(-60.1387042247095,57.495,7.3035));
#51341=CARTESIAN_POINT('',(-59.5559758770617,54.32,7.3035));
#51342=CARTESIAN_POINT('Origin',(-58.9199378926815,54.32,5.556));
#51343=CARTESIAN_POINT('',(-58.9199378926815,54.32,5.556));
#51344=CARTESIAN_POINT('',(-59.5559758770617,54.32,7.3035));
#51345=CARTESIAN_POINT('',(-58.9199378926815,57.495,5.556));
#51346=CARTESIAN_POINT('',(-59.5559758770617,57.495,7.3035));
#51347=CARTESIAN_POINT('',(-58.9199378926815,54.32,5.556));
#51348=CARTESIAN_POINT('Origin',(-58.2811030403027,54.32,5.556));
#51349=CARTESIAN_POINT('',(-58.2811030403027,54.32,5.556));
#51350=CARTESIAN_POINT('',(-58.9199378926815,54.32,5.556));
#51351=CARTESIAN_POINT('',(-58.2811030403027,57.495,5.556));
#51352=CARTESIAN_POINT('',(-58.9199378926815,57.495,5.556));
#51353=CARTESIAN_POINT('',(-58.2811030403027,54.32,5.556));
#51354=CARTESIAN_POINT('Origin',(-57.6450650559226,54.32,7.3035));
#51355=CARTESIAN_POINT('',(-57.6450650559226,54.32,7.3035));
#51356=CARTESIAN_POINT('',(-58.2811030403027,54.32,5.556));
#51357=CARTESIAN_POINT('',(-57.6450650559226,57.495,7.3035));
#51358=CARTESIAN_POINT('',(-58.2811030403027,57.495,5.556));
#51359=CARTESIAN_POINT('',(-57.6450650559226,54.32,7.3035));
#51360=CARTESIAN_POINT('Origin',(-57.0623367082748,54.32,7.3035));
#51361=CARTESIAN_POINT('',(-57.0623367082748,54.32,7.3035));
#51362=CARTESIAN_POINT('',(-57.6450650559226,54.32,7.3035));
#51363=CARTESIAN_POINT('',(-57.0623367082748,57.495,7.3035));
#51364=CARTESIAN_POINT('',(-57.6450650559226,57.495,7.3035));
#51365=CARTESIAN_POINT('',(-57.0623367082748,54.32,7.3035));
#51366=CARTESIAN_POINT('Origin',(-56.4262987238946,54.32,5.556));
#51367=CARTESIAN_POINT('',(-56.4262987238946,54.32,5.556));
#51368=CARTESIAN_POINT('',(-57.0623367082748,54.32,7.3035));
#51369=CARTESIAN_POINT('',(-56.4262987238946,57.495,5.556));
#51370=CARTESIAN_POINT('',(-57.0623367082748,57.495,7.3035));
#51371=CARTESIAN_POINT('',(-56.4262987238946,54.32,5.556));
#51372=CARTESIAN_POINT('Origin',(-55.7874638715158,54.32,5.556));
#51373=CARTESIAN_POINT('',(-55.7874638715158,54.32,5.556));
#51374=CARTESIAN_POINT('',(-56.4262987238946,54.32,5.556));
#51375=CARTESIAN_POINT('',(-55.7874638715158,57.495,5.556));
#51376=CARTESIAN_POINT('',(-56.4262987238946,57.495,5.556));
#51377=CARTESIAN_POINT('',(-55.7874638715158,54.32,5.556));
#51378=CARTESIAN_POINT('Origin',(-55.1514258871357,54.32,7.3035));
#51379=CARTESIAN_POINT('',(-55.1514258871357,54.32,7.3035));
#51380=CARTESIAN_POINT('',(-55.7874638715158,54.32,5.556));
#51381=CARTESIAN_POINT('',(-55.1514258871357,57.495,7.3035));
#51382=CARTESIAN_POINT('',(-55.7874638715158,57.495,5.556));
#51383=CARTESIAN_POINT('',(-55.1514258871357,54.32,7.3035));
#51384=CARTESIAN_POINT('Origin',(-54.5686975394879,54.32,7.3035));
#51385=CARTESIAN_POINT('',(-54.5686975394879,54.32,7.3035));
#51386=CARTESIAN_POINT('',(-55.1514258871357,54.32,7.3035));
#51387=CARTESIAN_POINT('',(-54.5686975394879,57.495,7.3035));
#51388=CARTESIAN_POINT('',(-55.1514258871357,57.495,7.3035));
#51389=CARTESIAN_POINT('',(-54.5686975394879,54.32,7.3035));
#51390=CARTESIAN_POINT('Origin',(-53.9326595551077,54.32,5.556));
#51391=CARTESIAN_POINT('',(-53.9326595551077,54.32,5.556));
#51392=CARTESIAN_POINT('',(-54.5686975394879,54.32,7.3035));
#51393=CARTESIAN_POINT('',(-53.9326595551077,57.495,5.556));
#51394=CARTESIAN_POINT('',(-54.5686975394879,57.495,7.3035));
#51395=CARTESIAN_POINT('',(-53.9326595551077,54.32,5.556));
#51396=CARTESIAN_POINT('Origin',(-53.293824702729,54.32,5.556));
#51397=CARTESIAN_POINT('',(-53.293824702729,54.32,5.556));
#51398=CARTESIAN_POINT('',(-53.9326595551077,54.32,5.556));
#51399=CARTESIAN_POINT('',(-53.293824702729,57.495,5.556));
#51400=CARTESIAN_POINT('',(-53.9326595551077,57.495,5.556));
#51401=CARTESIAN_POINT('',(-53.293824702729,54.32,5.556));
#51402=CARTESIAN_POINT('Origin',(-52.6577867183488,54.32,7.3035));
#51403=CARTESIAN_POINT('',(-52.6577867183488,54.32,7.3035));
#51404=CARTESIAN_POINT('',(-53.293824702729,54.32,5.556));
#51405=CARTESIAN_POINT('',(-52.6577867183488,57.495,7.3035));
#51406=CARTESIAN_POINT('',(-53.293824702729,57.495,5.556));
#51407=CARTESIAN_POINT('',(-52.6577867183488,54.32,7.3035));
#51408=CARTESIAN_POINT('Origin',(-52.075058370701,54.32,7.3035));
#51409=CARTESIAN_POINT('',(-52.075058370701,54.32,7.3035));
#51410=CARTESIAN_POINT('',(-52.6577867183488,54.32,7.3035));
#51411=CARTESIAN_POINT('',(-52.075058370701,57.495,7.3035));
#51412=CARTESIAN_POINT('',(-52.6577867183488,57.495,7.3035));
#51413=CARTESIAN_POINT('',(-52.075058370701,54.32,7.3035));
#51414=CARTESIAN_POINT('Origin',(-51.4390203863208,54.32,5.556));
#51415=CARTESIAN_POINT('',(-51.4390203863208,54.32,5.556));
#51416=CARTESIAN_POINT('',(-52.075058370701,54.32,7.3035));
#51417=CARTESIAN_POINT('',(-51.4390203863208,57.495,5.556));
#51418=CARTESIAN_POINT('',(-52.075058370701,57.495,7.3035));
#51419=CARTESIAN_POINT('',(-51.4390203863208,54.32,5.556));
#51420=CARTESIAN_POINT('Origin',(-50.800185533942,54.32,5.556));
#51421=CARTESIAN_POINT('',(-50.800185533942,54.32,5.556));
#51422=CARTESIAN_POINT('',(-51.4390203863208,54.32,5.556));
#51423=CARTESIAN_POINT('',(-50.800185533942,57.495,5.556));
#51424=CARTESIAN_POINT('',(-51.4390203863208,57.495,5.556));
#51425=CARTESIAN_POINT('',(-50.800185533942,54.32,5.556));
#51426=CARTESIAN_POINT('Origin',(-50.1641475495619,54.32,7.3035));
#51427=CARTESIAN_POINT('',(-50.1641475495619,54.32,7.3035));
#51428=CARTESIAN_POINT('',(-50.800185533942,54.32,5.556));
#51429=CARTESIAN_POINT('',(-50.1641475495619,57.495,7.3035));
#51430=CARTESIAN_POINT('',(-50.800185533942,57.495,5.556));
#51431=CARTESIAN_POINT('',(-50.1641475495619,54.32,7.3035));
#51432=CARTESIAN_POINT('Origin',(-49.5814192019141,54.32,7.3035));
#51433=CARTESIAN_POINT('',(-49.5814192019141,54.32,7.3035));
#51434=CARTESIAN_POINT('',(-50.1641475495619,54.32,7.3035));
#51435=CARTESIAN_POINT('',(-49.5814192019141,57.495,7.3035));
#51436=CARTESIAN_POINT('',(-50.1641475495619,57.495,7.3035));
#51437=CARTESIAN_POINT('',(-49.5814192019141,54.32,7.3035));
#51438=CARTESIAN_POINT('Origin',(-48.9453812175339,54.32,5.556));
#51439=CARTESIAN_POINT('',(-48.9453812175339,54.32,5.556));
#51440=CARTESIAN_POINT('',(-49.5814192019141,54.32,7.3035));
#51441=CARTESIAN_POINT('',(-48.9453812175339,57.495,5.556));
#51442=CARTESIAN_POINT('',(-49.5814192019141,57.495,7.3035));
#51443=CARTESIAN_POINT('',(-48.9453812175339,54.32,5.556));
#51444=CARTESIAN_POINT('Origin',(-48.3065463651552,54.32,5.556));
#51445=CARTESIAN_POINT('',(-48.3065463651552,54.32,5.556));
#51446=CARTESIAN_POINT('',(-48.9453812175339,54.32,5.556));
#51447=CARTESIAN_POINT('',(-48.3065463651552,57.495,5.556));
#51448=CARTESIAN_POINT('',(-48.9453812175339,57.495,5.556));
#51449=CARTESIAN_POINT('',(-48.3065463651552,54.32,5.556));
#51450=CARTESIAN_POINT('Origin',(-47.670508380775,54.32,7.3035));
#51451=CARTESIAN_POINT('',(-47.670508380775,54.32,7.3035));
#51452=CARTESIAN_POINT('',(-48.3065463651552,54.32,5.556));
#51453=CARTESIAN_POINT('',(-47.670508380775,57.495,7.3035));
#51454=CARTESIAN_POINT('',(-48.3065463651552,57.495,5.556));
#51455=CARTESIAN_POINT('',(-47.670508380775,54.32,7.3035));
#51456=CARTESIAN_POINT('Origin',(-47.0877800331272,54.32,7.3035));
#51457=CARTESIAN_POINT('',(-47.0877800331272,54.32,7.3035));
#51458=CARTESIAN_POINT('',(-47.670508380775,54.32,7.3035));
#51459=CARTESIAN_POINT('',(-47.0877800331272,57.495,7.3035));
#51460=CARTESIAN_POINT('',(-47.670508380775,57.495,7.3035));
#51461=CARTESIAN_POINT('',(-47.0877800331272,54.32,7.3035));
#51462=CARTESIAN_POINT('Origin',(-46.451742048747,54.32,5.556));
#51463=CARTESIAN_POINT('',(-46.451742048747,54.32,5.556));
#51464=CARTESIAN_POINT('',(-47.0877800331272,54.32,7.3035));
#51465=CARTESIAN_POINT('',(-46.451742048747,57.495,5.556));
#51466=CARTESIAN_POINT('',(-47.0877800331272,57.495,7.3035));
#51467=CARTESIAN_POINT('',(-46.451742048747,54.32,5.556));
#51468=CARTESIAN_POINT('Origin',(-45.8129071963683,54.32,5.556));
#51469=CARTESIAN_POINT('',(-45.8129071963683,54.32,5.556));
#51470=CARTESIAN_POINT('',(-46.451742048747,54.32,5.556));
#51471=CARTESIAN_POINT('',(-45.8129071963683,57.495,5.556));
#51472=CARTESIAN_POINT('',(-46.451742048747,57.495,5.556));
#51473=CARTESIAN_POINT('',(-45.8129071963683,54.32,5.556));
#51474=CARTESIAN_POINT('Origin',(-45.1768692119881,54.32,7.3035));
#51475=CARTESIAN_POINT('',(-45.1768692119881,54.32,7.3035));
#51476=CARTESIAN_POINT('',(-45.8129071963683,54.32,5.556));
#51477=CARTESIAN_POINT('',(-45.1768692119881,57.495,7.3035));
#51478=CARTESIAN_POINT('',(-45.8129071963683,57.495,5.556));
#51479=CARTESIAN_POINT('',(-45.1768692119881,54.32,7.3035));
#51480=CARTESIAN_POINT('Origin',(-44.5941408643403,54.32,7.3035));
#51481=CARTESIAN_POINT('',(-44.5941408643403,54.32,7.3035));
#51482=CARTESIAN_POINT('',(-45.1768692119881,54.32,7.3035));
#51483=CARTESIAN_POINT('',(-44.5941408643403,57.495,7.3035));
#51484=CARTESIAN_POINT('',(-45.1768692119881,57.495,7.3035));
#51485=CARTESIAN_POINT('',(-44.5941408643403,54.32,7.3035));
#51486=CARTESIAN_POINT('Origin',(-43.9581028799601,54.32,5.556));
#51487=CARTESIAN_POINT('',(-43.9581028799601,54.32,5.556));
#51488=CARTESIAN_POINT('',(-44.5941408643403,54.32,7.3035));
#51489=CARTESIAN_POINT('',(-43.9581028799601,57.495,5.556));
#51490=CARTESIAN_POINT('',(-44.5941408643403,57.495,7.3035));
#51491=CARTESIAN_POINT('',(-43.9581028799601,54.32,5.556));
#51492=CARTESIAN_POINT('Origin',(-43.3192680275814,54.32,5.556));
#51493=CARTESIAN_POINT('',(-43.3192680275814,54.32,5.556));
#51494=CARTESIAN_POINT('',(-43.9581028799601,54.32,5.556));
#51495=CARTESIAN_POINT('',(-43.3192680275814,57.495,5.556));
#51496=CARTESIAN_POINT('',(-43.9581028799601,57.495,5.556));
#51497=CARTESIAN_POINT('',(-43.3192680275814,54.32,5.556));
#51498=CARTESIAN_POINT('Origin',(-42.6832300432012,54.32,7.3035));
#51499=CARTESIAN_POINT('',(-42.6832300432012,54.32,7.3035));
#51500=CARTESIAN_POINT('',(-43.3192680275814,54.32,5.556));
#51501=CARTESIAN_POINT('',(-42.6832300432012,57.495,7.3035));
#51502=CARTESIAN_POINT('',(-43.3192680275814,57.495,5.556));
#51503=CARTESIAN_POINT('',(-42.6832300432012,54.32,7.3035));
#51504=CARTESIAN_POINT('Origin',(-42.1005016955534,54.32,7.3035));
#51505=CARTESIAN_POINT('',(-42.1005016955534,54.32,7.3035));
#51506=CARTESIAN_POINT('',(-42.6832300432012,54.32,7.3035));
#51507=CARTESIAN_POINT('',(-42.1005016955534,57.495,7.3035));
#51508=CARTESIAN_POINT('',(-42.6832300432012,57.495,7.3035));
#51509=CARTESIAN_POINT('',(-42.1005016955534,54.32,7.3035));
#51510=CARTESIAN_POINT('Origin',(-41.4644637111732,54.32,5.556));
#51511=CARTESIAN_POINT('',(-41.4644637111732,54.32,5.556));
#51512=CARTESIAN_POINT('',(-42.1005016955534,54.32,7.3035));
#51513=CARTESIAN_POINT('',(-41.4644637111732,57.495,5.556));
#51514=CARTESIAN_POINT('',(-42.1005016955534,57.495,7.3035));
#51515=CARTESIAN_POINT('',(-41.4644637111732,54.32,5.556));
#51516=CARTESIAN_POINT('Origin',(-40.8256288587945,54.32,5.556));
#51517=CARTESIAN_POINT('',(-40.8256288587945,54.32,5.556));
#51518=CARTESIAN_POINT('',(-41.4644637111732,54.32,5.556));
#51519=CARTESIAN_POINT('',(-40.8256288587945,57.495,5.556));
#51520=CARTESIAN_POINT('',(-41.4644637111732,57.495,5.556));
#51521=CARTESIAN_POINT('',(-40.8256288587945,54.32,5.556));
#51522=CARTESIAN_POINT('Origin',(-40.1895908744143,54.32,7.3035));
#51523=CARTESIAN_POINT('',(-40.1895908744143,54.32,7.3035));
#51524=CARTESIAN_POINT('',(-40.8256288587945,54.32,5.556));
#51525=CARTESIAN_POINT('',(-40.1895908744143,57.495,7.3035));
#51526=CARTESIAN_POINT('',(-40.8256288587945,57.495,5.556));
#51527=CARTESIAN_POINT('',(-40.1895908744143,54.32,7.3035));
#51528=CARTESIAN_POINT('Origin',(-39.6068625267665,54.32,7.3035));
#51529=CARTESIAN_POINT('',(-39.6068625267665,54.32,7.3035));
#51530=CARTESIAN_POINT('',(-40.1895908744143,54.32,7.3035));
#51531=CARTESIAN_POINT('',(-39.6068625267665,57.495,7.3035));
#51532=CARTESIAN_POINT('',(-40.1895908744143,57.495,7.3035));
#51533=CARTESIAN_POINT('',(-39.6068625267665,54.32,7.3035));
#51534=CARTESIAN_POINT('Origin',(-38.9708245423863,54.32,5.556));
#51535=CARTESIAN_POINT('',(-38.9708245423863,54.32,5.556));
#51536=CARTESIAN_POINT('',(-39.6068625267665,54.32,7.3035));
#51537=CARTESIAN_POINT('',(-38.9708245423863,57.495,5.556));
#51538=CARTESIAN_POINT('',(-39.6068625267665,57.495,7.3035));
#51539=CARTESIAN_POINT('',(-38.9708245423863,54.32,5.556));
#51540=CARTESIAN_POINT('Origin',(-38.3319896900076,54.32,5.556));
#51541=CARTESIAN_POINT('',(-38.3319896900076,54.32,5.556));
#51542=CARTESIAN_POINT('',(-38.9708245423863,54.32,5.556));
#51543=CARTESIAN_POINT('',(-38.3319896900076,57.495,5.556));
#51544=CARTESIAN_POINT('',(-38.9708245423863,57.495,5.556));
#51545=CARTESIAN_POINT('',(-38.3319896900076,54.32,5.556));
#51546=CARTESIAN_POINT('Origin',(-37.6959517056274,54.32,7.3035));
#51547=CARTESIAN_POINT('',(-37.6959517056274,54.32,7.3035));
#51548=CARTESIAN_POINT('',(-38.3319896900076,54.32,5.556));
#51549=CARTESIAN_POINT('',(-37.6959517056274,57.495,7.3035));
#51550=CARTESIAN_POINT('',(-38.3319896900076,57.495,5.556));
#51551=CARTESIAN_POINT('',(-37.6959517056274,54.32,7.3035));
#51552=CARTESIAN_POINT('Origin',(-37.1132233579796,54.32,7.3035));
#51553=CARTESIAN_POINT('',(-37.1132233579796,54.32,7.3035));
#51554=CARTESIAN_POINT('',(-37.6959517056274,54.32,7.3035));
#51555=CARTESIAN_POINT('',(-37.1132233579796,57.495,7.3035));
#51556=CARTESIAN_POINT('',(-37.6959517056274,57.495,7.3035));
#51557=CARTESIAN_POINT('',(-37.1132233579796,54.32,7.3035));
#51558=CARTESIAN_POINT('Origin',(-36.4771853735994,54.32,5.556));
#51559=CARTESIAN_POINT('',(-36.4771853735994,54.32,5.556));
#51560=CARTESIAN_POINT('',(-37.1132233579796,54.32,7.3035));
#51561=CARTESIAN_POINT('',(-36.4771853735994,57.495,5.556));
#51562=CARTESIAN_POINT('',(-37.1132233579796,57.495,7.3035));
#51563=CARTESIAN_POINT('',(-36.4771853735994,54.32,5.556));
#51564=CARTESIAN_POINT('Origin',(-35.8383505212207,54.32,5.556));
#51565=CARTESIAN_POINT('',(-35.8383505212207,54.32,5.556));
#51566=CARTESIAN_POINT('',(-36.4771853735994,54.32,5.556));
#51567=CARTESIAN_POINT('',(-35.8383505212207,57.495,5.556));
#51568=CARTESIAN_POINT('',(-36.4771853735994,57.495,5.556));
#51569=CARTESIAN_POINT('',(-35.8383505212207,54.32,5.556));
#51570=CARTESIAN_POINT('Origin',(-35.2023125368405,54.32,7.3035));
#51571=CARTESIAN_POINT('',(-35.2023125368405,54.32,7.3035));
#51572=CARTESIAN_POINT('',(-35.8383505212207,54.32,5.556));
#51573=CARTESIAN_POINT('',(-35.2023125368405,57.495,7.3035));
#51574=CARTESIAN_POINT('',(-35.8383505212207,57.495,5.556));
#51575=CARTESIAN_POINT('',(-35.2023125368405,54.32,7.3035));
#51576=CARTESIAN_POINT('Origin',(-34.6195841891927,54.32,7.3035));
#51577=CARTESIAN_POINT('',(-34.6195841891927,54.32,7.3035));
#51578=CARTESIAN_POINT('',(-35.2023125368405,54.32,7.3035));
#51579=CARTESIAN_POINT('',(-34.6195841891927,57.495,7.3035));
#51580=CARTESIAN_POINT('',(-35.2023125368405,57.495,7.3035));
#51581=CARTESIAN_POINT('',(-34.6195841891927,54.32,7.3035));
#51582=CARTESIAN_POINT('Origin',(-33.9835462048125,54.32,5.556));
#51583=CARTESIAN_POINT('',(-33.9835462048125,54.32,5.556));
#51584=CARTESIAN_POINT('',(-34.6195841891927,54.32,7.3035));
#51585=CARTESIAN_POINT('',(-33.9835462048125,57.495,5.556));
#51586=CARTESIAN_POINT('',(-34.6195841891927,57.495,7.3035));
#51587=CARTESIAN_POINT('',(-33.9835462048125,54.32,5.556));
#51588=CARTESIAN_POINT('Origin',(-33.3447113524338,54.32,5.556));
#51589=CARTESIAN_POINT('',(-33.3447113524338,54.32,5.556));
#51590=CARTESIAN_POINT('',(-33.9835462048125,54.32,5.556));
#51591=CARTESIAN_POINT('',(-33.3447113524338,57.495,5.556));
#51592=CARTESIAN_POINT('',(-33.9835462048125,57.495,5.556));
#51593=CARTESIAN_POINT('',(-33.3447113524338,54.32,5.556));
#51594=CARTESIAN_POINT('Origin',(-32.7086733680536,54.32,7.3035));
#51595=CARTESIAN_POINT('',(-32.7086733680536,54.32,7.3035));
#51596=CARTESIAN_POINT('',(-33.3447113524338,54.32,5.556));
#51597=CARTESIAN_POINT('',(-32.7086733680536,57.495,7.3035));
#51598=CARTESIAN_POINT('',(-33.3447113524338,57.495,5.556));
#51599=CARTESIAN_POINT('',(-32.7086733680536,54.32,7.3035));
#51600=CARTESIAN_POINT('Origin',(-32.1259450204058,54.32,7.3035));
#51601=CARTESIAN_POINT('',(-32.1259450204058,54.32,7.3035));
#51602=CARTESIAN_POINT('',(-32.7086733680536,54.32,7.3035));
#51603=CARTESIAN_POINT('',(-32.1259450204058,57.495,7.3035));
#51604=CARTESIAN_POINT('',(-32.7086733680536,57.495,7.3035));
#51605=CARTESIAN_POINT('',(-32.1259450204058,54.32,7.3035));
#51606=CARTESIAN_POINT('Origin',(-31.4899070360256,54.32,5.556));
#51607=CARTESIAN_POINT('',(-31.4899070360256,54.32,5.556));
#51608=CARTESIAN_POINT('',(-32.1259450204058,54.32,7.3035));
#51609=CARTESIAN_POINT('',(-31.4899070360256,57.495,5.556));
#51610=CARTESIAN_POINT('',(-32.1259450204058,57.495,7.3035));
#51611=CARTESIAN_POINT('',(-31.4899070360256,54.32,5.556));
#51612=CARTESIAN_POINT('Origin',(-30.8510721836469,54.32,5.556));
#51613=CARTESIAN_POINT('',(-30.8510721836469,54.32,5.556));
#51614=CARTESIAN_POINT('',(-31.4899070360256,54.32,5.556));
#51615=CARTESIAN_POINT('',(-30.8510721836469,57.495,5.556));
#51616=CARTESIAN_POINT('',(-31.4899070360256,57.495,5.556));
#51617=CARTESIAN_POINT('',(-30.8510721836469,54.32,5.556));
#51618=CARTESIAN_POINT('Origin',(-30.2150341992667,54.32,7.3035));
#51619=CARTESIAN_POINT('',(-30.2150341992667,54.32,7.3035));
#51620=CARTESIAN_POINT('',(-30.8510721836469,54.32,5.556));
#51621=CARTESIAN_POINT('',(-30.2150341992667,57.495,7.3035));
#51622=CARTESIAN_POINT('',(-30.8510721836469,57.495,5.556));
#51623=CARTESIAN_POINT('',(-30.2150341992667,54.32,7.3035));
#51624=CARTESIAN_POINT('Origin',(-29.6323058516189,54.32,7.3035));
#51625=CARTESIAN_POINT('',(-29.6323058516189,54.32,7.3035));
#51626=CARTESIAN_POINT('',(-30.2150341992667,54.32,7.3035));
#51627=CARTESIAN_POINT('',(-29.6323058516189,57.495,7.3035));
#51628=CARTESIAN_POINT('',(-30.2150341992667,57.495,7.3035));
#51629=CARTESIAN_POINT('',(-29.6323058516189,54.32,7.3035));
#51630=CARTESIAN_POINT('Origin',(-28.9962678672387,54.32,5.556));
#51631=CARTESIAN_POINT('',(-28.9962678672387,54.32,5.556));
#51632=CARTESIAN_POINT('',(-29.6323058516189,54.32,7.3035));
#51633=CARTESIAN_POINT('',(-28.9962678672387,57.495,5.556));
#51634=CARTESIAN_POINT('',(-29.6323058516189,57.495,7.3035));
#51635=CARTESIAN_POINT('',(-28.9962678672387,54.32,5.556));
#51636=CARTESIAN_POINT('Origin',(-28.35743301486,54.32,5.556));
#51637=CARTESIAN_POINT('',(-28.35743301486,54.32,5.556));
#51638=CARTESIAN_POINT('',(-28.9962678672387,54.32,5.556));
#51639=CARTESIAN_POINT('',(-28.35743301486,57.495,5.556));
#51640=CARTESIAN_POINT('',(-28.9962678672387,57.495,5.556));
#51641=CARTESIAN_POINT('',(-28.35743301486,54.32,5.556));
#51642=CARTESIAN_POINT('Origin',(-27.7213950304798,54.32,7.3035));
#51643=CARTESIAN_POINT('',(-27.7213950304798,54.32,7.3035));
#51644=CARTESIAN_POINT('',(-28.35743301486,54.32,5.556));
#51645=CARTESIAN_POINT('',(-27.7213950304798,57.495,7.3035));
#51646=CARTESIAN_POINT('',(-28.35743301486,57.495,5.556));
#51647=CARTESIAN_POINT('',(-27.7213950304798,54.32,7.3035));
#51648=CARTESIAN_POINT('Origin',(-27.138666682832,54.32,7.3035));
#51649=CARTESIAN_POINT('',(-27.138666682832,54.32,7.3035));
#51650=CARTESIAN_POINT('',(-27.7213950304798,54.32,7.3035));
#51651=CARTESIAN_POINT('',(-27.138666682832,57.495,7.3035));
#51652=CARTESIAN_POINT('',(-27.7213950304798,57.495,7.3035));
#51653=CARTESIAN_POINT('',(-27.138666682832,54.32,7.3035));
#51654=CARTESIAN_POINT('Origin',(-26.5026286984518,54.32,5.556));
#51655=CARTESIAN_POINT('',(-26.5026286984518,54.32,5.556));
#51656=CARTESIAN_POINT('',(-27.138666682832,54.32,7.3035));
#51657=CARTESIAN_POINT('',(-26.5026286984518,57.495,5.556));
#51658=CARTESIAN_POINT('',(-27.138666682832,57.495,7.3035));
#51659=CARTESIAN_POINT('',(-26.5026286984518,54.32,5.556));
#51660=CARTESIAN_POINT('Origin',(-25.8637938460731,54.32,5.556));
#51661=CARTESIAN_POINT('',(-25.8637938460731,54.32,5.556));
#51662=CARTESIAN_POINT('',(-26.5026286984518,54.32,5.556));
#51663=CARTESIAN_POINT('',(-25.8637938460731,57.495,5.556));
#51664=CARTESIAN_POINT('',(-26.5026286984518,57.495,5.556));
#51665=CARTESIAN_POINT('',(-25.8637938460731,54.32,5.556));
#51666=CARTESIAN_POINT('Origin',(-25.2277558616929,54.32,7.3035));
#51667=CARTESIAN_POINT('',(-25.2277558616929,54.32,7.3035));
#51668=CARTESIAN_POINT('',(-25.8637938460731,54.32,5.556));
#51669=CARTESIAN_POINT('',(-25.2277558616929,57.495,7.3035));
#51670=CARTESIAN_POINT('',(-25.8637938460731,57.495,5.556));
#51671=CARTESIAN_POINT('',(-25.2277558616929,54.32,7.3035));
#51672=CARTESIAN_POINT('Origin',(-24.6450275140451,54.32,7.3035));
#51673=CARTESIAN_POINT('',(-24.6450275140451,54.32,7.3035));
#51674=CARTESIAN_POINT('',(-25.2277558616929,54.32,7.3035));
#51675=CARTESIAN_POINT('',(-24.6450275140451,57.495,7.3035));
#51676=CARTESIAN_POINT('',(-25.2277558616929,57.495,7.3035));
#51677=CARTESIAN_POINT('',(-24.6450275140451,54.32,7.3035));
#51678=CARTESIAN_POINT('Origin',(-24.0089895296649,54.32,5.556));
#51679=CARTESIAN_POINT('',(-24.0089895296649,54.32,5.556));
#51680=CARTESIAN_POINT('',(-24.6450275140451,54.32,7.3035));
#51681=CARTESIAN_POINT('',(-24.0089895296649,57.495,5.556));
#51682=CARTESIAN_POINT('',(-24.6450275140451,57.495,7.3035));
#51683=CARTESIAN_POINT('',(-24.0089895296649,54.32,5.556));
#51684=CARTESIAN_POINT('Origin',(-23.3701546772862,54.32,5.556));
#51685=CARTESIAN_POINT('',(-23.3701546772862,54.32,5.556));
#51686=CARTESIAN_POINT('',(-24.0089895296649,54.32,5.556));
#51687=CARTESIAN_POINT('',(-23.3701546772862,57.495,5.556));
#51688=CARTESIAN_POINT('',(-24.0089895296649,57.495,5.556));
#51689=CARTESIAN_POINT('',(-23.3701546772862,54.32,5.556));
#51690=CARTESIAN_POINT('Origin',(-22.734116692906,54.32,7.3035));
#51691=CARTESIAN_POINT('',(-22.734116692906,54.32,7.3035));
#51692=CARTESIAN_POINT('',(-23.3701546772862,54.32,5.556));
#51693=CARTESIAN_POINT('',(-22.734116692906,57.495,7.3035));
#51694=CARTESIAN_POINT('',(-23.3701546772862,57.495,5.556));
#51695=CARTESIAN_POINT('',(-22.734116692906,54.32,7.3035));
#51696=CARTESIAN_POINT('Origin',(-22.1513883452582,54.32,7.3035));
#51697=CARTESIAN_POINT('',(-22.1513883452582,54.32,7.3035));
#51698=CARTESIAN_POINT('',(-22.734116692906,54.32,7.3035));
#51699=CARTESIAN_POINT('',(-22.1513883452582,57.495,7.3035));
#51700=CARTESIAN_POINT('',(-22.734116692906,57.495,7.3035));
#51701=CARTESIAN_POINT('',(-22.1513883452582,54.32,7.3035));
#51702=CARTESIAN_POINT('Origin',(-21.515350360878,54.32,5.556));
#51703=CARTESIAN_POINT('',(-21.515350360878,54.32,5.556));
#51704=CARTESIAN_POINT('',(-22.1513883452582,54.32,7.3035));
#51705=CARTESIAN_POINT('',(-21.515350360878,57.495,5.556));
#51706=CARTESIAN_POINT('',(-22.1513883452582,57.495,7.3035));
#51707=CARTESIAN_POINT('',(-21.515350360878,54.32,5.556));
#51708=CARTESIAN_POINT('Origin',(-20.8765155084993,54.32,5.556));
#51709=CARTESIAN_POINT('',(-20.8765155084993,54.32,5.556));
#51710=CARTESIAN_POINT('',(-21.515350360878,54.32,5.556));
#51711=CARTESIAN_POINT('',(-20.8765155084993,57.495,5.556));
#51712=CARTESIAN_POINT('',(-21.515350360878,57.495,5.556));
#51713=CARTESIAN_POINT('',(-20.8765155084993,54.32,5.556));
#51714=CARTESIAN_POINT('Origin',(-20.2404775241191,54.32,7.3035));
#51715=CARTESIAN_POINT('',(-20.2404775241191,54.32,7.3035));
#51716=CARTESIAN_POINT('',(-20.8765155084993,54.32,5.556));
#51717=CARTESIAN_POINT('',(-20.2404775241191,57.495,7.3035));
#51718=CARTESIAN_POINT('',(-20.8765155084993,57.495,5.556));
#51719=CARTESIAN_POINT('',(-20.2404775241191,54.32,7.3035));
#51720=CARTESIAN_POINT('Origin',(-19.6577491764713,54.32,7.3035));
#51721=CARTESIAN_POINT('',(-19.6577491764713,54.32,7.3035));
#51722=CARTESIAN_POINT('',(-20.2404775241191,54.32,7.3035));
#51723=CARTESIAN_POINT('',(-19.6577491764713,57.495,7.3035));
#51724=CARTESIAN_POINT('',(-20.2404775241191,57.495,7.3035));
#51725=CARTESIAN_POINT('',(-19.6577491764713,54.32,7.3035));
#51726=CARTESIAN_POINT('Origin',(-19.0217111920911,54.32,5.556));
#51727=CARTESIAN_POINT('',(-19.0217111920911,54.32,5.556));
#51728=CARTESIAN_POINT('',(-19.6577491764713,54.32,7.3035));
#51729=CARTESIAN_POINT('',(-19.0217111920911,57.495,5.556));
#51730=CARTESIAN_POINT('',(-19.6577491764713,57.495,7.3035));
#51731=CARTESIAN_POINT('',(-19.0217111920911,54.32,5.556));
#51732=CARTESIAN_POINT('Origin',(-18.3828763397124,54.32,5.556));
#51733=CARTESIAN_POINT('',(-18.3828763397124,54.32,5.556));
#51734=CARTESIAN_POINT('',(-19.0217111920911,54.32,5.556));
#51735=CARTESIAN_POINT('',(-18.3828763397124,57.495,5.556));
#51736=CARTESIAN_POINT('',(-19.0217111920911,57.495,5.556));
#51737=CARTESIAN_POINT('',(-18.3828763397124,54.32,5.556));
#51738=CARTESIAN_POINT('Origin',(-17.7468383553322,54.32,7.3035));
#51739=CARTESIAN_POINT('',(-17.7468383553322,54.32,7.3035));
#51740=CARTESIAN_POINT('',(-18.3828763397124,54.32,5.556));
#51741=CARTESIAN_POINT('',(-17.7468383553322,57.495,7.3035));
#51742=CARTESIAN_POINT('',(-18.3828763397124,57.495,5.556));
#51743=CARTESIAN_POINT('',(-17.7468383553322,54.32,7.3035));
#51744=CARTESIAN_POINT('Origin',(-17.1641100076844,54.32,7.3035));
#51745=CARTESIAN_POINT('',(-17.1641100076844,54.32,7.3035));
#51746=CARTESIAN_POINT('',(-17.7468383553322,54.32,7.3035));
#51747=CARTESIAN_POINT('',(-17.1641100076844,57.495,7.3035));
#51748=CARTESIAN_POINT('',(-17.7468383553322,57.495,7.3035));
#51749=CARTESIAN_POINT('',(-17.1641100076844,54.32,7.3035));
#51750=CARTESIAN_POINT('Origin',(-16.5280720233042,54.32,5.556));
#51751=CARTESIAN_POINT('',(-16.5280720233042,54.32,5.556));
#51752=CARTESIAN_POINT('',(-17.1641100076844,54.32,7.3035));
#51753=CARTESIAN_POINT('',(-16.5280720233042,57.495,5.556));
#51754=CARTESIAN_POINT('',(-17.1641100076844,57.495,7.3035));
#51755=CARTESIAN_POINT('',(-16.5280720233042,54.32,5.556));
#51756=CARTESIAN_POINT('Origin',(-15.8892371709255,54.32,5.556));
#51757=CARTESIAN_POINT('',(-15.8892371709255,54.32,5.556));
#51758=CARTESIAN_POINT('',(-16.5280720233042,54.32,5.556));
#51759=CARTESIAN_POINT('',(-15.8892371709255,57.495,5.556));
#51760=CARTESIAN_POINT('',(-16.5280720233042,57.495,5.556));
#51761=CARTESIAN_POINT('',(-15.8892371709255,54.32,5.556));
#51762=CARTESIAN_POINT('Origin',(-15.2531991865453,54.32,7.3035));
#51763=CARTESIAN_POINT('',(-15.2531991865453,54.32,7.3035));
#51764=CARTESIAN_POINT('',(-15.8892371709255,54.32,5.556));
#51765=CARTESIAN_POINT('',(-15.2531991865453,57.495,7.3035));
#51766=CARTESIAN_POINT('',(-15.8892371709255,57.495,5.556));
#51767=CARTESIAN_POINT('',(-15.2531991865453,54.32,7.3035));
#51768=CARTESIAN_POINT('Origin',(-14.6704708388975,54.32,7.3035));
#51769=CARTESIAN_POINT('',(-14.6704708388975,54.32,7.3035));
#51770=CARTESIAN_POINT('',(-15.2531991865453,54.32,7.3035));
#51771=CARTESIAN_POINT('',(-14.6704708388975,57.495,7.3035));
#51772=CARTESIAN_POINT('',(-15.2531991865453,57.495,7.3035));
#51773=CARTESIAN_POINT('',(-14.6704708388975,54.32,7.3035));
#51774=CARTESIAN_POINT('Origin',(-14.0344328545173,54.32,5.556));
#51775=CARTESIAN_POINT('',(-14.0344328545173,54.32,5.556));
#51776=CARTESIAN_POINT('',(-14.6704708388975,54.32,7.3035));
#51777=CARTESIAN_POINT('',(-14.0344328545173,57.495,5.556));
#51778=CARTESIAN_POINT('',(-14.6704708388975,57.495,7.3035));
#51779=CARTESIAN_POINT('',(-14.0344328545173,54.32,5.556));
#51780=CARTESIAN_POINT('Origin',(-13.3955980021386,54.32,5.556));
#51781=CARTESIAN_POINT('',(-13.3955980021386,54.32,5.556));
#51782=CARTESIAN_POINT('',(-14.0344328545173,54.32,5.556));
#51783=CARTESIAN_POINT('',(-13.3955980021386,57.495,5.556));
#51784=CARTESIAN_POINT('',(-14.0344328545173,57.495,5.556));
#51785=CARTESIAN_POINT('',(-13.3955980021386,54.32,5.556));
#51786=CARTESIAN_POINT('Origin',(-12.7595600177584,54.32,7.3035));
#51787=CARTESIAN_POINT('',(-12.7595600177584,54.32,7.3035));
#51788=CARTESIAN_POINT('',(-13.3955980021386,54.32,5.556));
#51789=CARTESIAN_POINT('',(-12.7595600177584,57.495,7.3035));
#51790=CARTESIAN_POINT('',(-13.3955980021386,57.495,5.556));
#51791=CARTESIAN_POINT('',(-12.7595600177584,54.32,7.3035));
#51792=CARTESIAN_POINT('Origin',(-12.1768316701106,54.32,7.3035));
#51793=CARTESIAN_POINT('',(-12.1768316701106,54.32,7.3035));
#51794=CARTESIAN_POINT('',(-12.7595600177584,54.32,7.3035));
#51795=CARTESIAN_POINT('',(-12.1768316701106,57.495,7.3035));
#51796=CARTESIAN_POINT('',(-12.7595600177584,57.495,7.3035));
#51797=CARTESIAN_POINT('',(-12.1768316701106,54.32,7.3035));
#51798=CARTESIAN_POINT('Origin',(-11.5407936857304,54.32,5.556));
#51799=CARTESIAN_POINT('',(-11.5407936857304,54.32,5.556));
#51800=CARTESIAN_POINT('',(-12.1768316701106,54.32,7.3035));
#51801=CARTESIAN_POINT('',(-11.5407936857304,57.495,5.556));
#51802=CARTESIAN_POINT('',(-12.1768316701106,57.495,7.3035));
#51803=CARTESIAN_POINT('',(-11.5407936857304,54.32,5.556));
#51804=CARTESIAN_POINT('Origin',(-10.9019588333517,54.32,5.556));
#51805=CARTESIAN_POINT('',(-10.9019588333517,54.32,5.556));
#51806=CARTESIAN_POINT('',(-11.5407936857304,54.32,5.556));
#51807=CARTESIAN_POINT('',(-10.9019588333517,57.495,5.556));
#51808=CARTESIAN_POINT('',(-11.5407936857304,57.495,5.556));
#51809=CARTESIAN_POINT('',(-10.9019588333517,54.32,5.556));
#51810=CARTESIAN_POINT('Origin',(-10.2659208489715,54.32,7.3035));
#51811=CARTESIAN_POINT('',(-10.2659208489715,54.32,7.3035));
#51812=CARTESIAN_POINT('',(-10.9019588333517,54.32,5.556));
#51813=CARTESIAN_POINT('',(-10.2659208489715,57.495,7.3035));
#51814=CARTESIAN_POINT('',(-10.9019588333517,57.495,5.556));
#51815=CARTESIAN_POINT('',(-10.2659208489715,54.32,7.3035));
#51816=CARTESIAN_POINT('Origin',(-9.68319250132369,54.32,7.3035));
#51817=CARTESIAN_POINT('',(-9.68319250132369,54.32,7.3035));
#51818=CARTESIAN_POINT('',(-10.2659208489715,54.32,7.3035));
#51819=CARTESIAN_POINT('',(-9.68319250132369,57.495,7.3035));
#51820=CARTESIAN_POINT('',(-10.2659208489715,57.495,7.3035));
#51821=CARTESIAN_POINT('',(-9.68319250132369,54.32,7.3035));
#51822=CARTESIAN_POINT('Origin',(-9.0471545169435,54.32,5.556));
#51823=CARTESIAN_POINT('',(-9.0471545169435,54.32,5.556));
#51824=CARTESIAN_POINT('',(-9.68319250132369,54.32,7.3035));
#51825=CARTESIAN_POINT('',(-9.0471545169435,57.495,5.556));
#51826=CARTESIAN_POINT('',(-9.68319250132369,57.495,7.3035));
#51827=CARTESIAN_POINT('',(-9.0471545169435,54.32,5.556));
#51828=CARTESIAN_POINT('Origin',(-8.40831966456478,54.32,5.556));
#51829=CARTESIAN_POINT('',(-8.40831966456478,54.32,5.556));
#51830=CARTESIAN_POINT('',(-9.0471545169435,54.32,5.556));
#51831=CARTESIAN_POINT('',(-8.40831966456478,57.495,5.556));
#51832=CARTESIAN_POINT('',(-9.0471545169435,57.495,5.556));
#51833=CARTESIAN_POINT('',(-8.40831966456478,54.32,5.556));
#51834=CARTESIAN_POINT('Origin',(-7.7722816801846,54.32,7.3035));
#51835=CARTESIAN_POINT('',(-7.7722816801846,54.32,7.3035));
#51836=CARTESIAN_POINT('',(-8.40831966456478,54.32,5.556));
#51837=CARTESIAN_POINT('',(-7.77228168018459,57.495,7.3035));
#51838=CARTESIAN_POINT('',(-8.40831966456478,57.495,5.556));
#51839=CARTESIAN_POINT('',(-7.7722816801846,54.32,7.3035));
#51840=CARTESIAN_POINT('Origin',(-7.18955333253679,54.32,7.3035));
#51841=CARTESIAN_POINT('',(-7.18955333253679,54.32,7.3035));
#51842=CARTESIAN_POINT('',(-7.7722816801846,54.32,7.3035));
#51843=CARTESIAN_POINT('',(-7.1895533325368,57.495,7.3035));
#51844=CARTESIAN_POINT('',(-7.7722816801846,57.495,7.3035));
#51845=CARTESIAN_POINT('',(-7.18955333253679,54.32,7.3035));
#51846=CARTESIAN_POINT('Origin',(-6.55351534815661,54.32,5.556));
#51847=CARTESIAN_POINT('',(-6.55351534815661,54.32,5.556));
#51848=CARTESIAN_POINT('',(-7.18955333253679,54.32,7.3035));
#51849=CARTESIAN_POINT('',(-6.5535153481566,57.495,5.556));
#51850=CARTESIAN_POINT('',(-7.18955333253679,57.495,7.3035));
#51851=CARTESIAN_POINT('',(-6.55351534815661,54.32,5.556));
#51852=CARTESIAN_POINT('Origin',(-5.91468049577789,54.32,5.556));
#51853=CARTESIAN_POINT('',(-5.91468049577789,54.32,5.556));
#51854=CARTESIAN_POINT('',(-6.55351534815661,54.32,5.556));
#51855=CARTESIAN_POINT('',(-5.91468049577788,57.495,5.556));
#51856=CARTESIAN_POINT('',(-6.55351534815661,57.495,5.556));
#51857=CARTESIAN_POINT('',(-5.91468049577789,54.32,5.556));
#51858=CARTESIAN_POINT('Origin',(-5.2786425113977,54.32,7.3035));
#51859=CARTESIAN_POINT('',(-5.2786425113977,54.32,7.3035));
#51860=CARTESIAN_POINT('',(-5.91468049577789,54.32,5.556));
#51861=CARTESIAN_POINT('',(-5.2786425113977,57.495,7.3035));
#51862=CARTESIAN_POINT('',(-5.91468049577789,57.495,5.556));
#51863=CARTESIAN_POINT('',(-5.2786425113977,54.32,7.3035));
#51864=CARTESIAN_POINT('Origin',(-4.6959141637499,54.32,7.3035));
#51865=CARTESIAN_POINT('',(-4.6959141637499,54.32,7.3035));
#51866=CARTESIAN_POINT('',(-5.2786425113977,54.32,7.3035));
#51867=CARTESIAN_POINT('',(-4.69591416374989,57.495,7.3035));
#51868=CARTESIAN_POINT('',(-5.2786425113977,57.495,7.3035));
#51869=CARTESIAN_POINT('',(-4.6959141637499,54.32,7.3035));
#51870=CARTESIAN_POINT('Origin',(-4.05987617936971,54.32,5.556));
#51871=CARTESIAN_POINT('',(-4.05987617936971,54.32,5.556));
#51872=CARTESIAN_POINT('',(-4.6959141637499,54.32,7.3035));
#51873=CARTESIAN_POINT('',(-4.05987617936971,57.495,5.556));
#51874=CARTESIAN_POINT('',(-4.6959141637499,57.495,7.3035));
#51875=CARTESIAN_POINT('',(-4.05987617936971,54.32,5.556));
#51876=CARTESIAN_POINT('Origin',(-3.42104132699099,54.32,5.556));
#51877=CARTESIAN_POINT('',(-3.42104132699099,54.32,5.556));
#51878=CARTESIAN_POINT('',(-4.05987617936971,54.32,5.556));
#51879=CARTESIAN_POINT('',(-3.42104132699099,57.495,5.556));
#51880=CARTESIAN_POINT('',(-4.05987617936971,57.495,5.556));
#51881=CARTESIAN_POINT('',(-3.42104132699099,54.32,5.556));
#51882=CARTESIAN_POINT('Origin',(-2.7850033426108,54.32,7.3035));
#51883=CARTESIAN_POINT('',(-2.7850033426108,54.32,7.3035));
#51884=CARTESIAN_POINT('',(-3.42104132699099,54.32,5.556));
#51885=CARTESIAN_POINT('',(-2.7850033426108,57.495,7.3035));
#51886=CARTESIAN_POINT('',(-3.42104132699099,57.495,5.556));
#51887=CARTESIAN_POINT('',(-2.7850033426108,54.32,7.3035));
#51888=CARTESIAN_POINT('Origin',(-2.202274994963,54.32,7.3035));
#51889=CARTESIAN_POINT('',(-2.202274994963,54.32,7.3035));
#51890=CARTESIAN_POINT('',(-2.7850033426108,54.32,7.3035));
#51891=CARTESIAN_POINT('',(-2.202274994963,57.495,7.3035));
#51892=CARTESIAN_POINT('',(-2.7850033426108,57.495,7.3035));
#51893=CARTESIAN_POINT('',(-2.202274994963,54.32,7.3035));
#51894=CARTESIAN_POINT('Origin',(-1.56623701058281,54.32,5.556));
#51895=CARTESIAN_POINT('',(-1.56623701058281,54.32,5.556));
#51896=CARTESIAN_POINT('',(-2.202274994963,54.32,7.3035));
#51897=CARTESIAN_POINT('',(-1.56623701058281,57.495,5.556));
#51898=CARTESIAN_POINT('',(-2.202274994963,57.495,7.3035));
#51899=CARTESIAN_POINT('',(-1.56623701058281,54.32,5.556));
#51900=CARTESIAN_POINT('Origin',(-0.927402158204089,54.32,5.556));
#51901=CARTESIAN_POINT('',(-0.927402158204089,54.32,5.556));
#51902=CARTESIAN_POINT('',(-1.56623701058281,54.32,5.556));
#51903=CARTESIAN_POINT('',(-0.927402158204096,57.495,5.556));
#51904=CARTESIAN_POINT('',(-1.56623701058281,57.495,5.556));
#51905=CARTESIAN_POINT('',(-0.927402158204089,54.32,5.556));
#51906=CARTESIAN_POINT('Origin',(-0.291364173823901,54.32,7.3035));
#51907=CARTESIAN_POINT('',(-0.291364173823901,54.32,7.3035));
#51908=CARTESIAN_POINT('',(-0.927402158204089,54.32,5.556));
#51909=CARTESIAN_POINT('',(-0.291364173823894,57.495,7.3035));
#51910=CARTESIAN_POINT('',(-0.927402158204089,57.495,5.556));
#51911=CARTESIAN_POINT('',(-0.291364173823901,54.32,7.3035));
#51912=CARTESIAN_POINT('Origin',(0.291364173823901,54.32,7.3035));
#51913=CARTESIAN_POINT('',(0.291364173823901,54.32,7.3035));
#51914=CARTESIAN_POINT('',(-0.291364173823901,54.32,7.3035));
#51915=CARTESIAN_POINT('',(0.291364173823894,57.495,7.3035));
#51916=CARTESIAN_POINT('',(-0.291364173823901,57.495,7.3035));
#51917=CARTESIAN_POINT('',(0.291364173823901,54.32,7.3035));
#51918=CARTESIAN_POINT('Origin',(0.927402158204089,54.32,5.556));
#51919=CARTESIAN_POINT('',(0.927402158204089,54.32,5.556));
#51920=CARTESIAN_POINT('',(0.291364173823901,54.32,7.3035));
#51921=CARTESIAN_POINT('',(0.927402158204096,57.495,5.556));
#51922=CARTESIAN_POINT('',(0.291364173823901,57.495,7.3035));
#51923=CARTESIAN_POINT('',(0.927402158204089,54.32,5.556));
#51924=CARTESIAN_POINT('Origin',(1.56623701058281,54.32,5.556));
#51925=CARTESIAN_POINT('',(1.56623701058281,54.32,5.556));
#51926=CARTESIAN_POINT('',(0.927402158204089,54.32,5.556));
#51927=CARTESIAN_POINT('',(1.56623701058281,57.495,5.556));
#51928=CARTESIAN_POINT('',(0.927402158204089,57.495,5.556));
#51929=CARTESIAN_POINT('',(1.56623701058281,54.32,5.556));
#51930=CARTESIAN_POINT('Origin',(2.202274994963,54.32,7.3035));
#51931=CARTESIAN_POINT('',(2.202274994963,54.32,7.3035));
#51932=CARTESIAN_POINT('',(1.56623701058281,54.32,5.556));
#51933=CARTESIAN_POINT('',(2.202274994963,57.495,7.3035));
#51934=CARTESIAN_POINT('',(1.56623701058281,57.495,5.556));
#51935=CARTESIAN_POINT('',(2.202274994963,54.32,7.3035));
#51936=CARTESIAN_POINT('Origin',(2.7850033426108,54.32,7.3035));
#51937=CARTESIAN_POINT('',(2.7850033426108,54.32,7.3035));
#51938=CARTESIAN_POINT('',(2.202274994963,54.32,7.3035));
#51939=CARTESIAN_POINT('',(2.7850033426108,57.495,7.3035));
#51940=CARTESIAN_POINT('',(2.202274994963,57.495,7.3035));
#51941=CARTESIAN_POINT('',(2.7850033426108,54.32,7.3035));
#51942=CARTESIAN_POINT('Origin',(3.42104132699099,54.32,5.556));
#51943=CARTESIAN_POINT('',(3.42104132699099,54.32,5.556));
#51944=CARTESIAN_POINT('',(2.7850033426108,54.32,7.3035));
#51945=CARTESIAN_POINT('',(3.42104132699099,57.495,5.556));
#51946=CARTESIAN_POINT('',(2.7850033426108,57.495,7.3035));
#51947=CARTESIAN_POINT('',(3.42104132699099,54.32,5.556));
#51948=CARTESIAN_POINT('Origin',(4.05987617936971,54.32,5.556));
#51949=CARTESIAN_POINT('',(4.05987617936971,54.32,5.556));
#51950=CARTESIAN_POINT('',(3.42104132699099,54.32,5.556));
#51951=CARTESIAN_POINT('',(4.05987617936971,57.495,5.556));
#51952=CARTESIAN_POINT('',(3.42104132699099,57.495,5.556));
#51953=CARTESIAN_POINT('',(4.05987617936971,54.32,5.556));
#51954=CARTESIAN_POINT('Origin',(4.6959141637499,54.32,7.3035));
#51955=CARTESIAN_POINT('',(4.6959141637499,54.32,7.3035));
#51956=CARTESIAN_POINT('',(4.05987617936971,54.32,5.556));
#51957=CARTESIAN_POINT('',(4.69591416374989,57.495,7.3035));
#51958=CARTESIAN_POINT('',(4.05987617936971,57.495,5.556));
#51959=CARTESIAN_POINT('',(4.6959141637499,54.32,7.3035));
#51960=CARTESIAN_POINT('Origin',(5.2786425113977,54.32,7.3035));
#51961=CARTESIAN_POINT('',(5.2786425113977,54.32,7.3035));
#51962=CARTESIAN_POINT('',(4.6959141637499,54.32,7.3035));
#51963=CARTESIAN_POINT('',(5.2786425113977,57.495,7.3035));
#51964=CARTESIAN_POINT('',(4.6959141637499,57.495,7.3035));
#51965=CARTESIAN_POINT('',(5.2786425113977,54.32,7.3035));
#51966=CARTESIAN_POINT('Origin',(5.91468049577789,54.32,5.556));
#51967=CARTESIAN_POINT('',(5.91468049577789,54.32,5.556));
#51968=CARTESIAN_POINT('',(5.2786425113977,54.32,7.3035));
#51969=CARTESIAN_POINT('',(5.91468049577788,57.495,5.556));
#51970=CARTESIAN_POINT('',(5.2786425113977,57.495,7.3035));
#51971=CARTESIAN_POINT('',(5.91468049577789,54.32,5.556));
#51972=CARTESIAN_POINT('Origin',(6.55351534815661,54.32,5.556));
#51973=CARTESIAN_POINT('',(6.55351534815661,54.32,5.556));
#51974=CARTESIAN_POINT('',(5.91468049577789,54.32,5.556));
#51975=CARTESIAN_POINT('',(6.5535153481566,57.495,5.556));
#51976=CARTESIAN_POINT('',(5.91468049577789,57.495,5.556));
#51977=CARTESIAN_POINT('',(6.55351534815661,54.32,5.556));
#51978=CARTESIAN_POINT('Origin',(7.18955333253679,54.32,7.3035));
#51979=CARTESIAN_POINT('',(7.18955333253679,54.32,7.3035));
#51980=CARTESIAN_POINT('',(6.55351534815661,54.32,5.556));
#51981=CARTESIAN_POINT('',(7.1895533325368,57.495,7.3035));
#51982=CARTESIAN_POINT('',(6.55351534815661,57.495,5.556));
#51983=CARTESIAN_POINT('',(7.18955333253679,54.32,7.3035));
#51984=CARTESIAN_POINT('Origin',(7.7722816801846,54.32,7.3035));
#51985=CARTESIAN_POINT('',(7.7722816801846,54.32,7.3035));
#51986=CARTESIAN_POINT('',(7.18955333253679,54.32,7.3035));
#51987=CARTESIAN_POINT('',(7.77228168018459,57.495,7.3035));
#51988=CARTESIAN_POINT('',(7.18955333253679,57.495,7.3035));
#51989=CARTESIAN_POINT('',(7.7722816801846,54.32,7.3035));
#51990=CARTESIAN_POINT('Origin',(8.40831966456478,54.32,5.556));
#51991=CARTESIAN_POINT('',(8.40831966456478,54.32,5.556));
#51992=CARTESIAN_POINT('',(7.7722816801846,54.32,7.3035));
#51993=CARTESIAN_POINT('',(8.40831966456479,57.495,5.556));
#51994=CARTESIAN_POINT('',(7.7722816801846,57.495,7.3035));
#51995=CARTESIAN_POINT('',(8.40831966456478,54.32,5.556));
#51996=CARTESIAN_POINT('Origin',(9.0471545169435,54.32,5.556));
#51997=CARTESIAN_POINT('',(9.0471545169435,54.32,5.556));
#51998=CARTESIAN_POINT('',(8.40831966456478,54.32,5.556));
#51999=CARTESIAN_POINT('',(9.04715451694351,57.495,5.556));
#52000=CARTESIAN_POINT('',(8.40831966456478,57.495,5.556));
#52001=CARTESIAN_POINT('',(9.0471545169435,54.32,5.556));
#52002=CARTESIAN_POINT('Origin',(9.68319250132369,54.32,7.3035));
#52003=CARTESIAN_POINT('',(9.68319250132369,54.32,7.3035));
#52004=CARTESIAN_POINT('',(9.0471545169435,54.32,5.556));
#52005=CARTESIAN_POINT('',(9.68319250132369,57.495,7.3035));
#52006=CARTESIAN_POINT('',(9.0471545169435,57.495,5.556));
#52007=CARTESIAN_POINT('',(9.68319250132369,54.32,7.3035));
#52008=CARTESIAN_POINT('Origin',(10.2659208489715,54.32,7.3035));
#52009=CARTESIAN_POINT('',(10.2659208489715,54.32,7.3035));
#52010=CARTESIAN_POINT('',(9.68319250132369,54.32,7.3035));
#52011=CARTESIAN_POINT('',(10.2659208489715,57.495,7.3035));
#52012=CARTESIAN_POINT('',(9.68319250132369,57.495,7.3035));
#52013=CARTESIAN_POINT('',(10.2659208489715,54.32,7.3035));
#52014=CARTESIAN_POINT('Origin',(10.9019588333517,54.32,5.556));
#52015=CARTESIAN_POINT('',(10.9019588333517,54.32,5.556));
#52016=CARTESIAN_POINT('',(10.2659208489715,54.32,7.3035));
#52017=CARTESIAN_POINT('',(10.9019588333517,57.495,5.556));
#52018=CARTESIAN_POINT('',(10.2659208489715,57.495,7.3035));
#52019=CARTESIAN_POINT('',(10.9019588333517,54.32,5.556));
#52020=CARTESIAN_POINT('Origin',(11.5407936857304,54.32,5.556));
#52021=CARTESIAN_POINT('',(11.5407936857304,54.32,5.556));
#52022=CARTESIAN_POINT('',(10.9019588333517,54.32,5.556));
#52023=CARTESIAN_POINT('',(11.5407936857304,57.495,5.556));
#52024=CARTESIAN_POINT('',(10.9019588333517,57.495,5.556));
#52025=CARTESIAN_POINT('',(11.5407936857304,54.32,5.556));
#52026=CARTESIAN_POINT('Origin',(12.1768316701106,54.32,7.3035));
#52027=CARTESIAN_POINT('',(12.1768316701106,54.32,7.3035));
#52028=CARTESIAN_POINT('',(11.5407936857304,54.32,5.556));
#52029=CARTESIAN_POINT('',(12.1768316701106,57.495,7.3035));
#52030=CARTESIAN_POINT('',(11.5407936857304,57.495,5.556));
#52031=CARTESIAN_POINT('',(12.1768316701106,54.32,7.3035));
#52032=CARTESIAN_POINT('Origin',(12.7595600177584,54.32,7.3035));
#52033=CARTESIAN_POINT('',(12.7595600177584,54.32,7.3035));
#52034=CARTESIAN_POINT('',(12.1768316701106,54.32,7.3035));
#52035=CARTESIAN_POINT('',(12.7595600177584,57.495,7.3035));
#52036=CARTESIAN_POINT('',(12.1768316701106,57.495,7.3035));
#52037=CARTESIAN_POINT('',(12.7595600177584,54.32,7.3035));
#52038=CARTESIAN_POINT('Origin',(13.3955980021386,54.32,5.556));
#52039=CARTESIAN_POINT('',(13.3955980021386,54.32,5.556));
#52040=CARTESIAN_POINT('',(12.7595600177584,54.32,7.3035));
#52041=CARTESIAN_POINT('',(13.3955980021386,57.495,5.556));
#52042=CARTESIAN_POINT('',(12.7595600177584,57.495,7.3035));
#52043=CARTESIAN_POINT('',(13.3955980021386,54.32,5.556));
#52044=CARTESIAN_POINT('Origin',(14.0344328545173,54.32,5.556));
#52045=CARTESIAN_POINT('',(14.0344328545173,54.32,5.556));
#52046=CARTESIAN_POINT('',(13.3955980021386,54.32,5.556));
#52047=CARTESIAN_POINT('',(14.0344328545173,57.495,5.556));
#52048=CARTESIAN_POINT('',(13.3955980021386,57.495,5.556));
#52049=CARTESIAN_POINT('',(14.0344328545173,54.32,5.556));
#52050=CARTESIAN_POINT('Origin',(14.6704708388975,54.32,7.3035));
#52051=CARTESIAN_POINT('',(14.6704708388975,54.32,7.3035));
#52052=CARTESIAN_POINT('',(14.0344328545173,54.32,5.556));
#52053=CARTESIAN_POINT('',(14.6704708388975,57.495,7.3035));
#52054=CARTESIAN_POINT('',(14.0344328545173,57.495,5.556));
#52055=CARTESIAN_POINT('',(14.6704708388975,54.32,7.3035));
#52056=CARTESIAN_POINT('Origin',(15.2531991865453,54.32,7.3035));
#52057=CARTESIAN_POINT('',(15.2531991865453,54.32,7.3035));
#52058=CARTESIAN_POINT('',(14.6704708388975,54.32,7.3035));
#52059=CARTESIAN_POINT('',(15.2531991865453,57.495,7.3035));
#52060=CARTESIAN_POINT('',(14.6704708388975,57.495,7.3035));
#52061=CARTESIAN_POINT('',(15.2531991865453,54.32,7.3035));
#52062=CARTESIAN_POINT('Origin',(15.8892371709255,54.32,5.556));
#52063=CARTESIAN_POINT('',(15.8892371709255,54.32,5.556));
#52064=CARTESIAN_POINT('',(15.2531991865453,54.32,7.3035));
#52065=CARTESIAN_POINT('',(15.8892371709255,57.495,5.556));
#52066=CARTESIAN_POINT('',(15.2531991865453,57.495,7.3035));
#52067=CARTESIAN_POINT('',(15.8892371709255,54.32,5.556));
#52068=CARTESIAN_POINT('Origin',(16.5280720233042,54.32,5.556));
#52069=CARTESIAN_POINT('',(16.5280720233042,54.32,5.556));
#52070=CARTESIAN_POINT('',(15.8892371709255,54.32,5.556));
#52071=CARTESIAN_POINT('',(16.5280720233042,57.495,5.556));
#52072=CARTESIAN_POINT('',(15.8892371709255,57.495,5.556));
#52073=CARTESIAN_POINT('',(16.5280720233042,54.32,5.556));
#52074=CARTESIAN_POINT('Origin',(17.1641100076844,54.32,7.3035));
#52075=CARTESIAN_POINT('',(17.1641100076844,54.32,7.3035));
#52076=CARTESIAN_POINT('',(16.5280720233042,54.32,5.556));
#52077=CARTESIAN_POINT('',(17.1641100076844,57.495,7.3035));
#52078=CARTESIAN_POINT('',(16.5280720233042,57.495,5.556));
#52079=CARTESIAN_POINT('',(17.1641100076844,54.32,7.3035));
#52080=CARTESIAN_POINT('Origin',(17.7468383553322,54.32,7.3035));
#52081=CARTESIAN_POINT('',(17.7468383553322,54.32,7.3035));
#52082=CARTESIAN_POINT('',(17.1641100076844,54.32,7.3035));
#52083=CARTESIAN_POINT('',(17.7468383553322,57.495,7.3035));
#52084=CARTESIAN_POINT('',(17.1641100076844,57.495,7.3035));
#52085=CARTESIAN_POINT('',(17.7468383553322,54.32,7.3035));
#52086=CARTESIAN_POINT('Origin',(18.3828763397124,54.32,5.556));
#52087=CARTESIAN_POINT('',(18.3828763397124,54.32,5.556));
#52088=CARTESIAN_POINT('',(17.7468383553322,54.32,7.3035));
#52089=CARTESIAN_POINT('',(18.3828763397124,57.495,5.556));
#52090=CARTESIAN_POINT('',(17.7468383553322,57.495,7.3035));
#52091=CARTESIAN_POINT('',(18.3828763397124,54.32,5.556));
#52092=CARTESIAN_POINT('Origin',(19.0217111920911,54.32,5.556));
#52093=CARTESIAN_POINT('',(19.0217111920911,54.32,5.556));
#52094=CARTESIAN_POINT('',(18.3828763397124,54.32,5.556));
#52095=CARTESIAN_POINT('',(19.0217111920911,57.495,5.556));
#52096=CARTESIAN_POINT('',(18.3828763397124,57.495,5.556));
#52097=CARTESIAN_POINT('',(19.0217111920911,54.32,5.556));
#52098=CARTESIAN_POINT('Origin',(19.6577491764713,54.32,7.3035));
#52099=CARTESIAN_POINT('',(19.6577491764713,54.32,7.3035));
#52100=CARTESIAN_POINT('',(19.0217111920911,54.32,5.556));
#52101=CARTESIAN_POINT('',(19.6577491764713,57.495,7.3035));
#52102=CARTESIAN_POINT('',(19.0217111920911,57.495,5.556));
#52103=CARTESIAN_POINT('',(19.6577491764713,54.32,7.3035));
#52104=CARTESIAN_POINT('Origin',(20.2404775241191,54.32,7.3035));
#52105=CARTESIAN_POINT('',(20.2404775241191,54.32,7.3035));
#52106=CARTESIAN_POINT('',(19.6577491764713,54.32,7.3035));
#52107=CARTESIAN_POINT('',(20.2404775241191,57.495,7.3035));
#52108=CARTESIAN_POINT('',(19.6577491764713,57.495,7.3035));
#52109=CARTESIAN_POINT('',(20.2404775241191,54.32,7.3035));
#52110=CARTESIAN_POINT('Origin',(20.8765155084993,54.32,5.556));
#52111=CARTESIAN_POINT('',(20.8765155084993,54.32,5.556));
#52112=CARTESIAN_POINT('',(20.2404775241191,54.32,7.3035));
#52113=CARTESIAN_POINT('',(20.8765155084993,57.495,5.556));
#52114=CARTESIAN_POINT('',(20.2404775241191,57.495,7.3035));
#52115=CARTESIAN_POINT('',(20.8765155084993,54.32,5.556));
#52116=CARTESIAN_POINT('Origin',(21.515350360878,54.32,5.556));
#52117=CARTESIAN_POINT('',(21.515350360878,54.32,5.556));
#52118=CARTESIAN_POINT('',(20.8765155084993,54.32,5.556));
#52119=CARTESIAN_POINT('',(21.515350360878,57.495,5.556));
#52120=CARTESIAN_POINT('',(20.8765155084993,57.495,5.556));
#52121=CARTESIAN_POINT('',(21.515350360878,54.32,5.556));
#52122=CARTESIAN_POINT('Origin',(22.1513883452582,54.32,7.3035));
#52123=CARTESIAN_POINT('',(22.1513883452582,54.32,7.3035));
#52124=CARTESIAN_POINT('',(21.515350360878,54.32,5.556));
#52125=CARTESIAN_POINT('',(22.1513883452582,57.495,7.3035));
#52126=CARTESIAN_POINT('',(21.515350360878,57.495,5.556));
#52127=CARTESIAN_POINT('',(22.1513883452582,54.32,7.3035));
#52128=CARTESIAN_POINT('Origin',(22.734116692906,54.32,7.3035));
#52129=CARTESIAN_POINT('',(22.734116692906,54.32,7.3035));
#52130=CARTESIAN_POINT('',(22.1513883452582,54.32,7.3035));
#52131=CARTESIAN_POINT('',(22.734116692906,57.495,7.3035));
#52132=CARTESIAN_POINT('',(22.1513883452582,57.495,7.3035));
#52133=CARTESIAN_POINT('',(22.734116692906,54.32,7.3035));
#52134=CARTESIAN_POINT('Origin',(23.3701546772862,54.32,5.556));
#52135=CARTESIAN_POINT('',(23.3701546772862,54.32,5.556));
#52136=CARTESIAN_POINT('',(22.734116692906,54.32,7.3035));
#52137=CARTESIAN_POINT('',(23.3701546772862,57.495,5.556));
#52138=CARTESIAN_POINT('',(22.734116692906,57.495,7.3035));
#52139=CARTESIAN_POINT('',(23.3701546772862,54.32,5.556));
#52140=CARTESIAN_POINT('Origin',(24.0089895296649,54.32,5.556));
#52141=CARTESIAN_POINT('',(24.0089895296649,54.32,5.556));
#52142=CARTESIAN_POINT('',(23.3701546772862,54.32,5.556));
#52143=CARTESIAN_POINT('',(24.0089895296649,57.495,5.556));
#52144=CARTESIAN_POINT('',(23.3701546772862,57.495,5.556));
#52145=CARTESIAN_POINT('',(24.0089895296649,54.32,5.556));
#52146=CARTESIAN_POINT('Origin',(24.6450275140451,54.32,7.3035));
#52147=CARTESIAN_POINT('',(24.6450275140451,54.32,7.3035));
#52148=CARTESIAN_POINT('',(24.0089895296649,54.32,5.556));
#52149=CARTESIAN_POINT('',(24.6450275140451,57.495,7.3035));
#52150=CARTESIAN_POINT('',(24.0089895296649,57.495,5.556));
#52151=CARTESIAN_POINT('',(24.6450275140451,54.32,7.3035));
#52152=CARTESIAN_POINT('Origin',(25.2277558616929,54.32,7.3035));
#52153=CARTESIAN_POINT('',(25.2277558616929,54.32,7.3035));
#52154=CARTESIAN_POINT('',(24.6450275140451,54.32,7.3035));
#52155=CARTESIAN_POINT('',(25.2277558616929,57.495,7.3035));
#52156=CARTESIAN_POINT('',(24.6450275140451,57.495,7.3035));
#52157=CARTESIAN_POINT('',(25.2277558616929,54.32,7.3035));
#52158=CARTESIAN_POINT('Origin',(25.8637938460731,54.32,5.556));
#52159=CARTESIAN_POINT('',(25.8637938460731,54.32,5.556));
#52160=CARTESIAN_POINT('',(25.2277558616929,54.32,7.3035));
#52161=CARTESIAN_POINT('',(25.8637938460731,57.495,5.556));
#52162=CARTESIAN_POINT('',(25.2277558616929,57.495,7.3035));
#52163=CARTESIAN_POINT('',(25.8637938460731,54.32,5.556));
#52164=CARTESIAN_POINT('Origin',(26.5026286984518,54.32,5.556));
#52165=CARTESIAN_POINT('',(26.5026286984518,54.32,5.556));
#52166=CARTESIAN_POINT('',(25.8637938460731,54.32,5.556));
#52167=CARTESIAN_POINT('',(26.5026286984518,57.495,5.556));
#52168=CARTESIAN_POINT('',(25.8637938460731,57.495,5.556));
#52169=CARTESIAN_POINT('',(26.5026286984518,54.32,5.556));
#52170=CARTESIAN_POINT('Origin',(27.138666682832,54.32,7.3035));
#52171=CARTESIAN_POINT('',(27.138666682832,54.32,7.3035));
#52172=CARTESIAN_POINT('',(26.5026286984518,54.32,5.556));
#52173=CARTESIAN_POINT('',(27.138666682832,57.495,7.3035));
#52174=CARTESIAN_POINT('',(26.5026286984518,57.495,5.556));
#52175=CARTESIAN_POINT('',(27.138666682832,54.32,7.3035));
#52176=CARTESIAN_POINT('Origin',(27.7213950304798,54.32,7.3035));
#52177=CARTESIAN_POINT('',(27.7213950304798,54.32,7.3035));
#52178=CARTESIAN_POINT('',(27.138666682832,54.32,7.3035));
#52179=CARTESIAN_POINT('',(27.7213950304798,57.495,7.3035));
#52180=CARTESIAN_POINT('',(27.138666682832,57.495,7.3035));
#52181=CARTESIAN_POINT('',(27.7213950304798,54.32,7.3035));
#52182=CARTESIAN_POINT('Origin',(28.35743301486,54.32,5.556));
#52183=CARTESIAN_POINT('',(28.35743301486,54.32,5.556));
#52184=CARTESIAN_POINT('',(27.7213950304798,54.32,7.3035));
#52185=CARTESIAN_POINT('',(28.35743301486,57.495,5.556));
#52186=CARTESIAN_POINT('',(27.7213950304798,57.495,7.3035));
#52187=CARTESIAN_POINT('',(28.35743301486,54.32,5.556));
#52188=CARTESIAN_POINT('Origin',(28.9962678672387,54.32,5.556));
#52189=CARTESIAN_POINT('',(28.9962678672387,54.32,5.556));
#52190=CARTESIAN_POINT('',(28.35743301486,54.32,5.556));
#52191=CARTESIAN_POINT('',(28.9962678672387,57.495,5.556));
#52192=CARTESIAN_POINT('',(28.35743301486,57.495,5.556));
#52193=CARTESIAN_POINT('',(28.9962678672387,54.32,5.556));
#52194=CARTESIAN_POINT('Origin',(29.6323058516189,54.32,7.3035));
#52195=CARTESIAN_POINT('',(29.6323058516189,54.32,7.3035));
#52196=CARTESIAN_POINT('',(28.9962678672387,54.32,5.556));
#52197=CARTESIAN_POINT('',(29.6323058516189,57.495,7.3035));
#52198=CARTESIAN_POINT('',(28.9962678672387,57.495,5.556));
#52199=CARTESIAN_POINT('',(29.6323058516189,54.32,7.3035));
#52200=CARTESIAN_POINT('Origin',(30.2150341992667,54.32,7.3035));
#52201=CARTESIAN_POINT('',(30.2150341992667,54.32,7.3035));
#52202=CARTESIAN_POINT('',(29.6323058516189,54.32,7.3035));
#52203=CARTESIAN_POINT('',(30.2150341992667,57.495,7.3035));
#52204=CARTESIAN_POINT('',(29.6323058516189,57.495,7.3035));
#52205=CARTESIAN_POINT('',(30.2150341992667,54.32,7.3035));
#52206=CARTESIAN_POINT('Origin',(30.8510721836469,54.32,5.556));
#52207=CARTESIAN_POINT('',(30.8510721836469,54.32,5.556));
#52208=CARTESIAN_POINT('',(30.2150341992667,54.32,7.3035));
#52209=CARTESIAN_POINT('',(30.8510721836469,57.495,5.556));
#52210=CARTESIAN_POINT('',(30.2150341992667,57.495,7.3035));
#52211=CARTESIAN_POINT('',(30.8510721836469,54.32,5.556));
#52212=CARTESIAN_POINT('Origin',(31.4899070360256,54.32,5.556));
#52213=CARTESIAN_POINT('',(31.4899070360256,54.32,5.556));
#52214=CARTESIAN_POINT('',(30.8510721836469,54.32,5.556));
#52215=CARTESIAN_POINT('',(31.4899070360256,57.495,5.556));
#52216=CARTESIAN_POINT('',(30.8510721836469,57.495,5.556));
#52217=CARTESIAN_POINT('',(31.4899070360256,54.32,5.556));
#52218=CARTESIAN_POINT('Origin',(32.1259450204058,54.32,7.3035));
#52219=CARTESIAN_POINT('',(32.1259450204058,54.32,7.3035));
#52220=CARTESIAN_POINT('',(31.4899070360256,54.32,5.556));
#52221=CARTESIAN_POINT('',(32.1259450204058,57.495,7.3035));
#52222=CARTESIAN_POINT('',(31.4899070360256,57.495,5.556));
#52223=CARTESIAN_POINT('',(32.1259450204058,54.32,7.3035));
#52224=CARTESIAN_POINT('Origin',(32.7086733680536,54.32,7.3035));
#52225=CARTESIAN_POINT('',(32.7086733680536,54.32,7.3035));
#52226=CARTESIAN_POINT('',(32.1259450204058,54.32,7.3035));
#52227=CARTESIAN_POINT('',(32.7086733680536,57.495,7.3035));
#52228=CARTESIAN_POINT('',(32.1259450204058,57.495,7.3035));
#52229=CARTESIAN_POINT('',(32.7086733680536,54.32,7.3035));
#52230=CARTESIAN_POINT('Origin',(33.3447113524338,54.32,5.556));
#52231=CARTESIAN_POINT('',(33.3447113524338,54.32,5.556));
#52232=CARTESIAN_POINT('',(32.7086733680536,54.32,7.3035));
#52233=CARTESIAN_POINT('',(33.3447113524338,57.495,5.556));
#52234=CARTESIAN_POINT('',(32.7086733680536,57.495,7.3035));
#52235=CARTESIAN_POINT('',(33.3447113524338,54.32,5.556));
#52236=CARTESIAN_POINT('Origin',(33.9835462048125,54.32,5.556));
#52237=CARTESIAN_POINT('',(33.9835462048125,54.32,5.556));
#52238=CARTESIAN_POINT('',(33.3447113524338,54.32,5.556));
#52239=CARTESIAN_POINT('',(33.9835462048125,57.495,5.556));
#52240=CARTESIAN_POINT('',(33.3447113524338,57.495,5.556));
#52241=CARTESIAN_POINT('',(33.9835462048125,54.32,5.556));
#52242=CARTESIAN_POINT('Origin',(34.6195841891927,54.32,7.3035));
#52243=CARTESIAN_POINT('',(34.6195841891927,54.32,7.3035));
#52244=CARTESIAN_POINT('',(33.9835462048125,54.32,5.556));
#52245=CARTESIAN_POINT('',(34.6195841891927,57.495,7.3035));
#52246=CARTESIAN_POINT('',(33.9835462048125,57.495,5.556));
#52247=CARTESIAN_POINT('',(34.6195841891927,54.32,7.3035));
#52248=CARTESIAN_POINT('Origin',(35.2023125368405,54.32,7.3035));
#52249=CARTESIAN_POINT('',(35.2023125368405,54.32,7.3035));
#52250=CARTESIAN_POINT('',(34.6195841891927,54.32,7.3035));
#52251=CARTESIAN_POINT('',(35.2023125368405,57.495,7.3035));
#52252=CARTESIAN_POINT('',(34.6195841891927,57.495,7.3035));
#52253=CARTESIAN_POINT('',(35.2023125368405,54.32,7.3035));
#52254=CARTESIAN_POINT('Origin',(35.8383505212207,54.32,5.556));
#52255=CARTESIAN_POINT('',(35.8383505212207,54.32,5.556));
#52256=CARTESIAN_POINT('',(35.2023125368405,54.32,7.3035));
#52257=CARTESIAN_POINT('',(35.8383505212207,57.495,5.556));
#52258=CARTESIAN_POINT('',(35.2023125368405,57.495,7.3035));
#52259=CARTESIAN_POINT('',(35.8383505212207,54.32,5.556));
#52260=CARTESIAN_POINT('Origin',(36.4771853735994,54.32,5.556));
#52261=CARTESIAN_POINT('',(36.4771853735994,54.32,5.556));
#52262=CARTESIAN_POINT('',(35.8383505212207,54.32,5.556));
#52263=CARTESIAN_POINT('',(36.4771853735994,57.495,5.556));
#52264=CARTESIAN_POINT('',(35.8383505212207,57.495,5.556));
#52265=CARTESIAN_POINT('',(36.4771853735994,54.32,5.556));
#52266=CARTESIAN_POINT('Origin',(37.1132233579796,54.32,7.3035));
#52267=CARTESIAN_POINT('',(37.1132233579796,54.32,7.3035));
#52268=CARTESIAN_POINT('',(36.4771853735994,54.32,5.556));
#52269=CARTESIAN_POINT('',(37.1132233579796,57.495,7.3035));
#52270=CARTESIAN_POINT('',(36.4771853735994,57.495,5.556));
#52271=CARTESIAN_POINT('',(37.1132233579796,54.32,7.3035));
#52272=CARTESIAN_POINT('Origin',(37.6959517056274,54.32,7.3035));
#52273=CARTESIAN_POINT('',(37.6959517056274,54.32,7.3035));
#52274=CARTESIAN_POINT('',(37.1132233579796,54.32,7.3035));
#52275=CARTESIAN_POINT('',(37.6959517056274,57.495,7.3035));
#52276=CARTESIAN_POINT('',(37.1132233579796,57.495,7.3035));
#52277=CARTESIAN_POINT('',(37.6959517056274,54.32,7.3035));
#52278=CARTESIAN_POINT('Origin',(38.3319896900076,54.32,5.556));
#52279=CARTESIAN_POINT('',(38.3319896900076,54.32,5.556));
#52280=CARTESIAN_POINT('',(37.6959517056274,54.32,7.3035));
#52281=CARTESIAN_POINT('',(38.3319896900076,57.495,5.556));
#52282=CARTESIAN_POINT('',(37.6959517056274,57.495,7.3035));
#52283=CARTESIAN_POINT('',(38.3319896900076,54.32,5.556));
#52284=CARTESIAN_POINT('Origin',(38.9708245423863,54.32,5.556));
#52285=CARTESIAN_POINT('',(38.9708245423863,54.32,5.556));
#52286=CARTESIAN_POINT('',(38.3319896900076,54.32,5.556));
#52287=CARTESIAN_POINT('',(38.9708245423863,57.495,5.556));
#52288=CARTESIAN_POINT('',(38.3319896900076,57.495,5.556));
#52289=CARTESIAN_POINT('',(38.9708245423863,54.32,5.556));
#52290=CARTESIAN_POINT('Origin',(39.6068625267665,54.32,7.3035));
#52291=CARTESIAN_POINT('',(39.6068625267665,54.32,7.3035));
#52292=CARTESIAN_POINT('',(38.9708245423863,54.32,5.556));
#52293=CARTESIAN_POINT('',(39.6068625267665,57.495,7.3035));
#52294=CARTESIAN_POINT('',(38.9708245423863,57.495,5.556));
#52295=CARTESIAN_POINT('',(39.6068625267665,54.32,7.3035));
#52296=CARTESIAN_POINT('Origin',(40.1895908744143,54.32,7.3035));
#52297=CARTESIAN_POINT('',(40.1895908744143,54.32,7.3035));
#52298=CARTESIAN_POINT('',(39.6068625267665,54.32,7.3035));
#52299=CARTESIAN_POINT('',(40.1895908744143,57.495,7.3035));
#52300=CARTESIAN_POINT('',(39.6068625267665,57.495,7.3035));
#52301=CARTESIAN_POINT('',(40.1895908744143,54.32,7.3035));
#52302=CARTESIAN_POINT('Origin',(40.8256288587945,54.32,5.556));
#52303=CARTESIAN_POINT('',(40.8256288587945,54.32,5.556));
#52304=CARTESIAN_POINT('',(40.1895908744143,54.32,7.3035));
#52305=CARTESIAN_POINT('',(40.8256288587945,57.495,5.556));
#52306=CARTESIAN_POINT('',(40.1895908744143,57.495,7.3035));
#52307=CARTESIAN_POINT('',(40.8256288587945,54.32,5.556));
#52308=CARTESIAN_POINT('Origin',(41.4644637111732,54.32,5.556));
#52309=CARTESIAN_POINT('',(41.4644637111732,54.32,5.556));
#52310=CARTESIAN_POINT('',(40.8256288587945,54.32,5.556));
#52311=CARTESIAN_POINT('',(41.4644637111732,57.495,5.556));
#52312=CARTESIAN_POINT('',(40.8256288587945,57.495,5.556));
#52313=CARTESIAN_POINT('',(41.4644637111732,54.32,5.556));
#52314=CARTESIAN_POINT('Origin',(42.1005016955534,54.32,7.3035));
#52315=CARTESIAN_POINT('',(42.1005016955534,54.32,7.3035));
#52316=CARTESIAN_POINT('',(41.4644637111732,54.32,5.556));
#52317=CARTESIAN_POINT('',(42.1005016955534,57.495,7.3035));
#52318=CARTESIAN_POINT('',(41.4644637111732,57.495,5.556));
#52319=CARTESIAN_POINT('',(42.1005016955534,54.32,7.3035));
#52320=CARTESIAN_POINT('Origin',(42.6832300432012,54.32,7.3035));
#52321=CARTESIAN_POINT('',(42.6832300432012,54.32,7.3035));
#52322=CARTESIAN_POINT('',(42.1005016955534,54.32,7.3035));
#52323=CARTESIAN_POINT('',(42.6832300432012,57.495,7.3035));
#52324=CARTESIAN_POINT('',(42.1005016955534,57.495,7.3035));
#52325=CARTESIAN_POINT('',(42.6832300432012,54.32,7.3035));
#52326=CARTESIAN_POINT('Origin',(43.3192680275814,54.32,5.556));
#52327=CARTESIAN_POINT('',(43.3192680275814,54.32,5.556));
#52328=CARTESIAN_POINT('',(42.6832300432012,54.32,7.3035));
#52329=CARTESIAN_POINT('',(43.3192680275813,57.495,5.556));
#52330=CARTESIAN_POINT('',(42.6832300432012,57.495,7.3035));
#52331=CARTESIAN_POINT('',(43.3192680275814,54.32,5.556));
#52332=CARTESIAN_POINT('Origin',(43.9581028799601,54.32,5.556));
#52333=CARTESIAN_POINT('',(43.9581028799601,54.32,5.556));
#52334=CARTESIAN_POINT('',(43.3192680275814,54.32,5.556));
#52335=CARTESIAN_POINT('',(43.9581028799601,57.495,5.556));
#52336=CARTESIAN_POINT('',(43.3192680275814,57.495,5.556));
#52337=CARTESIAN_POINT('',(43.9581028799601,54.32,5.556));
#52338=CARTESIAN_POINT('Origin',(44.5941408643403,54.32,7.3035));
#52339=CARTESIAN_POINT('',(44.5941408643403,54.32,7.3035));
#52340=CARTESIAN_POINT('',(43.9581028799601,54.32,5.556));
#52341=CARTESIAN_POINT('',(44.5941408643403,57.495,7.3035));
#52342=CARTESIAN_POINT('',(43.9581028799601,57.495,5.556));
#52343=CARTESIAN_POINT('',(44.5941408643403,54.32,7.3035));
#52344=CARTESIAN_POINT('Origin',(45.1768692119881,54.32,7.3035));
#52345=CARTESIAN_POINT('',(45.1768692119881,54.32,7.3035));
#52346=CARTESIAN_POINT('',(44.5941408643403,54.32,7.3035));
#52347=CARTESIAN_POINT('',(45.1768692119881,57.495,7.3035));
#52348=CARTESIAN_POINT('',(44.5941408643403,57.495,7.3035));
#52349=CARTESIAN_POINT('',(45.1768692119881,54.32,7.3035));
#52350=CARTESIAN_POINT('Origin',(45.8129071963683,54.32,5.556));
#52351=CARTESIAN_POINT('',(45.8129071963683,54.32,5.556));
#52352=CARTESIAN_POINT('',(45.1768692119881,54.32,7.3035));
#52353=CARTESIAN_POINT('',(45.8129071963683,57.495,5.556));
#52354=CARTESIAN_POINT('',(45.1768692119881,57.495,7.3035));
#52355=CARTESIAN_POINT('',(45.8129071963683,54.32,5.556));
#52356=CARTESIAN_POINT('Origin',(46.451742048747,54.32,5.556));
#52357=CARTESIAN_POINT('',(46.451742048747,54.32,5.556));
#52358=CARTESIAN_POINT('',(45.8129071963683,54.32,5.556));
#52359=CARTESIAN_POINT('',(46.451742048747,57.495,5.556));
#52360=CARTESIAN_POINT('',(45.8129071963683,57.495,5.556));
#52361=CARTESIAN_POINT('',(46.451742048747,54.32,5.556));
#52362=CARTESIAN_POINT('Origin',(47.0877800331272,54.32,7.3035));
#52363=CARTESIAN_POINT('',(47.0877800331272,54.32,7.3035));
#52364=CARTESIAN_POINT('',(46.451742048747,54.32,5.556));
#52365=CARTESIAN_POINT('',(47.0877800331272,57.495,7.3035));
#52366=CARTESIAN_POINT('',(46.451742048747,57.495,5.556));
#52367=CARTESIAN_POINT('',(47.0877800331272,54.32,7.3035));
#52368=CARTESIAN_POINT('Origin',(47.670508380775,54.32,7.3035));
#52369=CARTESIAN_POINT('',(47.670508380775,54.32,7.3035));
#52370=CARTESIAN_POINT('',(47.0877800331272,54.32,7.3035));
#52371=CARTESIAN_POINT('',(47.670508380775,57.495,7.3035));
#52372=CARTESIAN_POINT('',(47.0877800331272,57.495,7.3035));
#52373=CARTESIAN_POINT('',(47.670508380775,54.32,7.3035));
#52374=CARTESIAN_POINT('Origin',(48.3065463651552,54.32,5.556));
#52375=CARTESIAN_POINT('',(48.3065463651552,54.32,5.556));
#52376=CARTESIAN_POINT('',(47.670508380775,54.32,7.3035));
#52377=CARTESIAN_POINT('',(48.3065463651552,57.495,5.556));
#52378=CARTESIAN_POINT('',(47.670508380775,57.495,7.3035));
#52379=CARTESIAN_POINT('',(48.3065463651552,54.32,5.556));
#52380=CARTESIAN_POINT('Origin',(48.9453812175339,54.32,5.556));
#52381=CARTESIAN_POINT('',(48.9453812175339,54.32,5.556));
#52382=CARTESIAN_POINT('',(48.3065463651552,54.32,5.556));
#52383=CARTESIAN_POINT('',(48.9453812175339,57.495,5.556));
#52384=CARTESIAN_POINT('',(48.3065463651552,57.495,5.556));
#52385=CARTESIAN_POINT('',(48.9453812175339,54.32,5.556));
#52386=CARTESIAN_POINT('Origin',(49.5814192019141,54.32,7.3035));
#52387=CARTESIAN_POINT('',(49.5814192019141,54.32,7.3035));
#52388=CARTESIAN_POINT('',(48.9453812175339,54.32,5.556));
#52389=CARTESIAN_POINT('',(49.5814192019141,57.495,7.3035));
#52390=CARTESIAN_POINT('',(48.9453812175339,57.495,5.556));
#52391=CARTESIAN_POINT('',(49.5814192019141,54.32,7.3035));
#52392=CARTESIAN_POINT('Origin',(50.1641475495619,54.32,7.3035));
#52393=CARTESIAN_POINT('',(50.1641475495619,54.32,7.3035));
#52394=CARTESIAN_POINT('',(49.5814192019141,54.32,7.3035));
#52395=CARTESIAN_POINT('',(50.1641475495619,57.495,7.3035));
#52396=CARTESIAN_POINT('',(49.5814192019141,57.495,7.3035));
#52397=CARTESIAN_POINT('',(50.1641475495619,54.32,7.3035));
#52398=CARTESIAN_POINT('Origin',(50.800185533942,54.32,5.556));
#52399=CARTESIAN_POINT('',(50.800185533942,54.32,5.556));
#52400=CARTESIAN_POINT('',(50.1641475495619,54.32,7.3035));
#52401=CARTESIAN_POINT('',(50.8001855339421,57.495,5.556));
#52402=CARTESIAN_POINT('',(50.1641475495619,57.495,7.3035));
#52403=CARTESIAN_POINT('',(50.800185533942,54.32,5.556));
#52404=CARTESIAN_POINT('Origin',(51.4390203863208,54.32,5.556));
#52405=CARTESIAN_POINT('',(51.4390203863208,54.32,5.556));
#52406=CARTESIAN_POINT('',(50.800185533942,54.32,5.556));
#52407=CARTESIAN_POINT('',(51.4390203863208,57.495,5.556));
#52408=CARTESIAN_POINT('',(50.800185533942,57.495,5.556));
#52409=CARTESIAN_POINT('',(51.4390203863208,54.32,5.556));
#52410=CARTESIAN_POINT('Origin',(52.075058370701,54.32,7.3035));
#52411=CARTESIAN_POINT('',(52.075058370701,54.32,7.3035));
#52412=CARTESIAN_POINT('',(51.4390203863208,54.32,5.556));
#52413=CARTESIAN_POINT('',(52.075058370701,57.495,7.3035));
#52414=CARTESIAN_POINT('',(51.4390203863208,57.495,5.556));
#52415=CARTESIAN_POINT('',(52.075058370701,54.32,7.3035));
#52416=CARTESIAN_POINT('Origin',(52.6577867183488,54.32,7.3035));
#52417=CARTESIAN_POINT('',(52.6577867183488,54.32,7.3035));
#52418=CARTESIAN_POINT('',(52.075058370701,54.32,7.3035));
#52419=CARTESIAN_POINT('',(52.6577867183487,57.495,7.3035));
#52420=CARTESIAN_POINT('',(52.075058370701,57.495,7.3035));
#52421=CARTESIAN_POINT('',(52.6577867183488,54.32,7.3035));
#52422=CARTESIAN_POINT('Origin',(53.293824702729,54.32,5.556));
#52423=CARTESIAN_POINT('',(53.293824702729,54.32,5.556));
#52424=CARTESIAN_POINT('',(52.6577867183488,54.32,7.3035));
#52425=CARTESIAN_POINT('',(53.293824702729,57.495,5.556));
#52426=CARTESIAN_POINT('',(52.6577867183488,57.495,7.3035));
#52427=CARTESIAN_POINT('',(53.293824702729,54.32,5.556));
#52428=CARTESIAN_POINT('Origin',(53.9326595551077,54.32,5.556));
#52429=CARTESIAN_POINT('',(53.9326595551077,54.32,5.556));
#52430=CARTESIAN_POINT('',(53.293824702729,54.32,5.556));
#52431=CARTESIAN_POINT('',(53.9326595551077,57.495,5.556));
#52432=CARTESIAN_POINT('',(53.293824702729,57.495,5.556));
#52433=CARTESIAN_POINT('',(53.9326595551077,54.32,5.556));
#52434=CARTESIAN_POINT('Origin',(54.5686975394879,54.32,7.3035));
#52435=CARTESIAN_POINT('',(54.5686975394879,54.32,7.3035));
#52436=CARTESIAN_POINT('',(53.9326595551077,54.32,5.556));
#52437=CARTESIAN_POINT('',(54.5686975394879,57.495,7.3035));
#52438=CARTESIAN_POINT('',(53.9326595551077,57.495,5.556));
#52439=CARTESIAN_POINT('',(54.5686975394879,54.32,7.3035));
#52440=CARTESIAN_POINT('Origin',(55.1514258871357,54.32,7.3035));
#52441=CARTESIAN_POINT('',(55.1514258871357,54.32,7.3035));
#52442=CARTESIAN_POINT('',(54.5686975394879,54.32,7.3035));
#52443=CARTESIAN_POINT('',(55.1514258871357,57.495,7.3035));
#52444=CARTESIAN_POINT('',(54.5686975394879,57.495,7.3035));
#52445=CARTESIAN_POINT('',(55.1514258871357,54.32,7.3035));
#52446=CARTESIAN_POINT('Origin',(55.7874638715158,54.32,5.556));
#52447=CARTESIAN_POINT('',(55.7874638715158,54.32,5.556));
#52448=CARTESIAN_POINT('',(55.1514258871357,54.32,7.3035));
#52449=CARTESIAN_POINT('',(55.7874638715158,57.495,5.556));
#52450=CARTESIAN_POINT('',(55.1514258871357,57.495,7.3035));
#52451=CARTESIAN_POINT('',(55.7874638715158,54.32,5.556));
#52452=CARTESIAN_POINT('Origin',(56.4262987238946,54.32,5.556));
#52453=CARTESIAN_POINT('',(56.4262987238946,54.32,5.556));
#52454=CARTESIAN_POINT('',(55.7874638715158,54.32,5.556));
#52455=CARTESIAN_POINT('',(56.4262987238946,57.495,5.556));
#52456=CARTESIAN_POINT('',(55.7874638715158,57.495,5.556));
#52457=CARTESIAN_POINT('',(56.4262987238946,54.32,5.556));
#52458=CARTESIAN_POINT('Origin',(57.0623367082748,54.32,7.3035));
#52459=CARTESIAN_POINT('',(57.0623367082748,54.32,7.3035));
#52460=CARTESIAN_POINT('',(56.4262987238946,54.32,5.556));
#52461=CARTESIAN_POINT('',(57.0623367082747,57.495,7.3035));
#52462=CARTESIAN_POINT('',(56.4262987238946,57.495,5.556));
#52463=CARTESIAN_POINT('',(57.0623367082748,54.32,7.3035));
#52464=CARTESIAN_POINT('Origin',(57.6450650559226,54.32,7.3035));
#52465=CARTESIAN_POINT('',(57.6450650559226,54.32,7.3035));
#52466=CARTESIAN_POINT('',(57.0623367082748,54.32,7.3035));
#52467=CARTESIAN_POINT('',(57.6450650559226,57.495,7.3035));
#52468=CARTESIAN_POINT('',(57.0623367082748,57.495,7.3035));
#52469=CARTESIAN_POINT('',(57.6450650559226,54.32,7.3035));
#52470=CARTESIAN_POINT('Origin',(58.2811030403027,54.32,5.556));
#52471=CARTESIAN_POINT('',(58.2811030403027,54.32,5.556));
#52472=CARTESIAN_POINT('',(57.6450650559226,54.32,7.3035));
#52473=CARTESIAN_POINT('',(58.2811030403027,57.495,5.556));
#52474=CARTESIAN_POINT('',(57.6450650559226,57.495,7.3035));
#52475=CARTESIAN_POINT('',(58.2811030403027,54.32,5.556));
#52476=CARTESIAN_POINT('Origin',(58.9199378926815,54.32,5.556));
#52477=CARTESIAN_POINT('',(58.9199378926815,54.32,5.556));
#52478=CARTESIAN_POINT('',(58.2811030403027,54.32,5.556));
#52479=CARTESIAN_POINT('',(58.9199378926815,57.495,5.556));
#52480=CARTESIAN_POINT('',(58.2811030403027,57.495,5.556));
#52481=CARTESIAN_POINT('',(58.9199378926815,54.32,5.556));
#52482=CARTESIAN_POINT('Origin',(59.5559758770617,54.32,7.3035));
#52483=CARTESIAN_POINT('',(59.5559758770617,54.32,7.3035));
#52484=CARTESIAN_POINT('',(58.9199378926815,54.32,5.556));
#52485=CARTESIAN_POINT('',(59.5559758770617,57.495,7.3035));
#52486=CARTESIAN_POINT('',(58.9199378926815,57.495,5.556));
#52487=CARTESIAN_POINT('',(59.5559758770617,54.32,7.3035));
#52488=CARTESIAN_POINT('Origin',(60.1387042247095,54.32,7.3035));
#52489=CARTESIAN_POINT('',(60.1387042247095,54.32,7.3035));
#52490=CARTESIAN_POINT('',(59.5559758770617,54.32,7.3035));
#52491=CARTESIAN_POINT('',(60.1387042247095,57.495,7.3035));
#52492=CARTESIAN_POINT('',(59.5559758770617,57.495,7.3035));
#52493=CARTESIAN_POINT('',(60.1387042247095,54.32,7.3035));
#52494=CARTESIAN_POINT('Origin',(60.7747422090896,54.32,5.556));
#52495=CARTESIAN_POINT('',(60.7747422090896,54.32,5.556));
#52496=CARTESIAN_POINT('',(60.1387042247095,54.32,7.3035));
#52497=CARTESIAN_POINT('',(60.7747422090896,57.495,5.556));
#52498=CARTESIAN_POINT('',(60.1387042247095,57.495,7.3035));
#52499=CARTESIAN_POINT('',(60.7747422090896,54.32,5.556));
#52500=CARTESIAN_POINT('Origin',(61.4135770614684,54.32,5.556));
#52501=CARTESIAN_POINT('',(61.4135770614684,54.32,5.556));
#52502=CARTESIAN_POINT('',(60.7747422090896,54.32,5.556));
#52503=CARTESIAN_POINT('',(61.4135770614684,57.495,5.556));
#52504=CARTESIAN_POINT('',(60.7747422090896,57.495,5.556));
#52505=CARTESIAN_POINT('',(61.4135770614684,54.32,5.556));
#52506=CARTESIAN_POINT('Origin',(62.0496150458486,54.32,7.3035));
#52507=CARTESIAN_POINT('',(62.0496150458486,54.32,7.3035));
#52508=CARTESIAN_POINT('',(61.4135770614684,54.32,5.556));
#52509=CARTESIAN_POINT('',(62.0496150458486,57.495,7.3035));
#52510=CARTESIAN_POINT('',(61.4135770614684,57.495,5.556));
#52511=CARTESIAN_POINT('',(62.0496150458486,54.32,7.3035));
#52512=CARTESIAN_POINT('Origin',(62.6323433934964,54.32,7.3035));
#52513=CARTESIAN_POINT('',(62.6323433934964,54.32,7.3035));
#52514=CARTESIAN_POINT('',(62.0496150458486,54.32,7.3035));
#52515=CARTESIAN_POINT('',(62.6323433934964,57.495,7.3035));
#52516=CARTESIAN_POINT('',(62.0496150458486,57.495,7.3035));
#52517=CARTESIAN_POINT('',(62.6323433934964,54.32,7.3035));
#52518=CARTESIAN_POINT('Origin',(63.2683813778765,54.32,5.556));
#52519=CARTESIAN_POINT('',(63.2683813778765,54.32,5.556));
#52520=CARTESIAN_POINT('',(62.6323433934964,54.32,7.3035));
#52521=CARTESIAN_POINT('',(63.2683813778766,57.495,5.556));
#52522=CARTESIAN_POINT('',(62.6323433934964,57.495,7.3035));
#52523=CARTESIAN_POINT('',(63.2683813778765,54.32,5.556));
#52524=CARTESIAN_POINT('Origin',(63.9072162302553,54.32,5.556));
#52525=CARTESIAN_POINT('',(63.9072162302553,54.32,5.556));
#52526=CARTESIAN_POINT('',(63.2683813778765,54.32,5.556));
#52527=CARTESIAN_POINT('',(63.9072162302553,57.495,5.556));
#52528=CARTESIAN_POINT('',(63.2683813778765,57.495,5.556));
#52529=CARTESIAN_POINT('',(63.9072162302553,54.32,5.556));
#52530=CARTESIAN_POINT('Origin',(64.5432542146355,54.32,7.3035));
#52531=CARTESIAN_POINT('',(64.5432542146355,54.32,7.3035));
#52532=CARTESIAN_POINT('',(63.9072162302553,54.32,5.556));
#52533=CARTESIAN_POINT('',(64.5432542146355,57.495,7.3035));
#52534=CARTESIAN_POINT('',(63.9072162302553,57.495,5.556));
#52535=CARTESIAN_POINT('',(64.5432542146355,54.32,7.3035));
#52536=CARTESIAN_POINT('Origin',(65.1259825622833,54.32,7.3035));
#52537=CARTESIAN_POINT('',(65.1259825622833,54.32,7.3035));
#52538=CARTESIAN_POINT('',(64.5432542146355,54.32,7.3035));
#52539=CARTESIAN_POINT('',(65.1259825622832,57.495,7.3035));
#52540=CARTESIAN_POINT('',(64.5432542146355,57.495,7.3035));
#52541=CARTESIAN_POINT('',(65.1259825622833,54.32,7.3035));
#52542=CARTESIAN_POINT('Origin',(65.7620205466634,54.32,5.556));
#52543=CARTESIAN_POINT('',(65.7620205466634,54.32,5.556));
#52544=CARTESIAN_POINT('',(65.1259825622833,54.32,7.3035));
#52545=CARTESIAN_POINT('',(65.7620205466635,57.495,5.556));
#52546=CARTESIAN_POINT('',(65.1259825622833,57.495,7.3035));
#52547=CARTESIAN_POINT('',(65.7620205466634,54.32,5.556));
#52548=CARTESIAN_POINT('Origin',(66.4008553990422,54.32,5.556));
#52549=CARTESIAN_POINT('',(66.4008553990422,54.32,5.556));
#52550=CARTESIAN_POINT('',(65.7620205466634,54.32,5.556));
#52551=CARTESIAN_POINT('',(66.4008553990421,57.495,5.556));
#52552=CARTESIAN_POINT('',(65.7620205466634,57.495,5.556));
#52553=CARTESIAN_POINT('',(66.4008553990422,54.32,5.556));
#52554=CARTESIAN_POINT('Origin',(67.0368933834223,54.32,7.3035));
#52555=CARTESIAN_POINT('',(67.0368933834223,54.32,7.3035));
#52556=CARTESIAN_POINT('',(66.4008553990422,54.32,5.556));
#52557=CARTESIAN_POINT('',(67.0368933834224,57.495,7.3035));
#52558=CARTESIAN_POINT('',(66.4008553990422,57.495,5.556));
#52559=CARTESIAN_POINT('',(67.0368933834223,54.32,7.3035));
#52560=CARTESIAN_POINT('Origin',(67.6196217310702,54.32,7.3035));
#52561=CARTESIAN_POINT('',(67.6196217310702,54.32,7.3035));
#52562=CARTESIAN_POINT('',(67.0368933834223,54.32,7.3035));
#52563=CARTESIAN_POINT('',(67.6196217310702,57.495,7.3035));
#52564=CARTESIAN_POINT('',(67.0368933834223,57.495,7.3035));
#52565=CARTESIAN_POINT('',(67.6196217310702,54.32,7.3035));
#52566=CARTESIAN_POINT('Origin',(68.2556597154503,54.32,5.556));
#52567=CARTESIAN_POINT('',(68.2556597154503,54.32,5.556));
#52568=CARTESIAN_POINT('',(67.6196217310702,54.32,7.3035));
#52569=CARTESIAN_POINT('',(68.2556597154503,57.495,5.556));
#52570=CARTESIAN_POINT('',(67.6196217310702,57.495,7.3035));
#52571=CARTESIAN_POINT('',(68.2556597154503,54.32,5.556));
#52572=CARTESIAN_POINT('Origin',(68.8944945678291,54.32,5.556));
#52573=CARTESIAN_POINT('',(68.8944945678291,54.32,5.556));
#52574=CARTESIAN_POINT('',(68.2556597154503,54.32,5.556));
#52575=CARTESIAN_POINT('',(68.8944945678291,57.495,5.556));
#52576=CARTESIAN_POINT('',(68.2556597154503,57.495,5.556));
#52577=CARTESIAN_POINT('',(68.8944945678291,54.32,5.556));
#52578=CARTESIAN_POINT('Origin',(69.5305325522092,54.32,7.3035));
#52579=CARTESIAN_POINT('',(69.5305325522092,54.32,7.3035));
#52580=CARTESIAN_POINT('',(68.8944945678291,54.32,5.556));
#52581=CARTESIAN_POINT('',(69.5305325522092,57.495,7.3035));
#52582=CARTESIAN_POINT('',(68.8944945678291,57.495,5.556));
#52583=CARTESIAN_POINT('',(69.5305325522092,54.32,7.3035));
#52584=CARTESIAN_POINT('Origin',(70.1132608998571,54.32,7.3035));
#52585=CARTESIAN_POINT('',(70.1132608998571,54.32,7.3035));
#52586=CARTESIAN_POINT('',(69.5305325522092,54.32,7.3035));
#52587=CARTESIAN_POINT('',(70.1132608998571,57.495,7.3035));
#52588=CARTESIAN_POINT('',(69.5305325522092,57.495,7.3035));
#52589=CARTESIAN_POINT('',(70.1132608998571,54.32,7.3035));
#52590=CARTESIAN_POINT('Origin',(70.7492988842372,54.32,5.556));
#52591=CARTESIAN_POINT('',(70.7492988842372,54.32,5.556));
#52592=CARTESIAN_POINT('',(70.1132608998571,54.32,7.3035));
#52593=CARTESIAN_POINT('',(70.7492988842372,57.495,5.556));
#52594=CARTESIAN_POINT('',(70.1132608998571,57.495,7.3035));
#52595=CARTESIAN_POINT('',(70.7492988842372,54.32,5.556));
#52596=CARTESIAN_POINT('Origin',(71.388133736616,54.32,5.556));
#52597=CARTESIAN_POINT('',(71.388133736616,54.32,5.556));
#52598=CARTESIAN_POINT('',(70.7492988842372,54.32,5.556));
#52599=CARTESIAN_POINT('',(71.388133736616,57.495,5.556));
#52600=CARTESIAN_POINT('',(70.7492988842372,57.495,5.556));
#52601=CARTESIAN_POINT('',(71.388133736616,54.32,5.556));
#52602=CARTESIAN_POINT('Origin',(72.0241717209961,54.32,7.3035));
#52603=CARTESIAN_POINT('',(72.0241717209961,54.32,7.3035));
#52604=CARTESIAN_POINT('',(71.388133736616,54.32,5.556));
#52605=CARTESIAN_POINT('',(72.0241717209961,57.495,7.3035));
#52606=CARTESIAN_POINT('',(71.388133736616,57.495,5.556));
#52607=CARTESIAN_POINT('',(72.0241717209961,54.32,7.3035));
#52608=CARTESIAN_POINT('Origin',(72.606900068644,54.32,7.3035));
#52609=CARTESIAN_POINT('',(72.606900068644,54.32,7.3035));
#52610=CARTESIAN_POINT('',(72.0241717209961,54.32,7.3035));
#52611=CARTESIAN_POINT('',(72.606900068644,57.495,7.3035));
#52612=CARTESIAN_POINT('',(72.0241717209961,57.495,7.3035));
#52613=CARTESIAN_POINT('',(72.606900068644,54.32,7.3035));
#52614=CARTESIAN_POINT('Origin',(73.2429380530241,54.32,5.556));
#52615=CARTESIAN_POINT('',(73.2429380530241,54.32,5.556));
#52616=CARTESIAN_POINT('',(72.606900068644,54.32,7.3035));
#52617=CARTESIAN_POINT('',(73.2429380530241,57.495,5.556));
#52618=CARTESIAN_POINT('',(72.606900068644,57.495,7.3035));
#52619=CARTESIAN_POINT('',(73.2429380530241,54.32,5.556));
#52620=CARTESIAN_POINT('Origin',(73.8817729054029,54.32,5.556));
#52621=CARTESIAN_POINT('',(73.8817729054029,54.32,5.556));
#52622=CARTESIAN_POINT('',(73.2429380530241,54.32,5.556));
#52623=CARTESIAN_POINT('',(73.8817729054029,57.495,5.556));
#52624=CARTESIAN_POINT('',(73.2429380530241,57.495,5.556));
#52625=CARTESIAN_POINT('',(73.8817729054029,54.32,5.556));
#52626=CARTESIAN_POINT('Origin',(74.517810889783,54.32,7.3035));
#52627=CARTESIAN_POINT('',(74.517810889783,54.32,7.3035));
#52628=CARTESIAN_POINT('',(73.8817729054029,54.32,5.556));
#52629=CARTESIAN_POINT('',(74.517810889783,57.495,7.3035));
#52630=CARTESIAN_POINT('',(73.8817729054029,57.495,5.556));
#52631=CARTESIAN_POINT('',(74.517810889783,54.32,7.3035));
#52632=CARTESIAN_POINT('Origin',(75.1005392374309,54.32,7.3035));
#52633=CARTESIAN_POINT('',(75.1005392374309,54.32,7.3035));
#52634=CARTESIAN_POINT('',(74.517810889783,54.32,7.3035));
#52635=CARTESIAN_POINT('',(75.1005392374309,57.495,7.3035));
#52636=CARTESIAN_POINT('',(74.517810889783,57.495,7.3035));
#52637=CARTESIAN_POINT('',(75.1005392374309,54.32,7.3035));
#52638=CARTESIAN_POINT('Origin',(75.736577221811,54.32,5.556));
#52639=CARTESIAN_POINT('',(75.736577221811,54.32,5.556));
#52640=CARTESIAN_POINT('',(75.1005392374309,54.32,7.3035));
#52641=CARTESIAN_POINT('',(75.736577221811,57.495,5.556));
#52642=CARTESIAN_POINT('',(75.1005392374309,57.495,7.3035));
#52643=CARTESIAN_POINT('',(75.736577221811,54.32,5.556));
#52644=CARTESIAN_POINT('Origin',(76.3754120741898,54.32,5.556));
#52645=CARTESIAN_POINT('',(76.3754120741898,54.32,5.556));
#52646=CARTESIAN_POINT('',(75.736577221811,54.32,5.556));
#52647=CARTESIAN_POINT('',(76.3754120741898,57.495,5.556));
#52648=CARTESIAN_POINT('',(75.736577221811,57.495,5.556));
#52649=CARTESIAN_POINT('',(76.3754120741898,54.32,5.556));
#52650=CARTESIAN_POINT('Origin',(77.0114500585699,54.32,7.3035));
#52651=CARTESIAN_POINT('',(77.0114500585699,54.32,7.3035));
#52652=CARTESIAN_POINT('',(76.3754120741898,54.32,5.556));
#52653=CARTESIAN_POINT('',(77.0114500585699,57.495,7.3035));
#52654=CARTESIAN_POINT('',(76.3754120741898,57.495,5.556));
#52655=CARTESIAN_POINT('',(77.0114500585699,54.32,7.3035));
#52656=CARTESIAN_POINT('Origin',(77.5941784062178,54.32,7.3035));
#52657=CARTESIAN_POINT('',(77.5941784062178,54.32,7.3035));
#52658=CARTESIAN_POINT('',(77.0114500585699,54.32,7.3035));
#52659=CARTESIAN_POINT('',(77.5941784062177,57.495,7.3035));
#52660=CARTESIAN_POINT('',(77.0114500585699,57.495,7.3035));
#52661=CARTESIAN_POINT('',(77.5941784062178,54.32,7.3035));
#52662=CARTESIAN_POINT('Origin',(78.2302163905979,54.32,5.556));
#52663=CARTESIAN_POINT('',(78.2302163905979,54.32,5.556));
#52664=CARTESIAN_POINT('',(77.5941784062178,54.32,7.3035));
#52665=CARTESIAN_POINT('',(78.2302163905979,57.495,5.556));
#52666=CARTESIAN_POINT('',(77.5941784062178,57.495,7.3035));
#52667=CARTESIAN_POINT('',(78.2302163905979,54.32,5.556));
#52668=CARTESIAN_POINT('Origin',(78.8690512429767,54.32,5.556));
#52669=CARTESIAN_POINT('',(78.8690512429767,54.32,5.556));
#52670=CARTESIAN_POINT('',(78.2302163905979,54.32,5.556));
#52671=CARTESIAN_POINT('',(78.8690512429766,57.495,5.556));
#52672=CARTESIAN_POINT('',(78.2302163905979,57.495,5.556));
#52673=CARTESIAN_POINT('',(78.8690512429767,54.32,5.556));
#52674=CARTESIAN_POINT('Origin',(79.5050892273568,54.32,7.3035));
#52675=CARTESIAN_POINT('',(79.5050892273568,54.32,7.3035));
#52676=CARTESIAN_POINT('',(78.8690512429767,54.32,5.556));
#52677=CARTESIAN_POINT('',(79.5050892273568,57.495,7.3035));
#52678=CARTESIAN_POINT('',(78.8690512429767,57.495,5.556));
#52679=CARTESIAN_POINT('',(79.5050892273568,54.32,7.3035));
#52680=CARTESIAN_POINT('Origin',(80.0878175750046,54.32,7.3035));
#52681=CARTESIAN_POINT('',(80.0878175750046,54.32,7.3035));
#52682=CARTESIAN_POINT('',(79.5050892273568,54.32,7.3035));
#52683=CARTESIAN_POINT('',(80.0878175750046,57.495,7.3035));
#52684=CARTESIAN_POINT('',(79.5050892273568,57.495,7.3035));
#52685=CARTESIAN_POINT('',(80.0878175750046,54.32,7.3035));
#52686=CARTESIAN_POINT('Origin',(80.7238555593848,54.32,5.556));
#52687=CARTESIAN_POINT('',(80.7238555593848,54.32,5.556));
#52688=CARTESIAN_POINT('',(80.0878175750046,54.32,7.3035));
#52689=CARTESIAN_POINT('',(80.7238555593848,57.495,5.556));
#52690=CARTESIAN_POINT('',(80.0878175750046,57.495,7.3035));
#52691=CARTESIAN_POINT('',(80.7238555593848,54.32,5.556));
#52692=CARTESIAN_POINT('Origin',(81.3626904117636,54.32,5.556));
#52693=CARTESIAN_POINT('',(81.3626904117636,54.32,5.556));
#52694=CARTESIAN_POINT('',(80.7238555593848,54.32,5.556));
#52695=CARTESIAN_POINT('',(81.3626904117635,57.495,5.556));
#52696=CARTESIAN_POINT('',(80.7238555593848,57.495,5.556));
#52697=CARTESIAN_POINT('',(81.3626904117636,54.32,5.556));
#52698=CARTESIAN_POINT('Origin',(81.9987283961437,54.32,7.3035));
#52699=CARTESIAN_POINT('',(81.9987283961437,54.32,7.3035));
#52700=CARTESIAN_POINT('',(81.3626904117636,54.32,5.556));
#52701=CARTESIAN_POINT('',(81.9987283961437,57.495,7.3035));
#52702=CARTESIAN_POINT('',(81.3626904117636,57.495,5.556));
#52703=CARTESIAN_POINT('',(81.9987283961437,54.32,7.3035));
#52704=CARTESIAN_POINT('Origin',(82.5814567437915,54.32,7.3035));
#52705=CARTESIAN_POINT('',(82.5814567437915,54.32,7.3035));
#52706=CARTESIAN_POINT('',(81.9987283961437,54.32,7.3035));
#52707=CARTESIAN_POINT('',(82.5814567437916,57.495,7.3035));
#52708=CARTESIAN_POINT('',(81.9987283961437,57.495,7.3035));
#52709=CARTESIAN_POINT('',(82.5814567437915,54.32,7.3035));
#52710=CARTESIAN_POINT('Origin',(83.2174947281717,54.32,5.556));
#52711=CARTESIAN_POINT('',(83.2174947281717,54.32,5.556));
#52712=CARTESIAN_POINT('',(82.5814567437915,54.32,7.3035));
#52713=CARTESIAN_POINT('',(83.2174947281717,57.495,5.556));
#52714=CARTESIAN_POINT('',(82.5814567437915,57.495,7.3035));
#52715=CARTESIAN_POINT('',(83.2174947281717,54.32,5.556));
#52716=CARTESIAN_POINT('Origin',(83.8563295805504,54.32,5.556));
#52717=CARTESIAN_POINT('',(83.8563295805504,54.32,5.556));
#52718=CARTESIAN_POINT('',(83.2174947281717,54.32,5.556));
#52719=CARTESIAN_POINT('',(83.8563295805505,57.495,5.556));
#52720=CARTESIAN_POINT('',(83.2174947281717,57.495,5.556));
#52721=CARTESIAN_POINT('',(83.8563295805504,54.32,5.556));
#52722=CARTESIAN_POINT('Origin',(84.4923675649306,54.32,7.3035));
#52723=CARTESIAN_POINT('',(84.4923675649306,54.32,7.3035));
#52724=CARTESIAN_POINT('',(83.8563295805504,54.32,5.556));
#52725=CARTESIAN_POINT('',(84.4923675649306,57.495,7.3035));
#52726=CARTESIAN_POINT('',(83.8563295805504,57.495,5.556));
#52727=CARTESIAN_POINT('',(84.4923675649306,54.32,7.3035));
#52728=CARTESIAN_POINT('Origin',(85.0750959125784,54.32,7.3035));
#52729=CARTESIAN_POINT('',(85.0750959125784,54.32,7.3035));
#52730=CARTESIAN_POINT('',(84.4923675649306,54.32,7.3035));
#52731=CARTESIAN_POINT('',(85.0750959125784,57.495,7.3035));
#52732=CARTESIAN_POINT('',(84.4923675649306,57.495,7.3035));
#52733=CARTESIAN_POINT('',(85.0750959125784,54.32,7.3035));
#52734=CARTESIAN_POINT('Origin',(85.7111338969586,54.32,5.556));
#52735=CARTESIAN_POINT('',(85.7111338969586,54.32,5.556));
#52736=CARTESIAN_POINT('',(85.0750959125784,54.32,7.3035));
#52737=CARTESIAN_POINT('',(85.7111338969587,57.495,5.556));
#52738=CARTESIAN_POINT('',(85.0750959125784,57.495,7.3035));
#52739=CARTESIAN_POINT('',(85.7111338969586,54.32,5.556));
#52740=CARTESIAN_POINT('Origin',(86.3499687493374,54.32,5.556));
#52741=CARTESIAN_POINT('',(86.3499687493374,54.32,5.556));
#52742=CARTESIAN_POINT('',(85.7111338969586,54.32,5.556));
#52743=CARTESIAN_POINT('',(86.3499687493374,57.495,5.556));
#52744=CARTESIAN_POINT('',(85.7111338969586,57.495,5.556));
#52745=CARTESIAN_POINT('',(86.3499687493374,54.32,5.556));
#52746=CARTESIAN_POINT('Origin',(86.9860067337175,54.32,7.3035));
#52747=CARTESIAN_POINT('',(86.3499687493374,54.32,5.556));
#52748=CARTESIAN_POINT('',(86.3499687493374,57.495,5.556));
#52749=CARTESIAN_POINT('Origin',(0.,57.495,11.19225));
#52750=CARTESIAN_POINT('Origin',(0.,54.32,11.19225));
#52751=CARTESIAN_POINT('',(0.,0.,0.));
#52752=CARTESIAN_POINT('Origin',(19.814,44.696,24.89));
#52753=CARTESIAN_POINT('',(19.689,44.696,26.668));
#52754=CARTESIAN_POINT('Origin',(19.689,44.696,24.89));
#52755=CARTESIAN_POINT('',(19.939,44.696,26.918));
#52756=CARTESIAN_POINT('',(19.814,44.696,26.793));
#52757=CARTESIAN_POINT('Origin',(19.939,44.696,24.89));
#52758=CARTESIAN_POINT('Origin',(19.939,58.158,0.));
#52759=CARTESIAN_POINT('',(19.939,50.584,14.4732));
#52760=CARTESIAN_POINT('',(19.939,41.694,14.4732));
#52761=CARTESIAN_POINT('',(19.939,49.776,14.4732));
#52762=CARTESIAN_POINT('',(19.939,50.584,-14.4732));
#52763=CARTESIAN_POINT('',(19.939,50.584,7.0866));
#52764=CARTESIAN_POINT('',(19.939,41.694,-14.4732));
#52765=CARTESIAN_POINT('',(19.939,54.221,-14.4732));
#52766=CARTESIAN_POINT('',(19.939,41.694,-27.767));
#52767=CARTESIAN_POINT('',(19.939,41.694,-7.0866));
#52768=CARTESIAN_POINT('',(19.939,74.622,-27.767));
#52769=CARTESIAN_POINT('',(19.939,49.776,-27.767));
#52770=CARTESIAN_POINT('',(19.939,74.622,27.767));
#52771=CARTESIAN_POINT('',(19.939,74.622,-14.0335));
#52772=CARTESIAN_POINT('',(19.939,41.694,27.767));
#52773=CARTESIAN_POINT('',(19.939,66.54,27.767));
#52774=CARTESIAN_POINT('',(19.939,41.694,14.0335));
#52775=CARTESIAN_POINT('',(19.939,44.696,-16.262));
#52776=CARTESIAN_POINT('Origin',(19.939,44.696,-18.29));
#52777=CARTESIAN_POINT('',(19.939,71.6454,15.498));
#52778=CARTESIAN_POINT('Origin',(19.939,71.6454,13.47));
#52779=CARTESIAN_POINT('',(19.939,71.6454,26.918));
#52780=CARTESIAN_POINT('Origin',(19.939,71.6454,24.89));
#52781=CARTESIAN_POINT('',(19.939,44.696,20.318));
#52782=CARTESIAN_POINT('Origin',(19.939,44.696,18.29));
#52783=CARTESIAN_POINT('',(19.939,57.565,5.1));
#52784=CARTESIAN_POINT('',(19.939,54.26,5.1));
#52785=CARTESIAN_POINT('',(19.939,56.209,5.1));
#52786=CARTESIAN_POINT('',(19.939,54.26,16.892));
#52787=CARTESIAN_POINT('',(19.939,54.26,8.446));
#52788=CARTESIAN_POINT('',(19.939,63.912,16.892));
#52789=CARTESIAN_POINT('',(19.939,61.035,16.892));
#52790=CARTESIAN_POINT('',(19.939,63.912,7.24));
#52791=CARTESIAN_POINT('',(19.939,63.912,3.62));
#52792=CARTESIAN_POINT('',(19.939,57.565,7.24));
#52793=CARTESIAN_POINT('',(19.939,57.8615,7.24));
#52794=CARTESIAN_POINT('',(19.939,57.565,2.55));
#52795=CARTESIAN_POINT('',(19.939,57.565,-5.1));
#52796=CARTESIAN_POINT('',(19.939,57.565,-7.24));
#52797=CARTESIAN_POINT('',(19.939,57.565,-3.62));
#52798=CARTESIAN_POINT('',(19.939,63.912,-7.24));
#52799=CARTESIAN_POINT('',(19.939,61.035,-7.24));
#52800=CARTESIAN_POINT('',(19.939,63.912,-16.892));
#52801=CARTESIAN_POINT('',(19.939,63.912,-8.446));
#52802=CARTESIAN_POINT('',(19.939,54.26,-16.892));
#52803=CARTESIAN_POINT('',(19.939,56.209,-16.892));
#52804=CARTESIAN_POINT('',(19.939,54.26,-5.1));
#52805=CARTESIAN_POINT('',(19.939,54.26,-2.55));
#52806=CARTESIAN_POINT('',(19.939,57.8615,-5.1));
#52807=CARTESIAN_POINT('',(19.939,44.696,-22.862));
#52808=CARTESIAN_POINT('Origin',(19.939,44.696,-24.89));
#52809=CARTESIAN_POINT('',(19.939,71.6454,-11.442));
#52810=CARTESIAN_POINT('Origin',(19.939,71.6454,-13.47));
#52811=CARTESIAN_POINT('',(19.939,71.6454,-22.862));
#52812=CARTESIAN_POINT('Origin',(19.939,71.6454,-24.89));
#52813=CARTESIAN_POINT('Origin',(19.939,44.696,24.89));
#52814=CARTESIAN_POINT('',(16.764,44.696,26.668));
#52815=CARTESIAN_POINT('',(19.939,44.696,26.668));
#52816=CARTESIAN_POINT('Origin',(16.764,44.696,24.89));
#52817=CARTESIAN_POINT('Origin',(19.814,44.696,-18.29));
#52818=CARTESIAN_POINT('',(19.689,44.696,-16.512));
#52819=CARTESIAN_POINT('Origin',(19.689,44.696,-18.29));
#52820=CARTESIAN_POINT('',(19.814,44.696,-16.387));
#52821=CARTESIAN_POINT('Origin',(19.939,44.696,-18.29));
#52822=CARTESIAN_POINT('',(16.764,44.696,-16.512));
#52823=CARTESIAN_POINT('',(19.939,44.696,-16.512));
#52824=CARTESIAN_POINT('Origin',(16.764,44.696,-18.29));
#52825=CARTESIAN_POINT('Origin',(19.814,71.6454,-24.89));
#52826=CARTESIAN_POINT('',(19.689,71.6454,-23.112));
#52827=CARTESIAN_POINT('Origin',(19.689,71.6454,-24.89));
#52828=CARTESIAN_POINT('',(19.814,71.6454,-22.987));
#52829=CARTESIAN_POINT('Origin',(19.939,71.6454,-24.89));
#52830=CARTESIAN_POINT('',(16.764,71.6454,-23.112));
#52831=CARTESIAN_POINT('',(19.939,71.6454,-23.112));
#52832=CARTESIAN_POINT('Origin',(16.764,71.6454,-24.89));
#52833=CARTESIAN_POINT('Origin',(19.814,71.6454,13.47));
#52834=CARTESIAN_POINT('',(19.689,71.6454,15.248));
#52835=CARTESIAN_POINT('Origin',(19.689,71.6454,13.47));
#52836=CARTESIAN_POINT('',(19.814,71.6454,15.373));
#52837=CARTESIAN_POINT('Origin',(19.939,71.6454,13.47));
#52838=CARTESIAN_POINT('',(16.764,71.6454,15.248));
#52839=CARTESIAN_POINT('',(19.939,71.6454,15.248));
#52840=CARTESIAN_POINT('Origin',(16.764,71.6454,13.47));
#52841=CARTESIAN_POINT('Origin',(19.814,71.6454,-13.47));
#52842=CARTESIAN_POINT('',(19.689,71.6454,-11.692));
#52843=CARTESIAN_POINT('Origin',(19.689,71.6454,-13.47));
#52844=CARTESIAN_POINT('',(19.814,71.6454,-11.567));
#52845=CARTESIAN_POINT('Origin',(19.939,71.6454,-13.47));
#52846=CARTESIAN_POINT('',(16.764,71.6454,-11.692));
#52847=CARTESIAN_POINT('',(19.939,71.6454,-11.692));
#52848=CARTESIAN_POINT('Origin',(16.764,71.6454,-13.47));
#52849=CARTESIAN_POINT('Origin',(19.814,71.6454,24.89));
#52850=CARTESIAN_POINT('',(19.689,71.6454,26.668));
#52851=CARTESIAN_POINT('Origin',(19.689,71.6454,24.89));
#52852=CARTESIAN_POINT('',(19.814,71.6454,26.793));
#52853=CARTESIAN_POINT('Origin',(19.939,71.6454,24.89));
#52854=CARTESIAN_POINT('',(16.764,71.6454,26.668));
#52855=CARTESIAN_POINT('',(19.939,71.6454,26.668));
#52856=CARTESIAN_POINT('Origin',(16.764,71.6454,24.89));
#52857=CARTESIAN_POINT('Origin',(19.814,44.696,-24.89));
#52858=CARTESIAN_POINT('',(19.689,44.696,-23.112));
#52859=CARTESIAN_POINT('Origin',(19.689,44.696,-24.89));
#52860=CARTESIAN_POINT('',(19.814,44.696,-22.987));
#52861=CARTESIAN_POINT('Origin',(19.939,44.696,-24.89));
#52862=CARTESIAN_POINT('',(16.764,44.696,-23.112));
#52863=CARTESIAN_POINT('',(19.939,44.696,-23.112));
#52864=CARTESIAN_POINT('Origin',(16.764,44.696,-24.89));
#52865=CARTESIAN_POINT('Origin',(19.814,44.696,18.29));
#52866=CARTESIAN_POINT('',(19.689,44.696,20.068));
#52867=CARTESIAN_POINT('Origin',(19.689,44.696,18.29));
#52868=CARTESIAN_POINT('',(19.814,44.696,20.193));
#52869=CARTESIAN_POINT('Origin',(19.939,44.696,18.29));
#52870=CARTESIAN_POINT('',(16.764,44.696,20.068));
#52871=CARTESIAN_POINT('',(19.939,44.696,20.068));
#52872=CARTESIAN_POINT('Origin',(16.764,44.696,18.29));
#52873=CARTESIAN_POINT('Origin',(16.764,57.565,-7.24));
#52874=CARTESIAN_POINT('',(16.764,57.565,-7.24));
#52875=CARTESIAN_POINT('',(16.764,57.565,-5.1));
#52876=CARTESIAN_POINT('',(16.764,57.565,-3.62));
#52877=CARTESIAN_POINT('',(16.764,57.565,-7.24));
#52878=CARTESIAN_POINT('',(16.764,57.565,-5.1));
#52879=CARTESIAN_POINT('Origin',(16.764,63.912,-7.24));
#52880=CARTESIAN_POINT('',(16.764,63.912,-7.24));
#52881=CARTESIAN_POINT('',(16.764,61.035,-7.24));
#52882=CARTESIAN_POINT('',(16.764,63.912,-7.24));
#52883=CARTESIAN_POINT('Origin',(16.764,63.912,-16.892));
#52884=CARTESIAN_POINT('',(16.764,63.912,-16.892));
#52885=CARTESIAN_POINT('',(16.764,63.912,-8.446));
#52886=CARTESIAN_POINT('',(16.764,63.912,-16.892));
#52887=CARTESIAN_POINT('Origin',(16.764,54.26,-16.892));
#52888=CARTESIAN_POINT('',(16.764,54.26,-16.892));
#52889=CARTESIAN_POINT('',(16.764,56.209,-16.892));
#52890=CARTESIAN_POINT('',(16.764,54.26,-16.892));
#52891=CARTESIAN_POINT('Origin',(16.764,54.26,-5.1));
#52892=CARTESIAN_POINT('',(16.764,54.26,-5.1));
#52893=CARTESIAN_POINT('',(16.764,54.26,-2.55));
#52894=CARTESIAN_POINT('',(16.764,54.26,-5.1));
#52895=CARTESIAN_POINT('Origin',(16.764,57.565,-5.1));
#52896=CARTESIAN_POINT('',(16.764,57.8615,-5.1));
#52897=CARTESIAN_POINT('Origin',(16.764,54.26,5.1));
#52898=CARTESIAN_POINT('',(16.764,54.26,5.1));
#52899=CARTESIAN_POINT('',(16.764,57.565,5.1));
#52900=CARTESIAN_POINT('',(16.764,56.209,5.1));
#52901=CARTESIAN_POINT('',(16.764,54.26,5.1));
#52902=CARTESIAN_POINT('',(16.764,57.565,5.1));
#52903=CARTESIAN_POINT('Origin',(16.764,54.26,16.892));
#52904=CARTESIAN_POINT('',(16.764,54.26,16.892));
#52905=CARTESIAN_POINT('',(16.764,54.26,8.446));
#52906=CARTESIAN_POINT('',(16.764,54.26,16.892));
#52907=CARTESIAN_POINT('Origin',(16.764,63.912,16.892));
#52908=CARTESIAN_POINT('',(16.764,63.912,16.892));
#52909=CARTESIAN_POINT('',(16.764,61.035,16.892));
#52910=CARTESIAN_POINT('',(16.764,63.912,16.892));
#52911=CARTESIAN_POINT('Origin',(16.764,63.912,7.24));
#52912=CARTESIAN_POINT('',(16.764,63.912,7.24));
#52913=CARTESIAN_POINT('',(16.764,63.912,3.62));
#52914=CARTESIAN_POINT('',(16.764,63.912,7.24));
#52915=CARTESIAN_POINT('Origin',(16.764,57.565,7.24));
#52916=CARTESIAN_POINT('',(16.764,57.565,7.24));
#52917=CARTESIAN_POINT('',(16.764,57.8615,7.24));
#52918=CARTESIAN_POINT('',(16.764,57.565,7.24));
#52919=CARTESIAN_POINT('Origin',(16.764,57.565,5.1));
#52920=CARTESIAN_POINT('',(16.764,57.565,2.55));
#52921=CARTESIAN_POINT('Origin',(19.789,49.776,14.3232));
#52922=CARTESIAN_POINT('',(19.639,41.394,14.1732));
#52923=CARTESIAN_POINT('',(19.939,41.694,14.4732));
#52924=CARTESIAN_POINT('',(19.639,50.284,14.1732));
#52925=CARTESIAN_POINT('',(19.639,49.776,14.1732));
#52926=CARTESIAN_POINT('',(19.939,50.584,14.4732));
#52927=CARTESIAN_POINT('Origin',(19.789,41.544,14.0335));
#52928=CARTESIAN_POINT('',(19.639,41.394,28.067));
#52929=CARTESIAN_POINT('',(19.939,41.694,27.767));
#52930=CARTESIAN_POINT('',(19.639,41.394,14.0335));
#52931=CARTESIAN_POINT('Origin',(19.789,66.54,27.917));
#52932=CARTESIAN_POINT('',(19.639,74.922,28.067));
#52933=CARTESIAN_POINT('',(19.939,74.622,27.767));
#52934=CARTESIAN_POINT('',(19.639,66.54,28.067));
#52935=CARTESIAN_POINT('Origin',(19.789,74.772,-14.0335));
#52936=CARTESIAN_POINT('',(19.639,74.922,-28.067));
#52937=CARTESIAN_POINT('',(19.939,74.622,-27.767));
#52938=CARTESIAN_POINT('',(19.639,74.922,-14.0335));
#52939=CARTESIAN_POINT('Origin',(19.789,49.776,-27.917));
#52940=CARTESIAN_POINT('',(19.639,41.394,-28.067));
#52941=CARTESIAN_POINT('',(19.939,41.694,-27.767));
#52942=CARTESIAN_POINT('',(19.639,49.776,-28.067));
#52943=CARTESIAN_POINT('Origin',(19.789,41.544,-7.0866));
#52944=CARTESIAN_POINT('',(19.639,41.394,-14.1732));
#52945=CARTESIAN_POINT('',(19.639,41.394,-7.0866));
#52946=CARTESIAN_POINT('',(19.939,41.694,-14.4732));
#52947=CARTESIAN_POINT('Origin',(19.789,54.221,-14.3232));
#52948=CARTESIAN_POINT('',(19.639,50.284,-14.1732));
#52949=CARTESIAN_POINT('',(19.639,54.221,-14.1732));
#52950=CARTESIAN_POINT('',(19.939,50.584,-14.4732));
#52951=CARTESIAN_POINT('Origin',(19.789,50.434,7.0866));
#52952=CARTESIAN_POINT('',(19.639,50.284,7.0866));
#52953=CARTESIAN_POINT('Origin',(16.764,41.394,-14.1732));
#52954=CARTESIAN_POINT('',(16.764,41.394,-14.1732));
#52955=CARTESIAN_POINT('',(16.764,41.394,-14.1732));
#52956=CARTESIAN_POINT('',(16.764,41.394,-28.067));
#52957=CARTESIAN_POINT('',(16.764,41.394,-28.067));
#52958=CARTESIAN_POINT('',(16.764,41.394,-28.067));
#52959=CARTESIAN_POINT('Origin',(16.764,50.284,-14.1732));
#52960=CARTESIAN_POINT('',(16.764,50.284,-14.1732));
#52961=CARTESIAN_POINT('',(16.764,50.284,-14.1732));
#52962=CARTESIAN_POINT('',(16.764,41.394,-14.1732));
#52963=CARTESIAN_POINT('Origin',(16.764,50.284,14.1732));
#52964=CARTESIAN_POINT('',(16.764,50.284,14.1732));
#52965=CARTESIAN_POINT('',(16.764,50.284,14.1732));
#52966=CARTESIAN_POINT('',(16.764,50.284,-14.1732));
#52967=CARTESIAN_POINT('Origin',(16.764,41.394,14.1732));
#52968=CARTESIAN_POINT('',(16.764,41.394,14.1732));
#52969=CARTESIAN_POINT('',(16.764,41.394,14.1732));
#52970=CARTESIAN_POINT('',(16.764,50.284,14.1732));
#52971=CARTESIAN_POINT('Origin',(16.764,41.394,-28.067));
#52972=CARTESIAN_POINT('',(16.764,74.922,-28.067));
#52973=CARTESIAN_POINT('',(16.764,74.922,-28.067));
#52974=CARTESIAN_POINT('',(16.764,74.922,-28.067));
#52975=CARTESIAN_POINT('Origin',(16.764,41.394,28.067));
#52976=CARTESIAN_POINT('',(16.764,41.394,28.067));
#52977=CARTESIAN_POINT('',(16.764,41.394,28.067));
#52978=CARTESIAN_POINT('',(16.764,41.394,14.1732));
#52979=CARTESIAN_POINT('Origin',(16.764,74.922,28.067));
#52980=CARTESIAN_POINT('',(16.764,74.922,28.067));
#52981=CARTESIAN_POINT('',(16.764,74.922,28.067));
#52982=CARTESIAN_POINT('',(16.764,41.394,28.067));
#52983=CARTESIAN_POINT('Origin',(16.764,74.922,-28.067));
#52984=CARTESIAN_POINT('',(16.764,74.922,28.067));
#52985=CARTESIAN_POINT('Origin',(16.764,58.158,0.));
#52986=CARTESIAN_POINT('',(0.,0.,0.));
#52987=CARTESIAN_POINT('Origin',(5.58,44.696,15.24));
#52988=CARTESIAN_POINT('',(3.802,44.696,15.24));
#52989=CARTESIAN_POINT('Origin',(5.58,44.696,15.24));
#52990=CARTESIAN_POINT('',(3.802,44.696,21.34));
#52991=CARTESIAN_POINT('',(3.802,44.696,15.24));
#52992=CARTESIAN_POINT('Origin',(5.58,44.696,21.34));
#52993=CARTESIAN_POINT('Origin',(-5.58,44.696,15.24));
#52994=CARTESIAN_POINT('',(-7.358,44.696,15.24));
#52995=CARTESIAN_POINT('Origin',(-5.58,44.696,15.24));
#52996=CARTESIAN_POINT('',(-7.358,44.696,21.34));
#52997=CARTESIAN_POINT('',(-7.358,44.696,15.24));
#52998=CARTESIAN_POINT('Origin',(-5.58,44.696,21.34));
#52999=CARTESIAN_POINT('Origin',(-13.47,39.266,18.29));
#53000=CARTESIAN_POINT('',(-15.2725,39.416,18.29));
#53001=CARTESIAN_POINT('Origin',(-13.47,39.416,18.29));
#53002=CARTESIAN_POINT('',(-15.5725,39.116,18.29));
#53003=CARTESIAN_POINT('',(-15.4225,39.266,18.29));
#53004=CARTESIAN_POINT('Origin',(-13.47,39.116,18.29));
#53005=CARTESIAN_POINT('Origin',(-13.47,39.116,18.29));
#53006=CARTESIAN_POINT('',(-15.2725,42.8935,18.29));
#53007=CARTESIAN_POINT('',(-15.2725,39.116,18.29));
#53008=CARTESIAN_POINT('',(-14.05,44.116,19.9966359453615));
#53009=CARTESIAN_POINT('Origin',(-13.47,44.696,18.29));
#53010=CARTESIAN_POINT('',(-12.89,44.116,19.9966359453615));
#53011=CARTESIAN_POINT('Origin',(-13.47,44.116,18.29));
#53012=CARTESIAN_POINT('',(-12.89,44.116,16.5833640546385));
#53013=CARTESIAN_POINT('Origin',(-13.47,44.696,18.29));
#53014=CARTESIAN_POINT('',(-14.05,44.116,16.5833640546385));
#53015=CARTESIAN_POINT('Origin',(-13.47,44.116,18.29));
#53016=CARTESIAN_POINT('Origin',(-13.47,44.696,18.29));
#53017=CARTESIAN_POINT('Origin',(-16.764,39.116,15.24));
#53018=CARTESIAN_POINT('',(-16.764,39.116,15.24));
#53019=CARTESIAN_POINT('',(-10.42,39.116,15.24));
#53020=CARTESIAN_POINT('',(-16.764,39.116,15.24));
#53021=CARTESIAN_POINT('',(-10.42,39.116,21.34));
#53022=CARTESIAN_POINT('',(-10.42,39.116,15.24));
#53023=CARTESIAN_POINT('',(-16.764,39.116,21.34));
#53024=CARTESIAN_POINT('',(-16.764,39.116,21.34));
#53025=CARTESIAN_POINT('',(-16.764,39.116,15.24));
#53026=CARTESIAN_POINT('Origin',(13.47,39.266,18.29));
#53027=CARTESIAN_POINT('',(11.6675,39.416,18.29));
#53028=CARTESIAN_POINT('Origin',(13.47,39.416,18.29));
#53029=CARTESIAN_POINT('',(11.3675,39.116,18.29));
#53030=CARTESIAN_POINT('',(11.5175,39.266,18.29));
#53031=CARTESIAN_POINT('Origin',(13.47,39.116,18.29));
#53032=CARTESIAN_POINT('Origin',(13.47,39.116,18.29));
#53033=CARTESIAN_POINT('',(11.6675,42.8935,18.29));
#53034=CARTESIAN_POINT('',(11.6675,39.116,18.29));
#53035=CARTESIAN_POINT('',(12.89,44.116,19.9966359453615));
#53036=CARTESIAN_POINT('Origin',(13.47,44.696,18.29));
#53037=CARTESIAN_POINT('',(14.05,44.116,19.9966359453615));
#53038=CARTESIAN_POINT('Origin',(13.47,44.116,18.29));
#53039=CARTESIAN_POINT('',(14.05,44.116,16.5833640546385));
#53040=CARTESIAN_POINT('Origin',(13.47,44.696,18.29));
#53041=CARTESIAN_POINT('',(12.89,44.116,16.5833640546385));
#53042=CARTESIAN_POINT('Origin',(13.47,44.116,18.29));
#53043=CARTESIAN_POINT('Origin',(13.47,44.696,18.29));
#53044=CARTESIAN_POINT('Origin',(10.42,39.116,15.24));
#53045=CARTESIAN_POINT('',(10.42,39.116,15.24));
#53046=CARTESIAN_POINT('',(16.764,39.116,15.24));
#53047=CARTESIAN_POINT('',(10.42,39.116,15.24));
#53048=CARTESIAN_POINT('',(16.764,39.116,21.34));
#53049=CARTESIAN_POINT('',(16.764,39.116,15.24));
#53050=CARTESIAN_POINT('',(10.42,39.116,21.34));
#53051=CARTESIAN_POINT('',(10.42,39.116,21.34));
#53052=CARTESIAN_POINT('',(10.42,39.116,15.24));
#53053=CARTESIAN_POINT('Origin',(-13.47,44.6575256328986,18.29));
#53054=CARTESIAN_POINT('Ctrl Pts',(-12.89,44.116,19.9966359453615));
#53055=CARTESIAN_POINT('Ctrl Pts',(-13.0870148223526,44.1479198171785,20.0074838910021));
#53056=CARTESIAN_POINT('Ctrl Pts',(-13.282624866759,44.1642087318133,20.012267196773));
#53057=CARTESIAN_POINT('Ctrl Pts',(-13.47,44.1642087318133,20.012267196773));
#53058=CARTESIAN_POINT('Ctrl Pts',(-13.657375133241,44.1642087318133,20.012267196773));
#53059=CARTESIAN_POINT('Ctrl Pts',(-13.8529851776474,44.1479198171785,20.0074838910021));
#53060=CARTESIAN_POINT('Ctrl Pts',(-14.05,44.116,19.9966359453615));
#53061=CARTESIAN_POINT('Origin',(-13.47,44.6575256328986,18.29));
#53062=CARTESIAN_POINT('Ctrl Pts',(-14.05,44.116,16.5833640546385));
#53063=CARTESIAN_POINT('Ctrl Pts',(-13.8529851776474,44.1479198171785,16.5725161089979));
#53064=CARTESIAN_POINT('Ctrl Pts',(-13.657375133241,44.1642087318133,16.567732803227));
#53065=CARTESIAN_POINT('Ctrl Pts',(-13.282624866759,44.1642087318133,16.567732803227));
#53066=CARTESIAN_POINT('Ctrl Pts',(-13.0870148223526,44.1479198171785,16.5725161089979));
#53067=CARTESIAN_POINT('Ctrl Pts',(-12.89,44.116,16.5833640546385));
#53068=CARTESIAN_POINT('Origin',(-16.764,44.696,18.29));
#53069=CARTESIAN_POINT('',(-16.464,44.696,20.0925));
#53070=CARTESIAN_POINT('Origin',(-16.464,44.696,18.29));
#53071=CARTESIAN_POINT('',(-8.964,44.696,20.0925));
#53072=CARTESIAN_POINT('',(-16.764,44.696,20.0925));
#53073=CARTESIAN_POINT('',(-8.964,42.8935,18.29));
#53074=CARTESIAN_POINT('Origin',(-8.964,44.696,18.29));
#53075=CARTESIAN_POINT('Origin',(-8.964,44.696,18.29));
#53076=CARTESIAN_POINT('Origin',(13.47,44.6575256328986,18.29));
#53077=CARTESIAN_POINT('Ctrl Pts',(12.89,44.116,16.5833640546385));
#53078=CARTESIAN_POINT('Ctrl Pts',(13.0870148223526,44.1479198171785,16.5725161089979));
#53079=CARTESIAN_POINT('Ctrl Pts',(13.282624866759,44.1642087318133,16.567732803227));
#53080=CARTESIAN_POINT('Ctrl Pts',(13.47,44.1642087318133,16.567732803227));
#53081=CARTESIAN_POINT('Ctrl Pts',(13.657375133241,44.1642087318133,16.567732803227));
#53082=CARTESIAN_POINT('Ctrl Pts',(13.8529851776474,44.1479198171785,16.5725161089979));
#53083=CARTESIAN_POINT('Ctrl Pts',(14.05,44.116,16.5833640546385));
#53084=CARTESIAN_POINT('Origin',(13.47,44.6575256328986,18.29));
#53085=CARTESIAN_POINT('Ctrl Pts',(14.05,44.116,19.9966359453615));
#53086=CARTESIAN_POINT('Ctrl Pts',(13.8529851776474,44.1479198171785,20.0074838910021));
#53087=CARTESIAN_POINT('Ctrl Pts',(13.657375133241,44.1642087318133,20.012267196773));
#53088=CARTESIAN_POINT('Ctrl Pts',(13.282624866759,44.1642087318133,20.012267196773));
#53089=CARTESIAN_POINT('Ctrl Pts',(13.0870148223526,44.1479198171785,20.0074838910021));
#53090=CARTESIAN_POINT('Ctrl Pts',(12.89,44.116,19.9966359453615));
#53091=CARTESIAN_POINT('Origin',(16.764,44.696,18.29));
#53092=CARTESIAN_POINT('',(16.464,44.696,20.0925));
#53093=CARTESIAN_POINT('Origin',(16.464,44.696,18.29));
#53094=CARTESIAN_POINT('',(8.964,44.696,20.0925));
#53095=CARTESIAN_POINT('',(16.764,44.696,20.0925));
#53096=CARTESIAN_POINT('',(8.964,42.8935,18.29));
#53097=CARTESIAN_POINT('Origin',(8.964,44.696,18.29));
#53098=CARTESIAN_POINT('Origin',(8.964,44.696,18.29));
#53099=CARTESIAN_POINT('Origin',(-16.614,44.696,18.29));
#53100=CARTESIAN_POINT('',(-16.764,44.696,20.3925));
#53101=CARTESIAN_POINT('',(-16.614,44.696,20.2425));
#53102=CARTESIAN_POINT('Origin',(-16.764,44.696,18.29));
#53103=CARTESIAN_POINT('Origin',(-16.764,47.746,15.24));
#53104=CARTESIAN_POINT('',(-16.764,47.746,21.04));
#53105=CARTESIAN_POINT('',(-16.764,47.446,21.34));
#53106=CARTESIAN_POINT('',(-16.764,49.121,19.665));
#53107=CARTESIAN_POINT('',(-16.764,47.746,15.54));
#53108=CARTESIAN_POINT('',(-16.764,47.746,15.24));
#53109=CARTESIAN_POINT('',(-16.764,47.446,15.24));
#53110=CARTESIAN_POINT('',(-16.764,47.596,15.39));
#53111=CARTESIAN_POINT('',(-16.764,47.746,15.24));
#53112=CARTESIAN_POINT('',(-16.764,47.746,21.34));
#53113=CARTESIAN_POINT('Origin',(-8.964,44.696,18.29));
#53114=CARTESIAN_POINT('',(-7.88094873420282,44.696,18.29));
#53115=CARTESIAN_POINT('',(-8.964,42.8935,18.29));
#53116=CARTESIAN_POINT('Origin',(16.614,44.696,18.29));
#53117=CARTESIAN_POINT('',(16.764,44.696,20.3925));
#53118=CARTESIAN_POINT('',(16.614,44.696,20.2425));
#53119=CARTESIAN_POINT('Origin',(16.764,44.696,18.29));
#53120=CARTESIAN_POINT('Origin',(16.764,39.116,15.24));
#53121=CARTESIAN_POINT('',(16.764,47.446,21.34));
#53122=CARTESIAN_POINT('',(16.764,47.746,21.04));
#53123=CARTESIAN_POINT('',(16.764,46.9635,21.8225));
#53124=CARTESIAN_POINT('',(16.764,39.116,21.34));
#53125=CARTESIAN_POINT('',(16.764,47.446,15.24));
#53126=CARTESIAN_POINT('',(16.764,39.116,15.24));
#53127=CARTESIAN_POINT('',(16.764,47.746,15.54));
#53128=CARTESIAN_POINT('',(16.764,45.4385,13.2325));
#53129=CARTESIAN_POINT('',(16.764,47.746,15.24));
#53130=CARTESIAN_POINT('Origin',(8.42247436710141,44.696,18.29));
#53131=CARTESIAN_POINT('',(7.88094873420282,44.696,18.29));
#53132=CARTESIAN_POINT('',(8.42247436710141,43.79475,18.29));
#53133=CARTESIAN_POINT('Origin',(8.382,47.596,21.19));
#53134=CARTESIAN_POINT('',(8.382,47.446,21.34));
#53135=CARTESIAN_POINT('',(8.382,47.746,21.04));
#53136=CARTESIAN_POINT('Origin',(16.764,47.746,15.24));
#53137=CARTESIAN_POINT('',(8.382,47.746,15.54));
#53138=CARTESIAN_POINT('Origin',(8.382,47.596,15.39));
#53139=CARTESIAN_POINT('',(8.382,47.446,15.24));
#53140=CARTESIAN_POINT('Origin',(10.42,41.646,15.24));
#53141=CARTESIAN_POINT('',(10.42,41.646,15.24));
#53142=CARTESIAN_POINT('',(10.42,41.646,15.24));
#53143=CARTESIAN_POINT('',(10.42,41.646,21.34));
#53144=CARTESIAN_POINT('',(10.42,41.646,21.34));
#53145=CARTESIAN_POINT('',(10.42,41.646,15.24));
#53146=CARTESIAN_POINT('Origin',(-10.42,41.646,15.24));
#53147=CARTESIAN_POINT('',(-10.42,41.646,15.24));
#53148=CARTESIAN_POINT('',(-10.42,41.646,15.24));
#53149=CARTESIAN_POINT('',(-10.42,41.646,21.34));
#53150=CARTESIAN_POINT('',(-10.42,41.646,21.34));
#53151=CARTESIAN_POINT('',(-10.42,41.646,15.24));
#53152=CARTESIAN_POINT('Origin',(-10.42,39.116,15.24));
#53153=CARTESIAN_POINT('',(-10.42,39.116,15.24));
#53154=CARTESIAN_POINT('',(-10.42,39.116,21.34));
#53155=CARTESIAN_POINT('Origin',(0.,43.431,21.34));
#53156=CARTESIAN_POINT('Origin',(0.,43.431,15.24));
#53157=CARTESIAN_POINT('',(0.,0.,0.));
#53158=CARTESIAN_POINT('Origin',(21.26284859951,71.6454,13.47));
#53159=CARTESIAN_POINT('',(19.2164763792089,70.6843589395965,14.3002409771978));
#53160=CARTESIAN_POINT('',(19.3867992156006,70.6843590974191,14.3002411598846));
#53161=CARTESIAN_POINT('',(21.26284859951,70.6843589433668,14.3002409815622));
#53162=CARTESIAN_POINT('',(19.789,72.647668068024,14.249973537897));
#53163=CARTESIAN_POINT('Ctrl Pts',(19.2164763792089,70.6843589395965,14.3002409771978));
#53164=CARTESIAN_POINT('Ctrl Pts',(19.2168429075804,70.681863837098,14.2973527844721));
#53165=CARTESIAN_POINT('Ctrl Pts',(19.2172098790625,70.679381571615,14.2944531325613));
#53166=CARTESIAN_POINT('Ctrl Pts',(19.2203735586003,70.6581199751139,14.2693885665096));
#53167=CARTESIAN_POINT('Ctrl Pts',(19.2231939759151,70.6400952029175,14.2465989227062));
#53168=CARTESIAN_POINT('Ctrl Pts',(19.2283298761436,70.6090614176701,14.2044687577327));
#53169=CARTESIAN_POINT('Ctrl Pts',(19.2306334126591,70.5957730093062,14.1853495767784));
#53170=CARTESIAN_POINT('Ctrl Pts',(19.2358933228042,70.566899472208,14.1412689611443));
#53171=CARTESIAN_POINT('Ctrl Pts',(19.2388601162184,70.5516421023775,14.1161104475929));
#53172=CARTESIAN_POINT('Ctrl Pts',(19.245306516531,70.5207313108932,14.0609034025463));
#53173=CARTESIAN_POINT('Ctrl Pts',(19.248793395299,70.5053792974457,14.0307127787972));
#53174=CARTESIAN_POINT('Ctrl Pts',(19.260638083729,70.4577964388134,13.9270844769763));
#53175=CARTESIAN_POINT('Ctrl Pts',(19.2691208238696,70.4313164707027,13.851218962717));
#53176=CARTESIAN_POINT('Ctrl Pts',(19.2811264822653,70.403892231256,13.7397374214405));
#53177=CARTESIAN_POINT('Ctrl Pts',(19.2847231573083,70.3969964706005,13.7057732353553));
#53178=CARTESIAN_POINT('Ctrl Pts',(19.2899042395514,70.3889490281663,13.6557116143545));
#53179=CARTESIAN_POINT('Ctrl Pts',(19.2915324535741,70.3867011485181,13.6398091350018));
#53180=CARTESIAN_POINT('Ctrl Pts',(19.2945437089717,70.3830668610433,13.6100331070147));
#53181=CARTESIAN_POINT('Ctrl Pts',(19.295929794351,70.3816062560078,13.596173036667));
#53182=CARTESIAN_POINT('Ctrl Pts',(19.2997078124637,70.3782205834204,13.558030982768));
#53183=CARTESIAN_POINT('Ctrl Pts',(19.3020765616023,70.3767652524541,13.5337124428857));
#53184=CARTESIAN_POINT('Ctrl Pts',(19.3112196809774,70.3738224559109,13.4388155969604));
#53185=CARTESIAN_POINT('Ctrl Pts',(19.3178124549841,70.3775195642012,13.3681986156259));
#53186=CARTESIAN_POINT('Ctrl Pts',(19.3303011348092,70.3954907639043,13.2365338949063));
#53187=CARTESIAN_POINT('Ctrl Pts',(19.336170246313,70.4084416179811,13.1755310944575));
#53188=CARTESIAN_POINT('Ctrl Pts',(19.3449414390738,70.4338472116275,13.0880715213876));
#53189=CARTESIAN_POINT('Ctrl Pts',(19.3477390753848,70.4428192040899,13.0606973585204));
#53190=CARTESIAN_POINT('Ctrl Pts',(19.3528559857273,70.4607239213449,13.0117574570982));
#53191=CARTESIAN_POINT('Ctrl Pts',(19.3551639014561,70.4693356376713,12.9900874270695));
#53192=CARTESIAN_POINT('Ctrl Pts',(19.3604659406686,70.4902952193295,12.9413034783983));
#53193=CARTESIAN_POINT('Ctrl Pts',(19.3634711651694,70.5030099694296,12.9143636854465));
#53194=CARTESIAN_POINT('Ctrl Pts',(19.3700228310512,70.5324665265379,12.8572450724786));
#53195=CARTESIAN_POINT('Ctrl Pts',(19.3735771176978,70.5495150216147,12.8272518836919));
#53196=CARTESIAN_POINT('Ctrl Pts',(19.3859489294713,70.6124930226616,12.7262596317474));
#53197=CARTESIAN_POINT('Ctrl Pts',(19.3949053466999,70.6642753087591,12.6591736926245));
#53198=CARTESIAN_POINT('Ctrl Pts',(19.4070481448538,70.7442249556762,12.574567306746));
#53199=CARTESIAN_POINT('Ctrl Pts',(19.4103473619394,70.7669863786179,12.5522276023595));
#53200=CARTESIAN_POINT('Ctrl Pts',(19.4151268096689,70.8016787093509,12.5206527915009));
#53201=CARTESIAN_POINT('Ctrl Pts',(19.4166459995177,70.8129697896658,12.5107368649377));
#53202=CARTESIAN_POINT('Ctrl Pts',(19.4195932073838,70.8354252412169,12.4917115085214));
#53203=CARTESIAN_POINT('Ctrl Pts',(19.4210218878832,70.8465736314974,12.4825872339658));
#53204=CARTESIAN_POINT('Ctrl Pts',(19.4251914134929,70.8798241201264,12.45630563044));
#53205=CARTESIAN_POINT('Ctrl Pts',(19.4278994890532,70.902342629105,12.4396850803356));
#53206=CARTESIAN_POINT('Ctrl Pts',(19.4347054728509,70.9608637271432,12.3994094951654));
#53207=CARTESIAN_POINT('Ctrl Pts',(19.4387619929617,70.9975545483525,12.3768161769161));
#53208=CARTESIAN_POINT('Ctrl Pts',(19.4508471703472,71.110373258616,12.315024619423));
#53209=CARTESIAN_POINT('Ctrl Pts',(19.4588265941442,71.1893737152542,12.2816148369606));
#53210=CARTESIAN_POINT('Ctrl Pts',(19.4698025389508,71.2982724301739,12.2480305189914));
#53211=CARTESIAN_POINT('Ctrl Pts',(19.4725621440301,71.3256885414681,12.2405727938614));
#53212=CARTESIAN_POINT('Ctrl Pts',(19.4776248489093,71.3758648007065,12.2287155892559));
#53213=CARTESIAN_POINT('Ctrl Pts',(19.4799170825887,71.3985398628625,12.2240079817857));
#53214=CARTESIAN_POINT('Ctrl Pts',(19.4851976209107,71.4505879456488,12.2146785881989));
#53215=CARTESIAN_POINT('Ctrl Pts',(19.4881972703673,71.4800185947512,12.2104634964333));
#53216=CARTESIAN_POINT('Ctrl Pts',(19.4947439182504,71.5438588165329,12.2035960665193));
#53217=CARTESIAN_POINT('Ctrl Pts',(19.4982989405825,71.5782828528241,12.2013060533782));
#53218=CARTESIAN_POINT('Ctrl Pts',(19.5107312255758,71.6978178066059,12.1982323250094));
#53219=CARTESIAN_POINT('Ctrl Pts',(19.5197495849094,71.7828786800747,12.2045994047425));
#53220=CARTESIAN_POINT('Ctrl Pts',(19.5318875764421,71.8974776408687,12.2248749813478));
#53221=CARTESIAN_POINT('Ctrl Pts',(19.5351259120864,71.9280869601518,12.2314653790781));
#53222=CARTESIAN_POINT('Ctrl Pts',(19.5398337800826,71.9728712918292,12.2428550418573));
#53223=CARTESIAN_POINT('Ctrl Pts',(19.5413409228134,71.9872531055494,12.2467834505386));
#53224=CARTESIAN_POINT('Ctrl Pts',(19.5442942608923,72.015562915247,12.2550546821376));
#53225=CARTESIAN_POINT('Ctrl Pts',(19.5457407640702,72.0294918319582,12.259386005918));
#53226=CARTESIAN_POINT('Ctrl Pts',(19.5499984136167,72.0705925315987,12.2729475282185));
#53227=CARTESIAN_POINT('Ctrl Pts',(19.5527751996227,72.0975318150761,12.2828603534509));
#53228=CARTESIAN_POINT('Ctrl Pts',(19.5598205255003,72.1656581354462,12.3105850170304));
#53229=CARTESIAN_POINT('Ctrl Pts',(19.5640444489924,72.2062799415021,12.3296816135803));
#53230=CARTESIAN_POINT('Ctrl Pts',(19.5759528630704,72.3179256393901,12.3895801636631));
#53231=CARTESIAN_POINT('Ctrl Pts',(19.5836016786601,72.3861247366692,12.4351462409573));
#53232=CARTESIAN_POINT('Ctrl Pts',(19.5942649102365,72.4718197969328,12.5052385828239));
#53233=CARTESIAN_POINT('Ctrl Pts',(19.5970708789752,72.4935448817875,12.5242811033578));
#53234=CARTESIAN_POINT('Ctrl Pts',(19.6022046167316,72.5316602332081,12.5600602738273));
#53235=CARTESIAN_POINT('Ctrl Pts',(19.604521012432,72.5482729755313,12.5765417091077));
#53236=CARTESIAN_POINT('Ctrl Pts',(19.6098466804553,72.585077824801,12.6151307265006));
#53237=CARTESIAN_POINT('Ctrl Pts',(19.612867158386,72.6049614312251,12.637511336186));
#53238=CARTESIAN_POINT('Ctrl Pts',(19.6194588098718,72.6461681550016,12.6873320196457));
#53239=CARTESIAN_POINT('Ctrl Pts',(19.623037963183,72.6671927970557,12.7149867203004));
#53240=CARTESIAN_POINT('Ctrl Pts',(19.6356191537873,72.7364351073826,12.8142616228827));
#53241=CARTESIAN_POINT('Ctrl Pts',(19.6447635263264,72.7784644025375,12.8899017016047));
#53242=CARTESIAN_POINT('Ctrl Pts',(19.6568859224128,72.8243704710686,12.9968876180625));
#53243=CARTESIAN_POINT('Ctrl Pts',(19.6599963790701,72.8352575146703,13.02497615349));
#53244=CARTESIAN_POINT('Ctrl Pts',(19.6645720017463,72.8500065262947,13.0674536794229));
#53245=CARTESIAN_POINT('Ctrl Pts',(19.6660713638686,72.8546305486713,13.0815646861551));
#53246=CARTESIAN_POINT('Ctrl Pts',(19.6690754581906,72.8634810902459,13.1102653333141));
#53247=CARTESIAN_POINT('Ctrl Pts',(19.6705794803392,72.8676955066706,13.1248560476031));
#53248=CARTESIAN_POINT('Ctrl Pts',(19.6752168388686,72.8799792249048,13.170434856023));
#53249=CARTESIAN_POINT('Ctrl Pts',(19.6783069432916,72.8871399328896,13.2016576698065));
#53250=CARTESIAN_POINT('Ctrl Pts',(19.686625634525,72.9033779104689,13.2871882636698));
#53251=CARTESIAN_POINT('Ctrl Pts',(19.6917879714546,72.9101180824344,13.3418687883531));
#53252=CARTESIAN_POINT('Ctrl Pts',(19.7029309147804,72.9169394823104,13.4600500361316));
#53253=CARTESIAN_POINT('Ctrl Pts',(19.7089034057813,72.9158535470839,13.5234594134692));
#53254=CARTESIAN_POINT('Ctrl Pts',(19.7177908111219,72.9073934457991,13.615282351177));
#53255=CARTESIAN_POINT('Ctrl Pts',(19.7205984160596,72.9037628881701,13.6439452880197));
#53256=CARTESIAN_POINT('Ctrl Pts',(19.725726796497,72.8954411422604,13.6954794733644));
#53257=CARTESIAN_POINT('Ctrl Pts',(19.7280361519483,72.8910903866998,13.718393105371));
#53258=CARTESIAN_POINT('Ctrl Pts',(19.7333880858738,72.8796506962368,13.7707338614926));
#53259=CARTESIAN_POINT('Ctrl Pts',(19.73644264786,72.8721359288739,13.8000518319183));
#53260=CARTESIAN_POINT('Ctrl Pts',(19.7474350955257,72.8416656876718,13.9034251323406));
#53261=CARTESIAN_POINT('Ctrl Pts',(19.7555375219246,72.8129916041973,13.9756029856989));
#53262=CARTESIAN_POINT('Ctrl Pts',(19.7703697319023,72.7491901579731,14.1013317241615));
#53263=CARTESIAN_POINT('Ctrl Pts',(19.7770595157045,72.7162445241044,14.1557303774103));
#53264=CARTESIAN_POINT('Ctrl Pts',(19.7849207425938,72.6718520992,14.2179728876546));
#53265=CARTESIAN_POINT('Ctrl Pts',(19.7862437452096,72.6641794033323,14.2283903497352));
#53266=CARTESIAN_POINT('Ctrl Pts',(19.788039790452,72.6534761011556,14.2424668884386));
#53267=CARTESIAN_POINT('Ctrl Pts',(19.7885205481825,72.6505826200053,14.2462283308591));
#53268=CARTESIAN_POINT('Ctrl Pts',(19.789,72.647668068024,14.249973537897));
#53269=CARTESIAN_POINT('',(19.789,72.6399444526778,12.6802017145829));
#53270=CARTESIAN_POINT('Origin',(19.789,71.6454,13.47));
#53271=CARTESIAN_POINT('Ctrl Pts',(19.789,72.6399444526778,12.6802017145829));
#53272=CARTESIAN_POINT('Ctrl Pts',(19.7879988394882,72.6336852930391,12.672319939436));
#53273=CARTESIAN_POINT('Ctrl Pts',(19.7870028556559,72.6273323603128,12.6645124714419));
#53274=CARTESIAN_POINT('Ctrl Pts',(19.7847784439559,72.6128720806095,12.6471668188866));
#53275=CARTESIAN_POINT('Ctrl Pts',(19.7835526048889,72.6047150907637,12.6376711834672));
#53276=CARTESIAN_POINT('Ctrl Pts',(19.7773813155715,72.5627506193215,12.5902565904165));
#53277=CARTESIAN_POINT('Ctrl Pts',(19.7725303707011,72.5268266800043,12.5542659926393));
#53278=CARTESIAN_POINT('Ctrl Pts',(19.7617685551579,72.4422971478315,12.4791768851631));
#53279=CARTESIAN_POINT('Ctrl Pts',(19.7558780378122,72.3927802509567,12.4413126180756));
#53280=CARTESIAN_POINT('Ctrl Pts',(19.7462334159638,72.3087868944108,12.3863620821621));
#53281=CARTESIAN_POINT('Ctrl Pts',(19.7425421902648,72.2759649348693,12.3669403329942));
#53282=CARTESIAN_POINT('Ctrl Pts',(19.736254889877,72.2193745096782,12.3368057594637));
#53283=CARTESIAN_POINT('Ctrl Pts',(19.7336854247468,72.1960588739323,12.3252945758548));
#53284=CARTESIAN_POINT('Ctrl Pts',(19.7281348856773,72.1454268695547,12.3022018303799));
#53285=CARTESIAN_POINT('Ctrl Pts',(19.7251484813524,72.1180255286648,12.2908459830346));
#53286=CARTESIAN_POINT('Ctrl Pts',(19.7140452233699,72.0157999892946,12.2526164872599));
#53287=CARTESIAN_POINT('Ctrl Pts',(19.7057531723403,71.9389123233391,12.2318303828563));
#53288=CARTESIAN_POINT('Ctrl Pts',(19.6913527117728,71.8044342218704,12.2087084287361));
#53289=CARTESIAN_POINT('Ctrl Pts',(19.6853095854195,71.7476766647075,12.2028424775483));
#53290=CARTESIAN_POINT('Ctrl Pts',(19.6768504473155,71.6669693918566,12.1999608821039));
#53291=CARTESIAN_POINT('Ctrl Pts',(19.6743762563562,71.6432020505806,12.1997795629759));
#53292=CARTESIAN_POINT('Ctrl Pts',(19.669947988605,71.6002578236911,12.200657509051));
#53293=CARTESIAN_POINT('Ctrl Pts',(19.6679860457168,71.5810833269988,12.2014844546591));
#53294=CARTESIAN_POINT('Ctrl Pts',(19.6647026309535,71.5486777115068,12.2036188307956));
#53295=CARTESIAN_POINT('Ctrl Pts',(19.6633704522261,71.5354361464308,12.2046998399272));
#53296=CARTESIAN_POINT('Ctrl Pts',(19.6602845196912,71.5045364833099,12.2077112635583));
#53297=CARTESIAN_POINT('Ctrl Pts',(19.6585393557641,71.4868974890424,12.2098045934731));
#53298=CARTESIAN_POINT('Ctrl Pts',(19.6498582440392,71.3986097154966,12.2221656500283));
#53299=CARTESIAN_POINT('Ctrl Pts',(19.6431693056601,71.3288603498329,12.2380088120933));
#53300=CARTESIAN_POINT('Ctrl Pts',(19.6293829670148,71.1888474772813,12.2824984306449));
#53301=CARTESIAN_POINT('Ctrl Pts',(19.6223084569495,71.1190850290944,12.311729570797));
#53302=CARTESIAN_POINT('Ctrl Pts',(19.6124496507591,71.0286864704104,12.3594687047662));
#53303=CARTESIAN_POINT('Ctrl Pts',(19.6098485541804,71.0054387019098,12.3727012160118));
#53304=CARTESIAN_POINT('Ctrl Pts',(19.6050255725437,70.9635718536933,12.3983146807423));
#53305=CARTESIAN_POINT('Ctrl Pts',(19.6028126646699,70.9448283893441,12.410472605138));
#53306=CARTESIAN_POINT('Ctrl Pts',(19.5977221940172,70.9028369999673,12.4393116639029));
#53307=CARTESIAN_POINT('Ctrl Pts',(19.5948337905242,70.8798137824313,12.4562960714327));
#53308=CARTESIAN_POINT('Ctrl Pts',(19.5841226200794,70.797485542498,12.5214351470659));
#53309=CARTESIAN_POINT('Ctrl Pts',(19.5761269612599,70.7419955868275,12.5741261346011));
#53310=CARTESIAN_POINT('Ctrl Pts',(19.5627784869408,70.6585251082356,12.669072493034));
#53311=CARTESIAN_POINT('Ctrl Pts',(19.5574781612633,70.6277176693713,12.7085999416123));
#53312=CARTESIAN_POINT('Ctrl Pts',(19.5499662115609,70.5869744350306,12.7677823866825));
#53313=CARTESIAN_POINT('Ctrl Pts',(19.5477032092482,70.5750879154414,12.7860362186686));
#53314=CARTESIAN_POINT('Ctrl Pts',(19.5436336555357,70.5543660060603,12.819722713213));
#53315=CARTESIAN_POINT('Ctrl Pts',(19.5418202203562,70.5453738894984,12.8350524380318));
#53316=CARTESIAN_POINT('Ctrl Pts',(19.5387084575586,70.5303372145233,12.8619658983364));
#53317=CARTESIAN_POINT('Ctrl Pts',(19.5374020074727,70.5241452364414,12.8734614197647));
#53318=CARTESIAN_POINT('Ctrl Pts',(19.5342433060912,70.5094867933954,12.9017101196916));
#53319=CARTESIAN_POINT('Ctrl Pts',(19.532402211052,70.5012123517248,12.9185591906536));
#53320=CARTESIAN_POINT('Ctrl Pts',(19.5245275905332,70.4671254145594,12.9920437533232));
#53321=CARTESIAN_POINT('Ctrl Pts',(19.5186670208826,70.445118143105,13.0503583479718));
#53322=CARTESIAN_POINT('Ctrl Pts',(19.505389113183,70.4050624171872,13.1858947310944));
#53323=CARTESIAN_POINT('Ctrl Pts',(19.4980018544375,70.389784631206,13.263647936012));
#53324=CARTESIAN_POINT('Ctrl Pts',(19.4875001249208,70.3787966095861,13.3723817903781));
#53325=CARTESIAN_POINT('Ctrl Pts',(19.4845703988531,70.376832553647,13.4025480942954));
#53326=CARTESIAN_POINT('Ctrl Pts',(19.4793007955481,70.3752560384368,13.4562790365754));
#53327=CARTESIAN_POINT('Ctrl Pts',(19.4769748788724,70.3752199411901,13.4798176295983));
#53328=CARTESIAN_POINT('Ctrl Pts',(19.4717346745804,70.3765998513407,13.5323607598734));
#53329=CARTESIAN_POINT('Ctrl Pts',(19.4688113226574,70.3783565953324,13.5613419568591));
#53330=CARTESIAN_POINT('Ctrl Pts',(19.4591533400977,70.3873460382674,13.6558680040669));
#53331=CARTESIAN_POINT('Ctrl Pts',(19.4523070297242,70.3986879227047,13.7209038937591));
#53332=CARTESIAN_POINT('Ctrl Pts',(19.4398511109362,70.4281474718696,13.836061332478));
#53333=CARTESIAN_POINT('Ctrl Pts',(19.4342764055587,70.4444692454006,13.8864975665481));
#53334=CARTESIAN_POINT('Ctrl Pts',(19.4254955442047,70.4754023224365,13.9649649865178));
#53335=CARTESIAN_POINT('Ctrl Pts',(19.4222532025384,70.4879916706145,13.9937282944117));
#53336=CARTESIAN_POINT('Ctrl Pts',(19.4175229582569,70.5081964536159,14.0355934572513));
#53337=CARTESIAN_POINT('Ctrl Pts',(19.4159984281185,70.514999931154,14.0490713494076));
#53338=CARTESIAN_POINT('Ctrl Pts',(19.4129954177348,70.5290043609389,14.0756265349366));
#53339=CARTESIAN_POINT('Ctrl Pts',(19.4115170092043,70.5361986872056,14.0887044839687));
#53340=CARTESIAN_POINT('Ctrl Pts',(19.4071386715044,70.5583618679716,14.1273631674709));
#53341=CARTESIAN_POINT('Ctrl Pts',(19.4042749414895,70.5739985221918,14.1525522286725));
#53342=CARTESIAN_POINT('Ctrl Pts',(19.3964964233314,70.6192749395329,14.2200913337217));
#53343=CARTESIAN_POINT('Ctrl Pts',(19.3916486420623,70.6506210044543,14.2611878234796));
#53344=CARTESIAN_POINT('Ctrl Pts',(19.3867992156006,70.6843590974191,14.3002411598846));
#53345=CARTESIAN_POINT('Origin',(21.26284859951,71.6454,13.47));
#53346=CARTESIAN_POINT('',(18.4247393426037,70.684358943376,14.3002409815728));
#53347=CARTESIAN_POINT('',(18.5941331801233,70.6843589436049,14.3002409818378));
#53348=CARTESIAN_POINT('',(21.26284859951,70.6843589433668,14.3002409815622));
#53349=CARTESIAN_POINT('Ctrl Pts',(18.4247393426037,70.684358943376,14.3002409815728));
#53350=CARTESIAN_POINT('Ctrl Pts',(18.425741837683,70.677743151105,14.2925829062241));
#53351=CARTESIAN_POINT('Ctrl Pts',(18.426738253587,70.6712186152227,14.2848454309185));
#53352=CARTESIAN_POINT('Ctrl Pts',(18.4310008909796,70.6435570992383,14.251234236303));
#53353=CARTESIAN_POINT('Ctrl Pts',(18.4342130005463,70.62335075497,14.2246072170568));
#53354=CARTESIAN_POINT('Ctrl Pts',(18.4451512763027,70.557562841565,14.1304153569593));
#53355=CARTESIAN_POINT('Ctrl Pts',(18.4527090504329,70.5174438461248,14.0592829745899));
#53356=CARTESIAN_POINT('Ctrl Pts',(18.4636331169903,70.4706142053097,13.9536708102035));
#53357=CARTESIAN_POINT('Ctrl Pts',(18.4668715850954,70.4580719728617,13.9220076591756));
#53358=CARTESIAN_POINT('Ctrl Pts',(18.4729847990637,70.4370577292689,13.8620209287228));
#53359=CARTESIAN_POINT('Ctrl Pts',(18.4758486955719,70.428273161499,13.8338315433662));
#53360=CARTESIAN_POINT('Ctrl Pts',(18.4810269221752,70.4143335579837,13.7829170210937));
#53361=CARTESIAN_POINT('Ctrl Pts',(18.483328303393,70.4088065798096,13.7603070505413));
#53362=CARTESIAN_POINT('Ctrl Pts',(18.4885356144993,70.3978094517496,13.709279624219));
#53363=CARTESIAN_POINT('Ctrl Pts',(18.491450989609,70.3926834048692,13.680802528491));
#53364=CARTESIAN_POINT('Ctrl Pts',(18.5024808275012,70.3771409462211,13.5735734785334));
#53365=CARTESIAN_POINT('Ctrl Pts',(18.5107762815057,70.3731487127085,13.4940889856527));
#53366=CARTESIAN_POINT('Ctrl Pts',(18.5239525363185,70.3785970503642,13.3689271249055));
#53367=CARTESIAN_POINT('Ctrl Pts',(18.5287838083082,70.3830755652537,13.3232250803623));
#53368=CARTESIAN_POINT('Ctrl Pts',(18.5365832358525,70.394411456068,13.2491585425132));
#53369=CARTESIAN_POINT('Ctrl Pts',(18.5395816522431,70.3997885703953,13.2206090407001));
#53370=CARTESIAN_POINT('Ctrl Pts',(18.5440235569083,70.4093357795369,13.1780090611116));
#53371=CARTESIAN_POINT('Ctrl Pts',(18.5454989030837,70.4127770063366,13.1638070835307));
#53372=CARTESIAN_POINT('Ctrl Pts',(18.5484508306831,70.4202214396926,13.1352470496773));
#53373=CARTESIAN_POINT('Ctrl Pts',(18.5499267264548,70.4242337721853,13.1208937637423));
#53374=CARTESIAN_POINT('Ctrl Pts',(18.5544368803024,70.4373710838782,13.0768998218101));
#53375=CARTESIAN_POINT('Ctrl Pts',(18.5574299679871,70.447330451625,13.0475174934628));
#53376=CARTESIAN_POINT('Ctrl Pts',(18.5672561716199,70.4838962940663,12.9513764204617));
#53377=CARTESIAN_POINT('Ctrl Pts',(18.5739450902649,70.5150891527752,12.8865102397918));
#53378=CARTESIAN_POINT('Ctrl Pts',(18.584531299636,70.5722362610615,12.7896557921468));
#53379=CARTESIAN_POINT('Ctrl Pts',(18.5883696803837,70.5945332513164,12.755698062384));
#53380=CARTESIAN_POINT('Ctrl Pts',(18.5954163945729,70.6378460445888,12.6961616468645));
#53381=CARTESIAN_POINT('Ctrl Pts',(18.5986057031769,70.6583077968545,12.6702254514615));
#53382=CARTESIAN_POINT('Ctrl Pts',(18.6041314029079,70.6950198077227,12.6272486530822));
#53383=CARTESIAN_POINT('Ctrl Pts',(18.606447414308,70.7107764233039,12.609807618483));
#53384=CARTESIAN_POINT('Ctrl Pts',(18.6114353914224,70.7454265991816,12.5735296411886));
#53385=CARTESIAN_POINT('Ctrl Pts',(18.614111999859,70.7644477113742,12.5548311508484));
#53386=CARTESIAN_POINT('Ctrl Pts',(18.6230514054813,70.8292754194238,12.4949975469171));
#53387=CARTESIAN_POINT('Ctrl Pts',(18.629417008987,70.8774760617912,12.4566001537864));
#53388=CARTESIAN_POINT('Ctrl Pts',(18.642452446823,70.9802527148792,12.3862806296208));
#53389=CARTESIAN_POINT('Ctrl Pts',(18.6491085557561,71.0348184245439,12.3546262370709));
#53390=CARTESIAN_POINT('Ctrl Pts',(18.6582392870559,71.1134623988977,12.3165106668744));
#53391=CARTESIAN_POINT('Ctrl Pts',(18.6607746650606,71.1357213872924,12.3065039086482));
#53392=CARTESIAN_POINT('Ctrl Pts',(18.6652822071527,71.1761733835701,12.2897022520299));
#53393=CARTESIAN_POINT('Ctrl Pts',(18.6672627623462,71.1942601728435,12.2826713192427));
#53394=CARTESIAN_POINT('Ctrl Pts',(18.6705766991242,71.225123269539,12.271481044188));
#53395=CARTESIAN_POINT('Ctrl Pts',(18.6719206729941,71.2378157227746,12.2671054329145));
#53396=CARTESIAN_POINT('Ctrl Pts',(18.6751100446828,71.268354504273,12.2571164384364));
#53397=CARTESIAN_POINT('Ctrl Pts',(18.6769452671747,71.2862597317993,12.2516945187455));
#53398=CARTESIAN_POINT('Ctrl Pts',(18.6852311740424,71.3683470179891,12.2288048565841));
#53399=CARTESIAN_POINT('Ctrl Pts',(18.6914817290103,71.4337293142145,12.2159975481437));
#53400=CARTESIAN_POINT('Ctrl Pts',(18.7028746761604,71.5542198965642,12.202094430482));
#53401=CARTESIAN_POINT('Ctrl Pts',(18.7080048237426,71.6089618895223,12.1993426730394));
#53402=CARTESIAN_POINT('Ctrl Pts',(18.7149849456307,71.6823568457297,12.2004008361423));
#53403=CARTESIAN_POINT('Ctrl Pts',(18.7167661545181,71.7009964481357,12.2010804528747));
#53404=CARTESIAN_POINT('Ctrl Pts',(18.7214712191112,71.7498942503459,12.2039427274346));
#53405=CARTESIAN_POINT('Ctrl Pts',(18.7244104326693,71.7800987532055,12.2067993152529));
#53406=CARTESIAN_POINT('Ctrl Pts',(18.7296657776108,71.8332681954377,12.2137563011357));
#53407=CARTESIAN_POINT('Ctrl Pts',(18.7319672570578,71.8562774919834,12.2174133974531));
#53408=CARTESIAN_POINT('Ctrl Pts',(18.7371035289255,71.9069302170527,12.2268992316055));
#53409=CARTESIAN_POINT('Ctrl Pts',(18.7399463531597,71.9345049480494,12.2330215904059));
#53410=CARTESIAN_POINT('Ctrl Pts',(18.7517212305061,72.0466684808723,12.2618799734655));
#53411=CARTESIAN_POINT('Ctrl Pts',(18.76088556572,72.1289843684963,12.292413420382));
#53412=CARTESIAN_POINT('Ctrl Pts',(18.7745076957934,72.2451074152659,12.3497272481955));
#53413=CARTESIAN_POINT('Ctrl Pts',(18.7789187575112,72.2817864543717,12.3701487751323));
#53414=CARTESIAN_POINT('Ctrl Pts',(18.7861460998922,72.3407787665375,12.4069345453571));
#53415=CARTESIAN_POINT('Ctrl Pts',(18.7889883744013,72.3636900159105,12.4222788567443));
#53416=CARTESIAN_POINT('Ctrl Pts',(18.7932539191645,72.3977732989133,12.4467495813929));
#53417=CARTESIAN_POINT('Ctrl Pts',(18.7947055623812,72.4093182927454,12.4553394999471));
#53418=CARTESIAN_POINT('Ctrl Pts',(18.79765988588,72.4327308716207,12.4733856214846));
#53419=CARTESIAN_POINT('Ctrl Pts',(18.799161083622,72.4445798921469,12.4828618626807));
#53420=CARTESIAN_POINT('Ctrl Pts',(18.8038846964512,72.4816240808016,12.5135923548317));
#53421=CARTESIAN_POINT('Ctrl Pts',(18.8070599379444,72.5061655313132,12.5356180770225));
#53422=CARTESIAN_POINT('Ctrl Pts',(18.8181491769481,72.589626760429,12.6166070242412));
#53423=CARTESIAN_POINT('Ctrl Pts',(18.8258747786941,72.6435749784694,12.6803848022371));
#53424=CARTESIAN_POINT('Ctrl Pts',(18.8369962934314,72.7103646447034,12.7772322428483));
#53425=CARTESIAN_POINT('Ctrl Pts',(18.8402585235291,72.7286867616725,12.8062483155181));
#53426=CARTESIAN_POINT('Ctrl Pts',(18.8464092783241,72.760621014105,12.861672662604));
#53427=CARTESIAN_POINT('Ctrl Pts',(18.8492866633893,72.7745246579151,12.8878855406901));
#53428=CARTESIAN_POINT('Ctrl Pts',(18.8544785763088,72.7976767306835,12.9354907707228));
#53429=CARTESIAN_POINT('Ctrl Pts',(18.8567798516853,72.8072784404918,12.9566968795014));
#53430=CARTESIAN_POINT('Ctrl Pts',(18.8619734812797,72.8274443636432,13.0047039062497));
#53431=CARTESIAN_POINT('Ctrl Pts',(18.8648750106071,72.8376898225921,13.0316234780821));
#53432=CARTESIAN_POINT('Ctrl Pts',(18.874154985656,72.8672079936783,13.1178953273526));
#53433=CARTESIAN_POINT('Ctrl Pts',(18.8806325976069,72.88302443744,13.178322757841));
#53434=CARTESIAN_POINT('Ctrl Pts',(18.8945920094353,72.907162704179,13.3092022408263));
#53435=CARTESIAN_POINT('Ctrl Pts',(18.9020704643738,72.9141583153627,13.3796993284569));
#53436=CARTESIAN_POINT('Ctrl Pts',(18.9119271978859,72.9156252207459,13.4748095522636));
#53437=CARTESIAN_POINT('Ctrl Pts',(18.9144347044341,72.9152984675103,13.4992127829934));
#53438=CARTESIAN_POINT('Ctrl Pts',(18.9183225146682,72.9136811563357,13.5375035484363));
#53439=CARTESIAN_POINT('Ctrl Pts',(18.9197240610293,72.9128649145516,13.5514039632831));
#53440=CARTESIAN_POINT('Ctrl Pts',(18.9227081539455,72.9106201564345,13.5812371619966));
#53441=CARTESIAN_POINT('Ctrl Pts',(18.9242869939796,72.9091190194082,13.5971616420481));
#53442=CARTESIAN_POINT('Ctrl Pts',(18.929530722707,72.9030850235207,13.6503887701341));
#53443=CARTESIAN_POINT('Ctrl Pts',(18.9331337968108,72.897197432332,13.6875217404613));
#53444=CARTESIAN_POINT('Ctrl Pts',(18.9441228428679,72.8740214460814,13.8009005427082));
#53445=CARTESIAN_POINT('Ctrl Pts',(18.9513787991395,72.8513400118167,13.8758514502966));
#53446=CARTESIAN_POINT('Ctrl Pts',(18.9619460712768,72.8092765171444,13.9793304067216));
#53447=CARTESIAN_POINT('Ctrl Pts',(18.9651397873988,72.7954142676102,14.0099007837454));
#53448=CARTESIAN_POINT('Ctrl Pts',(18.9711823650676,72.7672352881783,14.0660209236222));
#53449=CARTESIAN_POINT('Ctrl Pts',(18.9740209227945,72.7532139580133,14.0916938783444));
#53450=CARTESIAN_POINT('Ctrl Pts',(18.9791743639213,72.7264646398409,14.1368890864682));
#53451=CARTESIAN_POINT('Ctrl Pts',(18.9814768837008,72.7140614694285,14.1565888845649));
#53452=CARTESIAN_POINT('Ctrl Pts',(18.9867141739085,72.6848893052458,14.2002158102131));
#53453=CARTESIAN_POINT('Ctrl Pts',(18.9896589474522,72.667822523857,14.2239263740537));
#53454=CARTESIAN_POINT('Ctrl Pts',(18.9998431830052,72.6066430915271,14.3030204892916));
#53455=CARTESIAN_POINT('Ctrl Pts',(19.0072179822778,72.5587329792036,14.355285654541));
#53456=CARTESIAN_POINT('Ctrl Pts',(19.0200248069847,72.4691747571639,14.4379394528602));
#53457=CARTESIAN_POINT('Ctrl Pts',(19.0254134155555,72.4295610924943,14.4703016448822));
#53458=CARTESIAN_POINT('Ctrl Pts',(19.0330524297008,72.3701141356545,14.5131592691046));
#53459=CARTESIAN_POINT('Ctrl Pts',(19.035351029317,72.3517862866908,14.525656387916));
#53460=CARTESIAN_POINT('Ctrl Pts',(19.0394926614683,72.3178742720979,14.5475008370576));
#53461=CARTESIAN_POINT('Ctrl Pts',(19.0413422669862,72.3023988252927,14.5570061498825));
#53462=CARTESIAN_POINT('Ctrl Pts',(19.0445271916547,72.2751189450706,14.5729663671099));
#53463=CARTESIAN_POINT('Ctrl Pts',(19.0458704314388,72.2634077516452,14.5795707397645));
#53464=CARTESIAN_POINT('Ctrl Pts',(19.0491881848486,72.2339835554525,14.595553612684));
#53465=CARTESIAN_POINT('Ctrl Pts',(19.0511494896536,72.2161494795621,14.604701164699));
#53466=CARTESIAN_POINT('Ctrl Pts',(19.0555730049531,72.1750771373837,14.6245545847283));
#53467=CARTESIAN_POINT('Ctrl Pts',(19.0580229246198,72.1517166425684,14.6349883476451));
#53468=CARTESIAN_POINT('Ctrl Pts',(19.0671648340642,72.0627933775437,14.6715243794105));
#53469=CARTESIAN_POINT('Ctrl Pts',(19.0737308568641,71.9954078705765,14.692854692719));
#53470=CARTESIAN_POINT('Ctrl Pts',(19.0853488019237,71.8752269736946,14.7201417605105));
#53471=CARTESIAN_POINT('Ctrl Pts',(19.0903495753432,71.8231882922918,14.7285964163104));
#53472=CARTESIAN_POINT('Ctrl Pts',(19.0979928876443,71.7445804236849,14.7363950571698));
#53473=CARTESIAN_POINT('Ctrl Pts',(19.1005616591792,71.7183083081137,14.7381787483975));
#53474=CARTESIAN_POINT('Ctrl Pts',(19.1054780163233,71.6684508723498,14.7400094711514));
#53475=CARTESIAN_POINT('Ctrl Pts',(19.1078195703161,71.644882395617,14.7402184640046));
#53476=CARTESIAN_POINT('Ctrl Pts',(19.1135665775289,71.5875599318104,14.7391315632282));
#53477=CARTESIAN_POINT('Ctrl Pts',(19.1169914913882,71.5538394041259,14.737145029325));
#53478=CARTESIAN_POINT('Ctrl Pts',(19.1227208930491,71.4982410112389,14.7316390191867));
#53479=CARTESIAN_POINT('Ctrl Pts',(19.1250029603896,71.4763023249277,14.7288862670089));
#53480=CARTESIAN_POINT('Ctrl Pts',(19.1351975063417,71.3792071612724,14.7141195697546));
#53481=CARTESIAN_POINT('Ctrl Pts',(19.1432393733349,71.3051513326321,14.6959368624199));
#53482=CARTESIAN_POINT('Ctrl Pts',(19.1552241639399,71.1969783564105,14.6588156635142));
#53483=CARTESIAN_POINT('Ctrl Pts',(19.1592094370848,71.1613551992887,14.6447620975226));
#53484=CARTESIAN_POINT('Ctrl Pts',(19.1648498746406,71.1110730828369,14.622248841776));
#53485=CARTESIAN_POINT('Ctrl Pts',(19.1665577966296,71.0958652805527,14.6150739468854));
#53486=CARTESIAN_POINT('Ctrl Pts',(19.1696202560236,71.0685826219487,14.6015334010914));
#53487=CARTESIAN_POINT('Ctrl Pts',(19.1709796977349,71.056461313854,14.5952721391617));
#53488=CARTESIAN_POINT('Ctrl Pts',(19.1745285607266,71.0248314318002,14.5782825235474));
#53489=CARTESIAN_POINT('Ctrl Pts',(19.1766996991741,71.0054996511563,14.5672343682509));
#53490=CARTESIAN_POINT('Ctrl Pts',(19.1803606290721,70.9731002478418,14.5475701849106));
#53491=CARTESIAN_POINT('Ctrl Pts',(19.1818604638763,70.9598843983955,14.539211332752));
#53492=CARTESIAN_POINT('Ctrl Pts',(19.1885942748069,70.9009588723045,14.5003998358305));
#53493=CARTESIAN_POINT('Ctrl Pts',(19.1937372306643,70.8570966217514,14.4672437627804));
#53494=CARTESIAN_POINT('Ctrl Pts',(19.2047114100082,70.7686518367894,14.3908938985588));
#53495=CARTESIAN_POINT('Ctrl Pts',(19.2105330337721,70.7248176249402,14.3470737148405));
#53496=CARTESIAN_POINT('Ctrl Pts',(19.2164763792089,70.6843589395965,14.3002409771978));
#53497=CARTESIAN_POINT('Ctrl Pts',(19.3867992156006,70.6843590974191,14.3002411598846));
#53498=CARTESIAN_POINT('Ctrl Pts',(19.3835334172154,70.7070796831207,14.3265412438178));
#53499=CARTESIAN_POINT('Ctrl Pts',(19.3802671931033,70.7308851081539,14.3519147508244));
#53500=CARTESIAN_POINT('Ctrl Pts',(19.3723650013119,70.7905264941611,14.4104628088744));
#53501=CARTESIAN_POINT('Ctrl Pts',(19.3677158978359,70.827268187921,14.4425935784481));
#53502=CARTESIAN_POINT('Ctrl Pts',(19.3605099636473,70.8858973050198,14.4881877372903));
#53503=CARTESIAN_POINT('Ctrl Pts',(19.3580149054582,70.9064977957848,14.5032346906094));
#53504=CARTESIAN_POINT('Ctrl Pts',(19.3531450225679,70.947173496373,14.5311062455875));
#53505=CARTESIAN_POINT('Ctrl Pts',(19.3507742593599,70.9671841027914,14.5440063877134));
#53506=CARTESIAN_POINT('Ctrl Pts',(19.3446757316856,71.0191051148364,14.5754483869345));
#53507=CARTESIAN_POINT('Ctrl Pts',(19.3409214743082,71.0514802001727,14.593174079633));
#53508=CARTESIAN_POINT('Ctrl Pts',(19.3280588222347,71.1636000090351,14.6483573920042));
#53509=CARTESIAN_POINT('Ctrl Pts',(19.318762402838,71.2464457944114,14.6789204257536));
#53510=CARTESIAN_POINT('Ctrl Pts',(19.3063063127941,71.3614685626476,14.7082335091833));
#53511=CARTESIAN_POINT('Ctrl Pts',(19.3031033733097,71.3914336600095,14.7147251387834));
#53512=CARTESIAN_POINT('Ctrl Pts',(19.2975911306912,71.4439042367553,14.7241182488114));
#53513=CARTESIAN_POINT('Ctrl Pts',(19.2952677222421,71.4663072489211,14.7275130730426));
#53514=CARTESIAN_POINT('Ctrl Pts',(19.2915852361487,71.5023810329232,14.7319956835361));
#53515=CARTESIAN_POINT('Ctrl Pts',(19.2902086670708,71.5159983745807,14.7334646177926));
#53516=CARTESIAN_POINT('Ctrl Pts',(19.2871920134304,71.5461564877241,14.7362250368024));
#53517=CARTESIAN_POINT('Ctrl Pts',(19.2855571924625,71.5627037056621,14.7374133278357));
#53518=CARTESIAN_POINT('Ctrl Pts',(19.2798939294452,71.6205847241462,14.7404312921623));
#53519=CARTESIAN_POINT('Ctrl Pts',(19.2759410503684,71.6619852170594,14.7405657764868));
#53520=CARTESIAN_POINT('Ctrl Pts',(19.2649967634848,71.7774643625782,14.7352933445566));
#53521=CARTESIAN_POINT('Ctrl Pts',(19.2580987963386,71.8511656874217,14.7254159256175));
#53522=CARTESIAN_POINT('Ctrl Pts',(19.2490087100834,71.9448882572721,14.7043757712989));
#53523=CARTESIAN_POINT('Ctrl Pts',(19.2469338402253,71.9660649296679,14.6990446188099));
#53524=CARTESIAN_POINT('Ctrl Pts',(19.2416456260955,72.0193236852016,14.6841667848063));
#53525=CARTESIAN_POINT('Ctrl Pts',(19.238416575831,72.0511827708328,14.6738936030261));
#53526=CARTESIAN_POINT('Ctrl Pts',(19.2328575530865,72.104602285102,14.6543068169986));
#53527=CARTESIAN_POINT('Ctrl Pts',(19.2305491570999,72.126378954612,14.6456310826091));
#53528=CARTESIAN_POINT('Ctrl Pts',(19.2256146017602,72.1719849569639,14.6259826805042));
#53529=CARTESIAN_POINT('Ctrl Pts',(19.2229844897638,72.1957389324514,14.6148643921935));
#53530=CARTESIAN_POINT('Ctrl Pts',(19.2146917655003,72.2688048503666,14.5778658517363));
#53531=CARTESIAN_POINT('Ctrl Pts',(19.2089482398177,72.3167629617254,14.5494767475252));
#53532=CARTESIAN_POINT('Ctrl Pts',(19.1959625531235,72.4193547329688,14.4792610613385));
#53533=CARTESIAN_POINT('Ctrl Pts',(19.1887013054433,72.4727722286487,14.4359547019324));
#53534=CARTESIAN_POINT('Ctrl Pts',(19.1788758673769,72.5407109939177,14.3710867405461));
#53535=CARTESIAN_POINT('Ctrl Pts',(19.1762454420603,72.5584714221768,14.3530854277425));
#53536=CARTESIAN_POINT('Ctrl Pts',(19.171594545553,72.5892051859747,14.3200154530666));
#53537=CARTESIAN_POINT('Ctrl Pts',(19.1695648353517,72.6023846532207,14.3051497058049));
#53538=CARTESIAN_POINT('Ctrl Pts',(19.1662046464435,72.6238594666724,14.279750880089));
#53539=CARTESIAN_POINT('Ctrl Pts',(19.1648624754853,72.6323455915356,14.2693859415454));
#53540=CARTESIAN_POINT('Ctrl Pts',(19.1617611329487,72.6517375256676,14.2449208857967));
#53541=CARTESIAN_POINT('Ctrl Pts',(19.160010246894,72.6625133959531,14.2307220622127));
#53542=CARTESIAN_POINT('Ctrl Pts',(19.1509426712797,72.7172310820457,14.1553807178038));
#53543=CARTESIAN_POINT('Ctrl Pts',(19.143894823342,72.7559774795807,14.0906369583843));
#53544=CARTESIAN_POINT('Ctrl Pts',(19.1303175689313,72.818911238099,13.9604775362638));
#53545=CARTESIAN_POINT('Ctrl Pts',(19.1238142214403,72.84390514277,13.8957704017116));
#53546=CARTESIAN_POINT('Ctrl Pts',(19.1143394148699,72.8717646259092,13.8013354538625));
#53547=CARTESIAN_POINT('Ctrl Pts',(19.1115039033327,72.879060527093,13.77304252555));
#53548=CARTESIAN_POINT('Ctrl Pts',(19.1063506160155,72.8904118553302,13.7217710012879));
#53549=CARTESIAN_POINT('Ctrl Pts',(19.1040450788607,72.8948219270255,13.6988838750791));
#53550=CARTESIAN_POINT('Ctrl Pts',(19.0987925361396,72.9033543897519,13.6469490137557));
#53551=CARTESIAN_POINT('Ctrl Pts',(19.0958353489916,72.9071046998967,13.6178549847112));
#53552=CARTESIAN_POINT('Ctrl Pts',(19.0894161910244,72.9129929155851,13.5551100496096));
#53553=CARTESIAN_POINT('Ctrl Pts',(19.0859471218489,72.9148045023225,13.5214516022515));
#53554=CARTESIAN_POINT('Ctrl Pts',(19.0742303435482,72.9163828165642,13.408626133998));
#53555=CARTESIAN_POINT('Ctrl Pts',(19.0658611661164,72.9100893775512,13.3295609693194));
#53556=CARTESIAN_POINT('Ctrl Pts',(19.0538693498735,72.8903750437942,13.2166270079168));
#53557=CARTESIAN_POINT('Ctrl Pts',(19.0501809790984,72.882804174797,13.1819162505287));
#53558=CARTESIAN_POINT('Ctrl Pts',(19.0448997172875,72.8696841659878,13.1319327399609));
#53559=CARTESIAN_POINT('Ctrl Pts',(19.043260721097,72.8652826184975,13.1163791825758));
#53560=CARTESIAN_POINT('Ctrl Pts',(19.0402436319074,72.8565492115874,13.0876252813873));
#53561=CARTESIAN_POINT('Ctrl Pts',(19.0388622495715,72.8522960385402,13.074405728853));
#53562=CARTESIAN_POINT('Ctrl Pts',(19.035117765819,72.8400834202761,13.0384790878007));
#53563=CARTESIAN_POINT('Ctrl Pts',(19.0327771621028,72.8316940318986,13.0159234595001));
#53564=CARTESIAN_POINT('Ctrl Pts',(19.02366998032,72.7962316099296,12.9282864123973));
#53565=CARTESIAN_POINT('Ctrl Pts',(19.0170869015605,72.7643997805837,12.8652612611433));
#53566=CARTESIAN_POINT('Ctrl Pts',(19.0045421227482,72.6945057156641,12.7514948773903));
#53567=CARTESIAN_POINT('Ctrl Pts',(18.9986062259607,72.6575653927919,12.7003299088967));
#53568=CARTESIAN_POINT('Ctrl Pts',(18.9897603435738,72.5984021476572,12.6300479386718));
#53569=CARTESIAN_POINT('Ctrl Pts',(18.9869580827932,72.5790750827161,12.608615592185));
#53570=CARTESIAN_POINT('Ctrl Pts',(18.9818403476615,72.5428670831154,12.5711147153745));
#53571=CARTESIAN_POINT('Ctrl Pts',(18.9795364134486,72.5262414254013,12.5548168889939));
#53572=CARTESIAN_POINT('Ctrl Pts',(18.974255651198,72.4874683691361,12.5188439049089));
#53573=CARTESIAN_POINT('Ctrl Pts',(18.9712679912811,72.4650625735697,12.4994692398638));
#53574=CARTESIAN_POINT('Ctrl Pts',(18.9647634159167,72.4153591063018,12.4594391208407));
#53575=CARTESIAN_POINT('Ctrl Pts',(18.9612388917027,72.3878625187693,12.4390687497138));
#53576=CARTESIAN_POINT('Ctrl Pts',(18.9491014393378,72.2912839867501,12.3733891071756));
#53577=CARTESIAN_POINT('Ctrl Pts',(18.9403558203981,72.2186214255504,12.3337178595366));
#53578=CARTESIAN_POINT('Ctrl Pts',(18.9283418743341,72.1127763948276,12.2886820971379));
#53579=CARTESIAN_POINT('Ctrl Pts',(18.9249781396343,72.0824419792335,12.2771263742594));
#53580=CARTESIAN_POINT('Ctrl Pts',(18.9200618800202,72.0368182962898,12.2617209508099));
#53581=CARTESIAN_POINT('Ctrl Pts',(18.9184710891769,72.0218485675283,12.2569735752404));
#53582=CARTESIAN_POINT('Ctrl Pts',(18.9154869129122,71.9933298926065,12.2485082786859));
#53583=CARTESIAN_POINT('Ctrl Pts',(18.9140912663641,71.9798014736675,12.244735567167));
#53584=CARTESIAN_POINT('Ctrl Pts',(18.9102135005467,71.9417415770098,12.2347991018166));
#53585=CARTESIAN_POINT('Ctrl Pts',(18.9077569843954,71.91708341829,12.2291422290321));
#53586=CARTESIAN_POINT('Ctrl Pts',(18.8984085658149,71.8217219741621,12.2102448562571));
#53587=CARTESIAN_POINT('Ctrl Pts',(18.8916998279305,71.7501058354853,12.2022809748681));
#53588=CARTESIAN_POINT('Ctrl Pts',(18.8792840033826,71.6180414770388,12.1988697204498));
#53589=CARTESIAN_POINT('Ctrl Pts',(18.8736092625322,71.5578624743169,12.2015929706202));
#53590=CARTESIAN_POINT('Ctrl Pts',(18.8650594582929,71.4696977367608,12.2118875665636));
#53591=CARTESIAN_POINT('Ctrl Pts',(18.8622806145463,71.4414098282073,12.2161635289731));
#53592=CARTESIAN_POINT('Ctrl Pts',(18.8571879752119,71.3904233093375,12.225641541198));
#53593=CARTESIAN_POINT('Ctrl Pts',(18.8548852384085,71.3676769078525,12.2305199500766));
#53594=CARTESIAN_POINT('Ctrl Pts',(18.8495836494129,71.3160965154503,12.2430733693154));
#53595=CARTESIAN_POINT('Ctrl Pts',(18.8465734819824,71.2873747069891,12.2511451033514));
#53596=CARTESIAN_POINT('Ctrl Pts',(18.8400040797361,71.225999086447,12.2707499774348));
#53597=CARTESIAN_POINT('Ctrl Pts',(18.8364368254665,71.1934795449908,12.282622574761));
#53598=CARTESIAN_POINT('Ctrl Pts',(18.823935902502,71.0823117180925,12.3284373388257));
#53599=CARTESIAN_POINT('Ctrl Pts',(18.8148601818198,71.0066449877238,12.368989461398));
#53600=CARTESIAN_POINT('Ctrl Pts',(18.8027178693168,70.9100520828578,12.4340871836399));
#53601=CARTESIAN_POINT('Ctrl Pts',(18.7995271528156,70.8851004929632,12.4522588535239));
#53602=CARTESIAN_POINT('Ctrl Pts',(18.7948697603024,70.8491387638335,12.4805106378641));
#53603=CARTESIAN_POINT('Ctrl Pts',(18.7933667202013,70.8376058556007,12.489903141957));
#53604=CARTESIAN_POINT('Ctrl Pts',(18.7904143244938,70.8150668434862,12.508927362591));
#53605=CARTESIAN_POINT('Ctrl Pts',(18.7889648188221,70.8040568498784,12.5185508227034));
#53606=CARTESIAN_POINT('Ctrl Pts',(18.784663942629,70.7716272204922,12.5478997721756));
#53607=CARTESIAN_POINT('Ctrl Pts',(18.7818482492416,70.7507152604635,12.5681755475808));
#53608=CARTESIAN_POINT('Ctrl Pts',(18.7746483999433,70.6985451674196,12.6223616481549));
#53609=CARTESIAN_POINT('Ctrl Pts',(18.7703116485295,70.6684027017918,12.6572873441909));
#53610=CARTESIAN_POINT('Ctrl Pts',(18.7585556056968,70.5919216516156,12.7563271567465));
#53611=CARTESIAN_POINT('Ctrl Pts',(18.7511640655145,70.5495687772447,12.8232409382886));
#53612=CARTESIAN_POINT('Ctrl Pts',(18.7407699886034,70.5005699321449,12.9194525237505));
#53613=CARTESIAN_POINT('Ctrl Pts',(18.7379584565224,70.4883170101541,12.9456937354539));
#53614=CARTESIAN_POINT('Ctrl Pts',(18.7328321304185,70.4678521641224,12.9937408611873));
#53615=CARTESIAN_POINT('Ctrl Pts',(18.7305290970881,70.4593230011766,13.0153981419959));
#53616=CARTESIAN_POINT('Ctrl Pts',(18.7252616144557,70.4413441281442,13.0650068237519));
#53617=CARTESIAN_POINT('Ctrl Pts',(18.7222865689622,70.4322642568377,13.093076501623));
#53618=CARTESIAN_POINT('Ctrl Pts',(18.7158166358718,70.4148377236653,13.1541317813105));
#53619=CARTESIAN_POINT('Ctrl Pts',(18.7123143314326,70.4068230111986,13.1871876657736));
#53620=CARTESIAN_POINT('Ctrl Pts',(18.7003464736732,70.3841940147418,13.3001389914435));
#53621=CARTESIAN_POINT('Ctrl Pts',(18.6917527005371,70.3759165010865,13.3810998188951));
#53622=CARTESIAN_POINT('Ctrl Pts',(18.6797501782105,70.3752190653075,13.495934949769));
#53623=CARTESIAN_POINT('Ctrl Pts',(18.6762586192099,70.3763520245786,13.5295818994106));
#53624=CARTESIAN_POINT('Ctrl Pts',(18.6711961982458,70.3799870492725,13.579009208535));
#53625=CARTESIAN_POINT('Ctrl Pts',(18.6695840960226,70.3814514898272,13.5948486988157));
#53626=CARTESIAN_POINT('Ctrl Pts',(18.666586969508,70.3847591501794,13.6245298308791));
#53627=CARTESIAN_POINT('Ctrl Pts',(18.6651992053597,70.3865335358021,13.6383748335243));
#53628=CARTESIAN_POINT('Ctrl Pts',(18.6613906152334,70.3920730347633,13.6765899379778));
#53629=CARTESIAN_POINT('Ctrl Pts',(18.6589937916027,70.3963202053588,13.7008848856826));
#53630=CARTESIAN_POINT('Ctrl Pts',(18.6497808092936,70.4155432923951,13.794657012063));
#53631=CARTESIAN_POINT('Ctrl Pts',(18.6431473560594,70.4356331538749,13.8629583712339));
#53632=CARTESIAN_POINT('Ctrl Pts',(18.6306681141832,70.483656522586,13.986781233989));
#53633=CARTESIAN_POINT('Ctrl Pts',(18.6248507353769,70.5101420777077,14.0426243712303));
#53634=CARTESIAN_POINT('Ctrl Pts',(18.6161388635988,70.5547556313678,14.1213226222846));
#53635=CARTESIAN_POINT('Ctrl Pts',(18.6133467919828,70.5697753109458,14.1458383886472));
#53636=CARTESIAN_POINT('Ctrl Pts',(18.6082398745516,70.5984364656055,14.1892419418408));
#53637=CARTESIAN_POINT('Ctrl Pts',(18.6059363573694,70.611790888589,14.2083045721645));
#53638=CARTESIAN_POINT('Ctrl Pts',(18.6006461328833,70.6433697818026,14.2508445396661));
#53639=CARTESIAN_POINT('Ctrl Pts',(18.5976483805331,70.6619089636197,14.2740695035649));
#53640=CARTESIAN_POINT('Ctrl Pts',(18.5944580111549,70.682279675732,14.2978295571791));
#53641=CARTESIAN_POINT('Ctrl Pts',(18.594295635599,70.6833181886463,14.2990362614413));
#53642=CARTESIAN_POINT('Ctrl Pts',(18.5941331801233,70.6843589436049,14.3002409818378));
#53643=CARTESIAN_POINT('Origin',(21.26284859951,71.6454,13.47));
#53644=CARTESIAN_POINT('',(17.6289974407812,70.6843588693663,14.3002408959033));
#53645=CARTESIAN_POINT('',(17.7982694921739,70.6843589433904,14.3002409815896));
#53646=CARTESIAN_POINT('',(21.26284859951,70.6843589433668,14.3002409815622));
#53647=CARTESIAN_POINT('',(18.3157450659502,71.646363655002,14.7399998049553));
#53648=CARTESIAN_POINT('Ctrl Pts',(17.6289974407812,70.6843588693663,14.3002408959033));
#53649=CARTESIAN_POINT('Ctrl Pts',(17.6346389774939,70.6485735080814,14.2588177327719));
#53650=CARTESIAN_POINT('Ctrl Pts',(17.6403669691112,70.6154972945373,14.215116859955));
#53651=CARTESIAN_POINT('Ctrl Pts',(17.6533971916263,70.5472400007928,14.1116625438007));
#53652=CARTESIAN_POINT('Ctrl Pts',(17.6606960210929,70.5139186929955,14.0508942837002));
#53653=CARTESIAN_POINT('Ctrl Pts',(17.6695292415001,70.4788740695717,13.9723928410434));
#53654=CARTESIAN_POINT('Ctrl Pts',(17.6712402932642,70.4723403708938,13.9569420051821));
#53655=CARTESIAN_POINT('Ctrl Pts',(17.6742947714227,70.4611201916754,13.9288707664881));
#53656=CARTESIAN_POINT('Ctrl Pts',(17.6756432994331,70.4563248994782,13.9162975721615));
#53657=CARTESIAN_POINT('Ctrl Pts',(17.6787762667129,70.4455579271645,13.8866601624838));
#53658=CARTESIAN_POINT('Ctrl Pts',(17.6805519707749,70.4397490289603,13.8695404276859));
#53659=CARTESIAN_POINT('Ctrl Pts',(17.6844573943771,70.4276747265706,13.8312901816871));
#53660=CARTESIAN_POINT('Ctrl Pts',(17.6865788759155,70.4215896721122,13.8101086373422));
#53661=CARTESIAN_POINT('Ctrl Pts',(17.6935028490101,70.4034042156482,13.7399778279591));
#53662=CARTESIAN_POINT('Ctrl Pts',(17.6982342791462,70.3936659435074,13.6904636943652));
#53663=CARTESIAN_POINT('Ctrl Pts',(17.7097112951337,70.3772591901405,13.569359941036));
#53664=CARTESIAN_POINT('Ctrl Pts',(17.7164446483401,70.3736716260103,13.4975414310448));
#53665=CARTESIAN_POINT('Ctrl Pts',(17.7261618985194,70.3771853059989,13.396620296412));
#53666=CARTESIAN_POINT('Ctrl Pts',(17.7289968140244,70.37920815591,13.3674768579708));
#53667=CARTESIAN_POINT('Ctrl Pts',(17.7341460687762,70.3846442786766,13.3152855468846));
#53668=CARTESIAN_POINT('Ctrl Pts',(17.7364481141296,70.3876906327177,13.2922121436989));
#53669=CARTESIAN_POINT('Ctrl Pts',(17.741687251276,70.3959896419891,13.2403737581136));
#53670=CARTESIAN_POINT('Ctrl Pts',(17.7446344040215,70.4016051254094,13.2116815679193));
#53671=CARTESIAN_POINT('Ctrl Pts',(17.7510262896919,70.4157765058223,13.1505467534375));
#53672=CARTESIAN_POINT('Ctrl Pts',(17.7544779948524,70.4246381795664,13.1181983032634));
#53673=CARTESIAN_POINT('Ctrl Pts',(17.7660552335088,70.4583289762784,13.0119149312245));
#53674=CARTESIAN_POINT('Ctrl Pts',(17.7742991018947,70.4886837105304,12.9399196243682));
#53675=CARTESIAN_POINT('Ctrl Pts',(17.7864128375122,70.543238359833,12.8378892576638));
#53676=CARTESIAN_POINT('Ctrl Pts',(17.7903369087447,70.5625102307927,12.8054138628221));
#53677=CARTESIAN_POINT('Ctrl Pts',(17.7958322287774,70.5919900250051,12.7604336429856));
#53678=CARTESIAN_POINT('Ctrl Pts',(17.7974577246906,70.6010313571855,12.7471921273928));
#53679=CARTESIAN_POINT('Ctrl Pts',(17.8004628021912,70.6183768110263,12.7227941224856));
#53680=CARTESIAN_POINT('Ctrl Pts',(17.8018454348783,70.6266169225172,12.7115975128283));
#53681=CARTESIAN_POINT('Ctrl Pts',(17.8056100922388,70.6497350268353,12.6812418018446));
#53682=CARTESIAN_POINT('Ctrl Pts',(17.8079690951011,70.6649810721522,12.662369374025));
#53683=CARTESIAN_POINT('Ctrl Pts',(17.8170962709051,70.7266277224934,12.5903805983487));
#53684=CARTESIAN_POINT('Ctrl Pts',(17.8236819544005,70.7768824870622,12.5407247208408));
#53685=CARTESIAN_POINT('Ctrl Pts',(17.8362032511098,70.8791482612832,12.4552613237198));
#53686=CARTESIAN_POINT('Ctrl Pts',(17.8421126389966,70.9301995577544,12.4186565433208));
#53687=CARTESIAN_POINT('Ctrl Pts',(17.8509285564544,71.0083498696919,12.3709557235073));
#53688=CARTESIAN_POINT('Ctrl Pts',(17.8537285068914,71.0334603257136,12.3567791211486));
#53689=CARTESIAN_POINT('Ctrl Pts',(17.8588434776343,71.0796748595025,12.3327239587012));
#53690=CARTESIAN_POINT('Ctrl Pts',(17.8611469967352,71.100610307492,12.3225481522738));
#53691=CARTESIAN_POINT('Ctrl Pts',(17.8664287030941,71.1488054765756,12.3007388025683));
#53692=CARTESIAN_POINT('Ctrl Pts',(17.8694177609855,71.1762153265732,12.289473318576));
#53693=CARTESIAN_POINT('Ctrl Pts',(17.8759268747967,71.2360967077403,12.2672767542085));
#53694=CARTESIAN_POINT('Ctrl Pts',(17.8794545760762,71.2686668367627,12.2566805727704));
#53695=CARTESIAN_POINT('Ctrl Pts',(17.8916235674072,71.3813929910568,12.2249831889868));
#53696=CARTESIAN_POINT('Ctrl Pts',(17.9003984218593,71.4631661037746,12.2104144687572));
#53697=CARTESIAN_POINT('Ctrl Pts',(17.9125379967623,71.5790644495894,12.2012938538969));
#53698=CARTESIAN_POINT('Ctrl Pts',(17.9159990360092,71.6124581337761,12.1999877654215));
#53699=CARTESIAN_POINT('Ctrl Pts',(17.9209577942149,71.6610966323201,12.2000057022075));
#53700=CARTESIAN_POINT('Ctrl Pts',(17.9224985391921,71.6763249412809,12.200285217019));
#53701=CARTESIAN_POINT('Ctrl Pts',(17.9254620409761,71.7058831297117,12.2013599326175));
#53702=CARTESIAN_POINT('Ctrl Pts',(17.9268859070433,71.7202114131176,12.2021241645522));
#53703=CARTESIAN_POINT('Ctrl Pts',(17.9309845729074,71.7617436911101,12.205045973));
#53704=CARTESIAN_POINT('Ctrl Pts',(17.9336287166111,71.78889732772,12.2078377983099));
#53705=CARTESIAN_POINT('Ctrl Pts',(17.9402026343141,71.8568121087723,12.2170411543457));
#53706=CARTESIAN_POINT('Ctrl Pts',(17.944094941471,71.8973908433042,12.2245674752926));
#53707=CARTESIAN_POINT('Ctrl Pts',(17.9563652086868,72.0243511397494,12.2545765242186));
#53708=CARTESIAN_POINT('Ctrl Pts',(17.9646784241461,72.1087534135119,12.2841841545359));
#53709=CARTESIAN_POINT('Ctrl Pts',(17.9759850837983,72.2147211298855,12.3344113317521));
#53710=CARTESIAN_POINT('Ctrl Pts',(17.9787150497899,72.2396819697554,12.3472725921183));
#53711=CARTESIAN_POINT('Ctrl Pts',(17.9837640665872,72.2845481889901,12.3723056652532));
#53712=CARTESIAN_POINT('Ctrl Pts',(17.9860732187937,72.3045840240859,12.3842194032067));
#53713=CARTESIAN_POINT('Ctrl Pts',(17.9914568728277,72.3501079195851,12.4130133585766));
#53714=CARTESIAN_POINT('Ctrl Pts',(17.9945441413881,72.3753355944863,12.4302752090745));
#53715=CARTESIAN_POINT('Ctrl Pts',(17.9995895710402,72.4150937784589,12.4596398541954));
#53716=CARTESIAN_POINT('Ctrl Pts',(18.001527366384,72.4300211243848,12.4711878335554));
#53717=CARTESIAN_POINT('Ctrl Pts',(18.0092467665939,72.4881275980583,12.5182461973859));
#53718=CARTESIAN_POINT('Ctrl Pts',(18.0151038192601,72.5291952001873,12.5562550686432));
#53719=CARTESIAN_POINT('Ctrl Pts',(18.0277676721154,72.6119813358572,12.6436928755246));
#53720=CARTESIAN_POINT('Ctrl Pts',(18.0345653015757,72.6527108656485,12.6938624462724));
#53721=CARTESIAN_POINT('Ctrl Pts',(18.0431239767362,72.7001203159455,12.7623164442262));
#53722=CARTESIAN_POINT('Ctrl Pts',(18.0450342872524,72.7104455995707,12.7779530602499));
#53723=CARTESIAN_POINT('Ctrl Pts',(18.0482779914553,72.7275696059023,12.8051773473902));
#53724=CARTESIAN_POINT('Ctrl Pts',(18.0496205462495,72.7345365027106,12.8166532688021));
#53725=CARTESIAN_POINT('Ctrl Pts',(18.0528729390209,72.751109138655,12.8449540178626));
#53726=CARTESIAN_POINT('Ctrl Pts',(18.0547710939944,72.7605143396402,12.8618920000066));
#53727=CARTESIAN_POINT('Ctrl Pts',(18.0590156276763,72.7808555690324,12.9005852779468));
#53728=CARTESIAN_POINT('Ctrl Pts',(18.0613512102647,72.791561172505,12.9224534259517));
#53729=CARTESIAN_POINT('Ctrl Pts',(18.0696376337968,72.8275514280754,13.0016587942693));
#53730=CARTESIAN_POINT('Ctrl Pts',(18.0754851951364,72.8492154947339,13.0605433269499));
#53731=CARTESIAN_POINT('Ctrl Pts',(18.0872087205534,72.8834922402098,13.1803951172995));
#53732=CARTESIAN_POINT('Ctrl Pts',(18.0930682250896,72.8961493751874,13.2411602912818));
#53733=CARTESIAN_POINT('Ctrl Pts',(18.1016400192758,72.9078348968004,13.3290405035049));
#53734=CARTESIAN_POINT('Ctrl Pts',(18.1042406037443,72.9105165338626,13.3555825269681));
#53735=CARTESIAN_POINT('Ctrl Pts',(18.1091814819325,72.9139853824082,13.4056309028339));
#53736=CARTESIAN_POINT('Ctrl Pts',(18.1115149711916,72.914959113901,13.429113253711));
#53737=CARTESIAN_POINT('Ctrl Pts',(18.1171759757326,72.9157330273195,13.4856181668505));
#53738=CARTESIAN_POINT('Ctrl Pts',(18.1205213177689,72.9148977504257,13.5186301553941));
#53739=CARTESIAN_POINT('Ctrl Pts',(18.1280597341658,72.9101715518525,13.5920638626517));
#53740=CARTESIAN_POINT('Ctrl Pts',(18.1322673423076,72.9056262255898,13.6324063010571));
#53741=CARTESIAN_POINT('Ctrl Pts',(18.1440167519786,72.8877075829968,13.7433709623424));
#53742=CARTESIAN_POINT('Ctrl Pts',(18.1516163840293,72.8702612544447,13.8131829284471));
#53743=CARTESIAN_POINT('Ctrl Pts',(18.162343436967,72.8369511893909,13.9105344689111));
#53744=CARTESIAN_POINT('Ctrl Pts',(18.1655562045799,72.8258191547202,13.9395486564026));
#53745=CARTESIAN_POINT('Ctrl Pts',(18.1702389940427,72.8077854020337,13.9818421937544));
#53746=CARTESIAN_POINT('Ctrl Pts',(18.1717458793826,72.8016964699614,13.9954529522606));
#53747=CARTESIAN_POINT('Ctrl Pts',(18.1747004474569,72.7891713552702,14.0221778257484));
#53748=CARTESIAN_POINT('Ctrl Pts',(18.1761483551711,72.7827458861653,14.0352943178888));
#53749=CARTESIAN_POINT('Ctrl Pts',(18.1804357150977,72.7628935658343,14.0741098048386));
#53750=CARTESIAN_POINT('Ctrl Pts',(18.1832398383454,72.7488103961094,14.0994652055762));
#53751=CARTESIAN_POINT('Ctrl Pts',(18.1903959229063,72.7102975847404,14.1635318352467));
#53752=CARTESIAN_POINT('Ctrl Pts',(18.1947012106833,72.6846216048335,14.2014454540741));
#53753=CARTESIAN_POINT('Ctrl Pts',(18.2064854929538,72.6087834121687,14.3013478136545));
#53754=CARTESIAN_POINT('Ctrl Pts',(18.2139348965897,72.5547559660465,14.3601214992592));
#53755=CARTESIAN_POINT('Ctrl Pts',(18.2243869937911,72.4741059595387,14.4327992438687));
#53756=CARTESIAN_POINT('Ctrl Pts',(18.2271945836077,72.4519749014625,14.4514135608194));
#53757=CARTESIAN_POINT('Ctrl Pts',(18.2323169863518,72.4109178926607,14.4836192678949));
#53758=CARTESIAN_POINT('Ctrl Pts',(18.2346201247594,72.3922159986472,14.4974762049277));
#53759=CARTESIAN_POINT('Ctrl Pts',(18.2398921452152,72.3489374213081,14.5277370350171));
#53760=CARTESIAN_POINT('Ctrl Pts',(18.2428717145256,72.3241488654784,14.5438119733176));
#53761=CARTESIAN_POINT('Ctrl Pts',(18.2493542191822,72.2696028445018,14.5765406381842));
#53762=CARTESIAN_POINT('Ctrl Pts',(18.2528646451282,72.2396899265245,14.592889300668));
#53763=CARTESIAN_POINT('Ctrl Pts',(18.2648947632856,72.1359399545737,14.6442858327836));
#53764=CARTESIAN_POINT('Ctrl Pts',(18.2735443444823,72.0593933250985,14.6734053758334));
#53765=CARTESIAN_POINT('Ctrl Pts',(18.2855500966007,71.9485704074341,14.7037299972732));
#53766=CARTESIAN_POINT('Ctrl Pts',(18.2889936515305,71.9162159239663,14.7112337651819));
#53767=CARTESIAN_POINT('Ctrl Pts',(18.2940015296655,71.8680505476001,14.7204308714458));
#53768=CARTESIAN_POINT('Ctrl Pts',(18.2956059643778,71.8524446118942,14.7231094321163));
#53769=CARTESIAN_POINT('Ctrl Pts',(18.2984679648359,71.8242476018861,14.7274078639219));
#53770=CARTESIAN_POINT('Ctrl Pts',(18.2997304293162,71.8116764043031,14.7291319181347));
#53771=CARTESIAN_POINT('Ctrl Pts',(18.3024284729266,71.7845587862325,14.732437653291));
#53772=CARTESIAN_POINT('Ctrl Pts',(18.3038608346063,71.7700070826735,14.7339569356805));
#53773=CARTESIAN_POINT('Ctrl Pts',(18.3088224453373,71.7191640227705,14.7383785444306));
#53774=CARTESIAN_POINT('Ctrl Pts',(18.3122976264266,71.6827740069663,14.7399720473119));
#53775=CARTESIAN_POINT('Ctrl Pts',(18.3157454956419,71.6463622425315,14.7399996354682));
#53776=CARTESIAN_POINT('Ctrl Pts',(18.315745359276,71.6463636826444,14.7399996343762));
#53777=CARTESIAN_POINT('Ctrl Pts',(18.3256839003294,71.541406182485,14.7400792766994));
#53778=CARTESIAN_POINT('Ctrl Pts',(18.3353753375936,71.4368445038087,14.7271484664875));
#53779=CARTESIAN_POINT('Ctrl Pts',(18.3483273621578,71.3062132498836,14.6942293176145));
#53780=CARTESIAN_POINT('Ctrl Pts',(18.3512125677473,71.277632162101,14.6859488335247));
#53781=CARTESIAN_POINT('Ctrl Pts',(18.3564123717177,71.2272539108023,14.6694147261593));
#53782=CARTESIAN_POINT('Ctrl Pts',(18.3587135400297,71.205342846555,14.6615499832992));
#53783=CARTESIAN_POINT('Ctrl Pts',(18.3638991894459,71.1569055621928,14.6426457841576));
#53784=CARTESIAN_POINT('Ctrl Pts',(18.3667926908487,71.1305140061665,14.631299715972));
#53785=CARTESIAN_POINT('Ctrl Pts',(18.3759692296684,71.048922686953,14.5928946473237));
#53786=CARTESIAN_POINT('Ctrl Pts',(18.3823478497847,70.9952965746847,14.5627216455913));
#53787=CARTESIAN_POINT('Ctrl Pts',(18.3962593650635,70.8846926906335,14.4894594073753));
#53788=CARTESIAN_POINT('Ctrl Pts',(18.4037927950747,70.8287247474877,14.4452001769306));
#53789=CARTESIAN_POINT('Ctrl Pts',(18.4137450020772,70.7586899775641,14.3795377666154));
#53790=CARTESIAN_POINT('Ctrl Pts',(18.4162919818968,70.7411165966014,14.3620680524911));
#53791=CARTESIAN_POINT('Ctrl Pts',(18.4202240500033,70.7144463945094,14.3339563872702));
#53792=CARTESIAN_POINT('Ctrl Pts',(18.4216312040912,70.7049959745739,14.3236601302597));
#53793=CARTESIAN_POINT('Ctrl Pts',(18.4235989564324,70.6919012103889,14.3089118394509));
#53794=CARTESIAN_POINT('Ctrl Pts',(18.4241701294657,70.6881153666811,14.3045892094999));
#53795=CARTESIAN_POINT('Ctrl Pts',(18.4247393426037,70.684358943376,14.3002409815728));
#53796=CARTESIAN_POINT('',(18.4858211068938,71.645349016461,14.7399996799991));
#53797=CARTESIAN_POINT('Ctrl Pts',(18.5941331801233,70.6843589436049,14.3002409818378));
#53798=CARTESIAN_POINT('Ctrl Pts',(18.5907865350394,70.7057988947686,14.325058683886));
#53799=CARTESIAN_POINT('Ctrl Pts',(18.5874054687168,70.7281902732238,14.3490344495593));
#53800=CARTESIAN_POINT('Ctrl Pts',(18.5752698875643,70.8111251467179,14.4312156822484));
#53801=CARTESIAN_POINT('Ctrl Pts',(18.5663754828149,70.8764809986208,14.4842544402918));
#53802=CARTESIAN_POINT('Ctrl Pts',(18.5542369849415,70.9736114432448,14.5482614950515));
#53803=CARTESIAN_POINT('Ctrl Pts',(18.5508856285351,71.0013135803539,14.5650346634462));
#53804=CARTESIAN_POINT('Ctrl Pts',(18.5460485511096,71.0428260070941,14.5880484093272));
#53805=CARTESIAN_POINT('Ctrl Pts',(18.5445225702095,71.0561527869441,14.5951290877217));
#53806=CARTESIAN_POINT('Ctrl Pts',(18.541564339877,71.0824784619157,14.6085200871453));
#53807=CARTESIAN_POINT('Ctrl Pts',(18.5401313501845,71.0954648260161,14.6148493387851));
#53808=CARTESIAN_POINT('Ctrl Pts',(18.5359594460948,71.1338877916252,14.632771039288));
#53809=CARTESIAN_POINT('Ctrl Pts',(18.5332529837572,71.1596046085438,14.6437480355549));
#53810=CARTESIAN_POINT('Ctrl Pts',(18.5239302444666,71.2502775061027,14.6789592311908));
#53811=CARTESIAN_POINT('Ctrl Pts',(18.5174647761561,71.3168410088035,14.6987209114874));
#53812=CARTESIAN_POINT('Ctrl Pts',(18.5055123950072,71.441276410779,14.7248212602656));
#53813=CARTESIAN_POINT('Ctrl Pts',(18.500056217803,71.4986000308892,14.7328108636789));
#53814=CARTESIAN_POINT('Ctrl Pts',(18.4928819979801,71.5729290381079,14.7380406471959));
#53815=CARTESIAN_POINT('Ctrl Pts',(18.4912653341044,71.5896154585899,14.7388842152709));
#53816=CARTESIAN_POINT('Ctrl Pts',(18.4883724085359,71.619321579511,14.7397989225822));
#53817=CARTESIAN_POINT('Ctrl Pts',(18.487100038195,71.6323350556675,14.7399994731758));
#53818=CARTESIAN_POINT('Ctrl Pts',(18.4858216933514,71.6453486884009,14.7399999989634));
#53819=CARTESIAN_POINT('Ctrl Pts',(18.4858216558298,71.6453490703727,14.7399999989788));
#53820=CARTESIAN_POINT('Ctrl Pts',(18.4840637483041,71.663244680427,14.7400007166298));
#53821=CARTESIAN_POINT('Ctrl Pts',(18.482294843087,71.6811373155185,14.7396231841365));
#53822=CARTESIAN_POINT('Ctrl Pts',(18.4782654825454,71.7215925780454,14.7379137763227));
#53823=CARTESIAN_POINT('Ctrl Pts',(18.4759987726767,71.7441386739734,14.7363574390113));
#53824=CARTESIAN_POINT('Ctrl Pts',(18.4685594670071,71.8173651474842,14.7293354453857));
#53825=CARTESIAN_POINT('Ctrl Pts',(18.4633167768759,71.8677532169577,14.7214212683486));
#53826=CARTESIAN_POINT('Ctrl Pts',(18.4493532739256,71.9987014908871,14.692695895691));
#53827=CARTESIAN_POINT('Ctrl Pts',(18.4405463690157,72.0779316151334,14.6669639165977));
#53828=CARTESIAN_POINT('Ctrl Pts',(18.4296568718692,72.173736900525,14.6250846032055));
#53829=CARTESIAN_POINT('Ctrl Pts',(18.4274352410209,72.1931764897535,14.6159936230427));
#53830=CARTESIAN_POINT('Ctrl Pts',(18.4234138708816,72.2282528479709,14.5984933783508));
#53831=CARTESIAN_POINT('Ctrl Pts',(18.421608118556,72.2439616693562,14.5902405072629));
#53832=CARTESIAN_POINT('Ctrl Pts',(18.4184632784958,72.2712960892057,14.575140663398));
#53833=CARTESIAN_POINT('Ctrl Pts',(18.4171171918754,72.2829933447736,14.5684336907788));
#53834=CARTESIAN_POINT('Ctrl Pts',(18.4137399941561,72.3123084618777,14.5509988008193));
#53835=CARTESIAN_POINT('Ctrl Pts',(18.4117234080901,72.3297758978712,14.5400257527683));
#53836=CARTESIAN_POINT('Ctrl Pts',(18.400137615384,72.4294773205739,14.4739521750378));
#53837=CARTESIAN_POINT('Ctrl Pts',(18.390999655118,72.5053213920228,14.4098075870873));
#53838=CARTESIAN_POINT('Ctrl Pts',(18.3782410293835,72.5976497144407,14.3110872684802));
#53839=CARTESIAN_POINT('Ctrl Pts',(18.3748093649996,72.6212061965352,14.2836394715801));
#53840=CARTESIAN_POINT('Ctrl Pts',(18.3683925426735,72.6625300246403,14.2311097483416));
#53841=CARTESIAN_POINT('Ctrl Pts',(18.3654206773575,72.6806197171338,14.2063160472623));
#53842=CARTESIAN_POINT('Ctrl Pts',(18.3601313085065,72.7108408312795,14.1615773475406));
#53843=CARTESIAN_POINT('Ctrl Pts',(18.3578291968888,72.7233538303298,14.1419068059499));
#53844=CARTESIAN_POINT('Ctrl Pts',(18.3527196402942,72.7496784222156,14.0978947959057));
#53845=CARTESIAN_POINT('Ctrl Pts',(18.3499047110374,72.7632404814613,14.0734194702424));
#53846=CARTESIAN_POINT('Ctrl Pts',(18.3379039477335,72.8170377356596,13.9682850700007));
#53847=CARTESIAN_POINT('Ctrl Pts',(18.3284682238935,72.8494271547613,13.8839259139512));
#53848=CARTESIAN_POINT('Ctrl Pts',(18.3146944114495,72.8831294672406,13.7573932734595));
#53849=CARTESIAN_POINT('Ctrl Pts',(18.3104007072289,72.8917342225672,13.7174278508353));
#53850=CARTESIAN_POINT('Ctrl Pts',(18.3033353405523,72.9028224282651,13.6503467473071));
#53851=CARTESIAN_POINT('Ctrl Pts',(18.3005388771244,72.9063886847045,13.6234405012951));
#53852=CARTESIAN_POINT('Ctrl Pts',(18.2963252051142,72.9105162175549,13.5821875876307));
#53853=CARTESIAN_POINT('Ctrl Pts',(18.2948806267495,72.9117010161109,13.5679128447337));
#53854=CARTESIAN_POINT('Ctrl Pts',(18.2919249402125,72.9136486908722,13.5383960599083));
#53855=CARTESIAN_POINT('Ctrl Pts',(18.2904155684304,72.9143789032385,13.5231543835663));
#53856=CARTESIAN_POINT('Ctrl Pts',(18.2856188727244,72.9158379960445,13.4742855406007));
#53857=CARTESIAN_POINT('Ctrl Pts',(18.2823808775923,72.9155061169949,13.4406379507612));
#53858=CARTESIAN_POINT('Ctrl Pts',(18.2713021763805,72.9097426413883,13.3245247909113));
#53859=CARTESIAN_POINT('Ctrl Pts',(18.2636411054131,72.8976051508321,13.2426034582882));
#53860=CARTESIAN_POINT('Ctrl Pts',(18.2525956884939,72.8693120586383,13.1292520282826));
#53861=CARTESIAN_POINT('Ctrl Pts',(18.2493427518675,72.8596921526603,13.0964171786878));
#53862=CARTESIAN_POINT('Ctrl Pts',(18.2432068567256,72.8392949932667,13.0359592994719));
#53863=CARTESIAN_POINT('Ctrl Pts',(18.2403349265164,72.8288531504033,13.0082480057006));
#53864=CARTESIAN_POINT('Ctrl Pts',(18.2351490465228,72.8084924619636,12.9594537998925));
#53865=CARTESIAN_POINT('Ctrl Pts',(18.2328482340944,72.7989434883822,12.9382305558151));
#53866=CARTESIAN_POINT('Ctrl Pts',(18.227651005068,72.7762674632518,12.8913201476615));
#53867=CARTESIAN_POINT('Ctrl Pts',(18.2247453235574,72.7628378825125,12.8657948759892));
#53868=CARTESIAN_POINT('Ctrl Pts',(18.2154060802847,72.7173748613197,12.7860924546668));
#53869=CARTESIAN_POINT('Ctrl Pts',(18.2088712336361,72.6821835065995,12.7338363463221));
#53870=CARTESIAN_POINT('Ctrl Pts',(18.1948834508981,72.5997055018529,12.6290710077774));
#53871=CARTESIAN_POINT('Ctrl Pts',(18.18743600577,72.5516091393923,12.5774494804156));
#53872=CARTESIAN_POINT('Ctrl Pts',(18.1776332414141,72.48157927186,12.513815310477));
#53873=CARTESIAN_POINT('Ctrl Pts',(18.175148119483,72.4632167987984,12.4980633382184));
#53874=CARTESIAN_POINT('Ctrl Pts',(18.1712858161642,72.4336181126922,12.4741058777211));
#53875=CARTESIAN_POINT('Ctrl Pts',(18.1698878469869,72.4226788513101,12.4655446364968));
#53876=CARTESIAN_POINT('Ctrl Pts',(18.1669020070733,72.3988019514851,12.4474820225952));
#53877=CARTESIAN_POINT('Ctrl Pts',(18.165318002951,72.3858206037548,12.4380431512228));
#53878=CARTESIAN_POINT('Ctrl Pts',(18.1603550848147,72.344249433831,12.409004858421));
#53879=CARTESIAN_POINT('Ctrl Pts',(18.1570265323417,72.3150318396945,12.3903264116734));
#53880=CARTESIAN_POINT('Ctrl Pts',(18.146104194103,72.2158189557635,12.3324805174102));
#53881=CARTESIAN_POINT('Ctrl Pts',(18.1386639308201,72.1428842690816,12.2987447173984));
#53882=CARTESIAN_POINT('Ctrl Pts',(18.1278786644537,72.0353180146071,12.2608638434066));
#53883=CARTESIAN_POINT('Ctrl Pts',(18.1246574767609,72.0029489804888,12.2509000510684));
#53884=CARTESIAN_POINT('Ctrl Pts',(18.118571720353,71.9417882292341,12.2347190024447));
#53885=CARTESIAN_POINT('Ctrl Pts',(18.1157177937111,71.9131035623116,12.228186965682));
#53886=CARTESIAN_POINT('Ctrl Pts',(18.1105500675895,71.8613682897272,12.218281554135));
#53887=CARTESIAN_POINT('Ctrl Pts',(18.1082489994013,71.8384020656323,12.2145353862735));
#53888=CARTESIAN_POINT('Ctrl Pts',(18.1030329315977,71.7865915689535,12.2075393332325));
#53889=CARTESIAN_POINT('Ctrl Pts',(18.1001082989963,71.7577139120084,12.2046434354114));
#53890=CARTESIAN_POINT('Ctrl Pts',(18.0892228955812,71.6510312151929,12.1976254395082));
#53891=CARTESIAN_POINT('Ctrl Pts',(18.081089827151,71.5730068168395,12.1996758944694));
#53892=CARTESIAN_POINT('Ctrl Pts',(18.0679879977557,71.4492918110199,12.2143632947521));
#53893=CARTESIAN_POINT('Ctrl Pts',(18.063068441033,71.4032431413625,12.2224253826389));
#53894=CARTESIAN_POINT('Ctrl Pts',(18.0551504022456,71.3291696951112,12.2396509097847));
#53895=CARTESIAN_POINT('Ctrl Pts',(18.0521207649156,71.3008332617348,12.2472839005731));
#53896=CARTESIAN_POINT('Ctrl Pts',(18.0476438491228,71.2587755976031,12.2601916368784));
#53897=CARTESIAN_POINT('Ctrl Pts',(18.0461639997273,71.2448418263868,12.264733252419));
#53898=CARTESIAN_POINT('Ctrl Pts',(18.0432128237681,71.2169541504291,12.2743601758368));
#53899=CARTESIAN_POINT('Ctrl Pts',(18.0417420297667,71.2030045791085,12.2794510493998));
#53900=CARTESIAN_POINT('Ctrl Pts',(18.0372718794751,71.1605440245763,12.2957964376332));
#53901=CARTESIAN_POINT('Ctrl Pts',(18.0343126249969,71.1323459557959,12.3078402197336));
#53902=CARTESIAN_POINT('Ctrl Pts',(18.0231809422392,71.0269505745896,12.3574413891282));
#53903=CARTESIAN_POINT('Ctrl Pts',(18.0152293408142,70.9531931053143,12.4017686786448));
#53904=CARTESIAN_POINT('Ctrl Pts',(18.0038434143002,70.8567358864697,12.4739535123158));
#53905=CARTESIAN_POINT('Ctrl Pts',(18.0005508794765,70.8298677176999,12.4958303912643));
#53906=CARTESIAN_POINT('Ctrl Pts',(17.9943525436072,70.7815728334608,12.5385529841837));
#53907=CARTESIAN_POINT('Ctrl Pts',(17.991458259386,70.7599230154431,12.5591097218628));
#53908=CARTESIAN_POINT('Ctrl Pts',(17.9862496160912,70.7227154160695,12.5970195234435));
#53909=CARTESIAN_POINT('Ctrl Pts',(17.9839488984312,70.7068727845143,12.6140746273569));
#53910=CARTESIAN_POINT('Ctrl Pts',(17.9787736591296,70.6726104877898,12.6530544785039));
#53911=CARTESIAN_POINT('Ctrl Pts',(17.9758903074491,70.6544464551056,12.6751854547461));
#53912=CARTESIAN_POINT('Ctrl Pts',(17.9644907802717,70.5863305040555,12.7641450488083));
#53913=CARTESIAN_POINT('Ctrl Pts',(17.9557694668081,70.5422737533617,12.8352037232949));
#53914=CARTESIAN_POINT('Ctrl Pts',(17.9423837241819,70.4861668115996,12.9494209986068));
#53915=CARTESIAN_POINT('Ctrl Pts',(17.9377683655224,70.4688784489235,12.9897692841891));
#53916=CARTESIAN_POINT('Ctrl Pts',(17.9302615078548,70.4439298467833,13.057483261148));
#53917=CARTESIAN_POINT('Ctrl Pts',(17.9273419383479,70.4350365886228,13.0843558957413));
#53918=CARTESIAN_POINT('Ctrl Pts',(17.9229891842093,70.4229556585547,13.1254133142619));
#53919=CARTESIAN_POINT('Ctrl Pts',(17.921525915318,70.4191015775667,13.1393908411115));
#53920=CARTESIAN_POINT('Ctrl Pts',(17.9185739965236,70.4117420356213,13.167983794663));
#53921=CARTESIAN_POINT('Ctrl Pts',(17.9170864147555,70.4082549276517,13.1826014775612));
#53922=CARTESIAN_POINT('Ctrl Pts',(17.9125896385425,70.3984202553461,13.2273308864539));
#53923=CARTESIAN_POINT('Ctrl Pts',(17.9096203858763,70.3929061963926,13.2576169988945));
#53924=CARTESIAN_POINT('Ctrl Pts',(17.8998223083347,70.3782124163215,13.3591362158437));
#53925=CARTESIAN_POINT('Ctrl Pts',(17.8931374565105,70.3739710988272,13.4309446410726));
#53926=CARTESIAN_POINT('Ctrl Pts',(17.8825602727117,70.3768668947881,13.5432659352113));
#53927=CARTESIAN_POINT('Ctrl Pts',(17.8787269955245,70.3798524706749,13.5837238676785));
#53928=CARTESIAN_POINT('Ctrl Pts',(17.8716882588164,70.3887678897535,13.6567204655158));
#53929=CARTESIAN_POINT('Ctrl Pts',(17.8685017504575,70.3940427608706,13.6893021430525));
#53930=CARTESIAN_POINT('Ctrl Pts',(17.8629796112522,70.4052347088154,13.7446671426077));
#53931=CARTESIAN_POINT('Ctrl Pts',(17.8606643023507,70.4105276398742,13.7675601851188));
#53932=CARTESIAN_POINT('Ctrl Pts',(17.8556767514497,70.423178391136,13.8161007073866));
#53933=CARTESIAN_POINT('Ctrl Pts',(17.8529998485143,70.4307155321467,13.8416890302233));
#53934=CARTESIAN_POINT('Ctrl Pts',(17.8440140117216,70.4584369427401,13.9259209911582));
#53935=CARTESIAN_POINT('Ctrl Pts',(17.8376003499489,70.4821062392049,13.9833128969222));
#53936=CARTESIAN_POINT('Ctrl Pts',(17.824552203637,70.5379202404912,14.0947503930631));
#53937=CARTESIAN_POINT('Ctrl Pts',(17.8179334451509,70.5700799455042,14.1486097409248));
#53938=CARTESIAN_POINT('Ctrl Pts',(17.8088461515945,70.6200693884098,14.2197929446072));
#53939=CARTESIAN_POINT('Ctrl Pts',(17.8063171815365,70.6346271663127,14.2393053947095));
#53940=CARTESIAN_POINT('Ctrl Pts',(17.8019493230965,70.6609776077316,14.2725835627279));
#53941=CARTESIAN_POINT('Ctrl Pts',(17.8001000974776,70.6725205624489,14.2865375263508));
#53942=CARTESIAN_POINT('Ctrl Pts',(17.7982694921739,70.6843589433905,14.3002409815896));
#53943=CARTESIAN_POINT('Origin',(21.26284859951,71.6454,13.47));
#53944=CARTESIAN_POINT('',(16.8359541306755,70.6843588624425,14.3002408878887));
#53945=CARTESIAN_POINT('',(17.0063123822734,70.684359077848,14.3002411372302));
#53946=CARTESIAN_POINT('',(21.26284859951,70.6843589433668,14.3002409815622));
#53947=CARTESIAN_POINT('Ctrl Pts',(16.8359541306755,70.6843588624425,14.3002408878887));
#53948=CARTESIAN_POINT('Ctrl Pts',(16.8379502674075,70.6704802270336,14.2841757437171));
#53949=CARTESIAN_POINT('Ctrl Pts',(16.839950549689,70.6570003623999,14.2677579081367));
#53950=CARTESIAN_POINT('Ctrl Pts',(16.845164028052,70.6230991339372,14.224286865956));
#53951=CARTESIAN_POINT('Ctrl Pts',(16.8483871622081,70.6033442919936,14.1967511909312));
#53952=CARTESIAN_POINT('Ctrl Pts',(16.8544761522747,70.5685314353906,14.1438842720158));
#53953=CARTESIAN_POINT('Ctrl Pts',(16.8573313450209,70.553208424895,14.1187550882452));
#53954=CARTESIAN_POINT('Ctrl Pts',(16.86250082345,70.5273547155229,14.0728402269413));
#53955=CARTESIAN_POINT('Ctrl Pts',(16.8648023568894,70.5164968416139,14.0522534499787));
#53956=CARTESIAN_POINT('Ctrl Pts',(16.8700189304026,70.4933846757216,14.0053528887906));
#53957=CARTESIAN_POINT('Ctrl Pts',(16.8729435958922,70.4814551667086,13.9788949833143));
#53958=CARTESIAN_POINT('Ctrl Pts',(16.883833999383,70.440855195297,13.8799368366222));
#53959=CARTESIAN_POINT('Ctrl Pts',(16.8919723041514,70.4179755336285,13.8052624961549));
#53960=CARTESIAN_POINT('Ctrl Pts',(16.9050765319503,70.3925658381841,13.6832745343453));
#53961=CARTESIAN_POINT('Ctrl Pts',(16.9099932350481,70.3855727693127,13.6370785016066));
#53962=CARTESIAN_POINT('Ctrl Pts',(16.9179075539254,70.3783543322301,13.5614071749565));
#53963=CARTESIAN_POINT('Ctrl Pts',(16.9209362945866,70.3765811922217,13.5321227495037));
#53964=CARTESIAN_POINT('Ctrl Pts',(16.9254123744121,70.3754451816052,13.4881515204587));
#53965=CARTESIAN_POINT('Ctrl Pts',(16.9268922624674,70.3753202490823,13.4734963106848));
#53966=CARTESIAN_POINT('Ctrl Pts',(16.929844092251,70.37557953879,13.4439881082713));
#53967=CARTESIAN_POINT('Ctrl Pts',(16.9313154919548,70.375970619472,13.4291374594395));
#53968=CARTESIAN_POINT('Ctrl Pts',(16.9357893372522,70.3779679132012,13.3836449829257));
#53969=CARTESIAN_POINT('Ctrl Pts',(16.9387515883091,70.3804240206811,13.3530489802766));
#53970=CARTESIAN_POINT('Ctrl Pts',(16.9498826574407,70.3939460650015,13.2373555601887));
#53971=CARTESIAN_POINT('Ctrl Pts',(16.9578311141366,70.4125149637098,13.1533660574458));
#53972=CARTESIAN_POINT('Ctrl Pts',(16.9692135431134,70.4502697839419,13.0389973621562));
#53973=CARTESIAN_POINT('Ctrl Pts',(16.9725058433213,70.462466561564,13.0065697162679));
#53974=CARTESIAN_POINT('Ctrl Pts',(16.9787039585334,70.4876134337804,12.947198712339));
#53975=CARTESIAN_POINT('Ctrl Pts',(16.981598261852,70.5002188097435,12.92013580511));
#53976=CARTESIAN_POINT('Ctrl Pts',(16.9868073685666,70.5243313483591,12.8728006726035));
#53977=CARTESIAN_POINT('Ctrl Pts',(16.9891085369967,70.5354656490704,12.8523532411427));
#53978=CARTESIAN_POINT('Ctrl Pts',(16.9942854473045,70.5615359031707,12.8074604000989));
#53979=CARTESIAN_POINT('Ctrl Pts',(16.9971700354299,70.576749147576,12.7831920746164));
#53980=CARTESIAN_POINT('Ctrl Pts',(17.008560415326,70.6393835052347,12.6904020618607));
#53981=CARTESIAN_POINT('Ctrl Pts',(17.0172706903457,70.6926723967465,12.6261121605154));
#53982=CARTESIAN_POINT('Ctrl Pts',(17.0306508725578,70.7830640764349,12.5366162070676));
#53983=CARTESIAN_POINT('Ctrl Pts',(17.0352716721509,70.8158543917736,12.5073562171363));
#53984=CARTESIAN_POINT('Ctrl Pts',(17.0427860399314,70.8721718040111,12.4621210967851));
#53985=CARTESIAN_POINT('Ctrl Pts',(17.0457077329421,70.8948367125143,12.445130811959));
#53986=CARTESIAN_POINT('Ctrl Pts',(17.0500630526936,70.9299408716333,12.4206056392062));
#53987=CARTESIAN_POINT('Ctrl Pts',(17.0515268098408,70.9419709965363,12.4125038956092));
#53988=CARTESIAN_POINT('Ctrl Pts',(17.0544793513002,70.9667442439723,12.3964301761461));
#53989=CARTESIAN_POINT('Ctrl Pts',(17.0559670726542,70.979495279746,12.3884747877085));
#53990=CARTESIAN_POINT('Ctrl Pts',(17.0604637907267,71.0187745105876,12.3649266313307));
#53991=CARTESIAN_POINT('Ctrl Pts',(17.0634328534424,71.0457330009495,12.3500684711583));
#53992=CARTESIAN_POINT('Ctrl Pts',(17.0732315787877,71.1373148376821,12.3038499911104));
#53993=CARTESIAN_POINT('Ctrl Pts',(17.0799172088496,71.2040548050841,12.2769901861361));
#53994=CARTESIAN_POINT('Ctrl Pts',(17.0904951641001,71.3114743432413,12.2440155964545));
#53995=CARTESIAN_POINT('Ctrl Pts',(17.0943284069696,71.350781175896,12.233980832988));
#53996=CARTESIAN_POINT('Ctrl Pts',(17.1013672436168,71.422824624803,12.219220609583));
#53997=CARTESIAN_POINT('Ctrl Pts',(17.1045538890003,71.4553937696643,12.2138606404425));
#53998=CARTESIAN_POINT('Ctrl Pts',(17.1100765744997,71.511449267714,12.2068652560344));
#53999=CARTESIAN_POINT('Ctrl Pts',(17.1123922954551,71.5348411825001,12.2046033235569));
#54000=CARTESIAN_POINT('Ctrl Pts',(17.1173811510999,71.584897777677,12.2011614333445));
#54001=CARTESIAN_POINT('Ctrl Pts',(17.1200589558797,71.6115634051959,12.2001706246371));
#54002=CARTESIAN_POINT('Ctrl Pts',(17.1290858369526,71.7006423614078,12.199668268823));
#54003=CARTESIAN_POINT('Ctrl Pts',(17.1355413113164,71.7629756245786,12.2039164303789));
#54004=CARTESIAN_POINT('Ctrl Pts',(17.1486007471835,71.8864515560885,12.2215286294965));
#54005=CARTESIAN_POINT('Ctrl Pts',(17.1551872759319,71.9474367062982,12.2348642216444));
#54006=CARTESIAN_POINT('Ctrl Pts',(17.1642373003921,72.0304771966761,12.2595432882361));
#54007=CARTESIAN_POINT('Ctrl Pts',(17.1667609477631,72.05355725548,12.2671293746634));
#54008=CARTESIAN_POINT('Ctrl Pts',(17.1712504847815,72.0945997776521,12.2819370349647));
#54009=CARTESIAN_POINT('Ctrl Pts',(17.1732246725733,72.1126418150013,12.2889160560463));
#54010=CARTESIAN_POINT('Ctrl Pts',(17.1765321714097,72.1429248879647,12.3014328506582));
#54011=CARTESIAN_POINT('Ctrl Pts',(17.1778759447413,72.1552487368115,12.3067568927788));
#54012=CARTESIAN_POINT('Ctrl Pts',(17.1810706229633,72.1845901472999,12.3199887159938));
#54013=CARTESIAN_POINT('Ctrl Pts',(17.1829112245127,72.2015210873649,12.3280799311336));
#54014=CARTESIAN_POINT('Ctrl Pts',(17.1907897820885,72.2738470390506,12.36463471619));
#54015=CARTESIAN_POINT('Ctrl Pts',(17.1966549018235,72.3272936975534,12.3967798227777));
#54016=CARTESIAN_POINT('Ctrl Pts',(17.2098037094555,72.4415776912482,12.4775144449506));
#54017=CARTESIAN_POINT('Ctrl Pts',(17.2170589253695,72.5007355077009,12.5280202908593));
#54018=CARTESIAN_POINT('Ctrl Pts',(17.2274260378182,72.5760580239803,12.6053070860478));
#54019=CARTESIAN_POINT('Ctrl Pts',(17.2303624003649,72.5964214923708,12.6277553958142));
#54020=CARTESIAN_POINT('Ctrl Pts',(17.2356149248811,72.630985811239,12.6687114724665));
#54021=CARTESIAN_POINT('Ctrl Pts',(17.2379165027369,72.6455165714169,12.6869231436508));
#54022=CARTESIAN_POINT('Ctrl Pts',(17.2430557330966,72.6765538054759,12.7280963887751));
#54023=CARTESIAN_POINT('Ctrl Pts',(17.2459014712567,72.6928101230684,12.7512296235364));
#54024=CARTESIAN_POINT('Ctrl Pts',(17.2576524165042,72.7560685944708,12.8479560830587));
#54025=CARTESIAN_POINT('Ctrl Pts',(17.26678806957,72.7961846969771,12.9257467497746));
#54026=CARTESIAN_POINT('Ctrl Pts',(17.2803943905939,72.8433386395253,13.0461922455354));
#54027=CARTESIAN_POINT('Ctrl Pts',(17.2848181234015,72.8567206689711,13.0861085465591));
#54028=CARTESIAN_POINT('Ctrl Pts',(17.2920629203467,72.8755626411892,13.1532000122908));
#54029=CARTESIAN_POINT('Ctrl Pts',(17.2949101057792,72.8821600598556,13.1800219613069));
#54030=CARTESIAN_POINT('Ctrl Pts',(17.2991812538307,72.890858887507,13.2211237710634));
#54031=CARTESIAN_POINT('Ctrl Pts',(17.3006336956985,72.8936001077483,13.2352580206003));
#54032=CARTESIAN_POINT('Ctrl Pts',(17.3035880319527,72.8987337964409,13.2643686046479));
#54033=CARTESIAN_POINT('Ctrl Pts',(17.305088469304,72.9010995836649,13.2793471405344));
#54034=CARTESIAN_POINT('Ctrl Pts',(17.3098053885583,72.9077462890829,13.3269472257574));
#54035=CARTESIAN_POINT('Ctrl Pts',(17.3129748929082,72.9110287781448,13.3596975801237));
#54036=CARTESIAN_POINT('Ctrl Pts',(17.3240643116881,72.9181214440081,13.4757733198151));
#54037=CARTESIAN_POINT('Ctrl Pts',(17.3317950769148,72.9149980632514,13.559306641125));
#54038=CARTESIAN_POINT('Ctrl Pts',(17.3429225431855,72.8990624982484,13.6759312020774));
#54039=CARTESIAN_POINT('Ctrl Pts',(17.3461853877226,72.8930418323433,13.7097223903609));
#54040=CARTESIAN_POINT('Ctrl Pts',(17.3523370701615,72.8792781125012,13.7722003649012));
#54041=CARTESIAN_POINT('Ctrl Pts',(17.3552147605128,72.8718824100622,13.8009393175549));
#54042=CARTESIAN_POINT('Ctrl Pts',(17.3604069398278,72.8569013444631,13.8517148885454));
#54043=CARTESIAN_POINT('Ctrl Pts',(17.3627081686528,72.8497027366733,13.8738520842561));
#54044=CARTESIAN_POINT('Ctrl Pts',(17.3679013402921,72.8322471485367,13.9229050109656));
#54045=CARTESIAN_POINT('Ctrl Pts',(17.370802451131,72.8216749507958,13.9496936592688));
#54046=CARTESIAN_POINT('Ctrl Pts',(17.3800770330949,72.7853596538845,14.0332747275669));
#54047=CARTESIAN_POINT('Ctrl Pts',(17.3865494879895,72.7563447683254,14.0885349994856));
#54048=CARTESIAN_POINT('Ctrl Pts',(17.4005066698503,72.6859939171446,14.2014843657338));
#54049=CARTESIAN_POINT('Ctrl Pts',(17.4079882576799,72.6436376248547,14.2583067620268));
#54050=CARTESIAN_POINT('Ctrl Pts',(17.4178503181667,72.580592356801,14.3295996075902));
#54051=CARTESIAN_POINT('Ctrl Pts',(17.4203599717543,72.5638908540786,14.3474229552307));
#54052=CARTESIAN_POINT('Ctrl Pts',(17.4242500419274,72.5368745890423,14.3746363432778));
#54053=CARTESIAN_POINT('Ctrl Pts',(17.4256517500158,72.526902363284,14.3843563497114));
#54054=CARTESIAN_POINT('Ctrl Pts',(17.4286345206178,72.5051477424299,14.4048738343657));
#54055=CARTESIAN_POINT('Ctrl Pts',(17.4302119054587,72.4933177095941,14.415616686145));
#54056=CARTESIAN_POINT('Ctrl Pts',(17.43544837966,72.4530451967044,14.4508243635592));
#54057=CARTESIAN_POINT('Ctrl Pts',(17.4390458233716,72.4237192820745,14.4742544900942));
#54058=CARTESIAN_POINT('Ctrl Pts',(17.4500385044826,72.3301687276508,14.5424330059884));
#54059=CARTESIAN_POINT('Ctrl Pts',(17.4573028450546,72.2628186307826,14.5825717474207));
#54060=CARTESIAN_POINT('Ctrl Pts',(17.4678801303163,72.1619009041245,14.6307126383981));
#54061=CARTESIAN_POINT('Ctrl Pts',(17.4710751384315,72.1310421460964,14.6439584234647));
#54062=CARTESIAN_POINT('Ctrl Pts',(17.4771196613344,72.0723790579472,14.6664299692564));
#54063=CARTESIAN_POINT('Ctrl Pts',(17.4799588515385,72.044710173669,14.6759464585642));
#54064=CARTESIAN_POINT('Ctrl Pts',(17.4851123503572,71.9944855997353,14.691302909296));
#54065=CARTESIAN_POINT('Ctrl Pts',(17.4874142683972,71.9720504218978,14.6974937383329));
#54066=CARTESIAN_POINT('Ctrl Pts',(17.4926485278792,71.9211233612057,14.7100517715196));
#54067=CARTESIAN_POINT('Ctrl Pts',(17.4955908365224,71.8925577576327,14.7160595736707));
#54068=CARTESIAN_POINT('Ctrl Pts',(17.5060571430106,71.7913219326228,14.733733346607));
#54069=CARTESIAN_POINT('Ctrl Pts',(17.5137303089856,71.7178815674439,14.7400620565365));
#54070=CARTESIAN_POINT('Ctrl Pts',(17.5287987453517,71.5745430262868,14.739940241369));
#54071=CARTESIAN_POINT('Ctrl Pts',(17.5361615722082,71.5048822405677,14.7341303825615));
#54072=CARTESIAN_POINT('Ctrl Pts',(17.545050853754,71.4195441546375,14.7198676074413));
#54073=CARTESIAN_POINT('Ctrl Pts',(17.546757456842,71.403097516912,14.716783662814));
#54074=CARTESIAN_POINT('Ctrl Pts',(17.5498071241747,71.3735452815013,14.7106353082214));
#54075=CARTESIAN_POINT('Ctrl Pts',(17.5511552126588,71.3604192363079,14.7076861446184));
#54076=CARTESIAN_POINT('Ctrl Pts',(17.5542920712509,71.329727142343,14.7002759672918));
#54077=CARTESIAN_POINT('Ctrl Pts',(17.5560720033473,71.3122052388149,14.6956466404526));
#54078=CARTESIAN_POINT('Ctrl Pts',(17.5636398789525,71.2374923738237,14.6741863840508));
#54079=CARTESIAN_POINT('Ctrl Pts',(17.5692665344334,71.1814181620463,14.6537130723811));
#54080=CARTESIAN_POINT('Ctrl Pts',(17.5830649599599,71.0474544455944,14.5938106406161));
#54081=CARTESIAN_POINT('Ctrl Pts',(17.5911891660671,70.9718063104397,14.5501658537986));
#54082=CARTESIAN_POINT('Ctrl Pts',(17.6023102316911,70.8783030703642,14.4825524270219));
#54083=CARTESIAN_POINT('Ctrl Pts',(17.6050598076266,70.8559439559007,14.4652180592734));
#54084=CARTESIAN_POINT('Ctrl Pts',(17.6101050040048,70.8164321065771,14.4324159961435));
#54085=CARTESIAN_POINT('Ctrl Pts',(17.6123899221667,70.7990866290489,14.4171989355864));
#54086=CARTESIAN_POINT('Ctrl Pts',(17.6177045644565,70.7600656457738,14.3810384135039));
#54087=CARTESIAN_POINT('Ctrl Pts',(17.6207465576715,70.7387031385107,14.3597799322167));
#54088=CARTESIAN_POINT('Ctrl Pts',(17.6255371798314,70.7066136276283,14.3254903017749));
#54089=CARTESIAN_POINT('Ctrl Pts',(17.6272633913326,70.6953582812584,14.3129732092515));
#54090=CARTESIAN_POINT('Ctrl Pts',(17.6289974407812,70.6843588693663,14.3002408959033));
#54091=CARTESIAN_POINT('Ctrl Pts',(17.7982694921739,70.6843589433905,14.3002409815896));
#54092=CARTESIAN_POINT('Ctrl Pts',(17.798141983499,70.6851835319912,14.3011954797627));
#54093=CARTESIAN_POINT('Ctrl Pts',(17.7980145652821,70.6860095539031,14.3021487625671));
#54094=CARTESIAN_POINT('Ctrl Pts',(17.7965324570601,70.6956413124015,14.3132310313189));
#54095=CARTESIAN_POINT('Ctrl Pts',(17.7951888424883,70.7046057250814,14.3232211516946));
#54096=CARTESIAN_POINT('Ctrl Pts',(17.7919976091691,70.7264548485502,14.3468069948779));
#54097=CARTESIAN_POINT('Ctrl Pts',(17.7901602215311,70.739484893446,14.3602632509054));
#54098=CARTESIAN_POINT('Ctrl Pts',(17.7819760592256,70.7993647803753,14.4194248688467));
#54099=CARTESIAN_POINT('Ctrl Pts',(17.7758222886051,70.8494141499656,14.4617623107905));
#54100=CARTESIAN_POINT('Ctrl Pts',(17.7644724956504,70.9474075010228,14.5324360714136));
#54101=CARTESIAN_POINT('Ctrl Pts',(17.75928803274,70.9943686310677,14.5618431805322));
#54102=CARTESIAN_POINT('Ctrl Pts',(17.7522416694991,71.0596171213908,14.5969918223241));
#54103=CARTESIAN_POINT('Ctrl Pts',(17.7504498254515,71.0763325757062,14.6055238222977));
#54104=CARTESIAN_POINT('Ctrl Pts',(17.745723218479,71.1206518772488,14.6269211874799));
#54105=CARTESIAN_POINT('Ctrl Pts',(17.742773076104,71.1485381055385,14.6391685674617));
#54106=CARTESIAN_POINT('Ctrl Pts',(17.7375066056104,71.198489415022,14.6589969442097));
#54107=CARTESIAN_POINT('Ctrl Pts',(17.7352051797044,71.2203744606912,14.6669945359056));
#54108=CARTESIAN_POINT('Ctrl Pts',(17.7300789351109,71.2691560696397,14.6833147313981));
#54109=CARTESIAN_POINT('Ctrl Pts',(17.7272462799696,71.2961334417485,14.6913536297841));
#54110=CARTESIAN_POINT('Ctrl Pts',(17.7133070449797,71.4287812536618,14.7261271037611));
#54111=CARTESIAN_POINT('Ctrl Pts',(17.7018121006364,71.5373093967425,14.740072679018));
#54112=CARTESIAN_POINT('Ctrl Pts',(17.6859997248145,71.6880673818012,14.7399717082816));
#54113=CARTESIAN_POINT('Ctrl Pts',(17.6816401613189,71.729862731941,14.7378783747104));
#54114=CARTESIAN_POINT('Ctrl Pts',(17.6756593004317,71.7880195507758,14.7320759996778));
#54115=CARTESIAN_POINT('Ctrl Pts',(17.673971865577,71.8045232333242,14.7301016081262));
#54116=CARTESIAN_POINT('Ctrl Pts',(17.670924941542,71.8345475793578,14.7259103172365));
#54117=CARTESIAN_POINT('Ctrl Pts',(17.669561000977,71.8480780531925,14.7237979005548));
#54118=CARTESIAN_POINT('Ctrl Pts',(17.6659654593287,71.8839391742023,14.7176033821732));
#54119=CARTESIAN_POINT('Ctrl Pts',(17.6637531621711,71.9061994763753,14.7131407789932));
#54120=CARTESIAN_POINT('Ctrl Pts',(17.6585907781158,71.9583372227301,14.7012261023741));
#54121=CARTESIAN_POINT('Ctrl Pts',(17.6556600673009,71.9880874774465,14.6932796331891));
#54122=CARTESIAN_POINT('Ctrl Pts',(17.6444306207584,72.101582752939,14.6584978452878));
#54123=CARTESIAN_POINT('Ctrl Pts',(17.6362799460414,72.1827384372069,14.6240784404604));
#54124=CARTESIAN_POINT('Ctrl Pts',(17.6244143563793,72.2916626430337,14.5638826345195));
#54125=CARTESIAN_POINT('Ctrl Pts',(17.6208997167792,72.32285636335,14.5448427571435));
#54126=CARTESIAN_POINT('Ctrl Pts',(17.6150303068731,72.3728327829704,14.5112980357386));
#54127=CARTESIAN_POINT('Ctrl Pts',(17.6127042130437,72.3921081442529,14.497563535446));
#54128=CARTESIAN_POINT('Ctrl Pts',(17.6078383874262,72.4312534810866,14.467987719911));
#54129=CARTESIAN_POINT('Ctrl Pts',(17.6052966199824,72.4510539678347,14.4520726214928));
#54130=CARTESIAN_POINT('Ctrl Pts',(17.5978271729298,72.5072813189877,14.4040334777152));
#54131=CARTESIAN_POINT('Ctrl Pts',(17.5928421707213,72.5423547401596,14.3704047414771));
#54132=CARTESIAN_POINT('Ctrl Pts',(17.5789078217696,72.6336292891831,14.2722537912588));
#54133=CARTESIAN_POINT('Ctrl Pts',(17.5698486539841,72.68537154262,14.2039386287823));
#54134=CARTESIAN_POINT('Ctrl Pts',(17.557709771735,72.7459720791204,14.1045075597123));
#54135=CARTESIAN_POINT('Ctrl Pts',(17.5545074457054,72.761116175044,14.0774838469117));
#54136=CARTESIAN_POINT('Ctrl Pts',(17.5498365061385,72.7820591896073,14.0366812778136));
#54137=CARTESIAN_POINT('Ctrl Pts',(17.5483312785713,72.7886266611957,14.0233124453545));
#54138=CARTESIAN_POINT('Ctrl Pts',(17.5453776050037,72.801168773399,13.9966042514787));
#54139=CARTESIAN_POINT('Ctrl Pts',(17.5439289695145,72.807151347179,13.9832712435363));
#54140=CARTESIAN_POINT('Ctrl Pts',(17.5396346667906,72.8243386559848,13.9431256818056));
#54141=CARTESIAN_POINT('Ctrl Pts',(17.53682451205,72.8348557878354,13.9160264765483));
#54142=CARTESIAN_POINT('Ctrl Pts',(17.5296454289577,72.8595745239038,13.8452200890158));
#54143=CARTESIAN_POINT('Ctrl Pts',(17.5253235621992,72.872351471927,13.8010599695277));
#54144=CARTESIAN_POINT('Ctrl Pts',(17.5135547910652,72.9005905795693,13.679018946995));
#54145=CARTESIAN_POINT('Ctrl Pts',(17.5061364901567,72.9111912264958,13.6002407992517));
#54146=CARTESIAN_POINT('Ctrl Pts',(17.4957159300682,72.9155375001407,13.4920859852939));
#54147=CARTESIAN_POINT('Ctrl Pts',(17.492906582814,72.9157109144287,13.4631488791133));
#54148=CARTESIAN_POINT('Ctrl Pts',(17.4877829598304,72.9142409633729,13.410974289667));
#54149=CARTESIAN_POINT('Ctrl Pts',(17.4854804063338,72.9129466223417,13.3877393871097));
#54150=CARTESIAN_POINT('Ctrl Pts',(17.480212541908,72.9085653535684,13.3351527491892));
#54151=CARTESIAN_POINT('Ctrl Pts',(17.4772366060782,72.9050921350123,13.3058480712265));
#54152=CARTESIAN_POINT('Ctrl Pts',(17.470764007199,72.8954241158511,13.2430703679757));
#54153=CARTESIAN_POINT('Ctrl Pts',(17.4672599069287,72.8888976230325,13.2096722547715));
#54154=CARTESIAN_POINT('Ctrl Pts',(17.4552785663747,72.8622539155276,13.0974714049901));
#54155=CARTESIAN_POINT('Ctrl Pts',(17.4466727026678,72.835915210799,13.0203525431545));
#54156=CARTESIAN_POINT('Ctrl Pts',(17.4346671529625,72.7885467973745,12.9157054899961));
#54157=CARTESIAN_POINT('Ctrl Pts',(17.4311837785312,72.7734942208113,12.8856790532571));
#54158=CARTESIAN_POINT('Ctrl Pts',(17.4261308528543,72.7495888537697,12.8423699661083));
#54159=CARTESIAN_POINT('Ctrl Pts',(17.424520240526,72.7416491391683,12.828602775594));
#54160=CARTESIAN_POINT('Ctrl Pts',(17.4215244800588,72.726252905447,12.8030278476934));
#54161=CARTESIAN_POINT('Ctrl Pts',(17.4201366167005,72.718857017671,12.7911885940485));
#54162=CARTESIAN_POINT('Ctrl Pts',(17.4163260743003,72.6978503306809,12.7587636595334));
#54163=CARTESIAN_POINT('Ctrl Pts',(17.4139274502792,72.6838320316976,12.738448206734));
#54164=CARTESIAN_POINT('Ctrl Pts',(17.4047102847599,72.6271666217993,12.661243018992));
#54165=CARTESIAN_POINT('Ctrl Pts',(17.3980744836124,72.5803616724605,12.607560070858));
#54166=CARTESIAN_POINT('Ctrl Pts',(17.3855969523363,72.485010437708,12.51513903227));
#54167=CARTESIAN_POINT('Ctrl Pts',(17.3797837431378,72.4376530323125,12.4754957220317));
#54168=CARTESIAN_POINT('Ctrl Pts',(17.3710765894386,72.3642853098365,12.4226557457685));
#54169=CARTESIAN_POINT('Ctrl Pts',(17.3682848859161,72.3404016426804,12.4066569253156));
#54170=CARTESIAN_POINT('Ctrl Pts',(17.3631783751437,72.2962346105837,12.3791948356042));
#54171=CARTESIAN_POINT('Ctrl Pts',(17.3608748893241,72.2761388957315,12.3674530097827));
#54172=CARTESIAN_POINT('Ctrl Pts',(17.355584371041,72.2296754885995,12.3419906479214));
#54173=CARTESIAN_POINT('Ctrl Pts',(17.352586286185,72.2031271530486,12.3286310852776));
#54174=CARTESIAN_POINT('Ctrl Pts',(17.3460515616181,72.1448887439963,12.3018415765696));
#54175=CARTESIAN_POINT('Ctrl Pts',(17.342507122817,72.1130723463133,12.2887442290114));
#54176=CARTESIAN_POINT('Ctrl Pts',(17.330199531502,72.0018369041351,12.2481520945748));
#54177=CARTESIAN_POINT('Ctrl Pts',(17.3212990734474,71.920244606951,12.2272536875131));
#54178=CARTESIAN_POINT('Ctrl Pts',(17.3091615420306,71.805258828653,12.2096869520533));
#54179=CARTESIAN_POINT('Ctrl Pts',(17.3058165878547,71.7731425209669,12.206027617619));
#54180=CARTESIAN_POINT('Ctrl Pts',(17.300986611431,71.7258801783921,12.2024628763886));
#54181=CARTESIAN_POINT('Ctrl Pts',(17.2994614907288,71.7108221358062,12.2015964985493));
#54182=CARTESIAN_POINT('Ctrl Pts',(17.2965033515242,71.6813097716337,12.2004255184732));
#54183=CARTESIAN_POINT('Ctrl Pts',(17.2950696171364,71.6668588974209,12.2000990396116));
#54184=CARTESIAN_POINT('Ctrl Pts',(17.2908922410192,71.6244055833428,12.1998648881052));
#54185=CARTESIAN_POINT('Ctrl Pts',(17.2881811816254,71.5964056443573,12.2006364165488));
#54186=CARTESIAN_POINT('Ctrl Pts',(17.2813680828183,71.5254472352879,12.20494369563));
#54187=CARTESIAN_POINT('Ctrl Pts',(17.2773071733419,71.4826004675668,12.2097408646399));
#54188=CARTESIAN_POINT('Ctrl Pts',(17.2652595552661,71.3561276267572,12.2304605116588));
#54189=CARTESIAN_POINT('Ctrl Pts',(17.2573205669821,71.2737826252714,12.2526115082165));
#54190=CARTESIAN_POINT('Ctrl Pts',(17.246382167238,71.1676543898231,12.2929400448824));
#54191=CARTESIAN_POINT('Ctrl Pts',(17.2436148525212,71.1413837927782,12.3039475234733));
#54192=CARTESIAN_POINT('Ctrl Pts',(17.2387604746136,71.0964674642345,12.3245690723053));
#54193=CARTESIAN_POINT('Ctrl Pts',(17.2366876816335,71.0776480651545,12.333779708639));
#54194=CARTESIAN_POINT('Ctrl Pts',(17.2317448022951,71.0336793031375,12.3566640749602));
#54195=CARTESIAN_POINT('Ctrl Pts',(17.2288620527013,71.0087488329837,12.3707302178225));
#54196=CARTESIAN_POINT('Ctrl Pts',(17.2192338781193,70.927946956376,12.4199906085542));
#54197=CARTESIAN_POINT('Ctrl Pts',(17.2123729633305,70.8743528616671,12.4586929999178));
#54198=CARTESIAN_POINT('Ctrl Pts',(17.1969043749297,70.7619554551436,12.554004823185));
#54199=CARTESIAN_POINT('Ctrl Pts',(17.1882917929023,70.7050899597244,12.6124798420882));
#54200=CARTESIAN_POINT('Ctrl Pts',(17.1781621912139,70.6433154010782,12.6895962824722));
#54201=CARTESIAN_POINT('Ctrl Pts',(17.1763901216421,70.6327034709,12.7034170891637));
#54202=CARTESIAN_POINT('Ctrl Pts',(17.1732749092283,70.6143638683315,12.7283481756195));
#54203=CARTESIAN_POINT('Ctrl Pts',(17.171925481105,70.6065242720765,12.7393699992256));
#54204=CARTESIAN_POINT('Ctrl Pts',(17.1684960116535,70.5868910510645,12.7679279008583));
#54205=CARTESIAN_POINT('Ctrl Pts',(17.1664316471524,70.5753561939184,12.7856368880158));
#54206=CARTESIAN_POINT('Ctrl Pts',(17.1617108520211,70.549761173074,12.8271626154225));
#54207=CARTESIAN_POINT('Ctrl Pts',(17.159069362936,70.5360258941914,12.8511674602022));
#54208=CARTESIAN_POINT('Ctrl Pts',(17.1482066816013,70.4824396322375,12.9523469459207));
#54209=CARTESIAN_POINT('Ctrl Pts',(17.1401610702817,70.4497735727928,13.0330565493502));
#54210=CARTESIAN_POINT('Ctrl Pts',(17.1280650425046,70.4143337348233,13.1553361020459));
#54211=CARTESIAN_POINT('Ctrl Pts',(17.1241858023781,70.4049344902848,13.194714443131));
#54212=CARTESIAN_POINT('Ctrl Pts',(17.1178742009827,70.3929044227454,13.2584564757103));
#54213=CARTESIAN_POINT('Ctrl Pts',(17.1154798966656,70.3890703477681,13.2825661655011));
#54214=CARTESIAN_POINT('Ctrl Pts',(17.1106174439605,70.3827576480057,13.3312741583634));
#54215=CARTESIAN_POINT('Ctrl Pts',(17.1081498100667,70.3802978913764,13.3558640793717));
#54216=CARTESIAN_POINT('Ctrl Pts',(17.101346884584,70.3755411730672,13.4231998794733));
#54217=CARTESIAN_POINT('Ctrl Pts',(17.0969706808001,70.3746857316654,13.4660104356851));
#54218=CARTESIAN_POINT('Ctrl Pts',(17.0859018536995,70.3779506641692,13.572892161135));
#54219=CARTESIAN_POINT('Ctrl Pts',(17.0791547862547,70.3847637419577,13.6367609420507));
#54220=CARTESIAN_POINT('Ctrl Pts',(17.067050200821,70.4055949277603,13.7499674835915));
#54221=CARTESIAN_POINT('Ctrl Pts',(17.0617036569602,70.4178309180044,13.7995052637551));
#54222=CARTESIAN_POINT('Ctrl Pts',(17.0545203528982,70.4386360901675,13.8662037324912));
#54223=CARTESIAN_POINT('Ctrl Pts',(17.0525944326425,70.4446606084608,13.8841033494241));
#54224=CARTESIAN_POINT('Ctrl Pts',(17.0493356287976,70.4556459059956,13.914483150699));
#54225=CARTESIAN_POINT('Ctrl Pts',(17.0479932601698,70.460408792843,13.9270295105315));
#54226=CARTESIAN_POINT('Ctrl Pts',(17.0447573498571,70.4724689026983,13.957341080051));
#54227=CARTESIAN_POINT('Ctrl Pts',(17.0428751147352,70.4799717218789,13.9750205575763));
#54228=CARTESIAN_POINT('Ctrl Pts',(17.0354731465754,70.5113260111044,14.044478359014));
#54229=CARTESIAN_POINT('Ctrl Pts',(17.0300925955928,70.5382534603744,14.0948021249747));
#54230=CARTESIAN_POINT('Ctrl Pts',(17.0185997033284,70.6030362158332,14.1984429932677));
#54231=CARTESIAN_POINT('Ctrl Pts',(17.0125116167312,70.6417826788887,14.2509570679605));
#54232=CARTESIAN_POINT('Ctrl Pts',(17.0063123822734,70.684359077848,14.3002411372302));
#54233=CARTESIAN_POINT('Origin',(21.26284859951,71.6454,13.47));
#54234=CARTESIAN_POINT('',(16.0430985027246,70.6843589375946,14.3002409748806));
#54235=CARTESIAN_POINT('',(16.2122439422732,70.6843594233383,14.3002415371503));
#54236=CARTESIAN_POINT('',(21.26284859951,70.6843589433668,14.3002409815622));
#54237=CARTESIAN_POINT('',(16.7267333334667,71.6459398759342,14.7399998852496));
#54238=CARTESIAN_POINT('Ctrl Pts',(16.0430985027246,70.6843589375946,14.3002409748806));
#54239=CARTESIAN_POINT('Ctrl Pts',(16.0457968979002,70.6674222330724,14.2806359818724));
#54240=CARTESIAN_POINT('Ctrl Pts',(16.0484768065757,70.6510861315913,14.2605135379007));
#54241=CARTESIAN_POINT('Ctrl Pts',(16.0527622312145,70.6256610843513,14.2271586801896));
#54242=CARTESIAN_POINT('Ctrl Pts',(16.0543868472531,70.6161889809723,14.214232150367));
#54243=CARTESIAN_POINT('Ctrl Pts',(16.0573913841616,70.598958209715,14.1897589394869));
#54244=CARTESIAN_POINT('Ctrl Pts',(16.0587743359645,70.5911407522425,14.1782590115397));
#54245=CARTESIAN_POINT('Ctrl Pts',(16.062541736419,70.5701951498698,14.1463312665806));
#54246=CARTESIAN_POINT('Ctrl Pts',(16.0649031021133,70.5574609504884,14.1256510850315));
#54247=CARTESIAN_POINT('Ctrl Pts',(16.0740356478369,70.5100715005747,14.0435039596709));
#54248=CARTESIAN_POINT('Ctrl Pts',(16.0806243220723,70.4799661824146,13.9795527786189));
#54249=CARTESIAN_POINT('Ctrl Pts',(16.0931429713713,70.4334428877496,13.8546925219963));
#54250=CARTESIAN_POINT('Ctrl Pts',(16.0990465919072,70.4159394548933,13.79442807718));
#54251=CARTESIAN_POINT('Ctrl Pts',(16.1078560149509,70.3969842815363,13.704923595019));
#54252=CARTESIAN_POINT('Ctrl Pts',(16.1106555016447,70.3919745181581,13.6765312641368));
#54253=CARTESIAN_POINT('Ctrl Pts',(16.1157700230282,70.3846731502045,13.6249501327009));
#54254=CARTESIAN_POINT('Ctrl Pts',(16.1180735670501,70.3820454634826,13.6018213627777));
#54255=CARTESIAN_POINT('Ctrl Pts',(16.1233558714868,70.3775199257024,13.5491095100516));
#54256=CARTESIAN_POINT('Ctrl Pts',(16.1263455138177,70.3760194991303,13.5195073329416));
#54257=CARTESIAN_POINT('Ctrl Pts',(16.132856267677,70.3750194387979,13.45563679349));
#54258=CARTESIAN_POINT('Ctrl Pts',(16.1363850341362,70.3758688426986,13.4213869355575));
#54259=CARTESIAN_POINT('Ctrl Pts',(16.1485626788231,70.3835070596596,13.304456328561));
#54260=CARTESIAN_POINT('Ctrl Pts',(16.1573453525061,70.3970073472099,13.2224265162086));
#54261=CARTESIAN_POINT('Ctrl Pts',(16.1694847267194,70.4270053216461,13.1101034867471));
#54262=CARTESIAN_POINT('Ctrl Pts',(16.1729384506198,70.4368717438836,13.0782461280851));
#54263=CARTESIAN_POINT('Ctrl Pts',(16.1778891261556,70.4530531023261,13.0324608572622));
#54264=CARTESIAN_POINT('Ctrl Pts',(16.1794289167543,70.4583824481663,13.0182024360809));
#54265=CARTESIAN_POINT('Ctrl Pts',(16.1823920958983,70.469233471263,12.9906897528119));
#54266=CARTESIAN_POINT('Ctrl Pts',(16.1838165694037,70.4747259248912,12.9774268798847));
#54267=CARTESIAN_POINT('Ctrl Pts',(16.1879200104552,70.4913256204301,12.9391900256512));
#54268=CARTESIAN_POINT('Ctrl Pts',(16.1905682066448,70.5030165192185,12.914475699644));
#54269=CARTESIAN_POINT('Ctrl Pts',(16.1971564154835,70.5343774926917,12.8533647998398));
#54270=CARTESIAN_POINT('Ctrl Pts',(16.2010587474533,70.5550449202772,12.8175152148751));
#54271=CARTESIAN_POINT('Ctrl Pts',(16.2133148394049,70.6255639530281,12.7079323550637));
#54272=CARTESIAN_POINT('Ctrl Pts',(16.2216049834242,70.6814206568381,12.6384027979274));
#54273=CARTESIAN_POINT('Ctrl Pts',(16.232889006636,70.7638751976796,12.5553395806403));
#54274=CARTESIAN_POINT('Ctrl Pts',(16.2356214223749,70.784326892134,12.536060771956));
#54275=CARTESIAN_POINT('Ctrl Pts',(16.2406726793659,70.8228793148967,12.5020625543492));
#54276=CARTESIAN_POINT('Ctrl Pts',(16.2429815654238,70.8407788325318,12.4871328802961));
#54277=CARTESIAN_POINT('Ctrl Pts',(16.2483612149538,70.8830482039205,12.4538053636938));
#54278=CARTESIAN_POINT('Ctrl Pts',(16.2514446714262,70.9076898003573,12.435778039574));
#54279=CARTESIAN_POINT('Ctrl Pts',(16.2612931713798,70.9875625533193,12.3816519974347));
#54280=CARTESIAN_POINT('Ctrl Pts',(16.2681664630672,71.0449615646673,12.3489637362893));
#54281=CARTESIAN_POINT('Ctrl Pts',(16.2829762029345,71.1725051602726,12.2889420006337));
#54282=CARTESIAN_POINT('Ctrl Pts',(16.2909028634937,71.243084278038,12.2630734331405));
#54283=CARTESIAN_POINT('Ctrl Pts',(16.3004361507145,71.3327718454888,12.2389508386255));
#54284=CARTESIAN_POINT('Ctrl Pts',(16.3022535096169,71.3501006586327,12.2346794669514));
#54285=CARTESIAN_POINT('Ctrl Pts',(16.3054072904684,71.3806378251507,12.2278317949933));
#54286=CARTESIAN_POINT('Ctrl Pts',(16.3067509586642,71.3938058723744,12.225097873495));
#54287=CARTESIAN_POINT('Ctrl Pts',(16.3100682562025,71.4266897744507,12.2188137684601));
#54288=CARTESIAN_POINT('Ctrl Pts',(16.3120287117846,71.4464506851388,12.2155198353924));
#54289=CARTESIAN_POINT('Ctrl Pts',(16.3164494241793,71.4915824854841,12.2090903230319));
#54290=CARTESIAN_POINT('Ctrl Pts',(16.3188974282113,71.5169870352588,12.2062502681149));
#54291=CARTESIAN_POINT('Ctrl Pts',(16.3280224752007,71.6126231325824,12.198473047548));
#54292=CARTESIAN_POINT('Ctrl Pts',(16.3345741363555,71.6831402226275,12.1986102755095));
#54293=CARTESIAN_POINT('Ctrl Pts',(16.3461695590771,71.8056954850464,12.2090590389518));
#54294=CARTESIAN_POINT('Ctrl Pts',(16.3511627399253,71.8577702626365,12.2167783960845));
#54295=CARTESIAN_POINT('Ctrl Pts',(16.3588053718384,71.9350439962628,12.2331880600946));
#54296=CARTESIAN_POINT('Ctrl Pts',(16.361381637426,71.9606968865318,12.2394777316628));
#54297=CARTESIAN_POINT('Ctrl Pts',(16.366305144797,72.0088335147517,12.2528839972188));
#54298=CARTESIAN_POINT('Ctrl Pts',(16.3686461991881,72.0313516823379,12.2598362103956));
#54299=CARTESIAN_POINT('Ctrl Pts',(16.3743790819279,72.0855139863246,12.2782235192926));
#54300=CARTESIAN_POINT('Ctrl Pts',(16.3777900561168,72.1169201757066,12.2902967742913));
#54301=CARTESIAN_POINT('Ctrl Pts',(16.3884831092456,72.2127057857513,12.3315548066305));
#54302=CARTESIAN_POINT('Ctrl Pts',(16.3958819671871,72.2751484555832,12.3648723377557));
#54303=CARTESIAN_POINT('Ctrl Pts',(16.4097904124291,72.3862180546076,12.4366166187168));
#54304=CARTESIAN_POINT('Ctrl Pts',(16.4162725582957,72.4354551667727,12.4737535123514));
#54305=CARTESIAN_POINT('Ctrl Pts',(16.4245334987823,72.4959311524592,12.5266819004187));
#54306=CARTESIAN_POINT('Ctrl Pts',(16.4264475117904,72.5097805834224,12.5393558027144));
#54307=CARTESIAN_POINT('Ctrl Pts',(16.4296948513491,72.5330448506227,12.561613069218));
#54308=CARTESIAN_POINT('Ctrl Pts',(16.4310374147878,72.542596666844,12.5710459435503));
#54309=CARTESIAN_POINT('Ctrl Pts',(16.4342861248444,72.5655363158127,12.5944299779381));
#54310=CARTESIAN_POINT('Ctrl Pts',(16.4361806747742,72.5787584468723,12.6085385306702));
#54311=CARTESIAN_POINT('Ctrl Pts',(16.4437093813169,72.6304700397462,12.6663061199528));
#54312=CARTESIAN_POINT('Ctrl Pts',(16.4491985022156,72.6662651905521,12.7122908582067));
#54313=CARTESIAN_POINT('Ctrl Pts',(16.4627012773735,72.7464985118428,12.8314247455208));
#54314=CARTESIAN_POINT('Ctrl Pts',(16.4706719241718,72.7869384116978,12.90689797198));
#54315=CARTESIAN_POINT('Ctrl Pts',(16.4816418452697,72.8303412577702,13.0121533431639));
#54316=CARTESIAN_POINT('Ctrl Pts',(16.484406477761,72.8402987091472,13.0388084760384));
#54317=CARTESIAN_POINT('Ctrl Pts',(16.4894657680989,72.8566930970429,13.0876376318978));
#54318=CARTESIAN_POINT('Ctrl Pts',(16.4917493785743,72.863436511984,13.109696196646));
#54319=CARTESIAN_POINT('Ctrl Pts',(16.497041839608,72.8775424293203,13.1607738630282));
#54320=CARTESIAN_POINT('Ctrl Pts',(16.5000625507064,72.8844864841561,13.189892737007));
#54321=CARTESIAN_POINT('Ctrl Pts',(16.506660675449,72.8972627991428,13.2533223385596));
#54322=CARTESIAN_POINT('Ctrl Pts',(16.510246259894,72.9027262477712,13.2876819193343));
#54323=CARTESIAN_POINT('Ctrl Pts',(16.5229015036442,72.9168880680095,13.4085588906867));
#54324=CARTESIAN_POINT('Ctrl Pts',(16.5321173608654,72.9181116066767,13.4957021797642));
#54325=CARTESIAN_POINT('Ctrl Pts',(16.5442613612533,72.9078021753878,13.6118516610837));
#54326=CARTESIAN_POINT('Ctrl Pts',(16.5473280716812,72.9041415624331,13.6413220482175));
#54327=CARTESIAN_POINT('Ctrl Pts',(16.5518469196775,72.8971273743986,13.6851624261185));
#54328=CARTESIAN_POINT('Ctrl Pts',(16.5533324775568,72.8945516433668,13.6996443741214));
#54329=CARTESIAN_POINT('Ctrl Pts',(16.5562845024886,72.8888808433309,13.7286007425306));
#54330=CARTESIAN_POINT('Ctrl Pts',(16.5577506007882,72.8857832100899,13.7430723719536));
#54331=CARTESIAN_POINT('Ctrl Pts',(16.5621818089575,72.8755755493909,13.7869949786106));
#54332=CARTESIAN_POINT('Ctrl Pts',(16.5651078589645,72.8676635913933,13.816251183943));
#54333=CARTESIAN_POINT('Ctrl Pts',(16.5727350589945,72.8440929937661,13.8924731543663));
#54334=CARTESIAN_POINT('Ctrl Pts',(16.5773813486742,72.8267228578877,13.9388556034495));
#54335=CARTESIAN_POINT('Ctrl Pts',(16.5889057482074,72.7770485600492,14.0510616891612));
#54336=CARTESIAN_POINT('Ctrl Pts',(16.5957693602683,72.7416776939111,14.1153172774884));
#54337=CARTESIAN_POINT('Ctrl Pts',(16.6056231888466,72.6847402958427,14.2004272484636));
#54338=CARTESIAN_POINT('Ctrl Pts',(16.6084567155664,72.6676779472616,14.2241218101357));
#54339=CARTESIAN_POINT('Ctrl Pts',(16.6136045941521,72.6355746532537,14.2656102737153));
#54340=CARTESIAN_POINT('Ctrl Pts',(16.6159066835507,72.6208313240242,14.2836185268508));
#54341=CARTESIAN_POINT('Ctrl Pts',(16.6211474212582,72.5864613865069,14.3233222143153));
#54342=CARTESIAN_POINT('Ctrl Pts',(16.6240961612231,72.5665639342111,14.3447639619623));
#54343=CARTESIAN_POINT('Ctrl Pts',(16.6304924747682,72.5222842886282,14.3892932357848));
#54344=CARTESIAN_POINT('Ctrl Pts',(16.6339470456236,72.4976910599992,14.4121388427561));
#54345=CARTESIAN_POINT('Ctrl Pts',(16.6455457431029,72.4129073320717,14.484859386742));
#54346=CARTESIAN_POINT('Ctrl Pts',(16.6538087375679,72.3490231210971,14.5301508471307));
#54347=CARTESIAN_POINT('Ctrl Pts',(16.6659248330474,72.2488482508594,14.5881071698422));
#54348=CARTESIAN_POINT('Ctrl Pts',(16.6698334605561,72.2154821875759,14.6054824716453));
#54349=CARTESIAN_POINT('Ctrl Pts',(16.6753098507987,72.1668898627127,14.6281036878441));
#54350=CARTESIAN_POINT('Ctrl Pts',(16.6769315198381,72.1522619251528,14.6345801429689));
#54351=CARTESIAN_POINT('Ctrl Pts',(16.6799342636315,72.1246845391829,14.6461717617547));
#54352=CARTESIAN_POINT('Ctrl Pts',(16.6813183016168,72.1117676062248,14.6513530277532));
#54353=CARTESIAN_POINT('Ctrl Pts',(16.6850949991853,72.0760079642927,14.6650189822818));
#54354=CARTESIAN_POINT('Ctrl Pts',(16.6874643684248,72.053001423548,14.6730606542094));
#54355=CARTESIAN_POINT('Ctrl Pts',(16.7023510980548,71.9056438873701,14.7198541786761));
#54356=CARTESIAN_POINT('Ctrl Pts',(16.7142149269752,71.776189436049,14.7399445162659));
#54357=CARTESIAN_POINT('Ctrl Pts',(16.7267333334667,71.6459398759342,14.7399998852496));
#54358=CARTESIAN_POINT('Ctrl Pts',(16.7267334568494,71.6459385921818,14.7399998857947));
#54359=CARTESIAN_POINT('Ctrl Pts',(16.7283087818113,71.6295479013485,14.740006836896));
#54360=CARTESIAN_POINT('Ctrl Pts',(16.7298917004701,71.6131592909544,14.7396964791053));
#54361=CARTESIAN_POINT('Ctrl Pts',(16.7330390453341,71.580778104527,14.7384559543814));
#54362=CARTESIAN_POINT('Ctrl Pts',(16.7346027597629,71.5647882063487,14.737540209352));
#54363=CARTESIAN_POINT('Ctrl Pts',(16.7382648806629,71.5276094436234,14.734704677072));
#54364=CARTESIAN_POINT('Ctrl Pts',(16.7403696744464,71.5064438224708,14.7325543873976));
#54365=CARTESIAN_POINT('Ctrl Pts',(16.7453608999044,71.4567999988391,14.7262475601839));
#54366=CARTESIAN_POINT('Ctrl Pts',(16.7482597949872,71.4283908518236,14.7216527421321));
#54367=CARTESIAN_POINT('Ctrl Pts',(16.7575898068153,71.3384385650118,14.7039499174054));
#54368=CARTESIAN_POINT('Ctrl Pts',(16.7641223705281,71.2777112705777,14.6872345896589));
#54369=CARTESIAN_POINT('Ctrl Pts',(16.7781172477619,71.1520650620468,14.6423880758682));
#54370=CARTESIAN_POINT('Ctrl Pts',(16.7855743677902,71.0877359687437,14.6131906449981));
#54371=CARTESIAN_POINT('Ctrl Pts',(16.7953939221386,71.004987842676,14.5669778454279));
#54372=CARTESIAN_POINT('Ctrl Pts',(16.7978859896184,70.9841553711275,14.5545477964833));
#54373=CARTESIAN_POINT('Ctrl Pts',(16.8017562938427,70.9519619005673,14.5340661676507));
#54374=CARTESIAN_POINT('Ctrl Pts',(16.8031554588882,70.9403563019843,14.5264121756627));
#54375=CARTESIAN_POINT('Ctrl Pts',(16.8061409864774,70.9156406799535,14.509523135718));
#54376=CARTESIAN_POINT('Ctrl Pts',(16.8077235302394,70.9025754642845,14.5002275561205));
#54377=CARTESIAN_POINT('Ctrl Pts',(16.8126723557012,70.861939127614,14.4701405988433));
#54378=CARTESIAN_POINT('Ctrl Pts',(16.8159887023894,70.8350353009879,14.4484691314138));
#54379=CARTESIAN_POINT('Ctrl Pts',(16.8248913408023,70.7645987474944,14.3868301062798));
#54380=CARTESIAN_POINT('Ctrl Pts',(16.8304053615477,70.7229380551678,14.3448980371615));
#54381=CARTESIAN_POINT('Ctrl Pts',(16.8359541306755,70.6843588624425,14.3002408878887));
#54382=CARTESIAN_POINT('',(16.8971557431799,71.644308511249,14.7399995524375));
#54383=CARTESIAN_POINT('Ctrl Pts',(17.0063123822734,70.684359077848,14.3002411372302));
#54384=CARTESIAN_POINT('Ctrl Pts',(17.004197651672,70.698883066962,14.3170532984994));
#54385=CARTESIAN_POINT('Ctrl Pts',(17.0020705965369,70.7138527786965,14.3334896321051));
#54386=CARTESIAN_POINT('Ctrl Pts',(16.9972041541103,70.7488190402137,14.3699114831557));
#54387=CARTESIAN_POINT('Ctrl Pts',(16.9944579065253,70.7690565036005,14.3896302987457));
#54388=CARTESIAN_POINT('Ctrl Pts',(16.9893944179429,70.8071477492386,14.4243456783912));
#54389=CARTESIAN_POINT('Ctrl Pts',(16.9870874591459,70.824789601238,14.4395570667382));
#54390=CARTESIAN_POINT('Ctrl Pts',(16.9817318988848,70.8663295627702,14.4734281181958));
#54391=CARTESIAN_POINT('Ctrl Pts',(16.9786710336641,70.8904963976887,14.4917332802506));
#54392=CARTESIAN_POINT('Ctrl Pts',(16.9676687233899,70.9787221351955,14.5537204766961));
#54393=CARTESIAN_POINT('Ctrl Pts',(16.959562782828,71.0460874754797,14.5923767615868));
#54394=CARTESIAN_POINT('Ctrl Pts',(16.9448515577804,71.1732459639556,14.6506187042339));
#54395=CARTESIAN_POINT('Ctrl Pts',(16.9382850872234,71.2317927333729,14.6723812401327));
#54396=CARTESIAN_POINT('Ctrl Pts',(16.9299447864436,71.3097225241116,14.6949785555521));
#54397=CARTESIAN_POINT('Ctrl Pts',(16.9280320252777,71.3278528476496,14.6998031435263));
#54398=CARTESIAN_POINT('Ctrl Pts',(16.9247861977611,71.3591281407649,14.7073877921821));
#54399=CARTESIAN_POINT('Ctrl Pts',(16.9234439153868,71.3722203610649,14.7103439313893));
#54400=CARTESIAN_POINT('Ctrl Pts',(16.9207753841692,71.3985577590331,14.7158534155939));
#54401=CARTESIAN_POINT('Ctrl Pts',(16.9194490701011,71.411800421194,14.7184042274095));
#54402=CARTESIAN_POINT('Ctrl Pts',(16.9161224519484,71.4453424246085,14.724312633018));
#54403=CARTESIAN_POINT('Ctrl Pts',(16.9141347009732,71.465688166774,14.7273889680941));
#54404=CARTESIAN_POINT('Ctrl Pts',(16.9070905615411,71.5385729425552,14.7366038270448));
#54405=CARTESIAN_POINT('Ctrl Pts',(16.9021236939593,71.5914116579932,14.7399540766915));
#54406=CARTESIAN_POINT('Ctrl Pts',(16.8971556908388,71.644308689214,14.7399995311183));
#54407=CARTESIAN_POINT('Ctrl Pts',(16.8971557078627,71.6443085079506,14.7399995309626));
#54408=CARTESIAN_POINT('Ctrl Pts',(16.8898238968171,71.7223742875591,14.7400666240407));
#54409=CARTESIAN_POINT('Ctrl Pts',(16.882508327921,71.8002722681029,14.7329359717819));
#54410=CARTESIAN_POINT('Ctrl Pts',(16.8727912006366,71.8993012955568,14.7145672832214));
#54411=CARTESIAN_POINT('Ctrl Pts',(16.8705895249596,71.9214674462307,14.7098387834532));
#54412=CARTESIAN_POINT('Ctrl Pts',(16.8660858590211,71.9661548910853,14.699048318925));
#54413=CARTESIAN_POINT('Ctrl Pts',(16.8637836867908,71.9886591633842,14.6929539814569));
#54414=CARTESIAN_POINT('Ctrl Pts',(16.8586773709661,72.0377433907596,14.6782001431898));
#54415=CARTESIAN_POINT('Ctrl Pts',(16.8558658082793,72.0642299333635,14.6692756567084));
#54416=CARTESIAN_POINT('Ctrl Pts',(16.8439362426966,72.1741923750001,14.6281376483414));
#54417=CARTESIAN_POINT('Ctrl Pts',(16.8345724598089,72.2544218625557,14.588029396472));
#54418=CARTESIAN_POINT('Ctrl Pts',(16.8208188623443,72.364563975149,14.5175736741248));
#54419=CARTESIAN_POINT('Ctrl Pts',(16.8164753270358,72.3982672151862,14.4936204339921));
#54420=CARTESIAN_POINT('Ctrl Pts',(16.8093410991244,72.4522114516593,14.4511735044182));
#54421=CARTESIAN_POINT('Ctrl Pts',(16.8065250984956,72.4731304823411,14.4335915921712));
#54422=CARTESIAN_POINT('Ctrl Pts',(16.8022893732432,72.5041490837958,14.4057648737795));
#54423=CARTESIAN_POINT('Ctrl Pts',(16.8008418512951,72.5146678438209,14.396001831948));
#54424=CARTESIAN_POINT('Ctrl Pts',(16.7978870823546,72.5359959971195,14.3755221262385));
#54425=CARTESIAN_POINT('Ctrl Pts',(16.79638145965,72.5467826692345,14.3647854026018));
#54426=CARTESIAN_POINT('Ctrl Pts',(16.7916178843376,72.5805686988698,14.3299245332641));
#54427=CARTESIAN_POINT('Ctrl Pts',(16.7884082804306,72.6028148749541,14.3050856558141));
#54428=CARTESIAN_POINT('Ctrl Pts',(16.7773253388925,72.6769157129473,14.2154886056859));
#54429=CARTESIAN_POINT('Ctrl Pts',(16.7696355309042,72.7233863344534,14.1465537832464));
#54430=CARTESIAN_POINT('Ctrl Pts',(16.758556340246,72.7790822133142,14.0434435984024));
#54431=CARTESIAN_POINT('Ctrl Pts',(16.7552993748435,72.794131917593,14.01266707184));
#54432=CARTESIAN_POINT('Ctrl Pts',(16.7491571198527,72.8198488467096,13.954198254189));
#54433=CARTESIAN_POINT('Ctrl Pts',(16.7462829079392,72.8308249652517,13.9266676830575));
#54434=CARTESIAN_POINT('Ctrl Pts',(16.7410947149974,72.8486841728902,13.8768767856202));
#54435=CARTESIAN_POINT('Ctrl Pts',(16.7387939227902,72.8559366580059,13.8547627098241));
#54436=CARTESIAN_POINT('Ctrl Pts',(16.7335990037933,72.8708010811997,13.8048469867171));
#54437=CARTESIAN_POINT('Ctrl Pts',(16.730695657524,72.8780819001586,13.7769614150034));
#54438=CARTESIAN_POINT('Ctrl Pts',(16.7213875882034,72.8981626607147,13.6877386912922));
#54439=CARTESIAN_POINT('Ctrl Pts',(16.714882684886,72.9073744481245,13.625699308249));
#54440=CARTESIAN_POINT('Ctrl Pts',(16.7009097523629,72.9171544489058,13.4928537296476));
#54441=CARTESIAN_POINT('Ctrl Pts',(16.6934460971044,72.9164598121784,13.4221515159564));
#54442=CARTESIAN_POINT('Ctrl Pts',(16.6836151426093,72.9076342362242,13.3276798310376));
#54443=CARTESIAN_POINT('Ctrl Pts',(16.6811183426748,72.9046803614261,13.3035562331351));
#54444=CARTESIAN_POINT('Ctrl Pts',(16.6772429129132,72.8989504209894,13.2657827898844));
#54445=CARTESIAN_POINT('Ctrl Pts',(16.6758432547822,72.8966392856017,13.2520695727065));
#54446=CARTESIAN_POINT('Ctrl Pts',(16.6728592699188,72.8911832000533,13.2226529515872));
#54447=CARTESIAN_POINT('Ctrl Pts',(16.6712787153827,72.8879656900088,13.2069658901296));
#54448=CARTESIAN_POINT('Ctrl Pts',(16.6663453493649,72.8769068257915,13.1577925972059));
#54449=CARTESIAN_POINT('Ctrl Pts',(16.6630420265283,72.8680010488162,13.1245585085759));
#54450=CARTESIAN_POINT('Ctrl Pts',(16.6521171240674,72.8337932408401,13.0149245286979));
#54451=CARTESIAN_POINT('Ctrl Pts',(16.6446521472556,72.8025869702987,12.9405741658649));
#54452=CARTESIAN_POINT('Ctrl Pts',(16.6338376972792,72.7485319296961,12.8398024620172));
#54453=CARTESIAN_POINT('Ctrl Pts',(16.6306128764712,72.7313208429047,12.8105877093923));
#54454=CARTESIAN_POINT('Ctrl Pts',(16.624521374348,72.6970194685702,12.7573549754655));
#54455=CARTESIAN_POINT('Ctrl Pts',(16.6216653789363,72.6802218495953,12.7331758277679));
#54456=CARTESIAN_POINT('Ctrl Pts',(16.616495560632,72.6486698053715,12.6909678536147));
#54457=CARTESIAN_POINT('Ctrl Pts',(16.6141945154045,72.6342302321114,12.6727196331824));
#54458=CARTESIAN_POINT('Ctrl Pts',(16.6089806080293,72.6006880935583,12.6326437718998));
#54459=CARTESIAN_POINT('Ctrl Pts',(16.6060581555061,72.5813233460385,12.6110541684249));
#54460=CARTESIAN_POINT('Ctrl Pts',(16.5951373623247,72.5070105948463,12.5337019418147));
#54461=CARTESIAN_POINT('Ctrl Pts',(16.586964625559,72.4476908140349,12.4824010763034));
#54462=CARTESIAN_POINT('Ctrl Pts',(16.5738449414483,72.3462099571882,12.4098451833775));
#54463=CARTESIAN_POINT('Ctrl Pts',(16.5689473042014,72.3069196023169,12.3848939863757));
#54464=CARTESIAN_POINT('Ctrl Pts',(16.5610586935099,72.2408223042171,12.3478464930218));
#54465=CARTESIAN_POINT('Ctrl Pts',(16.5580367864398,72.2148072901669,12.3344243942052));
#54466=CARTESIAN_POINT('Ctrl Pts',(16.5535685769488,72.1751124023486,12.3156520644182));
#54467=CARTESIAN_POINT('Ctrl Pts',(16.5520898803886,72.1617675122463,12.3096211577383));
#54468=CARTESIAN_POINT('Ctrl Pts',(16.5491387126947,72.134675934975,12.2979377812818));
#54469=CARTESIAN_POINT('Ctrl Pts',(16.5476668100528,72.1209283926963,12.2922930712419));
#54470=CARTESIAN_POINT('Ctrl Pts',(16.5431876756537,72.078456251728,12.2757192066058));
#54471=CARTESIAN_POINT('Ctrl Pts',(16.5402207867651,72.0494289784177,12.2655891885108));
#54472=CARTESIAN_POINT('Ctrl Pts',(16.5290909242515,71.9381383450991,12.2312284329666));
#54473=CARTESIAN_POINT('Ctrl Pts',(16.5211475557702,71.8538618847231,12.2142944037521));
#54474=CARTESIAN_POINT('Ctrl Pts',(16.5097712556462,71.7340551849804,12.2026251064423));
#54475=CARTESIAN_POINT('Ctrl Pts',(16.5064798142118,71.6994736477007,12.2006794951786));
#54476=CARTESIAN_POINT('Ctrl Pts',(16.5002832041892,71.6350202433553,12.1996918564423));
#54477=CARTESIAN_POINT('Ctrl Pts',(16.497389538913,71.6051782909937,12.2002864869158));
#54478=CARTESIAN_POINT('Ctrl Pts',(16.4921815380517,71.5521476492758,12.2032144063171));
#54479=CARTESIAN_POINT('Ctrl Pts',(16.4898808301082,71.528949368463,12.205136048595));
#54480=CARTESIAN_POINT('Ctrl Pts',(16.4847050369037,71.477361280463,12.2108404704477));
#54481=CARTESIAN_POINT('Ctrl Pts',(16.4818211101908,71.4490213727214,12.2149482735687));
#54482=CARTESIAN_POINT('Ctrl Pts',(16.4704274426051,71.3388016828337,12.2347485379884));
#54483=CARTESIAN_POINT('Ctrl Pts',(16.4617129656493,71.2584232391943,12.2575264454181));
#54484=CARTESIAN_POINT('Ctrl Pts',(16.4483307050129,71.1400180036888,12.3040600982079));
#54485=CARTESIAN_POINT('Ctrl Pts',(16.4437120140976,71.1000218819484,12.3222239138478));
#54486=CARTESIAN_POINT('Ctrl Pts',(16.4362006204221,71.0359127986102,12.3554478021766));
#54487=CARTESIAN_POINT('Ctrl Pts',(16.4332798130589,71.0112202768836,12.3693103510359));
#54488=CARTESIAN_POINT('Ctrl Pts',(16.4289256651814,70.9746111516071,12.3915045096295));
#54489=CARTESIAN_POINT('Ctrl Pts',(16.4274622125727,70.9623415891651,12.3992332214284));
#54490=CARTESIAN_POINT('Ctrl Pts',(16.424510324749,70.9376334031449,12.4153947945783));
#54491=CARTESIAN_POINT('Ctrl Pts',(16.4230229512688,70.9252067403691,12.4238415784146));
#54492=CARTESIAN_POINT('Ctrl Pts',(16.418527791186,70.887807170194,12.450245623516));
#54493=CARTESIAN_POINT('Ctrl Pts',(16.4155599037374,70.8633318731906,12.4688927062628));
#54494=CARTESIAN_POINT('Ctrl Pts',(16.4057626400288,70.7840574338568,12.5339739358004));
#54495=CARTESIAN_POINT('Ctrl Pts',(16.399077350198,70.7325196459017,12.5841631690511));
#54496=CARTESIAN_POINT('Ctrl Pts',(16.3884990156058,70.6589424000847,12.6690966385489));
#54497=CARTESIAN_POINT('Ctrl Pts',(16.3846650008126,70.6338732437256,12.7010019877807));
#54498=CARTESIAN_POINT('Ctrl Pts',(16.3776251335946,70.5912511671718,12.7609447818084));
#54499=CARTESIAN_POINT('Ctrl Pts',(16.3744382434487,70.5731850605043,12.7885722600957));
#54500=CARTESIAN_POINT('Ctrl Pts',(16.3689156801596,70.5441338948886,12.8370189780933));
#54501=CARTESIAN_POINT('Ctrl Pts',(16.3666003378791,70.5326135603664,12.8574984334671));
#54502=CARTESIAN_POINT('Ctrl Pts',(16.3616129423117,70.5092428383312,12.9018819068115));
#54503=CARTESIAN_POINT('Ctrl Pts',(16.3589362322345,70.4975646688587,12.9258630252757));
#54504=CARTESIAN_POINT('Ctrl Pts',(16.3499637333487,70.4613233356284,13.0066516777853));
#54505=CARTESIAN_POINT('Ctrl Pts',(16.3435637629278,70.4401609084647,13.0648762941052));
#54506=CARTESIAN_POINT('Ctrl Pts',(16.3305192953921,70.4062530715105,13.1847775819259));
#54507=CARTESIAN_POINT('Ctrl Pts',(16.323889959174,70.3936766742012,13.2463360191253));
#54508=CARTESIAN_POINT('Ctrl Pts',(16.314790398906,70.3826056291999,13.3327283247775));
#54509=CARTESIAN_POINT('Ctrl Pts',(16.3122596482475,70.3802052275293,13.3569711872318));
#54510=CARTESIAN_POINT('Ctrl Pts',(16.3077592854686,70.3771496701396,13.4005987307025));
#54511=CARTESIAN_POINT('Ctrl Pts',(16.305781318091,70.3762383182268,13.4199579299138));
#54512=CARTESIAN_POINT('Ctrl Pts',(16.3024702415047,70.3754462288665,13.4527500364809));
#54513=CARTESIAN_POINT('Ctrl Pts',(16.3011265890288,70.375334822483,13.4661722607109));
#54514=CARTESIAN_POINT('Ctrl Pts',(16.2979361231732,70.3755776894921,13.498314059199));
#54515=CARTESIAN_POINT('Ctrl Pts',(16.2960995219557,70.3761329523695,13.5170285701444));
#54516=CARTESIAN_POINT('Ctrl Pts',(16.2878658788132,70.380515568799,13.6015990975334));
#54517=CARTESIAN_POINT('Ctrl Pts',(16.2816652417856,70.3890566987688,13.6671174483649));
#54518=CARTESIAN_POINT('Ctrl Pts',(16.2702951158908,70.413997414888,13.7855615517722));
#54519=CARTESIAN_POINT('Ctrl Pts',(16.2651374889677,70.4288330941904,13.8386405024776));
#54520=CARTESIAN_POINT('Ctrl Pts',(16.2581238708754,70.4532608742622,13.9082400229729));
#54521=CARTESIAN_POINT('Ctrl Pts',(16.2563372939143,70.4598456501824,13.9257530393238));
#54522=CARTESIAN_POINT('Ctrl Pts',(16.2516214080036,70.4781362916253,13.9713173413683));
#54523=CARTESIAN_POINT('Ctrl Pts',(16.2486767319952,70.4904656348527,13.9991029299502));
#54524=CARTESIAN_POINT('Ctrl Pts',(16.2434159765917,70.5139846694955,14.0473577981535));
#54525=CARTESIAN_POINT('Ctrl Pts',(16.2411146758863,70.524764307304,14.0680118269868));
#54526=CARTESIAN_POINT('Ctrl Pts',(16.2359839859797,70.5498299777805,14.1129781865077));
#54527=CARTESIAN_POINT('Ctrl Pts',(16.2331466684602,70.5643695712019,14.1371338078886));
#54528=CARTESIAN_POINT('Ctrl Pts',(16.2243594646087,70.611385522011,14.2096672950747));
#54529=CARTESIAN_POINT('Ctrl Pts',(16.2183306860113,70.6463625582953,14.2562585184042));
#54530=CARTESIAN_POINT('Ctrl Pts',(16.2122439422732,70.6843594233383,14.3002415371503));
#54531=CARTESIAN_POINT('Origin',(21.26284859951,71.6454,13.47));
#54532=CARTESIAN_POINT('',(15.2474530402596,70.6843589428744,14.3002409809922));
#54533=CARTESIAN_POINT('',(15.4172344952204,70.6843589433712,14.3002409815673));
#54534=CARTESIAN_POINT('',(21.26284859951,70.6843589433668,14.3002409815622));
#54535=CARTESIAN_POINT('Ctrl Pts',(15.2474530402596,70.6843589428744,14.3002409809922));
#54536=CARTESIAN_POINT('Ctrl Pts',(15.2478512541151,70.6817427021451,14.2972125653711));
#54537=CARTESIAN_POINT('Ctrl Pts',(15.2482500501357,70.6791407556303,14.2941717597417));
#54538=CARTESIAN_POINT('Ctrl Pts',(15.2515639828624,70.6576700862129,14.2688382842419));
#54539=CARTESIAN_POINT('Ctrl Pts',(15.2545084970404,70.6395632294921,14.2459156060063));
#54540=CARTESIAN_POINT('Ctrl Pts',(15.2647675752268,70.5798883327756,14.164767005487));
#54541=CARTESIAN_POINT('Ctrl Pts',(15.2722210661029,70.5424644562559,14.1036764139342));
#54542=CARTESIAN_POINT('Ctrl Pts',(15.2850536696927,70.4876847424598,13.9945528002066));
#54543=CARTESIAN_POINT('Ctrl Pts',(15.2903883927735,70.4677060149305,13.9480141297845));
#54544=CARTESIAN_POINT('Ctrl Pts',(15.2988584625137,70.4401642786459,13.8715559548569));
#54545=CARTESIAN_POINT('Ctrl Pts',(15.3020291120978,70.430818933401,13.8423353515714));
#54546=CARTESIAN_POINT('Ctrl Pts',(15.3066646878291,70.4185313342746,13.7985023820193));
#54547=CARTESIAN_POINT('Ctrl Pts',(15.3081654726918,70.4147736088042,13.7841326150186));
#54548=CARTESIAN_POINT('Ctrl Pts',(15.3111189513089,70.4078101425326,13.7554577359762));
#54549=CARTESIAN_POINT('Ctrl Pts',(15.3125717072818,70.4045982479306,13.7411565155594));
#54550=CARTESIAN_POINT('Ctrl Pts',(15.3168971783076,70.3957024048684,13.6980713580252));
#54551=CARTESIAN_POINT('Ctrl Pts',(15.319733590595,70.3907669208225,13.6691403883147));
#54552=CARTESIAN_POINT('Ctrl Pts',(15.3308977342618,70.3751450463372,13.5535282360151));
#54553=CARTESIAN_POINT('Ctrl Pts',(15.3389841601027,70.372406978328,13.4660143014262));
#54554=CARTESIAN_POINT('Ctrl Pts',(15.3505276621419,70.381169525788,13.3441648318202));
#54555=CARTESIAN_POINT('Ctrl Pts',(15.3538379834649,70.3850957784489,13.3095441266975));
#54556=CARTESIAN_POINT('Ctrl Pts',(15.3600645033139,70.3950361392639,13.2455279894205));
#54557=CARTESIAN_POINT('Ctrl Pts',(15.3629689659463,70.4006784071798,13.2160998363465));
#54558=CARTESIAN_POINT('Ctrl Pts',(15.368167172403,70.4124967696492,13.1644158835225));
#54559=CARTESIAN_POINT('Ctrl Pts',(15.3704467125983,70.4182495791076,13.1420766845061));
#54560=CARTESIAN_POINT('Ctrl Pts',(15.375579917579,70.4324433682094,13.0925820068369));
#54561=CARTESIAN_POINT('Ctrl Pts',(15.3784423821996,70.4411942683768,13.0655295264295));
#54562=CARTESIAN_POINT('Ctrl Pts',(15.3900456237335,70.4799307391602,12.9582186830499));
#54563=CARTESIAN_POINT('Ctrl Pts',(15.3990059087545,70.5170892740688,12.8808076629618));
#54564=CARTESIAN_POINT('Ctrl Pts',(15.4141202090388,70.5920148030536,12.7582067408705));
#54565=CARTESIAN_POINT('Ctrl Pts',(15.420225737011,70.6256506433206,12.7108012891064));
#54566=CARTESIAN_POINT('Ctrl Pts',(15.4281874274097,70.6746462290135,12.6509089046388));
#54567=CARTESIAN_POINT('Ctrl Pts',(15.4301590415946,70.6872174604953,12.6362377592349));
#54568=CARTESIAN_POINT('Ctrl Pts',(15.4334639646169,70.7090844811646,12.6118663011737));
#54569=CARTESIAN_POINT('Ctrl Pts',(15.4348076826581,70.718207123861,12.6020174942395));
#54570=CARTESIAN_POINT('Ctrl Pts',(15.4380046289984,70.7404678138127,12.5787365104635));
#54571=CARTESIAN_POINT('Ctrl Pts',(15.4398475003202,70.753750767017,12.5654478155695));
#54572=CARTESIAN_POINT('Ctrl Pts',(15.4496880002559,70.8268828966169,12.4954614202003));
#54573=CARTESIAN_POINT('Ctrl Pts',(15.4573700261058,70.8918590770472,12.4443897486525));
#54574=CARTESIAN_POINT('Ctrl Pts',(15.4694247059687,70.9999473436235,12.3752896554734));
#54575=CARTESIAN_POINT('Ctrl Pts',(15.4737400371088,71.0398609455861,12.3527167867678));
#54576=CARTESIAN_POINT('Ctrl Pts',(15.4815072719078,71.1127652144443,12.3165420581704));
#54577=CARTESIAN_POINT('Ctrl Pts',(15.4849323846649,71.1452725270213,12.3020800374201));
#54578=CARTESIAN_POINT('Ctrl Pts',(15.4907231644892,71.2004598791729,12.2802546192861));
#54579=CARTESIAN_POINT('Ctrl Pts',(15.493062773703,71.2228185879646,12.2721308302012));
#54580=CARTESIAN_POINT('Ctrl Pts',(15.497978570993,71.2698262624349,12.2565309076831));
#54581=CARTESIAN_POINT('Ctrl Pts',(15.5005572007895,71.2945006739808,12.2491673780782));
#54582=CARTESIAN_POINT('Ctrl Pts',(15.5083943330171,71.369423309474,12.2292671845683));
#54583=CARTESIAN_POINT('Ctrl Pts',(15.5137203365454,71.4202243477045,12.2190502539735));
#54584=CARTESIAN_POINT('Ctrl Pts',(15.526710103593,71.5437443460363,12.2019758560591));
#54585=CARTESIAN_POINT('Ctrl Pts',(15.5344217127366,71.6167139400239,12.1982314601836));
#54586=CARTESIAN_POINT('Ctrl Pts',(15.5447621526674,71.7154967085733,12.2016711166485));
#54587=CARTESIAN_POINT('Ctrl Pts',(15.5474596662302,71.7413667227091,12.2033657566169));
#54588=CARTESIAN_POINT('Ctrl Pts',(15.5522146077091,71.7872981001534,12.2077900800486));
#54589=CARTESIAN_POINT('Ctrl Pts',(15.5542817443091,71.8073803986679,12.2102097524672));
#54590=CARTESIAN_POINT('Ctrl Pts',(15.5576854938171,71.8407178315876,12.2150370224709));
#54591=CARTESIAN_POINT('Ctrl Pts',(15.5590344441554,71.8540063682806,12.2171773522098));
#54592=CARTESIAN_POINT('Ctrl Pts',(15.5621309792488,71.8846909747798,12.2226214639219));
#54593=CARTESIAN_POINT('Ctrl Pts',(15.5638706558884,71.9020564801243,12.2260783973999));
#54594=CARTESIAN_POINT('Ctrl Pts',(15.5742285588332,72.0058888612285,12.2490155602008));
#54595=CARTESIAN_POINT('Ctrl Pts',(15.582466671416,72.0902089971549,12.2771438233463));
#54596=CARTESIAN_POINT('Ctrl Pts',(15.5954802408073,72.2162159244106,12.3344189248631));
#54597=CARTESIAN_POINT('Ctrl Pts',(15.6001743058787,72.2602548631365,12.3576475888896));
#54598=CARTESIAN_POINT('Ctrl Pts',(15.6079872505939,72.3299841552851,12.3998350997683));
#54599=CARTESIAN_POINT('Ctrl Pts',(15.6110584837034,72.3565246267629,12.4172845775312));
#54600=CARTESIAN_POINT('Ctrl Pts',(15.6164545500316,72.4014270835153,12.4492796772511));
#54601=CARTESIAN_POINT('Ctrl Pts',(15.618761734872,72.4200929868029,12.4633731937572));
#54602=CARTESIAN_POINT('Ctrl Pts',(15.6238070466411,72.4596881563805,12.4950228273709));
#54603=CARTESIAN_POINT('Ctrl Pts',(15.6265512285425,72.4804608920149,12.5127546255014));
#54604=CARTESIAN_POINT('Ctrl Pts',(15.6348171993673,72.5406791838915,12.5676098365466));
#54605=CARTESIAN_POINT('Ctrl Pts',(15.6404106256085,72.5783336638097,12.6065964175463));
#54606=CARTESIAN_POINT('Ctrl Pts',(15.6530625299896,72.656716081412,12.6988832001763));
#54607=CARTESIAN_POINT('Ctrl Pts',(15.6601381860156,72.6959482007232,12.7532507905421));
#54608=CARTESIAN_POINT('Ctrl Pts',(15.6697529225791,72.7437124850371,12.8318492563327));
#54609=CARTESIAN_POINT('Ctrl Pts',(15.6723561459346,72.7560788184445,12.853623939215));
#54610=CARTESIAN_POINT('Ctrl Pts',(15.6769675177142,72.777034369683,12.8932040060956));
#54611=CARTESIAN_POINT('Ctrl Pts',(15.678984601826,72.7858671045772,12.9108712995588));
#54612=CARTESIAN_POINT('Ctrl Pts',(15.6823360845555,72.800010913826,12.94089307122));
#54613=CARTESIAN_POINT('Ctrl Pts',(15.6836818128242,72.8055437755759,12.9531373557262));
#54614=CARTESIAN_POINT('Ctrl Pts',(15.6868097388824,72.8180568776009,12.9820430192726));
#54615=CARTESIAN_POINT('Ctrl Pts',(15.688583219359,72.8248779306584,12.9987695847326));
#54616=CARTESIAN_POINT('Ctrl Pts',(15.6992715270306,72.8641669953806,13.1013187576491));
#54617=CARTESIAN_POINT('Ctrl Pts',(15.7077835988779,72.887617413542,13.1903203566669));
#54618=CARTESIAN_POINT('Ctrl Pts',(15.7205891076685,72.9078627850662,13.3249083827248));
#54619=CARTESIAN_POINT('Ctrl Pts',(15.7247755731598,72.9121559945579,13.3690420230747));
#54620=CARTESIAN_POINT('Ctrl Pts',(15.7321243262165,72.9155808947046,13.445687367422));
#54621=CARTESIAN_POINT('Ctrl Pts',(15.7352566549272,72.9157875237194,13.4781083081998));
#54622=CARTESIAN_POINT('Ctrl Pts',(15.7407194217992,72.9140065458678,13.5339296518394));
#54623=CARTESIAN_POINT('Ctrl Pts',(15.7430308052484,72.9126104268437,13.5573334094022));
#54624=CARTESIAN_POINT('Ctrl Pts',(15.7480440714304,72.9082182599346,13.6075381604161));
#54625=CARTESIAN_POINT('Ctrl Pts',(15.750751244167,72.9050146563437,13.634308681989));
#54626=CARTESIAN_POINT('Ctrl Pts',(15.7635593044991,72.8860222649612,13.7591872298019));
#54627=CARTESIAN_POINT('Ctrl Pts',(15.7739803759795,72.8596089083683,13.8553055344059));
#54628=CARTESIAN_POINT('Ctrl Pts',(15.7901226486762,72.8019071013486,13.9975693883632));
#54629=CARTESIAN_POINT('Ctrl Pts',(15.7958041458861,72.7783362795895,14.0464503822243));
#54630=CARTESIAN_POINT('Ctrl Pts',(15.8030951858812,72.7433755361682,14.1084651652291));
#54631=CARTESIAN_POINT('Ctrl Pts',(15.8048198843547,72.7347445475935,14.1230823900889));
#54632=CARTESIAN_POINT('Ctrl Pts',(15.8078959918652,72.7186684103895,14.1491024742073));
#54633=CARTESIAN_POINT('Ctrl Pts',(15.8092526620489,72.7113292292146,14.1605651080059));
#54634=CARTESIAN_POINT('Ctrl Pts',(15.8127696617139,72.6916695098266,14.1902099131262));
#54635=CARTESIAN_POINT('Ctrl Pts',(15.8149124090466,72.6790590824631,14.2081946325573));
#54636=CARTESIAN_POINT('Ctrl Pts',(15.8261845652096,72.609640658552,14.30192753067));
#54637=CARTESIAN_POINT('Ctrl Pts',(15.834938780409,72.544955901381,14.371480780459));
#54638=CARTESIAN_POINT('Ctrl Pts',(15.8473553903786,72.4451342709734,14.457262780635));
#54639=CARTESIAN_POINT('Ctrl Pts',(15.8508564136436,72.4161036794485,14.4800881829059));
#54640=CARTESIAN_POINT('Ctrl Pts',(15.8573817139584,72.3608632699526,14.5197520035265));
#54641=CARTESIAN_POINT('Ctrl Pts',(15.8603917794223,72.3349491295754,14.5369529481081));
#54642=CARTESIAN_POINT('Ctrl Pts',(15.8657220426888,72.288526544451,14.5653688662634));
#54643=CARTESIAN_POINT('Ctrl Pts',(15.8680259876459,72.2682903674222,14.5770014086535));
#54644=CARTESIAN_POINT('Ctrl Pts',(15.8731094775948,72.2233541058685,14.6012103032845));
#54645=CARTESIAN_POINT('Ctrl Pts',(15.8758959322651,72.1985404097865,14.6135484619975));
#54646=CARTESIAN_POINT('Ctrl Pts',(15.8881195547797,72.0890749083297,14.6635818836657));
#54647=CARTESIAN_POINT('Ctrl Pts',(15.8978248720789,72.0008601499585,14.6927533269636));
#54648=CARTESIAN_POINT('Ctrl Pts',(15.9136849533829,71.8533891361559,14.7242027223829));
#54649=CARTESIAN_POINT('Ctrl Pts',(15.9197922923734,71.7957229682606,14.73241382832));
#54650=CARTESIAN_POINT('Ctrl Pts',(15.9275069415758,71.7206197978507,14.737886008838));
#54651=CARTESIAN_POINT('Ctrl Pts',(15.929246800121,71.7035242756897,14.7387847045918));
#54652=CARTESIAN_POINT('Ctrl Pts',(15.9323352071073,71.6728402161795,14.7397761541977));
#54653=CARTESIAN_POINT('Ctrl Pts',(15.9336893449234,71.6592606999698,14.7399969953444));
#54654=CARTESIAN_POINT('Ctrl Pts',(15.9371770049191,71.6239961993076,14.7400047172771));
#54655=CARTESIAN_POINT('Ctrl Pts',(15.9392935850993,71.6023154015255,14.73945422267));
#54656=CARTESIAN_POINT('Ctrl Pts',(15.9428438068594,71.5656439317579,14.73758232507));
#54657=CARTESIAN_POINT('Ctrl Pts',(15.9442874294977,71.5506447699087,14.736549437199));
#54658=CARTESIAN_POINT('Ctrl Pts',(15.950620318836,71.4846089808678,14.7308222499309));
#54659=CARTESIAN_POINT('Ctrl Pts',(15.9554280594632,71.4338619219898,14.7233072209986));
#54660=CARTESIAN_POINT('Ctrl Pts',(15.966867913353,71.3146601021156,14.6982058486337));
#54661=CARTESIAN_POINT('Ctrl Pts',(15.9734893848709,71.2469560046675,14.6779399789805));
#54662=CARTESIAN_POINT('Ctrl Pts',(15.9830880599361,71.1541057150504,14.6414874404991));
#54663=CARTESIAN_POINT('Ctrl Pts',(15.9859226685923,71.127300108516,14.629881498222));
#54664=CARTESIAN_POINT('Ctrl Pts',(15.9910716177074,71.0798965434959,14.6073862101299));
#54665=CARTESIAN_POINT('Ctrl Pts',(15.9933736711862,71.059152485979,14.5968341608947));
#54666=CARTESIAN_POINT('Ctrl Pts',(15.9986131555517,71.0130286892704,14.5717536797824));
#54667=CARTESIAN_POINT('Ctrl Pts',(16.0015606541105,70.9878384618905,14.5569071339245));
#54668=CARTESIAN_POINT('Ctrl Pts',(16.0079535052726,70.9348981434087,14.523191253929));
#54669=CARTESIAN_POINT('Ctrl Pts',(16.0114058355853,70.9073387644444,14.5040647270978));
#54670=CARTESIAN_POINT('Ctrl Pts',(16.0229877539323,70.8182938882145,14.4368924574447));
#54671=CARTESIAN_POINT('Ctrl Pts',(16.0312357930627,70.7604807604503,14.3842766089763));
#54672=CARTESIAN_POINT('Ctrl Pts',(16.0406373207261,70.6999070861735,14.3179872322856));
#54673=CARTESIAN_POINT('Ctrl Pts',(16.041869838494,70.6920707520904,14.3091677450839));
#54674=CARTESIAN_POINT('Ctrl Pts',(16.0430985027246,70.6843589375946,14.3002409748806));
#54675=CARTESIAN_POINT('Ctrl Pts',(16.2122439422732,70.6843594233383,14.3002415371503));
#54676=CARTESIAN_POINT('Ctrl Pts',(16.2069536758919,70.7173842304241,14.3384691832336));
#54677=CARTESIAN_POINT('Ctrl Pts',(16.2016207101553,70.7526902012096,14.3747267551267));
#54678=CARTESIAN_POINT('Ctrl Pts',(16.1931820657435,70.8121650122961,14.4289109947777));
#54679=CARTESIAN_POINT('Ctrl Pts',(16.1900649309448,70.8349319996618,14.4482293885376));
#54680=CARTESIAN_POINT('Ctrl Pts',(16.1846813895207,70.8758144275889,14.4805110798706));
#54681=CARTESIAN_POINT('Ctrl Pts',(16.1824016250686,70.893629460446,14.4938339024359));
#54682=CARTESIAN_POINT('Ctrl Pts',(16.1787681662706,70.9229201699043,14.5145615872622));
#54683=CARTESIAN_POINT('Ctrl Pts',(16.1773978628202,70.9341803566216,14.5222607668843));
#54684=CARTESIAN_POINT('Ctrl Pts',(16.1743640415744,70.9596058599809,14.5390507694005));
#54685=CARTESIAN_POINT('Ctrl Pts',(16.1727063310864,70.9738317668644,14.5480442309101));
#54686=CARTESIAN_POINT('Ctrl Pts',(16.1664281650735,71.0288412626854,14.5813088201462));
#54687=CARTESIAN_POINT('Ctrl Pts',(16.1619102065471,71.0707998866339,14.6035731467499));
#54688=CARTESIAN_POINT('Ctrl Pts',(16.1508501650601,71.1771769448403,14.6525900885648));
#54689=CARTESIAN_POINT('Ctrl Pts',(16.1443641666752,71.2427313411019,14.6764866760144));
#54690=CARTESIAN_POINT('Ctrl Pts',(16.1347186985584,71.3409310256024,14.7033826840723));
#54691=CARTESIAN_POINT('Ctrl Pts',(16.1316529651547,71.3722566348716,14.7106960113178));
#54692=CARTESIAN_POINT('Ctrl Pts',(16.1258136010689,71.4317554096505,14.7222242037693));
#54693=CARTESIAN_POINT('Ctrl Pts',(16.1230487883803,71.4598583785599,14.7266954619482));
#54694=CARTESIAN_POINT('Ctrl Pts',(16.117967926395,71.5111879972875,14.7331029997539));
#54695=CARTESIAN_POINT('Ctrl Pts',(16.1156625851046,71.5343635911352,14.7353508558387));
#54696=CARTESIAN_POINT('Ctrl Pts',(16.1103865756748,71.587054319568,14.7390028893651));
#54697=CARTESIAN_POINT('Ctrl Pts',(16.1074052385265,71.6165816385375,14.7400164141687));
#54698=CARTESIAN_POINT('Ctrl Pts',(16.096514243595,71.7233954818661,14.7399563214959));
#54699=CARTESIAN_POINT('Ctrl Pts',(16.0884386510695,71.800496625268,14.7328590556421));
#54700=CARTESIAN_POINT('Ctrl Pts',(16.0736029800222,71.9391978527656,14.7071958721665));
#54701=CARTESIAN_POINT('Ctrl Pts',(16.0668825316892,72.0009784490667,14.6908752944312));
#54702=CARTESIAN_POINT('Ctrl Pts',(16.0583969433781,72.0789827105932,14.6638413676742));
#54703=CARTESIAN_POINT('Ctrl Pts',(16.056486011671,72.0965529886664,14.6573130568684));
#54704=CARTESIAN_POINT('Ctrl Pts',(16.0532419800624,72.1264484728621,14.6454456608615));
#54705=CARTESIAN_POINT('Ctrl Pts',(16.0518997015855,72.1388435905834,14.6402963792231));
#54706=CARTESIAN_POINT('Ctrl Pts',(16.0486491853745,72.1689090608831,14.6272436233034));
#54707=CARTESIAN_POINT('Ctrl Pts',(16.0467525976929,72.1864846085862,14.6191310358496));
#54708=CARTESIAN_POINT('Ctrl Pts',(16.04251232184,72.2257049395534,14.5999279883125));
#54709=CARTESIAN_POINT('Ctrl Pts',(16.0401793972825,72.2472307702321,14.5886111988781));
#54710=CARTESIAN_POINT('Ctrl Pts',(16.031910923693,72.3228748070702,14.5460264729737));
#54711=CARTESIAN_POINT('Ctrl Pts',(16.026078203658,72.374995959972,14.5113913035721));
#54712=CARTESIAN_POINT('Ctrl Pts',(16.0143505754315,72.4734894476723,14.4349028563842));
#54713=CARTESIAN_POINT('Ctrl Pts',(16.0084716325567,72.5197442915997,14.3931954999564));
#54714=CARTESIAN_POINT('Ctrl Pts',(15.9998795016945,72.5811989265552,14.3290062797088));
#54715=CARTESIAN_POINT('Ctrl Pts',(15.9972789894971,72.599031128145,14.3091655647484));
#54716=CARTESIAN_POINT('Ctrl Pts',(15.9923387811045,72.6313710283327,14.2708202725509));
#54717=CARTESIAN_POINT('Ctrl Pts',(15.9900058976087,72.6460153389615,14.2524453577068));
#54718=CARTESIAN_POINT('Ctrl Pts',(15.9843475054561,72.6799807927779,14.2073135164107));
#54719=CARTESIAN_POINT('Ctrl Pts',(15.9810042043377,72.6987837460787,14.1801906965875));
#54720=CARTESIAN_POINT('Ctrl Pts',(15.9734715810184,72.7382917441383,14.1181754634069));
#54721=CARTESIAN_POINT('Ctrl Pts',(15.9692677647825,72.7584234083624,14.0829616390773));
#54722=CARTESIAN_POINT('Ctrl Pts',(15.9575253866954,72.8094485285397,13.982880744287));
#54723=CARTESIAN_POINT('Ctrl Pts',(15.9499288974573,72.8365777569735,13.9162633524045));
#54724=CARTESIAN_POINT('Ctrl Pts',(15.9392337000661,72.8670866522122,13.8183233624603));
#54725=CARTESIAN_POINT('Ctrl Pts',(15.9360495874178,72.8751708051521,13.7886089442862));
#54726=CARTESIAN_POINT('Ctrl Pts',(15.9313815895581,72.8855829108748,13.7439929858682));
#54727=CARTESIAN_POINT('Ctrl Pts',(15.9298621260338,72.8887383173865,13.7292985076369));
#54728=CARTESIAN_POINT('Ctrl Pts',(15.9269054575026,72.8944236724162,13.7003258349149));
#54729=CARTESIAN_POINT('Ctrl Pts',(15.9254676845174,72.8969714053757,13.6860537010658));
#54730=CARTESIAN_POINT('Ctrl Pts',(15.9212586446076,72.9037675530326,13.6438136216966));
#54731=CARTESIAN_POINT('Ctrl Pts',(15.9185207440167,72.9073270648636,13.615741389039));
#54732=CARTESIAN_POINT('Ctrl Pts',(15.9116099942222,72.9140046563963,13.5439194899895));
#54733=CARTESIAN_POINT('Ctrl Pts',(15.9074798185523,72.9158005284265,13.5000838619579));
#54734=CARTESIAN_POINT('Ctrl Pts',(15.8955138427457,72.914421096906,13.3727779359948));
#54735=CARTESIAN_POINT('Ctrl Pts',(15.8877198970543,72.9052916300286,13.2896187949757));
#54736=CARTESIAN_POINT('Ctrl Pts',(15.876924827781,72.8821678164368,13.1799577962869));
#54737=CARTESIAN_POINT('Ctrl Pts',(15.8741443679683,72.8753182796234,13.1521638116845));
#54738=CARTESIAN_POINT('Ctrl Pts',(15.8690486463106,72.8612067654419,13.1022287846414));
#54739=CARTESIAN_POINT('Ctrl Pts',(15.8667444498011,72.8542630004628,13.0800104784567));
#54740=CARTESIAN_POINT('Ctrl Pts',(15.8614387727845,72.8370282514575,13.0297575796099));
#54741=CARTESIAN_POINT('Ctrl Pts',(15.8584259556878,72.826351520773,13.0018713737063));
#54742=CARTESIAN_POINT('Ctrl Pts',(15.8518498003061,72.8011824038681,12.9424893326376));
#54743=CARTESIAN_POINT('Ctrl Pts',(15.8482784182537,72.7863630186745,12.9111589108167));
#54744=CARTESIAN_POINT('Ctrl Pts',(15.8357440536633,72.7304007268286,12.8043759948167));
#54745=CARTESIAN_POINT('Ctrl Pts',(15.8266382249414,72.6829025171005,12.7325253309429));
#54746=CARTESIAN_POINT('Ctrl Pts',(15.8144982442271,72.6091601381511,12.6423518862821));
#54747=CARTESIAN_POINT('Ctrl Pts',(15.811336815638,72.5889517742661,12.61938522073));
#54748=CARTESIAN_POINT('Ctrl Pts',(15.8067116875847,72.5577346553901,12.5863905802694));
#54749=CARTESIAN_POINT('Ctrl Pts',(15.8052123499448,72.5473488152746,12.5757916679543));
#54750=CARTESIAN_POINT('Ctrl Pts',(15.8022596002214,72.5263344873181,12.5550850193422));
#54751=CARTESIAN_POINT('Ctrl Pts',(15.8008061580451,72.5157119719336,12.5449745222973));
#54752=CARTESIAN_POINT('Ctrl Pts',(15.7964740187286,72.4832732991461,12.5151531012146));
#54753=CARTESIAN_POINT('Ctrl Pts',(15.7936318032601,72.4609436491529,12.4960116745226));
#54754=CARTESIAN_POINT('Ctrl Pts',(15.7863309763494,72.4013272670519,12.4483969576202));
#54755=CARTESIAN_POINT('Ctrl Pts',(15.7819214878312,72.3630918888059,12.4211826119618));
#54756=CARTESIAN_POINT('Ctrl Pts',(15.7702293480454,72.2578480723481,12.3547313890348));
#54757=CARTESIAN_POINT('Ctrl Pts',(15.7629705486992,72.1886124456067,12.3194197956234));
#54758=CARTESIAN_POINT('Ctrl Pts',(15.7527109809555,72.089632020526,12.2798735726927));
#54759=CARTESIAN_POINT('Ctrl Pts',(15.7498921373544,72.0623110116881,12.2700300404668));
#54760=CARTESIAN_POINT('Ctrl Pts',(15.7447592194768,72.0125317692914,12.254000150787));
#54761=CARTESIAN_POINT('Ctrl Pts',(15.7424570827514,71.9901945073682,12.247478858865));
#54762=CARTESIAN_POINT('Ctrl Pts',(15.7372008795558,71.9392595700194,12.2341154449411));
#54763=CARTESIAN_POINT('Ctrl Pts',(15.7342364096056,71.9105793352779,12.2276459266755));
#54764=CARTESIAN_POINT('Ctrl Pts',(15.727795894836,71.8484684323509,12.215883823091));
#54765=CARTESIAN_POINT('Ctrl Pts',(15.7243125973126,71.8149989349126,12.2109210085884));
#54766=CARTESIAN_POINT('Ctrl Pts',(15.7124938778567,71.7018717016388,12.1987388322188));
#54767=CARTESIAN_POINT('Ctrl Pts',(15.704034031141,71.6217408758815,12.1977058039898));
#54768=CARTESIAN_POINT('Ctrl Pts',(15.6920231010298,71.507286949311,12.2070504313153));
#54769=CARTESIAN_POINT('Ctrl Pts',(15.6884002605089,71.4726469703922,12.2113206116902));
#54770=CARTESIAN_POINT('Ctrl Pts',(15.6831916643632,71.4223621283758,12.2196350330034));
#54771=CARTESIAN_POINT('Ctrl Pts',(15.6815613857106,71.4065510959083,12.2225587240702));
#54772=CARTESIAN_POINT('Ctrl Pts',(15.6785537789849,71.3772018334364,12.2285643984775));
#54773=CARTESIAN_POINT('Ctrl Pts',(15.6771732832589,71.3636523235524,12.2315691810899));
#54774=CARTESIAN_POINT('Ctrl Pts',(15.6734255340765,71.3267125564333,12.2403987821823));
#54775=CARTESIAN_POINT('Ctrl Pts',(15.6710809334944,71.3034337737362,12.2466683992065));
#54776=CARTESIAN_POINT('Ctrl Pts',(15.6619757980103,71.2128953905287,12.2738399089759));
#54777=CARTESIAN_POINT('Ctrl Pts',(15.6553982928698,71.1472379037731,12.2996598077427));
#54778=CARTESIAN_POINT('Ctrl Pts',(15.6428589077792,71.0275115229793,12.358655297591));
#54779=CARTESIAN_POINT('Ctrl Pts',(15.6369227566369,70.9731292604227,12.3906836947697));
#54780=CARTESIAN_POINT('Ctrl Pts',(15.6280770332459,70.8976512919767,12.4430607623033));
#54781=CARTESIAN_POINT('Ctrl Pts',(15.6252752727666,70.8745187034793,12.4603099216606));
#54782=CARTESIAN_POINT('Ctrl Pts',(15.6201590351721,70.8338252883133,12.4928674735473));
#54783=CARTESIAN_POINT('Ctrl Pts',(15.6178561081095,70.8160597266575,12.5079002020276));
#54784=CARTESIAN_POINT('Ctrl Pts',(15.6125786702471,70.7766613346707,12.5431403092564));
#54785=CARTESIAN_POINT('Ctrl Pts',(15.6095933534295,70.7553029696858,12.5636321565306));
#54786=CARTESIAN_POINT('Ctrl Pts',(15.603094464543,70.7108599706198,12.6093588770371));
#54787=CARTESIAN_POINT('Ctrl Pts',(15.5995733028404,70.6880399560309,12.6348176994625));
#54788=CARTESIAN_POINT('Ctrl Pts',(15.5874557765618,70.6137731297783,12.7247201212873));
#54789=CARTESIAN_POINT('Ctrl Pts',(15.5787272068727,70.5675845670795,12.7932368813912));
#54790=CARTESIAN_POINT('Ctrl Pts',(15.5667196782044,70.5128855554526,12.8943529511359));
#54791=CARTESIAN_POINT('Ctrl Pts',(15.5633465106992,70.4985091748802,12.923556565982));
#54792=CARTESIAN_POINT('Ctrl Pts',(15.5584194238919,70.4788742384884,12.9676408893398));
#54793=CARTESIAN_POINT('Ctrl Pts',(15.5568270297503,70.4727460091658,12.982117089778));
#54794=CARTESIAN_POINT('Ctrl Pts',(15.5538413186338,70.4616540380434,13.0097362582877));
#54795=CARTESIAN_POINT('Ctrl Pts',(15.5524457112825,70.456637105262,13.0228534524509));
#54796=CARTESIAN_POINT('Ctrl Pts',(15.5485710456865,70.4432076268704,13.0597909325706));
#54797=CARTESIAN_POINT('Ctrl Pts',(15.5461174907474,70.4352861821186,13.0837839645116));
#54798=CARTESIAN_POINT('Ctrl Pts',(15.5367756251387,70.4075969807519,13.176895814171));
#54799=CARTESIAN_POINT('Ctrl Pts',(15.5300703702451,70.3929925450788,13.2474144590393));
#54800=CARTESIAN_POINT('Ctrl Pts',(15.5176505444871,70.377259326907,13.3786227701155));
#54801=CARTESIAN_POINT('Ctrl Pts',(15.5119681015055,70.3743530396791,13.438875722459));
#54802=CARTESIAN_POINT('Ctrl Pts',(15.5034086926108,70.3763893068207,13.5277146557221));
#54803=CARTESIAN_POINT('Ctrl Pts',(15.5006282171801,70.3780120894559,13.5562943250599));
#54804=CARTESIAN_POINT('Ctrl Pts',(15.4955324715968,70.3827023879678,13.6079728310771));
#54805=CARTESIAN_POINT('Ctrl Pts',(15.4932282669454,70.3854429042861,13.6310891106407));
#54806=CARTESIAN_POINT('Ctrl Pts',(15.4879225741783,70.3931447677185,13.6836541974094));
#54807=CARTESIAN_POINT('Ctrl Pts',(15.4849097495037,70.3985125680241,13.7130280675454));
#54808=CARTESIAN_POINT('Ctrl Pts',(15.4783335782917,70.4123351546843,13.7760254271594));
#54809=CARTESIAN_POINT('Ctrl Pts',(15.4747621879987,70.4211417787942,13.8095464420371));
#54810=CARTESIAN_POINT('Ctrl Pts',(15.462227782131,70.4565179797245,13.9247982961317));
#54811=CARTESIAN_POINT('Ctrl Pts',(15.4531219198104,70.4899967856893,14.0041571189042));
#54812=CARTESIAN_POINT('Ctrl Pts',(15.4409819341652,70.5459036781837,14.1063511827171));
#54813=CARTESIAN_POINT('Ctrl Pts',(15.4378205312029,70.5615449875661,14.1326414949653));
#54814=CARTESIAN_POINT('Ctrl Pts',(15.4331954302685,70.586163708468,14.170812819673));
#54815=CARTESIAN_POINT('Ctrl Pts',(15.4316960947869,70.5944238694899,14.183140504408));
#54816=CARTESIAN_POINT('Ctrl Pts',(15.4287433527419,70.6112729861074,14.2073576543103));
#54817=CARTESIAN_POINT('Ctrl Pts',(15.4272899160967,70.6198555624758,14.2192487357362));
#54818=CARTESIAN_POINT('Ctrl Pts',(15.4229577860276,70.6462585003573,14.2545256703274));
#54819=CARTESIAN_POINT('Ctrl Pts',(15.4201155744588,70.6646883045403,14.2774461408655));
#54820=CARTESIAN_POINT('Ctrl Pts',(15.4172793358864,70.6840526097242,14.299886287465));
#54821=CARTESIAN_POINT('Ctrl Pts',(15.4172569145787,70.684205752265,14.3000636560126));
#54822=CARTESIAN_POINT('Ctrl Pts',(15.4172344952204,70.6843589433712,14.3002409815672));
#54823=CARTESIAN_POINT('Origin',(21.26284859951,71.6454,13.47));
#54824=CARTESIAN_POINT('',(14.4555370852546,70.6843589127286,14.3002409460971));
#54825=CARTESIAN_POINT('',(14.625502981677,70.6843589433681,14.3002409815636));
#54826=CARTESIAN_POINT('',(21.26284859951,70.6843589433668,14.3002409815622));
#54827=CARTESIAN_POINT('',(15.1394311199487,71.6444811469566,14.7399994594157));
#54828=CARTESIAN_POINT('Ctrl Pts',(14.4555370852546,70.6843589127286,14.3002409460971));
#54829=CARTESIAN_POINT('Ctrl Pts',(14.4623859954626,70.6371020472158,14.2455390073082));
#54830=CARTESIAN_POINT('Ctrl Pts',(14.4691094373412,70.5945863966558,14.1868844469984));
#54831=CARTESIAN_POINT('Ctrl Pts',(14.4791850657878,70.5396106440812,14.0955433899042));
#54832=CARTESIAN_POINT('Ctrl Pts',(14.4824433690888,70.5231342982942,14.0654779376296));
#54833=CARTESIAN_POINT('Ctrl Pts',(14.4885836748825,70.4947294907501,14.0082692683133));
#54834=CARTESIAN_POINT('Ctrl Pts',(14.491454478698,70.4824964662219,13.981303701591));
#54835=CARTESIAN_POINT('Ctrl Pts',(14.4966272647768,70.4623951160937,13.9325316271323));
#54836=CARTESIAN_POINT('Ctrl Pts',(14.4989158873162,70.4541603647051,13.9108900299642));
#54837=CARTESIAN_POINT('Ctrl Pts',(14.5040674383531,70.4371152865573,13.8621235595589));
#54838=CARTESIAN_POINT('Ctrl Pts',(14.5069392300526,70.428618261718,13.8349036962588));
#54839=CARTESIAN_POINT('Ctrl Pts',(14.5196627816136,70.395393565045,13.7143465831408));
#54840=CARTESIAN_POINT('Ctrl Pts',(14.5298064666729,70.3804448576273,13.618666643329));
#54841=CARTESIAN_POINT('Ctrl Pts',(14.5454537646757,70.3743247183194,13.4700151286904));
#54842=CARTESIAN_POINT('Ctrl Pts',(14.5509313223629,70.3754007001904,13.4176973733095));
#54843=CARTESIAN_POINT('Ctrl Pts',(14.5580345509482,70.3811000639259,13.3486081815444));
#54844=CARTESIAN_POINT('Ctrl Pts',(14.5597667491123,70.3828425463694,13.3316559140685));
#54845=CARTESIAN_POINT('Ctrl Pts',(14.5628437800497,70.3865813785695,13.3013018515283));
#54846=CARTESIAN_POINT('Ctrl Pts',(14.5641941507816,70.388451646137,13.287889425704));
#54847=CARTESIAN_POINT('Ctrl Pts',(14.5676665389007,70.3938554964315,13.2532022095279));
#54848=CARTESIAN_POINT('Ctrl Pts',(14.5697718242952,70.3977169838792,13.2319827395152));
#54849=CARTESIAN_POINT('Ctrl Pts',(14.5789568529845,70.4170965148864,13.139001595652));
#54850=CARTESIAN_POINT('Ctrl Pts',(14.5858149806443,70.4382810627897,13.0685571753205));
#54851=CARTESIAN_POINT('Ctrl Pts',(14.5987647869399,70.489264576998,12.9404702473549));
#54852=CARTESIAN_POINT('Ctrl Pts',(14.6048281180988,70.5176084360242,12.8825177248292));
#54853=CARTESIAN_POINT('Ctrl Pts',(14.6138195994487,70.5648991836087,12.8019744274072));
#54854=CARTESIAN_POINT('Ctrl Pts',(14.6166341133883,70.5804253819109,12.7774908386727));
#54855=CARTESIAN_POINT('Ctrl Pts',(14.6217672516889,70.6099251429435,12.7343130504535));
#54856=CARTESIAN_POINT('Ctrl Pts',(14.6240741211823,70.6236026045024,12.7154316647374));
#54857=CARTESIAN_POINT('Ctrl Pts',(14.6293539044472,70.6557964403548,12.6734701664474));
#54858=CARTESIAN_POINT('Ctrl Pts',(14.632337502544,70.6746145473083,12.6506403578733));
#54859=CARTESIAN_POINT('Ctrl Pts',(14.6388303449703,70.7168336807592,12.6029185013257));
#54860=CARTESIAN_POINT('Ctrl Pts',(14.6423471070369,70.7404764771294,12.5782720847042));
#54861=CARTESIAN_POINT('Ctrl Pts',(14.6544366052751,70.8243509191185,12.4976110567644));
#54862=CARTESIAN_POINT('Ctrl Pts',(14.663140400138,70.8890154553614,12.4465047058285));
#54863=CARTESIAN_POINT('Ctrl Pts',(14.6751219747651,70.9855045620111,12.3844146510052));
#54864=CARTESIAN_POINT('Ctrl Pts',(14.6784929690035,71.0135207757879,12.3678717488517));
#54865=CARTESIAN_POINT('Ctrl Pts',(14.6834195067839,71.0559896318912,12.3449475739994));
#54866=CARTESIAN_POINT('Ctrl Pts',(14.6850133449625,71.0699737924309,12.3377313432969));
#54867=CARTESIAN_POINT('Ctrl Pts',(14.688004649971,71.0967255854598,12.3245503875933));
#54868=CARTESIAN_POINT('Ctrl Pts',(14.6894043515429,71.1094638380836,12.3185353245126));
#54869=CARTESIAN_POINT('Ctrl Pts',(14.6933023674832,71.1454990476914,12.3022469747278));
#54870=CARTESIAN_POINT('Ctrl Pts',(14.6957747299264,71.169009672123,12.2924599163341));
#54871=CARTESIAN_POINT('Ctrl Pts',(14.705389226784,71.2624437855811,12.2568222720668));
#54872=CARTESIAN_POINT('Ctrl Pts',(14.7123344283293,71.334297335484,12.2364387673053));
#54873=CARTESIAN_POINT('Ctrl Pts',(14.7252861341219,71.4695970539378,12.2106408197926));
#54874=CARTESIAN_POINT('Ctrl Pts',(14.7312551922974,71.5324508028325,12.2034563342344));
#54875=CARTESIAN_POINT('Ctrl Pts',(14.7399439019398,71.6222436711666,12.1999306001911));
#54876=CARTESIAN_POINT('Ctrl Pts',(14.7425464224137,71.6489396660501,12.1997245494217));
#54877=CARTESIAN_POINT('Ctrl Pts',(14.7474900203272,71.6991209173944,12.2009189688201));
#54878=CARTESIAN_POINT('Ctrl Pts',(14.7498242687672,71.7225995988123,12.2021306695582));
#54879=CARTESIAN_POINT('Ctrl Pts',(14.7554856085747,71.7789348195803,12.2066085052873));
#54880=CARTESIAN_POINT('Ctrl Pts',(14.7588304984984,71.8117218740769,12.2105055957614));
#54881=CARTESIAN_POINT('Ctrl Pts',(14.7663664006841,71.8843745344286,12.2220271704995));
#54882=CARTESIAN_POINT('Ctrl Pts',(14.7705719091205,71.9241007175369,12.2302943078007));
#54883=CARTESIAN_POINT('Ctrl Pts',(14.7823181606159,72.0328925240294,12.2584275713604));
#54884=CARTESIAN_POINT('Ctrl Pts',(14.7899168574425,72.1007733730978,12.2822739837804));
#54885=CARTESIAN_POINT('Ctrl Pts',(14.8006174980588,72.1943734917263,12.3243659614619));
#54886=CARTESIAN_POINT('Ctrl Pts',(14.8038047871038,72.2220071058663,12.3380221101555));
#54887=CARTESIAN_POINT('Ctrl Pts',(14.8084766631513,72.2623464789848,12.3598184524329));
#54888=CARTESIAN_POINT('Ctrl Pts',(14.8099969046158,72.275446563061,12.3672001841706));
#54889=CARTESIAN_POINT('Ctrl Pts',(14.8129535390303,72.30090674186,12.3821485423193));
#54890=CARTESIAN_POINT('Ctrl Pts',(14.8143905197065,72.3132743516951,12.3896973607616));
#54891=CARTESIAN_POINT('Ctrl Pts',(14.8185950123231,72.349365970552,12.4125834350591));
#54892=CARTESIAN_POINT('Ctrl Pts',(14.8213292413831,72.3727126730733,12.428503696659));
#54893=CARTESIAN_POINT('Ctrl Pts',(14.8282269812653,72.4308072017112,12.4710261585479));
#54894=CARTESIAN_POINT('Ctrl Pts',(14.832347991805,72.4647477257508,12.4986693730336));
#54895=CARTESIAN_POINT('Ctrl Pts',(14.8443238389772,72.559257798012,12.5841304456661));
#54896=CARTESIAN_POINT('Ctrl Pts',(14.8521360561802,72.6156139081804,12.6462381828907));
#54897=CARTESIAN_POINT('Ctrl Pts',(14.8629486455118,72.6824861333793,12.7363992199886));
#54898=CARTESIAN_POINT('Ctrl Pts',(14.8657268142804,72.6987394144301,12.759934132309));
#54899=CARTESIAN_POINT('Ctrl Pts',(14.8708193040879,72.7267508801369,12.8035755116529));
#54900=CARTESIAN_POINT('Ctrl Pts',(14.8731225895676,72.738776961114,12.8234955771858));
#54901=CARTESIAN_POINT('Ctrl Pts',(14.8784270980967,72.7649688135127,12.8697027490863));
#54902=CARTESIAN_POINT('Ctrl Pts',(14.8814396754385,72.7787674898374,12.8961804488411));
#54903=CARTESIAN_POINT('Ctrl Pts',(14.8880155927676,72.8065390222253,12.9543871652908));
#54904=CARTESIAN_POINT('Ctrl Pts',(14.8915869870584,72.8201711365309,12.9862514037533));
#54905=CARTESIAN_POINT('Ctrl Pts',(14.9041216913923,72.8630187619736,13.0989386431305));
#54906=CARTESIAN_POINT('Ctrl Pts',(14.9132279746881,72.8853243854313,13.1821320421558));
#54907=CARTESIAN_POINT('Ctrl Pts',(14.9253711114549,72.90395367473,13.2971442475199));
#54908=CARTESIAN_POINT('Ctrl Pts',(14.9285351549297,72.907753836088,13.327522961839));
#54909=CARTESIAN_POINT('Ctrl Pts',(14.933162831648,72.9117611847237,13.372791591261));
#54910=CARTESIAN_POINT('Ctrl Pts',(14.9346621914832,72.9128104976783,13.3875934970797));
#54911=CARTESIAN_POINT('Ctrl Pts',(14.9376146228393,72.9143803639284,13.4170498272747));
#54912=CARTESIAN_POINT('Ctrl Pts',(14.9390677357706,72.9149070651269,13.43170160893));
#54913=CARTESIAN_POINT('Ctrl Pts',(14.9433957740632,72.9157264578889,13.4757145920993));
#54914=CARTESIAN_POINT('Ctrl Pts',(14.9462343331721,72.9152549560158,13.5050826407288));
#54915=CARTESIAN_POINT('Ctrl Pts',(14.953520749945,72.9113931473839,13.5811278212527));
#54916=CARTESIAN_POINT('Ctrl Pts',(14.9579197400882,72.9064413720226,13.6276814781811));
#54917=CARTESIAN_POINT('Ctrl Pts',(14.9696215869441,72.8864458116629,13.7506342367532));
#54918=CARTESIAN_POINT('Ctrl Pts',(14.9769000523872,72.8669349702154,13.8260904959691));
#54919=CARTESIAN_POINT('Ctrl Pts',(14.9871802758568,72.8308345331101,13.9266045876419));
#54920=CARTESIAN_POINT('Ctrl Pts',(14.9899988142451,72.8200886645546,13.9535793809008));
#54921=CARTESIAN_POINT('Ctrl Pts',(14.9951324792282,72.7990784358473,14.0014771110744));
#54922=CARTESIAN_POINT('Ctrl Pts',(14.9974356938212,72.7891442484205,14.022531239347));
#54923=CARTESIAN_POINT('Ctrl Pts',(15.0026964721551,72.7653530654631,14.0695591918255));
#54924=CARTESIAN_POINT('Ctrl Pts',(15.005664488695,72.7511608225082,14.0953468946793));
#54925=CARTESIAN_POINT('Ctrl Pts',(15.0121144821189,72.7187296772208,14.1497142051035));
#54926=CARTESIAN_POINT('Ctrl Pts',(15.0156037572945,72.7002164094905,14.1781030073912));
#54927=CARTESIAN_POINT('Ctrl Pts',(15.0274681411383,72.6340506589288,14.2712019345502));
#54928=CARTESIAN_POINT('Ctrl Pts',(15.0359687842437,72.5814012425502,14.3321221581525));
#54929=CARTESIAN_POINT('Ctrl Pts',(15.0479739647793,72.4984452249864,14.4114895455686));
#54930=CARTESIAN_POINT('Ctrl Pts',(15.0515536626689,72.4725694811561,14.4343028249508));
#54931=CARTESIAN_POINT('Ctrl Pts',(15.0567150271168,72.4333506005646,14.4661379036494));
#54932=CARTESIAN_POINT('Ctrl Pts',(15.0583400993012,72.4207157184319,14.4760032311401));
#54933=CARTESIAN_POINT('Ctrl Pts',(15.0613454038267,72.3967737347498,14.4939780040941));
#54934=CARTESIAN_POINT('Ctrl Pts',(15.0627286679121,72.385515204214,14.5021448367948));
#54935=CARTESIAN_POINT('Ctrl Pts',(15.0664975443531,72.3542292074216,14.5240641309082));
#54936=CARTESIAN_POINT('Ctrl Pts',(15.0688600499269,72.3339371394535,14.5374300511625));
#54937=CARTESIAN_POINT('Ctrl Pts',(15.0779950954556,72.253250337638,14.5873171930225));
#54938=CARTESIAN_POINT('Ctrl Pts',(15.0845851450513,72.190232864405,14.6193647444231));
#54939=CARTESIAN_POINT('Ctrl Pts',(15.0976326765066,72.0616363800101,14.6717947938584));
#54940=CARTESIAN_POINT('Ctrl Pts',(15.1040669574391,71.9964332881293,14.6924307606925));
#54941=CARTESIAN_POINT('Ctrl Pts',(15.1132679287311,71.9036371587971,14.7137602009614));
#54942=CARTESIAN_POINT('Ctrl Pts',(15.115893303152,71.8771969504096,14.7189578812514));
#54943=CARTESIAN_POINT('Ctrl Pts',(15.1207903773722,71.8281046082427,14.7269961290577));
#54944=CARTESIAN_POINT('Ctrl Pts',(15.123053648869,71.8055022330863,14.7300743429641));
#54945=CARTESIAN_POINT('Ctrl Pts',(15.1274646543716,71.7616870260599,14.7348437423548));
#54946=CARTESIAN_POINT('Ctrl Pts',(15.1296091768705,71.7404902318351,14.7366136258512));
#54947=CARTESIAN_POINT('Ctrl Pts',(15.1343033818943,71.6943578204931,14.739301139189));
#54948=CARTESIAN_POINT('Ctrl Pts',(15.1368579689929,71.669420131619,14.7400177389146));
#54949=CARTESIAN_POINT('Ctrl Pts',(15.1394309042231,71.6444797315774,14.7399996665771));
#54950=CARTESIAN_POINT('Ctrl Pts',(15.1394307620321,71.6444811098864,14.7399996675751));
#54951=CARTESIAN_POINT('Ctrl Pts',(15.1509210808744,71.533101228028,14.739919080253));
#54952=CARTESIAN_POINT('Ctrl Pts',(15.1627791610613,71.4222292170545,14.7251882517743));
#54953=CARTESIAN_POINT('Ctrl Pts',(15.1768284770286,71.2913020977506,14.6898779156159));
#54954=CARTESIAN_POINT('Ctrl Pts',(15.1793190930862,71.2680836105176,14.6828973793084));
#54955=CARTESIAN_POINT('Ctrl Pts',(15.1831877343141,71.2318876403853,14.6708749610823));
#54956=CARTESIAN_POINT('Ctrl Pts',(15.1845866594627,71.218769932039,14.666277569344));
#54957=CARTESIAN_POINT('Ctrl Pts',(15.1875722086513,71.190685709647,14.65591400007));
#54958=CARTESIAN_POINT('Ctrl Pts',(15.1891550046976,71.1757479795498,14.6500780374656));
#54959=CARTESIAN_POINT('Ctrl Pts',(15.1944197183191,71.1260255163516,14.6295582891983));
#54960=CARTESIAN_POINT('Ctrl Pts',(15.1980392416794,71.0917821032234,14.613605397761));
#54961=CARTESIAN_POINT('Ctrl Pts',(15.2090248745081,70.9891787709298,14.5601143564284));
#54962=CARTESIAN_POINT('Ctrl Pts',(15.2162629792696,70.9235239537745,14.5177936068783));
#54963=CARTESIAN_POINT('Ctrl Pts',(15.2268090935942,70.8357704161096,14.4490423742027));
#54964=CARTESIAN_POINT('Ctrl Pts',(15.2300000230711,70.8102101963678,14.4273305006902));
#54965=CARTESIAN_POINT('Ctrl Pts',(15.2360380432644,70.7640304866041,14.3848453839361));
#54966=CARTESIAN_POINT('Ctrl Pts',(15.2388748568639,70.7432120586773,14.3643214764988));
#54967=CARTESIAN_POINT('Ctrl Pts',(15.2436330533099,70.7098761913435,14.3291079197914));
#54968=CARTESIAN_POINT('Ctrl Pts',(15.2455362747428,70.6969519753471,14.3148179791374));
#54969=CARTESIAN_POINT('Ctrl Pts',(15.2474530402596,70.6843589428744,14.3002409809922));
#54970=CARTESIAN_POINT('',(15.3085945258992,71.645458134439,14.7400003205931));
#54971=CARTESIAN_POINT('Ctrl Pts',(15.4172344952204,70.6843589433712,14.3002409815672));
#54972=CARTESIAN_POINT('Ctrl Pts',(15.4127706930735,70.7148600299651,14.3355473530177));
#54973=CARTESIAN_POINT('Ctrl Pts',(15.4083832547445,70.7472863263589,14.3691492972001));
#54974=CARTESIAN_POINT('Ctrl Pts',(15.3967131226841,70.8383472626173,14.4536577777352));
#54975=CARTESIAN_POINT('Ctrl Pts',(15.3894543105498,70.8999107323482,14.5010966726018));
#54976=CARTESIAN_POINT('Ctrl Pts',(15.3791947372806,70.98993336973,14.5581665738801));
#54977=CARTESIAN_POINT('Ctrl Pts',(15.3763759031919,71.0149788345287,14.5728652884407));
#54978=CARTESIAN_POINT('Ctrl Pts',(15.371243010044,71.0609622006778,14.5977738342165));
#54979=CARTESIAN_POINT('Ctrl Pts',(15.3689408886463,71.0817196132603,14.6082906516138));
#54980=CARTESIAN_POINT('Ctrl Pts',(15.3636847355834,71.1293289710434,14.6307905726155));
#54981=CARTESIAN_POINT('Ctrl Pts',(15.3607203007963,71.1563305661364,14.6424226167686));
#54982=CARTESIAN_POINT('Ctrl Pts',(15.354279875988,71.2152194070113,14.6654031936946));
#54983=CARTESIAN_POINT('Ctrl Pts',(15.3507966335996,71.2472054438283,14.6764347331971));
#54984=CARTESIAN_POINT('Ctrl Pts',(15.3393010133244,71.3531858267669,14.7083122361119));
#54985=CARTESIAN_POINT('Ctrl Pts',(15.331176493587,71.4286354225623,14.7237215690252));
#54986=CARTESIAN_POINT('Ctrl Pts',(15.3198877989525,71.5357798711219,14.7356390330013));
#54987=CARTESIAN_POINT('Ctrl Pts',(15.3166634990233,71.5666714167958,14.7379356869999));
#54988=CARTESIAN_POINT('Ctrl Pts',(15.3118384439432,71.6135569828337,14.7397009132116));
#54989=CARTESIAN_POINT('Ctrl Pts',(15.3102091325305,71.6295062635558,14.7400007281653));
#54990=CARTESIAN_POINT('Ctrl Pts',(15.3085939729866,71.6454580784378,14.739999998672));
#54991=CARTESIAN_POINT('Ctrl Pts',(14.625502981677,70.6843589433682,14.3002409815638));
#54992=CARTESIAN_POINT('Ctrl Pts',(14.6281650357797,70.6666703255623,14.2797656155869));
#54993=CARTESIAN_POINT('Ctrl Pts',(14.6308005194417,70.6496391110251,14.2587284948775));
#54994=CARTESIAN_POINT('Ctrl Pts',(14.6411179044699,70.5851039435374,14.1735878753866));
#54995=CARTESIAN_POINT('Ctrl Pts',(14.648593760091,70.5430096721227,14.1056113942086));
#54996=CARTESIAN_POINT('Ctrl Pts',(14.6625924101878,70.4767980028742,13.9720636382048));
#54997=CARTESIAN_POINT('Ctrl Pts',(14.6690915769207,70.4511624437155,13.9075979717112));
#54998=CARTESIAN_POINT('Ctrl Pts',(14.6774573056598,70.426010423835,13.8253450487112));
#54999=CARTESIAN_POINT('Ctrl Pts',(14.6791009835702,70.4214265022496,13.8092194279602));
#55000=CARTESIAN_POINT('Ctrl Pts',(14.6820939757825,70.4137425546004,13.7800013626373));
#55001=CARTESIAN_POINT('Ctrl Pts',(14.6834373704991,70.4105290649238,13.7669421350229));
#55002=CARTESIAN_POINT('Ctrl Pts',(14.686612591975,70.4034860000019,13.7362254274108));
#55003=CARTESIAN_POINT('Ctrl Pts',(14.6884521353256,70.3998250761717,13.7185343971115));
#55004=CARTESIAN_POINT('Ctrl Pts',(14.6967219037202,70.3851863146071,13.6393149227284));
#55005=CARTESIAN_POINT('Ctrl Pts',(14.7032974414655,70.3783830775501,13.5771093715393));
#55006=CARTESIAN_POINT('Ctrl Pts',(14.7186402538576,70.3732534566918,13.4313400215769));
#55007=CARTESIAN_POINT('Ctrl Pts',(14.7273599950559,70.3785330673784,13.3479132534191));
#55008=CARTESIAN_POINT('Ctrl Pts',(14.7387587019873,70.3965651282886,13.237339522462));
#55009=CARTESIAN_POINT('Ctrl Pts',(14.7416426692286,70.4021268058687,13.2092481444338));
#55010=CARTESIAN_POINT('Ctrl Pts',(14.7468190743007,70.4139241861666,13.1586976489804));
#55011=CARTESIAN_POINT('Ctrl Pts',(14.7491203423951,70.4198370640752,13.1361774421891));
#55012=CARTESIAN_POINT('Ctrl Pts',(14.7543305600558,70.4347384645587,13.0851755539095));
#55013=CARTESIAN_POINT('Ctrl Pts',(14.7572258578014,70.4441191849167,13.0568221458506));
#55014=CARTESIAN_POINT('Ctrl Pts',(14.7634268590528,70.4665278387567,12.9963324610459));
#55015=CARTESIAN_POINT('Ctrl Pts',(14.766721030978,70.4798894970243,12.9643458324319));
#55016=CARTESIAN_POINT('Ctrl Pts',(14.7781217399889,70.5309020910025,12.8550311987522));
#55017=CARTESIAN_POINT('Ctrl Pts',(14.7860860949509,70.5750749040709,12.7810194578937));
#55018=CARTESIAN_POINT('Ctrl Pts',(14.7972187739038,70.6445886321964,12.6875631584461));
#55019=CARTESIAN_POINT('Ctrl Pts',(14.8001643096785,70.6636708562699,12.663750525638));
#55020=CARTESIAN_POINT('Ctrl Pts',(14.80461855296,70.6932741349911,12.6294190745434));
#55021=CARTESIAN_POINT('Ctrl Pts',(14.8060876079797,70.703154313686,12.6183586759229));
#55022=CARTESIAN_POINT('Ctrl Pts',(14.8090396473062,70.7231955128251,12.5966991301657));
#55023=CARTESIAN_POINT('Ctrl Pts',(14.8105221701063,70.7333512188006,12.5860981572875));
#55024=CARTESIAN_POINT('Ctrl Pts',(14.8150187030111,70.7644645464167,12.554727763174));
#55025=CARTESIAN_POINT('Ctrl Pts',(14.8180656787368,70.7859630046302,12.5345117963949));
#55026=CARTESIAN_POINT('Ctrl Pts',(14.8260499202662,70.8436170630015,12.483962527035));
#55027=CARTESIAN_POINT('Ctrl Pts',(14.8310188368833,70.8807949535119,12.4548623300102));
#55028=CARTESIAN_POINT('Ctrl Pts',(14.8440812699463,70.9827214779599,12.3838633423603));
#55029=CARTESIAN_POINT('Ctrl Pts',(14.8521258926325,71.0498271705976,12.345663234386));
#55030=CARTESIAN_POINT('Ctrl Pts',(14.8629319742427,71.1464456942483,12.3017582754833));
#55031=CARTESIAN_POINT('Ctrl Pts',(14.86586109953,71.1733038414498,12.2906486153169));
#55032=CARTESIAN_POINT('Ctrl Pts',(14.8710817197662,71.222312132462,12.2723198003389));
#55033=CARTESIAN_POINT('Ctrl Pts',(14.8733829333636,71.2443233816318,12.2647701767818));
#55034=CARTESIAN_POINT('Ctrl Pts',(14.8785467270058,71.2945589828123,12.249068855161));
#55035=CARTESIAN_POINT('Ctrl Pts',(14.8813966669327,71.3228842416262,12.2412827094571));
#55036=CARTESIAN_POINT('Ctrl Pts',(14.8874712550081,71.3843141124413,12.2266678333283));
#55037=CARTESIAN_POINT('Ctrl Pts',(14.8906853472985,71.4174725291364,12.2201639594458));
#55038=CARTESIAN_POINT('Ctrl Pts',(14.9014132207844,71.5295603224371,12.2027885712705));
#55039=CARTESIAN_POINT('Ctrl Pts',(14.9088048202201,71.6092359614705,12.1980193778373));
#55040=CARTESIAN_POINT('Ctrl Pts',(14.91972421691,71.7240322559499,12.2019472974245));
#55041=CARTESIAN_POINT('Ctrl Pts',(14.9231045297655,71.7591650869083,12.2046156587327));
#55042=CARTESIAN_POINT('Ctrl Pts',(14.9281275428201,71.810144883202,12.2106275581656));
#55043=CARTESIAN_POINT('Ctrl Pts',(14.9297180521815,71.826114158646,12.2128197734387));
#55044=CARTESIAN_POINT('Ctrl Pts',(14.9327074284313,71.8557319432653,12.2174615128714));
#55045=CARTESIAN_POINT('Ctrl Pts',(14.9341022506016,71.8693899663505,12.2198317755868));
#55046=CARTESIAN_POINT('Ctrl Pts',(14.9379401683027,71.906566753415,12.2269122244914));
#55047=CARTESIAN_POINT('Ctrl Pts',(14.9404036066684,71.9299941023716,12.2320657379584));
#55048=CARTESIAN_POINT('Ctrl Pts',(14.9501991470752,72.0217487154213,12.2549916236513));
#55049=CARTESIAN_POINT('Ctrl Pts',(14.9576632891323,72.0886885870838,12.2777844009164));
#55050=CARTESIAN_POINT('Ctrl Pts',(14.971685112274,72.2111849315068,12.331244288908));
#55051=CARTESIAN_POINT('Ctrl Pts',(14.9782370942326,72.2670350487451,12.3607436224752));
#55052=CARTESIAN_POINT('Ctrl Pts',(14.9875940308943,72.3449011490051,12.4096085389612));
#55053=CARTESIAN_POINT('Ctrl Pts',(14.9905009144876,72.3688047158754,12.4257692480362));
#55054=CARTESIAN_POINT('Ctrl Pts',(14.995699177761,72.4109576578052,12.4564109754643));
#55055=CARTESIAN_POINT('Ctrl Pts',(14.9979998490801,72.4293977176263,12.470605686936));
#55056=CARTESIAN_POINT('Ctrl Pts',(15.0031839515583,72.4703774544436,12.5039837220097));
#55057=CARTESIAN_POINT('Ctrl Pts',(15.006054278118,72.4926581163954,12.5234646046496));
#55058=CARTESIAN_POINT('Ctrl Pts',(15.0121857808431,72.5391615644335,12.5670837369629));
#55059=CARTESIAN_POINT('Ctrl Pts',(15.0154359609183,72.563131290677,12.5914573767965));
#55060=CARTESIAN_POINT('Ctrl Pts',(15.0264586787469,72.6414582315259,12.6778132522666));
#55061=CARTESIAN_POINT('Ctrl Pts',(15.0341004678183,72.6907488873929,12.7440964190608));
#55062=CARTESIAN_POINT('Ctrl Pts',(15.0450547094162,72.7500739692957,12.8425797998964));
#55063=CARTESIAN_POINT('Ctrl Pts',(15.048187766418,72.7657976174822,12.8711099278409));
#55064=CARTESIAN_POINT('Ctrl Pts',(15.0529179139282,72.7874603536593,12.9142613990469));
#55065=CARTESIAN_POINT('Ctrl Pts',(15.0544711149184,72.7942527713946,12.928442556352));
#55066=CARTESIAN_POINT('Ctrl Pts',(15.0574416316971,72.8066095283088,12.955520044123));
#55067=CARTESIAN_POINT('Ctrl Pts',(15.0588559326595,72.8122264226868,12.9683893951691));
#55068=CARTESIAN_POINT('Ctrl Pts',(15.0628436036574,72.8273417407841,13.0046495455841));
#55069=CARTESIAN_POINT('Ctrl Pts',(15.0654400750875,72.8363572428287,13.0282332221697));
#55070=CARTESIAN_POINT('Ctrl Pts',(15.0755115401593,72.8683120497401,13.1199278921612));
#55071=CARTESIAN_POINT('Ctrl Pts',(15.0831133857725,72.8861574442324,13.1896704384541));
#55072=CARTESIAN_POINT('Ctrl Pts',(15.0969656521181,72.9079524885354,13.3200120460876));
#55073=CARTESIAN_POINT('Ctrl Pts',(15.1032216474005,72.91365047315,13.3801205914671));
#55074=CARTESIAN_POINT('Ctrl Pts',(15.1122694267702,72.915721987669,13.4690252116037));
#55075=CARTESIAN_POINT('Ctrl Pts',(15.1151524317689,72.9154215180554,13.497650981896));
#55076=CARTESIAN_POINT('Ctrl Pts',(15.1203273983721,72.9131232239384,13.5494949149088));
#55077=CARTESIAN_POINT('Ctrl Pts',(15.122628181847,72.9114535835471,13.5727137465772));
#55078=CARTESIAN_POINT('Ctrl Pts',(15.127837453955,72.9061881208148,13.62557716566));
#55079=CARTESIAN_POINT('Ctrl Pts',(15.1307322902144,72.9021832539147,13.6551678180347));
#55080=CARTESIAN_POINT('Ctrl Pts',(15.1369321502809,72.8912853510357,13.7187362901842));
#55081=CARTESIAN_POINT('Ctrl Pts',(15.1402256459912,72.8840369798038,13.7526284521532));
#55082=CARTESIAN_POINT('Ctrl Pts',(15.1516201001995,72.8540199604457,13.8693997509815));
#55083=CARTESIAN_POINT('Ctrl Pts',(15.159579010404,72.8242413019048,13.9502221895792));
#55084=CARTESIAN_POINT('Ctrl Pts',(15.1707121077332,72.7731131753678,14.0548916325578));
#55085=CARTESIAN_POINT('Ctrl Pts',(15.1736643731797,72.7587042797595,14.0818728029703));
#55086=CARTESIAN_POINT('Ctrl Pts',(15.1781263249164,72.7358797538617,14.121132940331));
#55087=CARTESIAN_POINT('Ctrl Pts',(15.1795961315517,72.7281979672583,14.133828806804));
#55088=CARTESIAN_POINT('Ctrl Pts',(15.1825474325921,72.7124851301447,14.158799263465));
#55089=CARTESIAN_POINT('Ctrl Pts',(15.1840284283488,72.704460310662,14.1710750885831));
#55090=CARTESIAN_POINT('Ctrl Pts',(15.1885138951142,72.6797079287449,14.2075447179073));
#55091=CARTESIAN_POINT('Ctrl Pts',(15.1915511099815,72.6623517964571,14.2312974033249));
#55092=CARTESIAN_POINT('Ctrl Pts',(15.1994980567093,72.6152102830187,14.2913216621672));
#55093=CARTESIAN_POINT('Ctrl Pts',(15.204439160851,72.5842103376323,14.326583910747));
#55094=CARTESIAN_POINT('Ctrl Pts',(15.2175237121263,72.4970117535786,14.4153386370559));
#55095=CARTESIAN_POINT('Ctrl Pts',(15.2256180769774,72.4377334042762,14.4655501307541));
#55096=CARTESIAN_POINT('Ctrl Pts',(15.2364688499461,72.3504598248198,14.5267087662254));
#55097=CARTESIAN_POINT('Ctrl Pts',(15.2393955214991,72.326119135113,14.5425505008356));
#55098=CARTESIAN_POINT('Ctrl Pts',(15.2446136408711,72.2813327949977,14.5695593080877));
#55099=CARTESIAN_POINT('Ctrl Pts',(15.2469147608939,72.2610835513615,14.5810243618296));
#55100=CARTESIAN_POINT('Ctrl Pts',(15.2520806502773,72.2145676982552,14.6056988021584));
#55101=CARTESIAN_POINT('Ctrl Pts',(15.2549327303139,72.1881339944443,14.6185659600403));
#55102=CARTESIAN_POINT('Ctrl Pts',(15.265478793839,72.0879567899197,14.6630973513499));
#55103=CARTESIAN_POINT('Ctrl Pts',(15.2729768750885,72.0117112332123,14.6886697713735));
#55104=CARTESIAN_POINT('Ctrl Pts',(15.2862665339128,71.873981044218,14.7207567250915));
#55105=CARTESIAN_POINT('Ctrl Pts',(15.2920266258047,71.8134912599672,14.7303113450748));
#55106=CARTESIAN_POINT('Ctrl Pts',(15.2997933941884,71.7338225680731,14.7370576237826));
#55107=CARTESIAN_POINT('Ctrl Pts',(15.3016361639581,71.7150550039059,14.7382277455188));
#55108=CARTESIAN_POINT('Ctrl Pts',(15.3044043025565,71.6871607902727,14.7393459544147));
#55109=CARTESIAN_POINT('Ctrl Pts',(15.3053132419976,71.6780485569726,14.7396130026395));
#55110=CARTESIAN_POINT('Ctrl Pts',(15.3070127609763,71.6611088892174,14.7399269598222));
#55111=CARTESIAN_POINT('Ctrl Pts',(15.3078016756847,71.6532830495909,14.7399996448132));
#55112=CARTESIAN_POINT('Ctrl Pts',(15.3085940384764,71.64545743164,14.7399999987014));
#55113=CARTESIAN_POINT('Origin',(19.939,71.6454,13.47));
#55114=CARTESIAN_POINT('',(19.5292399153773,71.6444186650849,15.1743397174806));
#55115=CARTESIAN_POINT('',(19.7889963629056,70.1379689624582,12.6747475226976));
#55116=CARTESIAN_POINT('Ctrl Pts',(19.5292399154299,71.6444186643779,15.1743397174802));
#55117=CARTESIAN_POINT('Ctrl Pts',(19.5334081355681,71.5884378095259,15.1743074844656));
#55118=CARTESIAN_POINT('Ctrl Pts',(19.5375763557064,71.5325354676037,15.1715172641341));
#55119=CARTESIAN_POINT('Ctrl Pts',(19.5417445758447,71.4769114548334,15.1659912870495));
#55120=CARTESIAN_POINT('Ctrl Pts',(19.5463562733338,71.415369330973,15.159877374204));
#55121=CARTESIAN_POINT('Ctrl Pts',(19.550967970823,71.3540405821946,15.1503975106808));
#55122=CARTESIAN_POINT('Ctrl Pts',(19.5555796683121,71.2933205891731,15.137577561636));
#55123=CARTESIAN_POINT('Ctrl Pts',(19.5601909325851,71.2326063000995,15.1247588168786));
#55124=CARTESIAN_POINT('Ctrl Pts',(19.5648021968581,71.1725011599338,15.1086006332566));
#55125=CARTESIAN_POINT('Ctrl Pts',(19.5694134611311,71.1133962734374,15.0891809258151));
#55126=CARTESIAN_POINT('Ctrl Pts',(19.5740128278848,71.0544438834107,15.0698113231451));
#55127=CARTESIAN_POINT('Ctrl Pts',(19.5786121946386,70.9964870838616,15.0471971245032));
#55128=CARTESIAN_POINT('Ctrl Pts',(19.5832115613924,70.9399023287022,15.02146636167));
#55129=CARTESIAN_POINT('Ctrl Pts',(19.587808163908,70.8833515812112,14.99575106313));
#55130=CARTESIAN_POINT('Ctrl Pts',(19.5924047664236,70.8281717016542,14.966923124334));
#55131=CARTESIAN_POINT('Ctrl Pts',(19.5970013689392,70.7747195976396,14.9351588557373));
#55132=CARTESIAN_POINT('Ctrl Pts',(19.6015968666095,70.721280341442,14.9034022220414));
#55133=CARTESIAN_POINT('Ctrl Pts',(19.6061923642797,70.6695684702962,14.868710918185));
#55134=CARTESIAN_POINT('Ctrl Pts',(19.61078786195,70.6199149177897,14.8313064246392));
#55135=CARTESIAN_POINT('Ctrl Pts',(19.6154097076928,70.5699766789452,14.7936874741664));
#55136=CARTESIAN_POINT('Ctrl Pts',(19.6200315534356,70.522120864648,14.7533244120962));
#55137=CARTESIAN_POINT('Ctrl Pts',(19.6246533991784,70.4766514692552,14.7104844648289));
#55138=CARTESIAN_POINT('Ctrl Pts',(19.6292543668237,70.4313874711258,14.6678380369136));
#55139=CARTESIAN_POINT('Ctrl Pts',(19.6338553344691,70.3884886980699,14.622737453413));
#55140=CARTESIAN_POINT('Ctrl Pts',(19.6384563021145,70.3482171986574,14.5754825260949));
#55141=CARTESIAN_POINT('Ctrl Pts',(19.643088586906,70.3076715855085,14.5279059513366));
#55142=CARTESIAN_POINT('Ctrl Pts',(19.6477208716975,70.2697894690637,14.4781460013856));
#55143=CARTESIAN_POINT('Ctrl Pts',(19.652353156489,70.2347948046825,14.4265395018207));
#55144=CARTESIAN_POINT('Ctrl Pts',(19.6569854412805,70.1998001403013,14.3749330022558));
#55145=CARTESIAN_POINT('Ctrl Pts',(19.661617726072,70.1676931439373,14.3214804259295));
#55146=CARTESIAN_POINT('Ctrl Pts',(19.6662500108635,70.1386503546158,14.2665427431938));
#55147=CARTESIAN_POINT('Ctrl Pts',(19.6708443877018,70.1098452347706,14.2120546388416));
#55148=CARTESIAN_POINT('Ctrl Pts',(19.6754387645401,70.0839421319649,14.1558933370675));
#55149=CARTESIAN_POINT('Ctrl Pts',(19.6800331413783,70.0611374155199,14.0984002697456));
#55150=CARTESIAN_POINT('Ctrl Pts',(19.6846198308241,70.0383708563294,14.0410034008401));
#55151=CARTESIAN_POINT('Ctrl Pts',(19.6892065202698,70.0186925768024,13.9822796606064));
#55152=CARTESIAN_POINT('Ctrl Pts',(19.6937932097156,70.0022525532405,13.9225939723503));
#55153=CARTESIAN_POINT('Ctrl Pts',(19.6983756147656,69.9858278861939,13.8629640360935));
#55154=CARTESIAN_POINT('Ctrl Pts',(19.7029580198156,69.9726356143561,13.8023744217564));
#55155=CARTESIAN_POINT('Ctrl Pts',(19.7075404248657,69.9627766285917,13.7412073479659));
#55156=CARTESIAN_POINT('Ctrl Pts',(19.7121202365844,69.9529232223464,13.6800748906018));
#55157=CARTESIAN_POINT('Ctrl Pts',(19.7167000483031,69.9463994422805,13.6183661239773));
#55158=CARTESIAN_POINT('Ctrl Pts',(19.7212798600218,69.9432551338905,13.5564736397827));
#55159=CARTESIAN_POINT('Ctrl Pts',(19.7258587659086,69.9401114474072,13.4945933971816));
#55160=CARTESIAN_POINT('Ctrl Pts',(19.7304376717953,69.9403459308535,13.4325300178702));
#55161=CARTESIAN_POINT('Ctrl Pts',(19.735016577682,69.9439564243733,13.3706793346843));
#55162=CARTESIAN_POINT('Ctrl Pts',(19.7395995429358,69.9475701187275,13.3087738186113));
#55163=CARTESIAN_POINT('Ctrl Pts',(19.7441825081896,69.9545657749991,13.2470818853951));
#55164=CARTESIAN_POINT('Ctrl Pts',(19.7487654734434,69.9648891529298,13.1859962527016));
#55165=CARTESIAN_POINT('Ctrl Pts',(19.7533503268661,69.9752167840633,13.124885452899));
#55166=CARTESIAN_POINT('Ctrl Pts',(19.7579351802887,69.9888747583705,13.0643819498165));
#55167=CARTESIAN_POINT('Ctrl Pts',(19.7625200337113,70.005757866363,13.0048672133656));
#55168=CARTESIAN_POINT('Ctrl Pts',(19.7671134700236,70.0226725796959,12.9452410647561));
#55169=CARTESIAN_POINT('Ctrl Pts',(19.7717069063359,70.0428243259473,12.8866078653173));
#55170=CARTESIAN_POINT('Ctrl Pts',(19.7763003426482,70.0660585204686,12.8293321245516));
#55171=CARTESIAN_POINT('Ctrl Pts',(19.7805323494007,70.0874645575652,12.7765630633974));
#55172=CARTESIAN_POINT('Ctrl Pts',(19.7847643561531,70.1114863591526,12.7249462951846));
#55173=CARTESIAN_POINT('Ctrl Pts',(19.7889963629056,70.1379689624582,12.6747475226976));
#55174=CARTESIAN_POINT('',(19.789,70.1379459883857,14.2652089275579));
#55175=CARTESIAN_POINT('Origin',(19.789,71.6454,13.47));
#55176=CARTESIAN_POINT('',(19.6518850845702,71.6441855388828,15.174605651636));
#55177=CARTESIAN_POINT('Ctrl Pts',(19.789,70.1379459883857,14.2652089275579));
#55178=CARTESIAN_POINT('Ctrl Pts',(19.7474981883271,70.3991888501049,14.7604392830743));
#55179=CARTESIAN_POINT('Ctrl Pts',(19.7017932165172,70.9742539043654,15.1485528849809));
#55180=CARTESIAN_POINT('Ctrl Pts',(19.6560882447072,71.5877183033873,15.1763527703962));
#55181=CARTESIAN_POINT('Ctrl Pts',(19.6518850845702,71.6441845643294,15.1759735251619));
#55182=CARTESIAN_POINT('',(18.858135084626,71.6451886815825,15.1743399868995));
#55183=CARTESIAN_POINT('Ctrl Pts',(19.6518850845702,71.6441857284568,15.1743395674409));
#55184=CARTESIAN_POINT('Ctrl Pts',(19.6472227531282,71.7067602847858,15.1743841492276));
#55185=CARTESIAN_POINT('Ctrl Pts',(19.6425604216862,71.7694858767845,15.1709778041751));
#55186=CARTESIAN_POINT('Ctrl Pts',(19.6378980902442,71.8319411817604,15.1641007122091));
#55187=CARTESIAN_POINT('Ctrl Pts',(19.6333926468792,71.8922948573665,15.1574550353081));
#55188=CARTESIAN_POINT('Ctrl Pts',(19.6288872035141,71.9523955681993,15.1475685326357));
#55189=CARTESIAN_POINT('Ctrl Pts',(19.624381760149,72.0118616368733,15.1344761050553));
#55190=CARTESIAN_POINT('Ctrl Pts',(19.6198801777333,72.0712767459725,15.1213948970588));
#55191=CARTESIAN_POINT('Ctrl Pts',(19.6153785953175,72.1300577754547,15.1051133163245));
#55192=CARTESIAN_POINT('Ctrl Pts',(19.6108770129018,72.1878305538533,15.0857177754318));
#55193=CARTESIAN_POINT('Ctrl Pts',(19.6063775010452,72.2455767589396,15.0663311557609));
#55194=CARTESIAN_POINT('Ctrl Pts',(19.6018779891886,72.3023151312258,15.0438335819748));
#55195=CARTESIAN_POINT('Ctrl Pts',(19.5973784773321,72.3576863001101,15.0183614120338));
#55196=CARTESIAN_POINT('Ctrl Pts',(19.5928792492668,72.4130539766476,14.9928908486628));
#55197=CARTESIAN_POINT('Ctrl Pts',(19.5883800212015,72.4670541418949,14.9644462851191));
#55198=CARTESIAN_POINT('Ctrl Pts',(19.5838807931362,72.5193492133626,14.9332114023828));
#55199=CARTESIAN_POINT('Ctrl Pts',(19.5793772343218,72.5716946216507,14.901946454391));
#55200=CARTESIAN_POINT('Ctrl Pts',(19.5748736755074,72.6223312086906,14.8678861028988));
#55201=CARTESIAN_POINT('Ctrl Pts',(19.570370116693,72.6709491311669,14.831258173589));
#55202=CARTESIAN_POINT('Ctrl Pts',(19.5658639275193,72.7195954495422,14.7946088512839));
#55203=CARTESIAN_POINT('Ctrl Pts',(19.5613577383457,72.766220357122,14.7553893123699));
#55204=CARTESIAN_POINT('Ctrl Pts',(19.556851549172,72.810548448634,14.7138665234846));
#55205=CARTESIAN_POINT('Ctrl Pts',(19.5523379098736,72.8549498281948,14.6722750845837));
#55206=CARTESIAN_POINT('Ctrl Pts',(19.5478242705752,72.8970464603924,14.6283731881336));
#55207=CARTESIAN_POINT('Ctrl Pts',(19.5433106312768,72.9366020707453,14.5824621558072));
#55208=CARTESIAN_POINT('Ctrl Pts',(19.542203464172,72.9463048111941,14.5712004706397));
#55209=CARTESIAN_POINT('Ctrl Pts',(19.5410962970673,72.9558548642394,14.5598180361732));
#55210=CARTESIAN_POINT('Ctrl Pts',(19.5399891299625,72.9652491465984,14.5483195564504));
#55211=CARTESIAN_POINT('Ctrl Pts',(19.5353826477796,73.0043350209182,14.5004789533968));
#55212=CARTESIAN_POINT('Ctrl Pts',(19.5307761655967,73.0408937684296,14.4504158455636));
#55213=CARTESIAN_POINT('Ctrl Pts',(19.5261696834138,73.0746645583352,14.3984275189195));
#55214=CARTESIAN_POINT('Ctrl Pts',(19.5215577672275,73.1084751857084,14.3463778646225));
#55215=CARTESIAN_POINT('Ctrl Pts',(19.5169458510412,73.1394909176284,14.2923988142978));
#55216=CARTESIAN_POINT('Ctrl Pts',(19.512333934855,73.1674899195399,14.2368227386006));
#55217=CARTESIAN_POINT('Ctrl Pts',(19.5077398498217,73.1953806682949,14.1814615379067));
#55218=CARTESIAN_POINT('Ctrl Pts',(19.5031457647884,73.2202777143286,14.1245160771108));
#55219=CARTESIAN_POINT('Ctrl Pts',(19.498551679755,73.2420059035321,14.0663425394908));
#55220=CARTESIAN_POINT('Ctrl Pts',(19.4939603691465,73.2637209708136,14.0082041335893));
#55221=CARTESIAN_POINT('Ctrl Pts',(19.4893690585379,73.2822707998122,13.9488395953978));
#55222=CARTESIAN_POINT('Ctrl Pts',(19.4847777479293,73.2975282063429,13.8886253998578));
#55223=CARTESIAN_POINT('Ctrl Pts',(19.4801875437516,73.3127819360878,13.8284257149559));
#55224=CARTESIAN_POINT('Ctrl Pts',(19.475597339574,73.3247446945025,13.7673772701358));
#55225=CARTESIAN_POINT('Ctrl Pts',(19.4710071353963,73.3333396153203,13.7058700715062));
#55226=CARTESIAN_POINT('Ctrl Pts',(19.4663801820252,73.3420033471093,13.6438704459933));
#55227=CARTESIAN_POINT('Ctrl Pts',(19.4617532286542,73.3472449687181,13.5814052001833));
#55228=CARTESIAN_POINT('Ctrl Pts',(19.4571262752831,73.3490389145714,13.5188803064433));
#55229=CARTESIAN_POINT('Ctrl Pts',(19.4525305464212,73.3508207541694,13.4567773553848));
#55230=CARTESIAN_POINT('Ctrl Pts',(19.4479348175592,73.349201374521,13.3946160704898));
#55231=CARTESIAN_POINT('Ctrl Pts',(19.4433390886972,73.3442081332339,13.3327929955936));
#55232=CARTESIAN_POINT('Ctrl Pts',(19.4386965230716,73.3391640039879,13.2703398589962));
#55233=CARTESIAN_POINT('Ctrl Pts',(19.434053957446,73.330676909655,13.2082323908635));
#55234=CARTESIAN_POINT('Ctrl Pts',(19.4294113918204,73.3188282118031,13.1468702187333));
#55235=CARTESIAN_POINT('Ctrl Pts',(19.4247688261948,73.3069795139512,13.0855080466031));
#55236=CARTESIAN_POINT('Ctrl Pts',(19.4201262605693,73.2917693994114,13.0248916663312));
#55237=CARTESIAN_POINT('Ctrl Pts',(19.4154836949437,73.2733304595571,12.965403869965));
#55238=CARTESIAN_POINT('Ctrl Pts',(19.4108727106458,73.2550169516837,12.9063207428584));
#55239=CARTESIAN_POINT('Ctrl Pts',(19.406261726348,73.2334478747545,12.8481231124961));
#55240=CARTESIAN_POINT('Ctrl Pts',(19.4016507420502,73.2087284876023,12.7911930499391));
#55241=CARTESIAN_POINT('Ctrl Pts',(19.3970393886283,73.184007121584,12.7342584299483));
#55242=CARTESIAN_POINT('Ctrl Pts',(19.3924280352064,73.1561350620157,12.678592074235));
#55243=CARTESIAN_POINT('Ctrl Pts',(19.3878166817845,73.1252677430926,12.6245614755916));
#55244=CARTESIAN_POINT('Ctrl Pts',(19.3832176093261,73.0944826300603,12.5706747713206));
#55245=CARTESIAN_POINT('Ctrl Pts',(19.3786185368676,73.0607184085154,12.5184155797055));
#55246=CARTESIAN_POINT('Ctrl Pts',(19.3740194644092,73.0241765763943,12.4681267605198));
#55247=CARTESIAN_POINT('Ctrl Pts',(19.3694229982887,72.9876554528757,12.4178664404846));
#55248=CARTESIAN_POINT('Ctrl Pts',(19.3648265321682,72.9483601375223,12.3695746861601));
#55249=CARTESIAN_POINT('Ctrl Pts',(19.3602300660477,72.9065354499344,12.3235654346982));
#55250=CARTESIAN_POINT('Ctrl Pts',(19.3556345471125,72.864719381083,12.2775656642783));
#55251=CARTESIAN_POINT('Ctrl Pts',(19.3510390281773,72.8203753150686,12.2338478362991));
#55252=CARTESIAN_POINT('Ctrl Pts',(19.3464435092422,72.7737870453277,12.1926913013932));
#55253=CARTESIAN_POINT('Ctrl Pts',(19.3418214051324,72.7269292614575,12.1512966750592));
#55254=CARTESIAN_POINT('Ctrl Pts',(19.3371993010226,72.6778015952658,12.1124934315799));
#55255=CARTESIAN_POINT('Ctrl Pts',(19.3325771969128,72.6267271955063,12.0765252887261));
#55256=CARTESIAN_POINT('Ctrl Pts',(19.3279758236866,72.5758818726795,12.0407184688029));
#55257=CARTESIAN_POINT('Ctrl Pts',(19.3233744504603,72.5231076989931,12.0077216037023));
#55258=CARTESIAN_POINT('Ctrl Pts',(19.3187730772341,72.4687512366767,11.9777307291702));
#55259=CARTESIAN_POINT('Ctrl Pts',(19.3141406076826,72.4140274304933,11.9475371747109));
#55260=CARTESIAN_POINT('Ctrl Pts',(19.309508138131,72.3577003334321,11.9203906244013));
#55261=CARTESIAN_POINT('Ctrl Pts',(19.3048756685795,72.3001449413085,11.8964422802353));
#55262=CARTESIAN_POINT('Ctrl Pts',(19.300243199028,72.2425895491849,11.8724939360694));
#55263=CARTESIAN_POINT('Ctrl Pts',(19.2956107294764,72.1838063688168,11.8517439127542));
#55264=CARTESIAN_POINT('Ctrl Pts',(19.2909782599249,72.1241843895038,11.8342920969906));
#55265=CARTESIAN_POINT('Ctrl Pts',(19.286378296262,72.064980775686,11.8169627400522));
#55266=CARTESIAN_POINT('Ctrl Pts',(19.281778332599,72.00471595295,11.80281691182));
#55267=CARTESIAN_POINT('Ctrl Pts',(19.2771783689361,71.9437642251172,11.7919792537724));
#55268=CARTESIAN_POINT('Ctrl Pts',(19.2725656379349,71.8826433239197,11.781111515477));
#55269=CARTESIAN_POINT('Ctrl Pts',(19.2679529069336,71.8208321764191,11.7735705373702));
#55270=CARTESIAN_POINT('Ctrl Pts',(19.2633401759324,71.7587241672146,11.7694317218279));
#55271=CARTESIAN_POINT('Ctrl Pts',(19.2587526068373,71.69695494991,11.7653154830386));
#55272=CARTESIAN_POINT('Ctrl Pts',(19.2541650377422,71.63489261025,11.7645644418691));
#55273=CARTESIAN_POINT('Ctrl Pts',(19.2495774686471,71.5729324668579,11.7672013353775));
#55274=CARTESIAN_POINT('Ctrl Pts',(19.2449926537738,71.511009522247,11.7698366457838));
#55275=CARTESIAN_POINT('Ctrl Pts',(19.2404078389006,71.4491891590318,11.7758558357454));
#55276=CARTESIAN_POINT('Ctrl Pts',(19.2358230240273,71.3878667231025,11.7852295566189));
#55277=CARTESIAN_POINT('Ctrl Pts',(19.231239283968,71.3265586629355,11.7946010800197));
#55278=CARTESIAN_POINT('Ctrl Pts',(19.2266555439086,71.2657488004955,11.8073254961146));
#55279=CARTESIAN_POINT('Ctrl Pts',(19.2220718038493,71.2058253451771,11.8233218412703));
#55280=CARTESIAN_POINT('Ctrl Pts',(19.2174385556041,71.1452546669515,11.8394909601915));
#55281=CARTESIAN_POINT('Ctrl Pts',(19.2128053073588,71.0855901798453,11.8590030134026));
#55282=CARTESIAN_POINT('Ctrl Pts',(19.2081720591135,71.0272179277177,11.8817223916743));
#55283=CARTESIAN_POINT('Ctrl Pts',(19.2035826403476,70.969397863879,11.9042268497715));
#55284=CARTESIAN_POINT('Ctrl Pts',(19.1989932215818,70.9128461350012,11.9298779404172));
#55285=CARTESIAN_POINT('Ctrl Pts',(19.1944038028159,70.8579162553476,11.9584960511106));
#55286=CARTESIAN_POINT('Ctrl Pts',(19.1897486398309,70.80219949565,11.9875241211986));
#55287=CARTESIAN_POINT('Ctrl Pts',(19.185093476846,70.7481518940692,12.019604631197));
#55288=CARTESIAN_POINT('Ctrl Pts',(19.180438313861,70.6961127090668,12.0545041593587));
#55289=CARTESIAN_POINT('Ctrl Pts',(19.1757831508761,70.6440735240645,12.0894036875204));
#55290=CARTESIAN_POINT('Ctrl Pts',(19.1711279878911,70.5940431473507,12.1271218584828));
#55291=CARTESIAN_POINT('Ctrl Pts',(19.1664728249062,70.5463246698812,12.1673840725969));
#55292=CARTESIAN_POINT('Ctrl Pts',(19.1618680212956,70.4991224090686,12.2072107316248));
#55293=CARTESIAN_POINT('Ctrl Pts',(19.1572632176851,70.4539945476355,12.2496849530029));
#55294=CARTESIAN_POINT('Ctrl Pts',(19.1526584140745,70.4112518911924,12.2945625150071));
#55295=CARTESIAN_POINT('Ctrl Pts',(19.1480462880667,70.3684412668755,12.3395114397368));
#55296=CARTESIAN_POINT('Ctrl Pts',(19.1434341620589,70.3280238600468,12.3868710604633));
#55297=CARTESIAN_POINT('Ctrl Pts',(19.1388220360511,70.2902789032634,12.4363551631341));
#55298=CARTESIAN_POINT('Ctrl Pts',(19.1342294856661,70.2526941504803,12.4856292363898));
#55299=CARTESIAN_POINT('Ctrl Pts',(19.1296369352811,70.2177595391408,12.5370094069176));
#55300=CARTESIAN_POINT('Ctrl Pts',(19.1250443848961,70.1857124416265,12.590177820506));
#55301=CARTESIAN_POINT('Ctrl Pts',(19.1204545500048,70.1536842929931,12.6433147965536));
#55302=CARTESIAN_POINT('Ctrl Pts',(19.1158647151135,70.1245405333473,12.6982374852746));
#55303=CARTESIAN_POINT('Ctrl Pts',(19.1112748802221,70.0984750930454,12.7545992956089));
#55304=CARTESIAN_POINT('Ctrl Pts',(19.1066860900192,70.0724155854758,12.81094827748));
#55305=CARTESIAN_POINT('Ctrl Pts',(19.1020972998162,70.0494332186248,12.8687352705196));
#55306=CARTESIAN_POINT('Ctrl Pts',(19.0975085096132,70.0296749321915,12.9275911681626));
#55307=CARTESIAN_POINT('Ctrl Pts',(19.0928800829694,70.0097459802631,12.9869554434395));
#55308=CARTESIAN_POINT('Ctrl Pts',(19.0882516563256,69.9930972735942,13.0474066928886));
#55309=CARTESIAN_POINT('Ctrl Pts',(19.0836232296818,69.9798284057046,13.1085500036295));
#55310=CARTESIAN_POINT('Ctrl Pts',(19.0790287453758,69.9666568444012,13.1692449229259));
#55311=CARTESIAN_POINT('Ctrl Pts',(19.0744342610697,69.9568157404246,13.2306212706332));
#55312=CARTESIAN_POINT('Ctrl Pts',(19.0698397767637,69.9503507341686,13.2922844351097));
#55313=CARTESIAN_POINT('Ctrl Pts',(19.065194378951,69.9438140863272,13.3546309163049));
#55314=CARTESIAN_POINT('Ctrl Pts',(19.0605489811383,69.9407288640072,13.4172700805852));
#55315=CARTESIAN_POINT('Ctrl Pts',(19.0559035833256,69.9410881372469,13.4797933691354));
#55316=CARTESIAN_POINT('Ctrl Pts',(19.0512581855128,69.9414474104865,13.5423166576857));
#55317=CARTESIAN_POINT('Ctrl Pts',(19.0466127877001,69.9452510851302,13.6047235462825));
#55318=CARTESIAN_POINT('Ctrl Pts',(19.0419673898874,69.9524386089449,13.666612725928));
#55319=CARTESIAN_POINT('Ctrl Pts',(19.0373625663435,69.9595633548157,13.7279613473019));
#55320=CARTESIAN_POINT('Ctrl Pts',(19.0327577427996,69.9700410980345,13.7890430378238));
#55321=CARTESIAN_POINT('Ctrl Pts',(19.0281529192557,69.9838398718812,13.8494638009692));
#55322=CARTESIAN_POINT('Ctrl Pts',(19.0235407957396,69.9976605207607,13.9099803484349));
#55323=CARTESIAN_POINT('Ctrl Pts',(19.0189286722234,70.0148127251835,13.969833358198));
#55324=CARTESIAN_POINT('Ctrl Pts',(19.0143165487073,70.0352120763954,14.0286319774931));
#55325=CARTESIAN_POINT('Ctrl Pts',(19.0097239409176,70.0555251098499,14.0871817964759));
#55326=CARTESIAN_POINT('Ctrl Pts',(19.005131333128,70.0790577259536,14.1446856402258));
#55327=CARTESIAN_POINT('Ctrl Pts',(19.0005387253383,70.1056760189816,14.2007700718261));
#55328=CARTESIAN_POINT('Ctrl Pts',(18.9959488190682,70.1322786542737,14.2568215127606));
#55329=CARTESIAN_POINT('Ctrl Pts',(18.9913589127981,70.161963149739,14.311454740292));
#55330=CARTESIAN_POINT('Ctrl Pts',(18.986769006528,70.1945476521967,14.3643166667762));
#55331=CARTESIAN_POINT('Ctrl Pts',(18.9821801310537,70.2271248368648,14.4171667215906));
#55332=CARTESIAN_POINT('Ctrl Pts',(18.9775912555794,70.2626004692729,14.4682458339003));
#55333=CARTESIAN_POINT('Ctrl Pts',(18.9730023801051,70.3007479760522,14.517227659152));
#55334=CARTESIAN_POINT('Ctrl Pts',(18.9683740113354,70.339223792188,14.5666310372885));
#55335=CARTESIAN_POINT('Ctrl Pts',(18.9637456425657,70.3804173990726,14.6139004212703));
#55336=CARTESIAN_POINT('Ctrl Pts',(18.959117273796,70.4240545923065,14.6587347183901));
#55337=CARTESIAN_POINT('Ctrl Pts',(18.9545226708685,70.4673734343775,14.7032419309847));
#55338=CARTESIAN_POINT('Ctrl Pts',(18.9499280679409,70.5130999105703,14.7453491627486));
#55339=CARTESIAN_POINT('Ctrl Pts',(18.9453334650134,70.5609302450361,14.7848004358718));
#55340=CARTESIAN_POINT('Ctrl Pts',(18.9406882133226,70.6092878388378,14.82468660146));
#55341=CARTESIAN_POINT('Ctrl Pts',(18.9360429616318,70.6597955412824,14.8618575655445));
#55342=CARTESIAN_POINT('Ctrl Pts',(18.931397709941,70.7121089816365,14.8960935139892));
#55343=CARTESIAN_POINT('Ctrl Pts',(18.9267524582502,70.7644224219906,14.9303294624338));
#55344=CARTESIAN_POINT('Ctrl Pts',(18.9221072065594,70.8185411113404,14.9616301843882));
#55345=CARTESIAN_POINT('Ctrl Pts',(18.9174619548686,70.8740971202776,14.9898245633401));
#55346=CARTESIAN_POINT('Ctrl Pts',(18.912518049015,70.9332249557679,15.0198316252639));
#55347=CARTESIAN_POINT('Ctrl Pts',(18.9075741431615,70.9941931861682,15.046428425153));
#55348=CARTESIAN_POINT('Ctrl Pts',(18.9026302373079,71.0565973538058,15.0694018505162));
#55349=CARTESIAN_POINT('Ctrl Pts',(18.8977597888335,71.1180743098957,15.0920339328875));
#55350=CARTESIAN_POINT('Ctrl Pts',(18.892889340359,71.1809444334017,15.1111493959224));
#55351=CARTESIAN_POINT('Ctrl Pts',(18.8880188918845,71.2447962575595,15.1265903166271));
#55352=CARTESIAN_POINT('Ctrl Pts',(18.8830382573414,71.3100926266119,15.1423805633451));
#55353=CARTESIAN_POINT('Ctrl Pts',(18.8780576227984,71.376415286907,15.1543277305986));
#55354=CARTESIAN_POINT('Ctrl Pts',(18.8730769882553,71.4433035472524,15.1623155318636));
#55355=CARTESIAN_POINT('Ctrl Pts',(18.8680963537122,71.5101918075978,15.1703033331287));
#55356=CARTESIAN_POINT('Ctrl Pts',(18.8631157191691,71.5776452193343,15.1743316122925));
#55357=CARTESIAN_POINT('Ctrl Pts',(18.858135084626,71.6451886815825,15.1743399868995));
#55358=CARTESIAN_POINT('',(18.0643850846152,71.6466158347437,15.1743395663265));
#55359=CARTESIAN_POINT('Ctrl Pts',(18.8581350845702,71.6451886823392,15.1743399868996));
#55360=CARTESIAN_POINT('Ctrl Pts',(18.8533776934734,71.709704691929,15.1743479861089));
#55361=CARTESIAN_POINT('Ctrl Pts',(18.8486203023767,71.774167687991,15.1706883871686));
#55362=CARTESIAN_POINT('Ctrl Pts',(18.8438629112799,71.8381538247881,15.1634050899385));
#55363=CARTESIAN_POINT('Ctrl Pts',(18.8390945725359,71.9022872056611,15.1561050324783));
#55364=CARTESIAN_POINT('Ctrl Pts',(18.8343262337919,71.9659410868059,15.1451646747383));
#55365=CARTESIAN_POINT('Ctrl Pts',(18.8295578950479,72.0286995066004,15.1306794765517));
#55366=CARTESIAN_POINT('Ctrl Pts',(18.8247837352535,72.0915345400639,15.1161765952529));
#55367=CARTESIAN_POINT('Ctrl Pts',(18.8200095754591,72.1534715015155,15.0981203771717));
#55368=CARTESIAN_POINT('Ctrl Pts',(18.8152354156646,72.2141102507751,15.0766559949981));
#55369=CARTESIAN_POINT('Ctrl Pts',(18.8104493894206,72.2748997211437,15.0551382618645));
#55370=CARTESIAN_POINT('Ctrl Pts',(18.8056633631767,72.3343841154749,15.0301956123921));
#55371=CARTESIAN_POINT('Ctrl Pts',(18.8008773369327,72.392183944088,15.0020210757207));
#55372=CARTESIAN_POINT('Ctrl Pts',(18.7982370645717,72.424069956027,14.9864782335663));
#55373=CARTESIAN_POINT('Ctrl Pts',(18.7955967922108,72.4554437540396,14.9699526329256));
#55374=CARTESIAN_POINT('Ctrl Pts',(18.7929565198498,72.4862453494548,14.9524823553419));
#55375=CARTESIAN_POINT('Ctrl Pts',(18.7883522396236,72.5399591930735,14.9220165387032));
#55376=CARTESIAN_POINT('Ctrl Pts',(18.7837479593973,72.5921212668839,14.8885675029417));
#55377=CARTESIAN_POINT('Ctrl Pts',(18.7791436791711,72.6423812110903,14.8523180894182));
#55378=CARTESIAN_POINT('Ctrl Pts',(18.7745314877402,72.6927275133553,14.8160063911266));
#55379=CARTESIAN_POINT('Ctrl Pts',(18.7699192963094,72.7411646753013,14.7768848943094));
#55380=CARTESIAN_POINT('Ctrl Pts',(18.7653071048786,72.7873655229722,14.73518361511));
#55381=CARTESIAN_POINT('Ctrl Pts',(18.7607150744532,72.8333644155519,14.6936646222985));
#55382=CARTESIAN_POINT('Ctrl Pts',(18.7561230440278,72.87714610762,14.6495886741211));
#55383=CARTESIAN_POINT('Ctrl Pts',(18.7515310136024,72.9184188786279,14.6032245012605));
#55384=CARTESIAN_POINT('Ctrl Pts',(18.7469416958328,72.9596672685202,14.5568877171656));
#55385=CARTESIAN_POINT('Ctrl Pts',(18.7423523780633,72.9984093401351,14.5082657672341));
#55386=CARTESIAN_POINT('Ctrl Pts',(18.7377630602938,73.0343907899462,14.4576636173539));
#55387=CARTESIAN_POINT('Ctrl Pts',(18.7331747834526,73.0703640786072,14.4070729448251));
#55388=CARTESIAN_POINT('Ctrl Pts',(18.7285865066114,73.1035776951015,14.3545033773746));
#55389=CARTESIAN_POINT('Ctrl Pts',(18.7239982297702,73.1338193861151,14.3002906519025));
#55390=CARTESIAN_POINT('Ctrl Pts',(18.7193693010253,73.1643290170015,14.2455976043891));
#55391=CARTESIAN_POINT('Ctrl Pts',(18.7147403722804,73.1918135140614,14.189232578808));
#55392=CARTESIAN_POINT('Ctrl Pts',(18.7101114435354,73.2161023138299,14.1315656255653));
#55393=CARTESIAN_POINT('Ctrl Pts',(18.7055174572231,73.2402077645351,14.0743339833283));
#55394=CARTESIAN_POINT('Ctrl Pts',(18.7009234709108,73.2611654804613,14.0158205052203));
#55395=CARTESIAN_POINT('Ctrl Pts',(18.6963294845985,73.2788581046431,13.9564046216635));
#55396=CARTESIAN_POINT('Ctrl Pts',(18.6916830846372,73.2967525872828,13.8963108511804));
#55397=CARTESIAN_POINT('Ctrl Pts',(18.687036684676,73.3113068618472,13.8352944667737));
#55398=CARTESIAN_POINT('Ctrl Pts',(18.6823902847148,73.3224526273905,13.7737586551238));
#55399=CARTESIAN_POINT('Ctrl Pts',(18.6777438847535,73.3335983929338,13.7122228434739));
#55400=CARTESIAN_POINT('Ctrl Pts',(18.6730974847923,73.3413356457848,13.6501681381785));
#55401=CARTESIAN_POINT('Ctrl Pts',(18.6684510848311,73.3456501962626,13.5880004479189));
#55402=CARTESIAN_POINT('Ctrl Pts',(18.6638468640006,73.3499255800758,13.5263971040692));
#55403=CARTESIAN_POINT('Ctrl Pts',(18.6592426431701,73.3508570957658,13.4644393755095));
#55404=CARTESIAN_POINT('Ctrl Pts',(18.6546384223397,73.3484036191377,13.402520308211));
#55405=CARTESIAN_POINT('Ctrl Pts',(18.6500262234844,73.3459458912153,13.3404939498256));
#55406=CARTESIAN_POINT('Ctrl Pts',(18.6454140246291,73.3400913468835,13.2785068938624));
#55407=CARTESIAN_POINT('Ctrl Pts',(18.6408018257738,73.3308509946095,13.2169589354079));
#55408=CARTESIAN_POINT('Ctrl Pts',(18.6362098527738,73.3216511640115,13.1556808829443));
#55409=CARTESIAN_POINT('Ctrl Pts',(18.6316178797738,73.3090952070524,13.0948385923167));
#55410=CARTESIAN_POINT('Ctrl Pts',(18.6270259067737,73.2932459881658,13.0348236737988));
#55411=CARTESIAN_POINT('Ctrl Pts',(18.6224366455156,73.2774061288703,12.974844196466));
#55412=CARTESIAN_POINT('Ctrl Pts',(18.6178473842574,73.2582769938693,12.9156916116504));
#55413=CARTESIAN_POINT('Ctrl Pts',(18.6132581229993,73.23597232155,12.8577463552424));
#55414=CARTESIAN_POINT('Ctrl Pts',(18.6086699016529,73.2136727033977,12.799814229043));
#55415=CARTESIAN_POINT('Ctrl Pts',(18.6040816803066,73.1881991589405,12.7430893610911));
#55416=CARTESIAN_POINT('Ctrl Pts',(18.5994934589603,73.1597143048886,12.6879341321795));
#55417=CARTESIAN_POINT('Ctrl Pts',(18.5948644748646,73.1309763852414,12.6322888923026));
#55418=CARTESIAN_POINT('Ctrl Pts',(18.590235490769,73.0991735938314,12.5782418013657));
#55419=CARTESIAN_POINT('Ctrl Pts',(18.5856065066733,73.0645201952379,12.5261394663045));
#55420=CARTESIAN_POINT('Ctrl Pts',(18.5810125726861,73.030129187993,12.4744316438312));
#55421=CARTESIAN_POINT('Ctrl Pts',(18.5764186386989,72.9929309481254,12.4246396047205));
#55422=CARTESIAN_POINT('Ctrl Pts',(18.5718247047117,72.9531769349122,12.3770707597875));
#55423=CARTESIAN_POINT('Ctrl Pts',(18.5671781955618,72.9129679578885,12.3289575143976));
#55424=CARTESIAN_POINT('Ctrl Pts',(18.5625316864119,72.8701446873665,12.2831190737208));
#55425=CARTESIAN_POINT('Ctrl Pts',(18.557885177262,72.8250055143118,12.2398351060914));
#55426=CARTESIAN_POINT('Ctrl Pts',(18.5532386681121,72.7798663412571,12.196551138462));
#55427=CARTESIAN_POINT('Ctrl Pts',(18.5485921589622,72.7324117085443,12.1558219417343));
#55428=CARTESIAN_POINT('Ctrl Pts',(18.5439456498123,72.6829721695382,12.1178835743178));
#55429=CARTESIAN_POINT('Ctrl Pts',(18.5393415477255,72.6339838479048,12.0802914571052));
#55430=CARTESIAN_POINT('Ctrl Pts',(18.5347374456387,72.5828530488402,12.0452907683919));
#55431=CARTESIAN_POINT('Ctrl Pts',(18.5301333435519,72.5298846624105,12.0131329101251));
#55432=CARTESIAN_POINT('Ctrl Pts',(18.5255211298536,72.4768229550764,11.9809183954144));
#55433=CARTESIAN_POINT('Ctrl Pts',(18.5209089161553,72.4219175562888,11.9515570867998));
#55434=CARTESIAN_POINT('Ctrl Pts',(18.5162967024571,72.3655078129013,11.9252606778493));
#55435=CARTESIAN_POINT('Ctrl Pts',(18.5117048541812,72.309347149094,11.8990803817919));
#55436=CARTESIAN_POINT('Ctrl Pts',(18.5071130059053,72.2516958474173,11.8759382160423));
#55437=CARTESIAN_POINT('Ctrl Pts',(18.5025211576295,72.1929150497117,11.8559981084462));
#55438=CARTESIAN_POINT('Ctrl Pts',(18.4979320229831,72.134168989501,11.83606978479));
#55439=CARTESIAN_POINT('Ctrl Pts',(18.4933428883367,72.0742952364289,11.8193399290415));
#55440=CARTESIAN_POINT('Ctrl Pts',(18.4887537536904,72.0136737223021,11.8059238896428));
#55441=CARTESIAN_POINT('Ctrl Pts',(18.4841656606265,71.9530659672642,11.7925108952435));
#55442=CARTESIAN_POINT('Ctrl Pts',(18.4795775675627,71.8917112831891,11.7824103331851));
#55443=CARTESIAN_POINT('Ctrl Pts',(18.4749894744989,71.830001553527,11.7756868347217));
#55444=CARTESIAN_POINT('Ctrl Pts',(18.4703603695234,71.7677402147445,11.7689032364475));
#55445=CARTESIAN_POINT('Ctrl Pts',(18.465731264548,71.7051179685949,11.7655574681876));
#55446=CARTESIAN_POINT('Ctrl Pts',(18.4611021595725,71.6425421472726,11.7656623960383));
#55447=CARTESIAN_POINT('Ctrl Pts',(18.4565083564861,71.580443533685,11.7657665237017));
#55448=CARTESIAN_POINT('Ctrl Pts',(18.4519145533996,71.5183911493209,11.769268812178));
#55449=CARTESIAN_POINT('Ctrl Pts',(18.4473207503132,71.4567801341243,11.7761294672269));
#55450=CARTESIAN_POINT('Ctrl Pts',(18.4426739943933,71.3944589278792,11.7830692051441));
#55451=CARTESIAN_POINT('Ctrl Pts',(18.4380272384733,71.332589859076,11.7934451581334));
#55452=CARTESIAN_POINT('Ctrl Pts',(18.4333804825534,71.271570963609,11.8071630605646));
#55453=CARTESIAN_POINT('Ctrl Pts',(18.4287337266334,71.2105520681421,11.8208809629957));
#55454=CARTESIAN_POINT('Ctrl Pts',(18.4240869707134,71.1503838391696,11.8379406101307));
#55455=CARTESIAN_POINT('Ctrl Pts',(18.4194402147935,71.0914457198719,11.8581968199784));
#55456=CARTESIAN_POINT('Ctrl Pts',(18.4148360342462,71.0330476143894,11.878267434607));
#55457=CARTESIAN_POINT('Ctrl Pts',(18.4102318536989,70.9756262702442,11.9015555791544));
#55458=CARTESIAN_POINT('Ctrl Pts',(18.4056276731516,70.9195596795308,11.9279459591891));
#55459=CARTESIAN_POINT('Ctrl Pts',(18.4010154692609,70.8633953859784,11.9543823276639));
#55460=CARTESIAN_POINT('Ctrl Pts',(18.3964032653702,70.8085910710518,11.9839316321461));
#55461=CARTESIAN_POINT('Ctrl Pts',(18.3917910614795,70.755510637495,12.0164279315767));
#55462=CARTESIAN_POINT('Ctrl Pts',(18.3871991319811,70.7026635356731,12.0487813833058));
#55463=CARTESIAN_POINT('Ctrl Pts',(18.3826072024828,70.6515256397942,12.0840557332596));
#55464=CARTESIAN_POINT('Ctrl Pts',(18.3780152729844,70.6024330954231,12.1220404785168));
#55465=CARTESIAN_POINT('Ctrl Pts',(18.3734260563137,70.5533695540264,12.1600027830834));
#55466=CARTESIAN_POINT('Ctrl Pts',(18.3688368396431,70.5063493680446,12.2006719975531));
#55467=CARTESIAN_POINT('Ctrl Pts',(18.3642476229724,70.4616785664782,12.2437951217594));
#55468=CARTESIAN_POINT('Ctrl Pts',(18.3596594472243,70.4170178971089,12.2869084648116));
#55469=CARTESIAN_POINT('Ctrl Pts',(18.3550712714763,70.3747059186949,12.3324742602312));
#55470=CARTESIAN_POINT('Ctrl Pts',(18.3504830957282,70.3350129845232,12.3802015299746));
#55471=CARTESIAN_POINT('Ctrl Pts',(18.3458540693988,70.2949666464002,12.4283537369533));
#55472=CARTESIAN_POINT('Ctrl Pts',(18.3412250430693,70.2575865832869,12.4787057181409));
#55473=CARTESIAN_POINT('Ctrl Pts',(18.3365960167399,70.2231085072819,12.5309250587191));
#55474=CARTESIAN_POINT('Ctrl Pts',(18.3320021303128,70.188892161528,12.5827479914142));
#55475=CARTESIAN_POINT('Ctrl Pts',(18.3274082438856,70.1575341048607,12.6364095570815));
#55476=CARTESIAN_POINT('Ctrl Pts',(18.3228143574585,70.1292194430487,12.6915583809155));
#55477=CARTESIAN_POINT('Ctrl Pts',(18.3181677611779,70.1005799012685,12.7473399775601));
#55478=CARTESIAN_POINT('Ctrl Pts',(18.3135211648973,70.075054270936,12.8046427001273));
#55479=CARTESIAN_POINT('Ctrl Pts',(18.3088745686167,70.052783830391,12.8630827305967));
#55480=CARTESIAN_POINT('Ctrl Pts',(18.304227972336,70.030513389846,12.9215227610661));
#55481=CARTESIAN_POINT('Ctrl Pts',(18.2995813760554,70.0114982408165,12.9810995754133));
#55482=CARTESIAN_POINT('Ctrl Pts',(18.2949347797748,69.9958269593481,13.0414167301978));
#55483=CARTESIAN_POINT('Ctrl Pts',(18.2903306132046,69.9802987778814,13.1011831077552));
#55484=CARTESIAN_POINT('Ctrl Pts',(18.2857264466345,69.9679922107812,13.1619126164308));
#55485=CARTESIAN_POINT('Ctrl Pts',(18.2811222800644,69.9590199518388,13.2232264828556));
#55486=CARTESIAN_POINT('Ctrl Pts',(18.2765100744265,69.9500320269564,13.2846474058598));
#55487=CARTESIAN_POINT('Ctrl Pts',(18.2718978687887,69.9443902391824,13.3466542458907));
#55488=CARTESIAN_POINT('Ctrl Pts',(18.2672856631508,69.9421572818739,13.4088519930779));
#55489=CARTESIAN_POINT('Ctrl Pts',(18.2626937476903,69.9399341478698,13.4707761177468));
#55490=CARTESIAN_POINT('Ctrl Pts',(18.2581018322298,69.9410899606479,13.5328889657477));
#55491=CARTESIAN_POINT('Ctrl Pts',(18.2535099167693,69.9456349339227,13.594794053317));
#55492=CARTESIAN_POINT('Ctrl Pts',(18.2489207141178,69.950177222121,13.6566625686368));
#55493=CARTESIAN_POINT('Ctrl Pts',(18.2443315114663,69.9581046628539,13.7183230621107));
#55494=CARTESIAN_POINT('Ctrl Pts',(18.2397423088148,69.969375408636,13.7793806793307));
#55495=CARTESIAN_POINT('Ctrl Pts',(18.2351541470425,69.980643598095,13.8404244480443));
#55496=CARTESIAN_POINT('Ctrl Pts',(18.2305659852702,69.9952534947683,13.9008651135017));
#55497=CARTESIAN_POINT('Ctrl Pts',(18.2259778234979,70.0131118863953,13.9603165811849));
#55498=CARTESIAN_POINT('Ctrl Pts',(18.2213487836027,70.0311293869559,14.0202977303658));
#55499=CARTESIAN_POINT('Ctrl Pts',(18.2167197437076,70.0524534378522,14.079271455703));
#55500=CARTESIAN_POINT('Ctrl Pts',(18.2120907038124,70.0769371474875,14.1368576428956));
#55501=CARTESIAN_POINT('Ctrl Pts',(18.2074968310886,70.1012348525017,14.1940063434048));
#55502=CARTESIAN_POINT('Ctrl Pts',(18.2029029583647,70.1286440947259,14.2497880797131));
#55503=CARTESIAN_POINT('Ctrl Pts',(18.1983090856409,70.1589742257078,14.3038544555975));
#55504=CARTESIAN_POINT('Ctrl Pts',(18.1936624621601,70.1896526330711,14.358541667632));
#55505=CARTESIAN_POINT('Ctrl Pts',(18.1890158386793,70.2233191661855,14.4114734152918));
#55506=CARTESIAN_POINT('Ctrl Pts',(18.1843692151985,70.2597319159975,14.4623199063693));
#55507=CARTESIAN_POINT('Ctrl Pts',(18.1797225917176,70.2961446658095,14.5131663974469));
#55508=CARTESIAN_POINT('Ctrl Pts',(18.1750759682368,70.3353032516732,14.5619272576588));
#55509=CARTESIAN_POINT('Ctrl Pts',(18.170429344756,70.3769261265954,14.6083096538684));
#55510=CARTESIAN_POINT('Ctrl Pts',(18.1658930358871,70.4175608406918,14.6535908943545));
#55511=CARTESIAN_POINT('Ctrl Pts',(18.1613567270183,70.4607151649762,14.6967956968842));
#55512=CARTESIAN_POINT('Ctrl Pts',(18.1568204181494,70.5061456764191,14.7376255053454));
#55513=CARTESIAN_POINT('Ctrl Pts',(18.1522901777964,70.5515154125083,14.7784006931129));
#55514=CARTESIAN_POINT('Ctrl Pts',(18.1477599374433,70.5991549214016,14.8168068308777));
#55515=CARTESIAN_POINT('Ctrl Pts',(18.1432296970902,70.6487820235391,14.8525799957308));
#55516=CARTESIAN_POINT('Ctrl Pts',(18.1387037497788,70.6983620969985,14.8883192604652));
#55517=CARTESIAN_POINT('Ctrl Pts',(18.1341778024674,70.7499256102087,14.9214301901394));
#55518=CARTESIAN_POINT('Ctrl Pts',(18.1296518551559,70.8031568754621,14.9516886834854));
#55519=CARTESIAN_POINT('Ctrl Pts',(18.125128431986,70.8563584533952,14.9819303015311));
#55520=CARTESIAN_POINT('Ctrl Pts',(18.1206050088161,70.9112254852309,15.0093223788357));
#55521=CARTESIAN_POINT('Ctrl Pts',(18.1160815856462,70.9674147263675,15.0336850080299));
#55522=CARTESIAN_POINT('Ctrl Pts',(18.1115565317005,71.023624224741,15.0580564203922));
#55523=CARTESIAN_POINT('Ctrl Pts',(18.1070314777548,71.0811564091793,15.0793959821789));
#55524=CARTESIAN_POINT('Ctrl Pts',(18.1025064238091,71.1396464212039,15.0975712436434));
#55525=CARTESIAN_POINT('Ctrl Pts',(18.0979807351458,71.1981446374715,15.1157490545049));
#55526=CARTESIAN_POINT('Ctrl Pts',(18.0934550464825,71.2576004434866,15.1307615418621));
#55527=CARTESIAN_POINT('Ctrl Pts',(18.0889293578192,71.317634974436,15.1425265090925));
#55528=CARTESIAN_POINT('Ctrl Pts',(18.0843973318221,71.3777535718965,15.1543079508373));
#55529=CARTESIAN_POINT('Ctrl Pts',(18.0798653058251,71.4384519944004,15.1628327089221));
#55530=CARTESIAN_POINT('Ctrl Pts',(18.0753332798281,71.4993436244346,15.1680701901737));
#55531=CARTESIAN_POINT('Ctrl Pts',(18.0716838814238,71.5483764008631,15.1722876540045));
#55532=CARTESIAN_POINT('Ctrl Pts',(18.0680344830195,71.5975342312904,15.1743745799587));
#55533=CARTESIAN_POINT('Ctrl Pts',(18.0643850846152,71.6466158347437,15.1743395663265));
#55534=CARTESIAN_POINT('',(17.2706350845291,71.6439433034762,15.1743393774819));
#55535=CARTESIAN_POINT('Ctrl Pts',(18.0643850845702,71.6466158353495,15.174339566326));
#55536=CARTESIAN_POINT('Ctrl Pts',(18.0582313596258,71.7293787058325,15.1742805252608));
#55537=CARTESIAN_POINT('Ctrl Pts',(18.0520776346815,71.8119254455953,15.168191932043));
#55538=CARTESIAN_POINT('Ctrl Pts',(18.0459239097372,71.8935789255846,15.1561737919016));
#55539=CARTESIAN_POINT('Ctrl Pts',(18.0413197449804,71.9546713660552,15.1471819214845));
#55540=CARTESIAN_POINT('Ctrl Pts',(18.0367155802237,72.0153952534079,15.1348478116356));
#55541=CARTESIAN_POINT('Ctrl Pts',(18.0321114154669,72.0753578439467,15.1192152946261));
#55542=CARTESIAN_POINT('Ctrl Pts',(18.0274992096024,72.1354251582903,15.1035554756498));
#55543=CARTESIAN_POINT('Ctrl Pts',(18.0228870037379,72.1947280011364,15.0845857452346));
#55544=CARTESIAN_POINT('Ctrl Pts',(18.0182747978734,72.2528781616959,15.0624023105555));
#55545=CARTESIAN_POINT('Ctrl Pts',(18.0136828845006,72.3107724768554,15.0403164771498));
#55546=CARTESIAN_POINT('Ctrl Pts',(18.0090909711279,72.3675237460416,15.0150453146395));
#55547=CARTESIAN_POINT('Ctrl Pts',(18.0044990577551,72.4227628540532,14.9867339347223));
#55548=CARTESIAN_POINT('Ctrl Pts',(17.9999098572888,72.4779693267521,14.9584392811928));
#55549=CARTESIAN_POINT('Ctrl Pts',(17.9953206568224,72.5316649595835,14.9271082033252));
#55550=CARTESIAN_POINT('Ctrl Pts',(17.990731456356,72.58350242719,14.8929331227082));
#55551=CARTESIAN_POINT('Ctrl Pts',(17.9861432968626,72.6353281364512,14.8587657940595));
#55552=CARTESIAN_POINT('Ctrl Pts',(17.9815551373692,72.6852960942193,14.821756022743));
#55553=CARTESIAN_POINT('Ctrl Pts',(17.9769669778758,72.7330870603228,14.7821401199591));
#55554=CARTESIAN_POINT('Ctrl Pts',(17.972337935946,72.7813038640928,14.7421712227713));
#55555=CARTESIAN_POINT('Ctrl Pts',(17.9677088940163,72.8273042616491,14.6995498271725));
#55556=CARTESIAN_POINT('Ctrl Pts',(17.9630798520865,72.8707954393377,14.654559349653));
#55557=CARTESIAN_POINT('Ctrl Pts',(17.9584859818468,72.9139561689018,14.6099107120125));
#55558=CARTESIAN_POINT('Ctrl Pts',(17.9538921116071,72.9546453847161,14.5629292956482));
#55559=CARTESIAN_POINT('Ctrl Pts',(17.9492982413675,72.992616537172,14.5139264521844));
#55560=CARTESIAN_POINT('Ctrl Pts',(17.9446516135926,73.0310237629836,14.4643608437529));
#55561=CARTESIAN_POINT('Ctrl Pts',(17.9400049858178,73.0666497805645,14.412727510831));
#55562=CARTESIAN_POINT('Ctrl Pts',(17.935358358043,73.0992851498073,14.3593777638157));
#55563=CARTESIAN_POINT('Ctrl Pts',(17.9307117302681,73.1319205190501,14.3060280168005));
#55564=CARTESIAN_POINT('Ctrl Pts',(17.9260651024933,73.1615650436088,14.2509623521114));
#55565=CARTESIAN_POINT('Ctrl Pts',(17.9214184747185,73.1880587682366,14.1945541804328));
#55566=CARTESIAN_POINT('Ctrl Pts',(17.9168143123683,73.2143103673228,14.1386615217411));
#55567=CARTESIAN_POINT('Ctrl Pts',(17.9122101500181,73.2375723488741,14.0812298510895));
#55568=CARTESIAN_POINT('Ctrl Pts',(17.9076059876679,73.2576643014475,14.0226107652569));
#55569=CARTESIAN_POINT('Ctrl Pts',(17.9029937815025,73.2777913561613,13.9638892675077));
#55570=CARTESIAN_POINT('Ctrl Pts',(17.8983815753372,73.2947370347143,13.903976644647));
#55571=CARTESIAN_POINT('Ctrl Pts',(17.8937693691718,73.3083670882121,13.8432496471843));
#55572=CARTESIAN_POINT('Ctrl Pts',(17.8891774582468,73.3219371649438,13.782789868697));
#55573=CARTESIAN_POINT('Ctrl Pts',(17.8845855473217,73.3322205966582,13.7215233581769));
#55574=CARTESIAN_POINT('Ctrl Pts',(17.8799936363967,73.3391344489828,13.6598379622963));
#55575=CARTESIAN_POINT('Ctrl Pts',(17.8754044383863,73.3460442165829,13.5981890103313));
#55576=CARTESIAN_POINT('Ctrl Pts',(17.8708152403759,73.3495882965235,13.5361221668568));
#55577=CARTESIAN_POINT('Ctrl Pts',(17.8662260423655,73.3497352277371,13.4740332486111));
#55578=CARTESIAN_POINT('Ctrl Pts',(17.861637885332,73.3498821256219,13.4119584141191));
#55579=CARTESIAN_POINT('Ctrl Pts',(17.8570497282986,73.3466334037854,13.3498620217563));
#55580=CARTESIAN_POINT('Ctrl Pts',(17.8524615712652,73.3400097008886,13.2881407212866));
#55581=CARTESIAN_POINT('Ctrl Pts',(17.8478325269681,73.3333269710045,13.2258693927622));
#55582=CARTESIAN_POINT('Ctrl Pts',(17.8432034826709,73.3232088298502,13.1639803994117));
#55583=CARTESIAN_POINT('Ctrl Pts',(17.8385744383738,73.3097297803731,13.1028743842182));
#55584=CARTESIAN_POINT('Ctrl Pts',(17.8339805705749,73.2963531593303,13.0422327187901));
#55585=CARTESIAN_POINT('Ctrl Pts',(17.8293867027759,73.2796667272973,12.9823626523723));
#55586=CARTESIAN_POINT('Ctrl Pts',(17.824792834977,73.2597938292486,12.9236416929487));
#55587=CARTESIAN_POINT('Ctrl Pts',(17.8201462024308,73.2396926729023,12.8642462699315));
#55588=CARTESIAN_POINT('Ctrl Pts',(17.8154995698846,73.2163315668755,12.8060270196675));
#55589=CARTESIAN_POINT('Ctrl Pts',(17.8108529373383,73.1898876650216,12.7493525909322));
#55590=CARTESIAN_POINT('Ctrl Pts',(17.8062063047921,73.1634437631677,12.692678162197));
#55591=CARTESIAN_POINT('Ctrl Pts',(17.8015596722459,73.1339173708365,12.637548992884));
#55592=CARTESIAN_POINT('Ctrl Pts',(17.7969130396997,73.1015313997032,12.5843046898631));
#55593=CARTESIAN_POINT('Ctrl Pts',(17.7923088783088,73.0694414428552,12.5315470504733));
#55594=CARTESIAN_POINT('Ctrl Pts',(17.787704716918,73.0344171462522,12.4804313641601));
#55595=CARTESIAN_POINT('Ctrl Pts',(17.7831005555272,72.9966519366625,12.4313022387308));
#55596=CARTESIAN_POINT('Ctrl Pts',(17.7784883492419,72.9588207395676,12.3820872695193));
#55597=CARTESIAN_POINT('Ctrl Pts',(17.7738761429566,72.9182392675481,12.3348662716024));
#55598=CARTESIAN_POINT('Ctrl Pts',(17.7692639366714,72.8751474151999,12.2899592674788));
#55599=CARTESIAN_POINT('Ctrl Pts',(17.7646720267685,72.8322451919921,12.245249880216));
#55600=CARTESIAN_POINT('Ctrl Pts',(17.7600801168656,72.7868549688105,12.2028345500411));
#55601=CARTESIAN_POINT('Ctrl Pts',(17.7554882069628,72.7392542355005,12.1629966537619));
#55602=CARTESIAN_POINT('Ctrl Pts',(17.7508990099952,72.6916816250661,12.123182294015));
#55603=CARTESIAN_POINT('Ctrl Pts',(17.7463098130277,72.6419014827485,12.0859426730579));
#55604=CARTESIAN_POINT('Ctrl Pts',(17.7417206160601,72.5902263756589,12.0515226630435));
#55605=CARTESIAN_POINT('Ctrl Pts',(17.7371324600885,72.538562990353,12.0171104607326));
#55606=CARTESIAN_POINT('Ctrl Pts',(17.7325443041168,72.4850059157838,11.9855168803209));
#55607=CARTESIAN_POINT('Ctrl Pts',(17.7279561481451,72.4298971930433,11.956943824669));
#55608=CARTESIAN_POINT('Ctrl Pts',(17.7233271028564,72.3742973453172,11.928116127994));
#55609=CARTESIAN_POINT('Ctrl Pts',(17.7186980575677,72.3171185046177,11.9023633335533));
#55610=CARTESIAN_POINT('Ctrl Pts',(17.7140690122791,72.2587357955364,11.8798446498805));
#55611=CARTESIAN_POINT('Ctrl Pts',(17.7094751455761,72.2007967678215,11.8574970977036));
#55612=CARTESIAN_POINT('Ctrl Pts',(17.7048812788732,72.1416726131983,11.8383347737319));
#55613=CARTESIAN_POINT('Ctrl Pts',(17.7002874121703,72.0817461508561,11.8224633927487));
#55614=CARTESIAN_POINT('Ctrl Pts',(17.6956407775887,72.0211313376109,11.8064097036665));
#55615=CARTESIAN_POINT('Ctrl Pts',(17.6909941430072,71.9596961851791,11.7937231678153));
#55616=CARTESIAN_POINT('Ctrl Pts',(17.6863475084256,71.8978458523827,11.7844597521225));
#55617=CARTESIAN_POINT('Ctrl Pts',(17.681700873844,71.8359955195862,11.7751963364298));
#55618=CARTESIAN_POINT('Ctrl Pts',(17.6770542392624,71.7737305401214,11.7693560282505));
#55619=CARTESIAN_POINT('Ctrl Pts',(17.6724076046809,71.711457140305,11.766940608841));
#55620=CARTESIAN_POINT('Ctrl Pts',(17.6678034421943,71.6497529442226,11.7645472673292));
#55621=CARTESIAN_POINT('Ctrl Pts',(17.6631992797078,71.5877965422259,11.7655069489137));
#55622=CARTESIAN_POINT('Ctrl Pts',(17.6585951172212,71.5259820415606,11.7698487753137));
#55623=CARTESIAN_POINT('Ctrl Pts',(17.6539829110729,71.4640595484134,11.7741981870636));
#55624=CARTESIAN_POINT('Ctrl Pts',(17.6493707049246,71.4022799622413,11.7819416392346));
#55625=CARTESIAN_POINT('Ctrl Pts',(17.6447584987763,71.3410425645745,11.7930559379928));
#55626=CARTESIAN_POINT('Ctrl Pts',(17.6401665877339,71.2800746300298,11.8041213304657));
#55627=CARTESIAN_POINT('Ctrl Pts',(17.6355746766914,71.2196446281494,11.8185279025853));
#55628=CARTESIAN_POINT('Ctrl Pts',(17.630982765649,71.1601420609145,11.8362008788855));
#55629=CARTESIAN_POINT('Ctrl Pts',(17.6263935675287,71.1006746480699,11.85386341391));
#55630=CARTESIAN_POINT('Ctrl Pts',(17.6218043694085,71.042134068444,11.8747883817577));
#55631=CARTESIAN_POINT('Ctrl Pts',(17.6172151712882,70.9848971036271,11.8988504974118));
#55632=CARTESIAN_POINT('Ctrl Pts',(17.6126270141526,70.9276731220817,11.9229071549676));
#55633=CARTESIAN_POINT('Ctrl Pts',(17.608038857017,70.871752635484,11.9500993507606));
#55634=CARTESIAN_POINT('Ctrl Pts',(17.6034506998815,70.8174928881701,11.9802534947913));
#55635=CARTESIAN_POINT('Ctrl Pts',(17.5988216556965,70.7627496088187,12.0106763554199));
#55636=CARTESIAN_POINT('Ctrl Pts',(17.5941926115116,70.7096972901596,12.0441139932849));
#55637=CARTESIAN_POINT('Ctrl Pts',(17.5895635673266,70.6586758618685,12.0803416567988));
#55638=CARTESIAN_POINT('Ctrl Pts',(17.5849696994459,70.6080421475871,12.1162940247525));
#55639=CARTESIAN_POINT('Ctrl Pts',(17.5803758315651,70.5594089306551,12.1549937960996));
#55640=CARTESIAN_POINT('Ctrl Pts',(17.5757819636844,70.513075800205,12.1961802552329));
#55641=CARTESIAN_POINT('Ctrl Pts',(17.5711353313473,70.4662104945812,12.2378397756686));
#55642=CARTESIAN_POINT('Ctrl Pts',(17.5664886990103,70.4216988390947,12.2820431089427));
#55643=CARTESIAN_POINT('Ctrl Pts',(17.5618420666732,70.3798112935905,12.328483437786));
#55644=CARTESIAN_POINT('Ctrl Pts',(17.5571954343362,70.3379237480864,12.3749237666293));
#55645=CARTESIAN_POINT('Ctrl Pts',(17.5525488019991,70.2986605968331,12.4236006391787));
#55646=CARTESIAN_POINT('Ctrl Pts',(17.5479021696621,70.2622477212206,12.474176416574));
#55647=CARTESIAN_POINT('Ctrl Pts',(17.5432980075383,70.2261676592415,12.5242899314329));
#55648=CARTESIAN_POINT('Ctrl Pts',(17.5386938454145,70.19274330371,12.5764658699009));
#55649=CARTESIAN_POINT('Ctrl Pts',(17.5340896832906,70.1622166324098,12.6303917975009));
#55650=CARTESIAN_POINT('Ctrl Pts',(17.529477477097,70.1316366270462,12.6844119407072));
#55651=CARTESIAN_POINT('Ctrl Pts',(17.5248652709034,70.1039647779175,12.7401878061276));
#55652=CARTESIAN_POINT('Ctrl Pts',(17.5202530647097,70.079402311737,12.7973737472007));
#55653=CARTESIAN_POINT('Ctrl Pts',(17.5156611540387,70.0549479300753,12.8543080476249));
#55654=CARTESIAN_POINT('Ctrl Pts',(17.5110692433677,70.033575850036,12.9126395832101));
#55655=CARTESIAN_POINT('Ctrl Pts',(17.5064773326966,70.01543889853,12.9720023661757));
#55656=CARTESIAN_POINT('Ctrl Pts',(17.5018881349499,69.9973126624277,13.0313300773053));
#55657=CARTESIAN_POINT('Ctrl Pts',(17.4972989372032,69.9824179121745,13.0916873434003));
#55658=CARTESIAN_POINT('Ctrl Pts',(17.4927097394565,69.9708583441007,13.1526908790182));
#55659=CARTESIAN_POINT('Ctrl Pts',(17.488121582696,69.9593013981304,13.2136805769583));
#55660=CARTESIAN_POINT('Ctrl Pts',(17.4835334259355,69.9510782264169,13.2753157552192));
#55661=CARTESIAN_POINT('Ctrl Pts',(17.478945269175,69.9462414668071,13.3372027309104));
#55662=CARTESIAN_POINT('Ctrl Pts',(17.4743162246307,69.9413616039661,13.3996412181158));
#55663=CARTESIAN_POINT('Ctrl Pts',(17.4696871800864,69.9399288858088,13.4623354931853));
#55664=CARTESIAN_POINT('Ctrl Pts',(17.4650581355421,69.9419437382228,13.5248780449002));
#55665=CARTESIAN_POINT('Ctrl Pts',(17.4604642680357,69.9439432793692,13.5869453232204));
#55666=CARTESIAN_POINT('Ctrl Pts',(17.4558704005294,69.9493380718814,13.6488626690757));
#55667=CARTESIAN_POINT('Ctrl Pts',(17.451276533023,69.9580762787708,13.7102363323419));
#55668=CARTESIAN_POINT('Ctrl Pts',(17.4466298999597,69.9669148534553,13.7723149387781));
#55669=CARTESIAN_POINT('Ctrl Pts',(17.4419832668965,69.979174050854,13.8338367681197));
#55670=CARTESIAN_POINT('Ctrl Pts',(17.4373366338332,69.9947475134842,13.8944068853816));
#55671=CARTESIAN_POINT('Ctrl Pts',(17.4326900007699,70.0103209761145,13.9549770026436));
#55672=CARTESIAN_POINT('Ctrl Pts',(17.4280433677066,70.0292084843387,14.0145949212571));
#55673=CARTESIAN_POINT('Ctrl Pts',(17.4233967346434,70.0512533634033,14.0728858404604));
#55674=CARTESIAN_POINT('Ctrl Pts',(17.4187925725859,70.0730967485747,14.1306439708823));
#55675=CARTESIAN_POINT('Ctrl Pts',(17.4141884105284,70.0981263312731,14.1873276189205));
#55676=CARTESIAN_POINT('Ctrl Pts',(17.4095842484709,70.1262153383897,14.2425624890765));
#55677=CARTESIAN_POINT('Ctrl Pts',(17.404972042269,70.1543534211097,14.2978938626284));
#55678=CARTESIAN_POINT('Ctrl Pts',(17.4003598360671,70.1855614920188,14.3517708958831));
#55679=CARTESIAN_POINT('Ctrl Pts',(17.3957476298651,70.2196625823213,14.4038349165837));
#55680=CARTESIAN_POINT('Ctrl Pts',(17.3911557192663,70.2536136138097,14.4556698341931));
#55681=CARTESIAN_POINT('Ctrl Pts',(17.3865638086674,70.2904320014151,14.5057072208433));
#55682=CARTESIAN_POINT('Ctrl Pts',(17.3819718980685,70.329897084498,14.5536175131963));
#55683=CARTESIAN_POINT('Ctrl Pts',(17.377382700396,70.3693388513904,14.6014994998822));
#55684=CARTESIAN_POINT('Ctrl Pts',(17.3727935027234,70.411423890793,14.6472564938737));
#55685=CARTESIAN_POINT('Ctrl Pts',(17.3682043050508,70.4558899835954,14.6905903311403));
#55686=CARTESIAN_POINT('Ctrl Pts',(17.3636161483663,70.5003459899565,14.7339143388002));
#55687=CARTESIAN_POINT('Ctrl Pts',(17.3590279916819,70.547181614122,14.7748159274075));
#55688=CARTESIAN_POINT('Ctrl Pts',(17.3544398349974,70.5960977654515,14.8130337509429));
#55689=CARTESIAN_POINT('Ctrl Pts',(17.349810790383,70.6454498391579,14.8515921573741));
#55690=CARTESIAN_POINT('Ctrl Pts',(17.3451817457686,70.6969193148219,14.8874183771893));
#55691=CARTESIAN_POINT('Ctrl Pts',(17.3405527011542,70.7501667331433,14.9202869486805));
#55692=CARTESIAN_POINT('Ctrl Pts',(17.3359588337275,70.8030095119357,14.9529057442445));
#55693=CARTESIAN_POINT('Ctrl Pts',(17.3313649663009,70.8576028253208,14.9826114933668));
#55694=CARTESIAN_POINT('Ctrl Pts',(17.3267710988743,70.9135898153586,15.0092299013647));
#55695=CARTESIAN_POINT('Ctrl Pts',(17.322124465666,70.9702198795248,15.0361540519916));
#55696=CARTESIAN_POINT('Ctrl Pts',(17.3174778324577,71.0282753545279,15.0599192682865));
#55697=CARTESIAN_POINT('Ctrl Pts',(17.3128311992494,71.087368277907,15.0803960484111));
#55698=CARTESIAN_POINT('Ctrl Pts',(17.3081845660411,71.1464612012861,15.1008728285356));
#55699=CARTESIAN_POINT('Ctrl Pts',(17.3035379328328,71.2065910461191,15.1180610867985));
#55700=CARTESIAN_POINT('Ctrl Pts',(17.2988912996246,71.2673588385453,15.1318843870276));
#55701=CARTESIAN_POINT('Ctrl Pts',(17.2927452767469,71.3477353661799,15.1501682316186));
#55702=CARTESIAN_POINT('Ctrl Pts',(17.2865992538693,71.429481789506,15.1626267077974));
#55703=CARTESIAN_POINT('Ctrl Pts',(17.2804532309918,71.5118776892291,15.1691017121192));
#55704=CARTESIAN_POINT('Ctrl Pts',(17.2771805155179,71.5557529466724,15.1725496079795));
#55705=CARTESIAN_POINT('Ctrl Pts',(17.273907800044,71.5998120318739,15.1743016585303));
#55706=CARTESIAN_POINT('Ctrl Pts',(17.2706350845702,71.6439433029223,15.1743393774814));
#55707=CARTESIAN_POINT('',(16.4768850845224,71.6462429261512,15.1743397915543));
#55708=CARTESIAN_POINT('Ctrl Pts',(17.2706350845291,71.6439433034762,15.1743393774819));
#55709=CARTESIAN_POINT('Ctrl Pts',(17.2661002318933,71.7050939939149,15.1743916428929));
#55710=CARTESIAN_POINT('Ctrl Pts',(17.2615653792575,71.7663362412798,15.1711485740932));
#55711=CARTESIAN_POINT('Ctrl Pts',(17.2570305266217,71.8272822897832,15.1646072312672));
#55712=CARTESIAN_POINT('Ctrl Pts',(17.2524990686935,71.8881827151916,15.1580707851707));
#55713=CARTESIAN_POINT('Ctrl Pts',(17.2479676107653,71.9487868638439,15.1482410117791));
#55714=CARTESIAN_POINT('Ctrl Pts',(17.2434361528371,72.0087094547258,15.1351669813286));
#55715=CARTESIAN_POINT('Ctrl Pts',(17.2389063309392,72.0686104112505,15.1220976711053));
#55716=CARTESIAN_POINT('Ctrl Pts',(17.2343765090414,72.127829788608,15.1057865376919));
#55717=CARTESIAN_POINT('Ctrl Pts',(17.2298466871436,72.1859920963689,15.0863338210108));
#55718=CARTESIAN_POINT('Ctrl Pts',(17.2252249519321,72.2453345587928,15.066486394849));
#55719=CARTESIAN_POINT('Ctrl Pts',(17.2206032167206,72.3035760300047,15.0433686108237));
#55720=CARTESIAN_POINT('Ctrl Pts',(17.2159814815091,72.360335913905,15.0171397721631));
#55721=CARTESIAN_POINT('Ctrl Pts',(17.2114468974667,72.4160254876279,14.9914055256516));
#55722=CARTESIAN_POINT('Ctrl Pts',(17.2069123134242,72.4702884285972,14.9626768547615));
#55723=CARTESIAN_POINT('Ctrl Pts',(17.2023777293817,72.5227897819664,14.9311509183178));
#55724=CARTESIAN_POINT('Ctrl Pts',(17.1977124185857,72.5768046879385,14.8987161260046));
#55725=CARTESIAN_POINT('Ctrl Pts',(17.1930471077898,72.6289543599915,14.8633205988426));
#55726=CARTESIAN_POINT('Ctrl Pts',(17.1883817969938,72.6789081830433,14.8252253211856));
#55727=CARTESIAN_POINT('Ctrl Pts',(17.1837164861978,72.7288620060951,14.7871300435286));
#55728=CARTESIAN_POINT('Ctrl Pts',(17.1790511754018,72.7766195769644,14.7463354566648));
#55729=CARTESIAN_POINT('Ctrl Pts',(17.1743858646058,72.8218914468588,14.7031434268032));
#55730=CARTESIAN_POINT('Ctrl Pts',(17.1697817024763,72.866569934106,14.6605175189304));
#55731=CARTESIAN_POINT('Ctrl Pts',(17.1651775403467,72.9090171636797,14.6153760878356));
#55732=CARTESIAN_POINT('Ctrl Pts',(17.1605733782172,72.9489378409919,14.5679817542665));
#55733=CARTESIAN_POINT('Ctrl Pts',(17.1559611720242,72.9889282648613,14.5205046167016));
#55734=CARTESIAN_POINT('Ctrl Pts',(17.1513489658313,73.026382897014,14.4707670160188));
#55735=CARTESIAN_POINT('Ctrl Pts',(17.1467367596384,73.0610403932004,14.4190717110626));
#55736=CARTESIAN_POINT('Ctrl Pts',(17.1421448489636,73.0955453827958,14.3676038857457));
#55737=CARTESIAN_POINT('Ctrl Pts',(17.1375529382889,73.1272774953741,14.314195956707));
#55738=CARTESIAN_POINT('Ctrl Pts',(17.1329610276141,73.1560192217013,14.2591795756521));
#55739=CARTESIAN_POINT('Ctrl Pts',(17.1283718298645,73.1847439672648,14.2041956985659));
#55740=CARTESIAN_POINT('Ctrl Pts',(17.1237826321148,73.2104815960163,14.1476057027431));
#55741=CARTESIAN_POINT('Ctrl Pts',(17.1191934343652,73.2330597116227,14.0897672754269));
#55742=CARTESIAN_POINT('Ctrl Pts',(17.1146052776025,73.2556327057403,14.0319419678443));
#55743=CARTESIAN_POINT('Ctrl Pts',(17.1100171208399,73.2750474255411,13.9728692633669));
#55744=CARTESIAN_POINT('Ctrl Pts',(17.1054289640772,73.2911797512475,13.9129264566309));
#55745=CARTESIAN_POINT('Ctrl Pts',(17.1007999195364,73.3074558416485,13.8524494640956));
#55746=CARTESIAN_POINT('Ctrl Pts',(17.0961708749955,73.320390574276,13.7910872811148));
#55747=CARTESIAN_POINT('Ctrl Pts',(17.0915418304546,73.3299086089493,13.7292403941818));
#55748=CARTESIAN_POINT('Ctrl Pts',(17.0869479629481,73.3393543141755,13.6678634940993));
#55749=CARTESIAN_POINT('Ctrl Pts',(17.0823540954416,73.3454350780737,13.6060097486663));
#55750=CARTESIAN_POINT('Ctrl Pts',(17.0777602279351,73.3481294624658,13.5440757264631));
#55751=CARTESIAN_POINT('Ctrl Pts',(17.073113594877,73.3508547947852,13.4814303248322));
#55752=CARTESIAN_POINT('Ctrl Pts',(17.068466961819,73.350115447916,13.4187033228594));
#55753=CARTESIAN_POINT('Ctrl Pts',(17.063820328761,73.34594335698,13.3563024774627));
#55754=CARTESIAN_POINT('Ctrl Pts',(17.059173695703,73.3417712660441,13.2939016320661));
#55755=CARTESIAN_POINT('Ctrl Pts',(17.054527062645,73.3341665574789,13.231827461901));
#55756=CARTESIAN_POINT('Ctrl Pts',(17.049880429587,73.323214327678,13.1704771837765));
#55757=CARTESIAN_POINT('Ctrl Pts',(17.0452762674587,73.3123622029157,13.109687656483));
#55758=CARTESIAN_POINT('Ctrl Pts',(17.0406721053303,73.2981806471449,13.049368508845));
#55759=CARTESIAN_POINT('Ctrl Pts',(17.036067943202,73.2807254577291,12.9899109635671));
#55760=CARTESIAN_POINT('Ctrl Pts',(17.0314557370089,73.2632397718473,12.9303495382931));
#55761=CARTESIAN_POINT('Ctrl Pts',(17.0268435308159,73.2424690460747,12.8716532407826));
#55762=CARTESIAN_POINT('Ctrl Pts',(17.0222313246228,73.2185212901781,12.8142071653422));
#55763=CARTESIAN_POINT('Ctrl Pts',(17.0176394139498,73.1946789138198,12.7570138752125));
#55764=CARTESIAN_POINT('Ctrl Pts',(17.0130475032767,73.1676875793589,12.7010603077331));
#55765=CARTESIAN_POINT('Ctrl Pts',(17.0084555926037,73.1377035953588,12.6467109773116));
#55766=CARTESIAN_POINT('Ctrl Pts',(17.003866394856,73.1077373260562,12.592393756764));
#55767=CARTESIAN_POINT('Ctrl Pts',(16.9992771971082,73.0747821582154,12.5396793368136));
#55768=CARTESIAN_POINT('Ctrl Pts',(16.9946879993605,73.0390410232761,12.4889090083779));
#55769=CARTESIAN_POINT('Ctrl Pts',(16.9900998425999,73.0033079956498,12.438150196391));
#55770=CARTESIAN_POINT('Ctrl Pts',(16.9855116858393,72.9647905476703,12.389335014758));
#55771=CARTESIAN_POINT('Ctrl Pts',(16.9809235290787,72.9237346228418,12.3427753428691));
#55772=CARTESIAN_POINT('Ctrl Pts',(16.9762944845362,72.8823128243542,12.2958007501718));
#55773=CARTESIAN_POINT('Ctrl Pts',(16.9716654399937,72.8383074005824,12.2511224837385));
#55774=CARTESIAN_POINT('Ctrl Pts',(16.9670363954511,72.7920105729229,12.2090245721421));
#55775=CARTESIAN_POINT('Ctrl Pts',(16.9624425279471,72.746065564148,12.1672465710244));
#55776=CARTESIAN_POINT('Ctrl Pts',(16.957848660443,72.6978642923282,12.1280101223236));
#55777=CARTESIAN_POINT('Ctrl Pts',(16.9532547929389,72.6477254880847,12.0915521585726));
#55778=CARTESIAN_POINT('Ctrl Pts',(16.9486081598772,72.5970107852183,12.0546754355107));
#55779=CARTESIAN_POINT('Ctrl Pts',(16.9439615268154,72.5443141943564,12.0206417355799));
#55780=CARTESIAN_POINT('Ctrl Pts',(16.9393148937536,72.4899932556133,11.9896496805916));
#55781=CARTESIAN_POINT('Ctrl Pts',(16.9346682606918,72.4356723168703,11.9586576256034));
#55782=CARTESIAN_POINT('Ctrl Pts',(16.9300216276301,72.3797275324318,11.9307073966637));
#55783=CARTESIAN_POINT('Ctrl Pts',(16.9253749945683,72.3225370223109,11.9059474789458));
#55784=CARTESIAN_POINT('Ctrl Pts',(16.9207708324282,72.265869242013,11.8814138705821));
#55785=CARTESIAN_POINT('Ctrl Pts',(16.9161666702881,72.2077544052792,11.8599154550731));
#55786=CARTESIAN_POINT('Ctrl Pts',(16.9115625081481,72.1485494509366,11.8416218296654));
#55787=CARTESIAN_POINT('Ctrl Pts',(16.9069503019565,72.0892410580769,11.8232962429885));
#55788=CARTESIAN_POINT('Ctrl Pts',(16.9023380957649,72.0288391855924,11.8081869018611));
#55789=CARTESIAN_POINT('Ctrl Pts',(16.8977258895733,71.9677245055836,11.796416494853));
#55790=CARTESIAN_POINT('Ctrl Pts',(16.8931339788878,71.9068787540043,11.7846978822266));
#55791=CARTESIAN_POINT('Ctrl Pts',(16.8885420682024,71.8453269495663,11.7762890035574));
#55792=CARTESIAN_POINT('Ctrl Pts',(16.883950157517,71.7834592892696,11.7712609181377));
#55793=CARTESIAN_POINT('Ctrl Pts',(16.8793609597567,71.7216281807133,11.7662358033374));
#55794=CARTESIAN_POINT('Ctrl Pts',(16.8747717619964,71.6594820909183,11.7645875615234));
#55795=CARTESIAN_POINT('Ctrl Pts',(16.8701825642361,71.5974176123591,11.766335559426));
#55796=CARTESIAN_POINT('Ctrl Pts',(16.8655944074627,71.5353672121461,11.768083160823));
#55797=CARTESIAN_POINT('Ctrl Pts',(16.8610062506894,71.4733988931653,11.7732254578535));
#55798=CARTESIAN_POINT('Ctrl Pts',(16.8564180939161,71.4119084905315,11.7817297163647));
#55799=CARTESIAN_POINT('Ctrl Pts',(16.8517890493855,71.3498701108388,11.7903097613135));
#55800=CARTESIAN_POINT('Ctrl Pts',(16.847160004855,71.2883187317408,11.8023119494799));
#55801=CARTESIAN_POINT('Ctrl Pts',(16.8425309603244,71.2276525359906,11.8176495856164));
#55802=CARTESIAN_POINT('Ctrl Pts',(16.8379370928073,71.1674473545104,11.8328706680603));
#55803=CARTESIAN_POINT('Ctrl Pts',(16.8333432252902,71.1081144229225,11.8513764714748));
#55804=CARTESIAN_POINT('Ctrl Pts',(16.8287493577731,71.0500273090466,11.8730321874042));
#55805=CARTESIAN_POINT('Ctrl Pts',(16.8241027247359,70.9912730020554,11.8949366425739));
#55806=CARTESIAN_POINT('Ctrl Pts',(16.8194560916986,70.9337938089614,11.920063634761));
#55807=CARTESIAN_POINT('Ctrl Pts',(16.8148094586613,70.8779528005222,11.9482248419646));
#55808=CARTESIAN_POINT('Ctrl Pts',(16.810162825624,70.8221117920829,11.9763860491682));
#55809=CARTESIAN_POINT('Ctrl Pts',(16.8055161925867,70.7679093966695,12.0075811528165));
#55810=CARTESIAN_POINT('Ctrl Pts',(16.8008695595495,70.7156782601852,12.0415769806826));
#55811=CARTESIAN_POINT('Ctrl Pts',(16.7962653974163,70.6639245239118,12.0752620817202));
#55812=CARTESIAN_POINT('Ctrl Pts',(16.7916612352832,70.613901528645,12.1118300465224));
#55813=CARTESIAN_POINT('Ctrl Pts',(16.7870570731501,70.5659478186091,12.1510770213199));
#55814=CARTESIAN_POINT('Ctrl Pts',(16.7824448669576,70.5179103273163,12.1903925655956));
#55815=CARTESIAN_POINT('Ctrl Pts',(16.7778326607652,70.471949813175,12.2323962503146));
#55816=CARTESIAN_POINT('Ctrl Pts',(16.7732204545727,70.4283788282358,12.2768385259833));
#55817=CARTESIAN_POINT('Ctrl Pts',(16.7686285438945,70.3849995727013,12.3210852382268));
#55818=CARTESIAN_POINT('Ctrl Pts',(16.7640366332163,70.3439892368291,12.3677487808467));
#55819=CARTESIAN_POINT('Ctrl Pts',(16.7594447225381,70.3056225968613,12.4165431448612));
#55820=CARTESIAN_POINT('Ctrl Pts',(16.7548555247851,70.2672786241075,12.4653086809071));
#55821=CARTESIAN_POINT('Ctrl Pts',(16.7502663270321,70.2315755625268,12.5162021437496));
#55822=CARTESIAN_POINT('Ctrl Pts',(16.745677129279,70.1987486311264,12.5689036385956));
#55823=CARTESIAN_POINT('Ctrl Pts',(16.741088972513,70.1659291459973,12.6215931789393));
#55824=CARTESIAN_POINT('Ctrl Pts',(16.7365008157471,70.1359847635496,12.6760895065633));
#55825=CARTESIAN_POINT('Ctrl Pts',(16.7319126589811,70.1091068540045,12.7320445777913));
#55826=CARTESIAN_POINT('Ctrl Pts',(16.7272836144436,70.0819894195517,12.7884982976678));
#55827=CARTESIAN_POINT('Ctrl Pts',(16.722654569906,70.0579936425927,12.8464364326991));
#55828=CARTESIAN_POINT('Ctrl Pts',(16.7180255253685,70.0372672091046,12.905479174479));
#55829=CARTESIAN_POINT('Ctrl Pts',(16.7134316578588,70.0166982798967,12.9640732387497));
#55830=CARTESIAN_POINT('Ctrl Pts',(16.7088377903492,69.9993492646001,13.0237546695944));
#55831=CARTESIAN_POINT('Ctrl Pts',(16.7042439228395,69.9853141456875,13.0841375997697));
#55832=CARTESIAN_POINT('Ctrl Pts',(16.699597289788,69.9711178182393,13.1452140932704));
#55833=CARTESIAN_POINT('Ctrl Pts',(16.6949506567366,69.960312108809,13.2070077826231));
#55834=CARTESIAN_POINT('Ctrl Pts',(16.6903040236851,69.9529405933612,13.2691119902036));
#55835=CARTESIAN_POINT('Ctrl Pts',(16.6856573906336,69.9455690779134,13.3312161977841));
#55836=CARTESIAN_POINT('Ctrl Pts',(16.6810107575821,69.9416317275215,13.3936303905322));
#55837=CARTESIAN_POINT('Ctrl Pts',(16.6763641245307,69.9411179252497,13.455948477487));
#55838=CARTESIAN_POINT('Ctrl Pts',(16.6717599623902,69.9406088192064,13.5176969679418));
#55839=CARTESIAN_POINT('Ctrl Pts',(16.6671558002497,69.9434588708166,13.5795952177));
#55840=CARTESIAN_POINT('Ctrl Pts',(16.6625516381092,69.9496851607163,13.6412484143963));
#55841=CARTESIAN_POINT('Ctrl Pts',(16.6579394319176,69.9559223287286,13.703009326991));
#55842=CARTESIAN_POINT('Ctrl Pts',(16.653327225726,69.9655475949764,13.7645238182712));
#55843=CARTESIAN_POINT('Ctrl Pts',(16.6487150195345,69.9785255909888,13.8253935004803));
#55844=CARTESIAN_POINT('Ctrl Pts',(16.6441231088489,69.9914464787575,13.885995332349));
#55845=CARTESIAN_POINT('Ctrl Pts',(16.6395311981633,70.0076905724707,13.9459575145064));
#55846=CARTESIAN_POINT('Ctrl Pts',(16.6349392874778,70.0271712445152,14.0048930084812));
#55847=CARTESIAN_POINT('Ctrl Pts',(16.6303500897174,70.0466404072753,14.0637936830536));
#55848=CARTESIAN_POINT('Ctrl Pts',(16.625760891957,70.0693421972098,14.121668391791));
#55849=CARTESIAN_POINT('Ctrl Pts',(16.6211716941966,70.0951398888881,14.1781443521594));
#55850=CARTESIAN_POINT('Ctrl Pts',(16.6165835374232,70.1209317287671,14.2346075018473));
#55851=CARTESIAN_POINT('Ctrl Pts',(16.6119953806499,70.1498178652253,14.2896720720946));
#55852=CARTESIAN_POINT('Ctrl Pts',(16.6074072238766,70.1816138865965,14.3429862827142));
#55853=CARTESIAN_POINT('Ctrl Pts',(16.6027781793462,70.2136932609703,14.3967756075465));
#55854=CARTESIAN_POINT('Ctrl Pts',(16.5981491348158,70.2487344032401,14.448782752615));
#55855=CARTESIAN_POINT('Ctrl Pts',(16.5935200902854,70.2865022922881,14.498674805551));
#55856=CARTESIAN_POINT('Ctrl Pts',(16.5889262227686,70.3239831757702,14.5481877190316));
#55857=CARTESIAN_POINT('Ctrl Pts',(16.5843323552518,70.3641491303437,14.5956172206556));
#55858=CARTESIAN_POINT('Ctrl Pts',(16.5797384877349,70.4067304188606,14.6406718175304));
#55859=CARTESIAN_POINT('Ctrl Pts',(16.5750918546977,70.4498007993759,14.6862439150163));
#55860=CARTESIAN_POINT('Ctrl Pts',(16.5704452216606,70.4953419787245,14.7293858245651));
#55861=CARTESIAN_POINT('Ctrl Pts',(16.5657985886234,70.5430390283343,14.7698365757849));
#55862=CARTESIAN_POINT('Ctrl Pts',(16.5611519555862,70.5907360779441,14.8102873270047));
#55863=CARTESIAN_POINT('Ctrl Pts',(16.5565053225491,70.6405885374863,14.848046649549));
#55864=CARTESIAN_POINT('Ctrl Pts',(16.5518586895119,70.6922520315995,14.8828990713898));
#55865=CARTESIAN_POINT('Ctrl Pts',(16.5471911926695,70.7441474995034,14.9179079837766));
#55866=CARTESIAN_POINT('Ctrl Pts',(16.5425236958271,70.7980717651909,14.9501199881615));
#55867=CARTESIAN_POINT('Ctrl Pts',(16.5378561989847,70.8536966037079,14.9792980381288));
#55868=CARTESIAN_POINT('Ctrl Pts',(16.5331963030289,70.9092308587477,15.0084285724666));
#55869=CARTESIAN_POINT('Ctrl Pts',(16.5285364070732,70.9664597606,15.0345347338153));
#55870=CARTESIAN_POINT('Ctrl Pts',(16.5238765111174,71.02502660324,15.0574229695303));
#55871=CARTESIAN_POINT('Ctrl Pts',(16.5192236139525,71.0835054831689,15.0802768289468));
#55872=CARTESIAN_POINT('Ctrl Pts',(16.5145707167876,71.1433178571596,15.0999221917026));
#55873=CARTESIAN_POINT('Ctrl Pts',(16.5099178196227,71.204084775008,15.11621253421));
#55874=CARTESIAN_POINT('Ctrl Pts',(16.505269008793,71.2647983252484,15.1324885699756));
#55875=CARTESIAN_POINT('Ctrl Pts',(16.5006201979632,71.3264642846154,15.1454153088827));
#55876=CARTESIAN_POINT('Ctrl Pts',(16.4959713871335,71.3886875454887,15.1548957093241));
#55877=CARTESIAN_POINT('Ctrl Pts',(16.4913250410842,71.4508778158432,15.164371083296));
#55878=CARTESIAN_POINT('Ctrl Pts',(16.486678695035,71.5136243185004,15.1704036737768));
#55879=CARTESIAN_POINT('Ctrl Pts',(16.4820323489858,71.5765224629929,15.1729476564169));
#55880=CARTESIAN_POINT('Ctrl Pts',(16.4803165941806,71.5997488418521,15.1738870721197));
#55881=CARTESIAN_POINT('Ctrl Pts',(16.4786008393754,71.6229958356541,15.1743512890066));
#55882=CARTESIAN_POINT('Ctrl Pts',(16.4768850845702,71.646242925503,15.1743397915547));
#55883=CARTESIAN_POINT('',(15.6831350846103,71.6456222717028,15.1743399855062));
#55884=CARTESIAN_POINT('Ctrl Pts',(16.4768850845224,71.6462429261512,15.1743397915543));
#55885=CARTESIAN_POINT('Ctrl Pts',(16.4718160335965,71.7149244661725,15.1743058232891));
#55886=CARTESIAN_POINT('Ctrl Pts',(16.4667469826707,71.7834665079012,15.1701160948275));
#55887=CARTESIAN_POINT('Ctrl Pts',(16.4616779317449,71.8513919293067,15.1618457851295));
#55888=CARTESIAN_POINT('Ctrl Pts',(16.456590169375,71.9195680845766,15.1535449471452));
#55889=CARTESIAN_POINT('Ctrl Pts',(16.451502407005,71.9871227640871,15.141133486262));
#55890=CARTESIAN_POINT('Ctrl Pts',(16.4464146446351,72.0535901041082,15.1247373430572));
#55891=CARTESIAN_POINT('Ctrl Pts',(16.4413033881495,72.1203643750079,15.1082654862368));
#55892=CARTESIAN_POINT('Ctrl Pts',(16.4361921316639,72.1860409566487,15.0877722091777));
#55893=CARTESIAN_POINT('Ctrl Pts',(16.4310808751783,72.2501685556704,15.0634333464793));
#55894=CARTESIAN_POINT('Ctrl Pts',(16.4298383349499,72.2657578969132,15.0575165985915));
#55895=CARTESIAN_POINT('Ctrl Pts',(16.4285957947215,72.2812558061786,15.0513728042411));
#55896=CARTESIAN_POINT('Ctrl Pts',(16.4273532544931,72.2966560156161,15.0450049008571));
#55897=CARTESIAN_POINT('Ctrl Pts',(16.422749092363,72.3537206155941,15.0214089971274));
#55898=CARTESIAN_POINT('Ctrl Pts',(16.4181449302328,72.4096139955579,14.9946611715146));
#55899=CARTESIAN_POINT('Ctrl Pts',(16.4135407681026,72.4639659032766,14.9648995610384));
#55900=CARTESIAN_POINT('Ctrl Pts',(16.4089285619098,72.5184127707601,14.9350859532057));
#55901=CARTESIAN_POINT('Ctrl Pts',(16.4043163557169,72.5713122838385,14.9022481715234));
#55902=CARTESIAN_POINT('Ctrl Pts',(16.3997041495241,72.6223113381645,14.8665740485079));
#55903=CARTESIAN_POINT('Ctrl Pts',(16.3951122388491,72.6730859766308,14.8310569056382));
#55904=CARTESIAN_POINT('Ctrl Pts',(16.3905203281741,72.7219764138639,14.7927286001777));
#55905=CARTESIAN_POINT('Ctrl Pts',(16.3859284174991,72.7686599742686,14.7518197477828));
#55906=CARTESIAN_POINT('Ctrl Pts',(16.3813392197493,72.8153159537777,14.7109350645553));
#55907=CARTESIAN_POINT('Ctrl Pts',(16.3767500219996,72.8597672615453,14.6674731916271));
#55908=CARTESIAN_POINT('Ctrl Pts',(16.3721608242498,72.9017238749623,14.6217053255063));
#55909=CARTESIAN_POINT('Ctrl Pts',(16.3675726674872,72.9436709711833,14.5759478411042));
#55910=CARTESIAN_POINT('Ctrl Pts',(16.3629845107246,72.9831241541936,14.5278857759225));
#55911=CARTESIAN_POINT('Ctrl Pts',(16.358396353962,73.0198313275112,14.4778260571924));
#55912=CARTESIAN_POINT('Ctrl Pts',(16.3537673094213,73.056865620156,14.427320226707));
#55913=CARTESIAN_POINT('Ctrl Pts',(16.3491382648807,73.0911043789371,14.3747813629434));
#55914=CARTESIAN_POINT('Ctrl Pts',(16.3445092203401,73.1223326069817,14.3205556478174));
#55915=CARTESIAN_POINT('Ctrl Pts',(16.3399153528339,73.1533235254813,14.2667420047362));
#55916=CARTESIAN_POINT('Ctrl Pts',(16.3353214853277,73.1813493306058,14.2112675442954));
#55917=CARTESIAN_POINT('Ctrl Pts',(16.3307276178215,73.2062466996329,14.1544942774377));
#55918=CARTESIAN_POINT('Ctrl Pts',(16.3260809847637,73.2314300419517,14.0970689080232));
#55919=CARTESIAN_POINT('Ctrl Pts',(16.3214343517058,73.2534124201494,14.0383151978398));
#55920=CARTESIAN_POINT('Ctrl Pts',(16.316787718648,73.2720762327638,13.9786248807927));
#55921=CARTESIAN_POINT('Ctrl Pts',(16.3121410855901,73.2907400453782,13.9189345637456));
#55922=CARTESIAN_POINT('Ctrl Pts',(16.3074944525322,73.3060852228388,13.8583081691265));
#55923=CARTESIAN_POINT('Ctrl Pts',(16.3028478194744,73.3180475406727,13.7971468176242));
#55924=CARTESIAN_POINT('Ctrl Pts',(16.2982436572919,73.3299005212503,13.7365444894195));
#55925=CARTESIAN_POINT('Ctrl Pts',(16.2936394951094,73.3384791376836,13.6751773685297));
#55926=CARTESIAN_POINT('Ctrl Pts',(16.2890353329268,73.3436940136494,13.6134303970669));
#55927=CARTESIAN_POINT('Ctrl Pts',(16.2844231267405,73.3489180006065,13.5515755465041));
#55928=CARTESIAN_POINT('Ctrl Pts',(16.2798109205542,73.3507663378284,13.4893400098367));
#55929=CARTESIAN_POINT('Ctrl Pts',(16.2751987143679,73.3492005467128,13.427121886456));
#55930=CARTESIAN_POINT('Ctrl Pts',(16.2706068036402,73.3476416456727,13.365177546443));
#55931=CARTESIAN_POINT('Ctrl Pts',(16.2660148929124,73.342698585339,13.303250976302));
#55932=CARTESIAN_POINT('Ctrl Pts',(16.2614229821846,73.3343853590719,13.2417385436812));
#55933=CARTESIAN_POINT('Ctrl Pts',(16.256833784382,73.326077044303,13.180262452932));
#55934=CARTESIAN_POINT('Ctrl Pts',(16.2522445865795,73.3144025802111,13.1192005160946));
#55935=CARTESIAN_POINT('Ctrl Pts',(16.2476553887769,73.2994278249831,13.0589442984442));
#55936=CARTESIAN_POINT('Ctrl Pts',(16.2430672319615,73.2844564665425,12.9987017489675));
#55937=CARTESIAN_POINT('Ctrl Pts',(16.2384790751462,73.2661864258267,12.9392650477409));
#55938=CARTESIAN_POINT('Ctrl Pts',(16.2338909183309,73.2447342957133,12.8810138828842));
#55939=CARTESIAN_POINT('Ctrl Pts',(16.2292618738412,73.2230909934706,12.8222436087753));
#55940=CARTESIAN_POINT('Ctrl Pts',(16.2246328293516,73.198208753179,12.7646806099599));
#55941=CARTESIAN_POINT('Ctrl Pts',(16.220003784862,73.1702573833474,12.708695332964));
#55942=CARTESIAN_POINT('Ctrl Pts',(16.2154099173039,73.1425184209413,12.6531354980347));
#55943=CARTESIAN_POINT('Ctrl Pts',(16.2108160497458,73.1117571186373,12.5991299068633));
#55944=CARTESIAN_POINT('Ctrl Pts',(16.2062221821877,73.0781850242481,12.547014675149));
#55945=CARTESIAN_POINT('Ctrl Pts',(16.2015755492324,73.0442273190691,12.494300845223));
#55946=CARTESIAN_POINT('Ctrl Pts',(16.196928916277,73.0073941386226,12.4435215181809));
#55947=CARTESIAN_POINT('Ctrl Pts',(16.1922822833217,72.9679470634001,12.394991115994));
#55948=CARTESIAN_POINT('Ctrl Pts',(16.1876356503663,72.9284999881775,12.3464607138071));
#55949=CARTESIAN_POINT('Ctrl Pts',(16.1829890174109,72.8864394209574,12.3001795868457));
#55950=CARTESIAN_POINT('Ctrl Pts',(16.1783423844556,72.8420642520106,12.2564228481221));
#55951=CARTESIAN_POINT('Ctrl Pts',(16.1737382224058,72.7980946786054,12.2130660523975));
#55952=CARTESIAN_POINT('Ctrl Pts',(16.169134060356,72.7516788484522,12.1720162449868));
#55953=CARTESIAN_POINT('Ctrl Pts',(16.1645298983063,72.7030882719126,12.1335605681294));
#55954=CARTESIAN_POINT('Ctrl Pts',(16.1599176921034,72.654412800438,12.0950377035082));
#55955=CARTESIAN_POINT('Ctrl Pts',(16.1553054859005,72.6035553073447,12.0591184354327));
#55956=CARTESIAN_POINT('Ctrl Pts',(16.1506932796976,72.5508263862995,12.0260547466775));
#55957=CARTESIAN_POINT('Ctrl Pts',(16.1461013691019,72.4983294942275,11.9931365517727));
#55958=CARTESIAN_POINT('Ctrl Pts',(16.1415094585062,72.4439780262819,11.963049151286));
#55959=CARTESIAN_POINT('Ctrl Pts',(16.1369175479105,72.3881101177355,11.9359998316124));
#55960=CARTESIAN_POINT('Ctrl Pts',(16.1323283502394,72.3322752162393,11.9089664928171));
#55961=CARTESIAN_POINT('Ctrl Pts',(16.1277391525683,72.2749261065563,11.8849678957112));
#55962=CARTESIAN_POINT('Ctrl Pts',(16.1231499548973,72.2164255705906,11.8641654402362));
#55963=CARTESIAN_POINT('Ctrl Pts',(16.1185617982125,72.1579383045395,11.8433677034669));
#55964=CARTESIAN_POINT('Ctrl Pts',(16.1139736415278,72.0983006085148,11.8257648385037));
#55965=CARTESIAN_POINT('Ctrl Pts',(16.1093854848431,72.0378933893514,11.8114693928313));
#55966=CARTESIAN_POINT('Ctrl Pts',(16.104756440226,71.9769478436947,11.7970465515058));
#55967=CARTESIAN_POINT('Ctrl Pts',(16.1001273956088,71.9152194931725,11.7859905263778));
#55968=CARTESIAN_POINT('Ctrl Pts',(16.0954983509916,71.8531109370326,11.7783644002809));
#55969=CARTESIAN_POINT('Ctrl Pts',(16.0909044835606,71.7914743582494,11.770796226889));
#55970=CARTESIAN_POINT('Ctrl Pts',(16.0863106161296,71.729463849279,11.7666059799524));
#55971=CARTESIAN_POINT('Ctrl Pts',(16.0817167486986,71.667476448231,11.7658029849711));
#55972=CARTESIAN_POINT('Ctrl Pts',(16.0770701154883,71.6047770515562,11.7649907666814));
#55973=CARTESIAN_POINT('Ctrl Pts',(16.072423482278,71.5421018294417,11.7676441042901));
#55974=CARTESIAN_POINT('Ctrl Pts',(16.0677768490677,71.4798573743076,11.7737186333987));
#55975=CARTESIAN_POINT('Ctrl Pts',(16.0631302158574,71.4176129191735,11.7797931625072));
#55976=CARTESIAN_POINT('Ctrl Pts',(16.0584835826472,71.355799745575,11.7892887409084));
#55977=CARTESIAN_POINT('Ctrl Pts',(16.0538369494369,71.2948122883247,11.8021081893533));
#55978=CARTESIAN_POINT('Ctrl Pts',(16.0492327873053,71.2343822676048,11.8148104656913));
#55979=CARTESIAN_POINT('Ctrl Pts',(16.0446286251737,71.1745240167357,11.8308262668942));
#55980=CARTESIAN_POINT('Ctrl Pts',(16.0400244630421,71.115626873338,11.8500878820545));
#55981=CARTESIAN_POINT('Ctrl Pts',(16.0354122568494,71.0566268290858,11.8693831497239));
#55982=CARTESIAN_POINT('Ctrl Pts',(16.0308000506567,70.9985917641664,11.8919355246881));
#55983=CARTESIAN_POINT('Ctrl Pts',(16.0261878444641,70.9419032972114,11.9176252949866));
#55984=CARTESIAN_POINT('Ctrl Pts',(16.0215959337898,70.8854642817718,11.9432020202077));
#55985=CARTESIAN_POINT('Ctrl Pts',(16.0170040231156,70.830360513052,11.9718884022468));
#55986=CARTESIAN_POINT('Ctrl Pts',(16.0124121124413,70.776951565364,12.0035170809115));
#55987=CARTESIAN_POINT('Ctrl Pts',(16.0078229146931,70.7235741719756,12.0351270731792));
#55988=CARTESIAN_POINT('Ctrl Pts',(16.0032337169449,70.6718900493519,12.0696756566565));
#55989=CARTESIAN_POINT('Ctrl Pts',(15.9986445191967,70.6222341362716,12.1069495787386));
#55990=CARTESIAN_POINT('Ctrl Pts',(15.9940563624364,70.5725894868608,12.1442150458127));
#55991=CARTESIAN_POINT('Ctrl Pts',(15.9894682056761,70.5249725388424,12.1842043195397));
#55992=CARTESIAN_POINT('Ctrl Pts',(15.9848800489158,70.4796875205036,12.2266620528809));
#55993=CARTESIAN_POINT('Ctrl Pts',(15.9802510043744,70.4339989405564,12.26949815222));
#55994=CARTESIAN_POINT('Ctrl Pts',(15.9756219598329,70.390684465659,12.3148465929179));
#55995=CARTESIAN_POINT('Ctrl Pts',(15.9709929152914,70.3500190739218,12.3624066215651));
#55996=CARTESIAN_POINT('Ctrl Pts',(15.9663990477895,70.3096627066671,12.4096052319987));
#55997=CARTESIAN_POINT('Ctrl Pts',(15.9618051802875,70.2719155657789,12.4589814900987));
#55998=CARTESIAN_POINT('Ctrl Pts',(15.9572113127856,70.2370047462432,12.51020958288));
#55999=CARTESIAN_POINT('Ctrl Pts',(15.9525646797243,70.2016929380158,12.5620260859644));
#56000=CARTESIAN_POINT('Ctrl Pts',(15.9479180466631,70.1692833129285,12.6157367890329));
#56001=CARTESIAN_POINT('Ctrl Pts',(15.9432714136018,70.1399634886832,12.6709782568701));
#56002=CARTESIAN_POINT('Ctrl Pts',(15.9386247805406,70.1106436644379,12.7262197247073));
#56003=CARTESIAN_POINT('Ctrl Pts',(15.9339781474793,70.0844138067301,12.7829914498343));
#56004=CARTESIAN_POINT('Ctrl Pts',(15.9293315144181,70.061410791909,12.8409109568184));
#56005=CARTESIAN_POINT('Ctrl Pts',(15.924727351917,70.0386180262967,12.8983010753455));
#56006=CARTESIAN_POINT('Ctrl Pts',(15.9201231894159,70.0189032023114,12.9570449467636));
#56007=CARTESIAN_POINT('Ctrl Pts',(15.9155190269148,70.0024249449438,13.0167806225864));
#56008=CARTESIAN_POINT('Ctrl Pts',(15.9109068207683,69.9859178994396,13.0766206588861));
#56009=CARTESIAN_POINT('Ctrl Pts',(15.9062946146218,69.9726589726973,13.1374555102616));
#56010=CARTESIAN_POINT('Ctrl Pts',(15.9016824084754,69.9627591785472,13.1989009376986));
#56011=CARTESIAN_POINT('Ctrl Pts',(15.8970904974269,69.9529029464771,13.2600759867233));
#56012=CARTESIAN_POINT('Ctrl Pts',(15.8924985863785,69.9463764548892,13.321855751545));
#56013=CARTESIAN_POINT('Ctrl Pts',(15.8879066753301,69.9432388217305,13.3838480482384));
#56014=CARTESIAN_POINT('Ctrl Pts',(15.883317477207,69.9401030423022,13.4458037195546));
#56015=CARTESIAN_POINT('Ctrl Pts',(15.878728279084,69.9403521761729,13.5079711681707));
#56016=CARTESIAN_POINT('Ctrl Pts',(15.8741390809609,69.9439934776256,13.5699533952491));
#56017=CARTESIAN_POINT('Ctrl Pts',(15.8695509238258,69.9476339531059,13.6319215626273));
#56018=CARTESIAN_POINT('Ctrl Pts',(15.8649627666906,69.9546650384593,13.6937040858136));
#56019=CARTESIAN_POINT('Ctrl Pts',(15.8603746095555,69.9650419344671,13.75490631302));
#56020=CARTESIAN_POINT('Ctrl Pts',(15.8557455653758,69.9755113034651,13.8166539396354));
#56021=CARTESIAN_POINT('Ctrl Pts',(15.8511165211961,69.9893863585377,13.8778103537777));
#56022=CARTESIAN_POINT('Ctrl Pts',(15.8464874770164,70.00656829291,13.9379802041074));
#56023=CARTESIAN_POINT('Ctrl Pts',(15.8418936091439,70.0236196610188,13.9976928211387));
#56024=CARTESIAN_POINT('Ctrl Pts',(15.8372997412715,70.0439276007735,14.0564333496011));
#56025=CARTESIAN_POINT('Ctrl Pts',(15.832705873399,70.0673459657709,14.1138325097829));
#56026=CARTESIAN_POINT('Ctrl Pts',(15.8280592410657,70.0910333105118,14.1718909479024));
#56027=CARTESIAN_POINT('Ctrl Pts',(15.8234126087324,70.1179027756458,14.2285765194346));
#56028=CARTESIAN_POINT('Ctrl Pts',(15.8187659763991,70.147755046646,14.2835320702303));
#56029=CARTESIAN_POINT('Ctrl Pts',(15.8141193440658,70.1776073176461,14.3384876210261));
#56030=CARTESIAN_POINT('Ctrl Pts',(15.8094727117326,70.2104420630163,14.3917127326367));
#56031=CARTESIAN_POINT('Ctrl Pts',(15.8048260793993,70.2460160674514,14.4428820303227));
#56032=CARTESIAN_POINT('Ctrl Pts',(15.8002390201906,70.2811339878999,14.4933953012933));
#56033=CARTESIAN_POINT('Ctrl Pts',(15.7956519609819,70.3190625536555,14.5421082849052));
#56034=CARTESIAN_POINT('Ctrl Pts',(15.7910649017732,70.359590125684,14.5886902174917));
#56035=CARTESIAN_POINT('Ctrl Pts',(15.7864856588548,70.4000486392479,14.6351927750605));
#56036=CARTESIAN_POINT('Ctrl Pts',(15.7819064159364,70.4430970338756,14.6795711079166));
#56037=CARTESIAN_POINT('Ctrl Pts',(15.777327173018,70.4884814205779,14.7215247645125));
#56038=CARTESIAN_POINT('Ctrl Pts',(15.77275228342,70.5338226619869,14.7634385372859));
#56039=CARTESIAN_POINT('Ctrl Pts',(15.7681773938221,70.5814951205441,14.8029318564857));
#56040=CARTESIAN_POINT('Ctrl Pts',(15.7636025042241,70.6312069215191,14.8397398421458));
#56041=CARTESIAN_POINT('Ctrl Pts',(15.7590302639737,70.6808899340752,14.8765265120681));
#56042=CARTESIAN_POINT('Ctrl Pts',(15.7544580237233,70.7326095370287,14.9106306281275));
#56043=CARTESIAN_POINT('Ctrl Pts',(15.7498857834729,70.7860411279776,14.9418278311937));
#56044=CARTESIAN_POINT('Ctrl Pts',(15.7453144922606,70.8394616283865,14.9730185588055));
#56045=CARTESIAN_POINT('Ctrl Pts',(15.7407432010483,70.8945929695165,15.001303313918));
#56046=CARTESIAN_POINT('Ctrl Pts',(15.736171909836,70.9510837312444,15.0265024107085));
#56047=CARTESIAN_POINT('Ctrl Pts',(15.7315966771968,71.007623200043,15.0517232344885));
#56048=CARTESIAN_POINT('Ctrl Pts',(15.7270214445576,71.0655239636073,15.0738528742927));
#56049=CARTESIAN_POINT('Ctrl Pts',(15.7224462119185,71.1244134392268,15.092759328765));
#56050=CARTESIAN_POINT('Ctrl Pts',(15.717869102674,71.1833270693129,15.1116735380239));
#56051=CARTESIAN_POINT('Ctrl Pts',(15.7132919934295,71.2432297242223,15.1273617962317));
#56052=CARTESIAN_POINT('Ctrl Pts',(15.708714884185,71.3037353937151,15.1397425347676));
#56053=CARTESIAN_POINT('Ctrl Pts',(15.7041294199245,71.364351509739,15.1521458729977));
#56054=CARTESIAN_POINT('Ctrl Pts',(15.699543955664,71.4255723322453,15.161229552918));
#56055=CARTESIAN_POINT('Ctrl Pts',(15.6949584914034,71.4870043162473,15.1669636539916));
#56056=CARTESIAN_POINT('Ctrl Pts',(15.6910173558057,71.5398041561834,15.1718920251615));
#56057=CARTESIAN_POINT('Ctrl Pts',(15.687076220208,71.5927597118406,15.1743468795833));
#56058=CARTESIAN_POINT('Ctrl Pts',(15.6831350846103,71.6456222717028,15.1743399855062));
#56059=CARTESIAN_POINT('',(14.8893850846217,71.6442647494568,15.1743396219082));
#56060=CARTESIAN_POINT('Ctrl Pts',(15.6831350845702,71.6456222722405,15.1743399855061));
#56061=CARTESIAN_POINT('Ctrl Pts',(15.6821969378403,71.658205660058,15.1743383444381));
#56062=CARTESIAN_POINT('Ctrl Pts',(15.6812587911104,71.6707879882523,15.1741973479661));
#56063=CARTESIAN_POINT('Ctrl Pts',(15.6803206443805,71.683367201171,15.1739170540948));
#56064=CARTESIAN_POINT('Ctrl Pts',(15.6757164819436,71.7451024689719,15.1725414499677));
#56065=CARTESIAN_POINT('Ctrl Pts',(15.6711123195067,71.8068849098217,15.167803682167));
#56066=CARTESIAN_POINT('Ctrl Pts',(15.6665081570698,71.8683193739522,15.1596987270862));
#56067=CARTESIAN_POINT('Ctrl Pts',(15.6618959509153,71.9298611673719,15.1515796122161));
#56068=CARTESIAN_POINT('Ctrl Pts',(15.6572837447608,71.9910532545598,15.1400814978904));
#56069=CARTESIAN_POINT('Ctrl Pts',(15.6526715386063,72.0514985127723,15.125251894282));
#56070=CARTESIAN_POINT('Ctrl Pts',(15.6480796276455,72.1116777923658,15.1104875457094));
#56071=CARTESIAN_POINT('Ctrl Pts',(15.6434877166847,72.1711163008623,15.0924210600151));
#56072=CARTESIAN_POINT('Ctrl Pts',(15.6388958057239,72.2294298237826,15.0711508362838));
#56073=CARTESIAN_POINT('Ctrl Pts',(15.6343066076969,72.2877088946567,15.0498931791528));
#56074=CARTESIAN_POINT('Ctrl Pts',(15.6297174096699,72.3448638225535,15.0254357112682));
#56075=CARTESIAN_POINT('Ctrl Pts',(15.6251282116429,72.4005261711974,14.9979264711277));
#56076=CARTESIAN_POINT('Ctrl Pts',(15.6205400546121,72.4561758936071,14.970423471078));
#56077=CARTESIAN_POINT('Ctrl Pts',(15.6159518975812,72.5103332546068,14.9398702980457));
#56078=CARTESIAN_POINT('Ctrl Pts',(15.6113637405504,72.5626522657928,14.9064620135938));
#56079=CARTESIAN_POINT('Ctrl Pts',(15.6067346962846,72.6154375164042,14.8727560121364));
#56080=CARTESIAN_POINT('Ctrl Pts',(15.6021056520189,72.6663510289185,14.8361440122005));
#56081=CARTESIAN_POINT('Ctrl Pts',(15.5974766077532,72.7150672185874,14.796871085328));
#56082=CARTESIAN_POINT('Ctrl Pts',(15.5928827400036,72.7634132096295,14.7578965968945));
#56083=CARTESIAN_POINT('Ctrl Pts',(15.588288872254,72.809594814753,14.7163018703938));
#56084=CARTESIAN_POINT('Ctrl Pts',(15.5836950045044,72.8533289087601,14.6723654132508));
#56085=CARTESIAN_POINT('Ctrl Pts',(15.5790483719806,72.8975653288505,14.6279243056986));
#56086=CARTESIAN_POINT('Ctrl Pts',(15.5744017394569,72.9392972884855,14.5810877163756));
#56087=CARTESIAN_POINT('Ctrl Pts',(15.5697551069331,72.9782735500341,14.5321783914294));
#56088=CARTESIAN_POINT('Ctrl Pts',(15.5651084744093,73.0172498115826,14.4832690664832));
#56089=CARTESIAN_POINT('Ctrl Pts',(15.5604618418855,73.053470118873,14.4322874742781));
#56090=CARTESIAN_POINT('Ctrl Pts',(15.5558152093618,73.0867296100807,14.3795844054868));
#56091=CARTESIAN_POINT('Ctrl Pts',(15.5512110445284,73.1196851276543,14.3273630140382));
#56092=CARTESIAN_POINT('Ctrl Pts',(15.546606879695,73.1498640561934,14.2732450603545));
#56093=CARTESIAN_POINT('Ctrl Pts',(15.5420027148615,73.1770439298689,14.2175571601528));
#56094=CARTESIAN_POINT('Ctrl Pts',(15.5373905090066,73.2042712722944,14.1617720028761));
#56095=CARTESIAN_POINT('Ctrl Pts',(15.5327783031517,73.228488761569,14.1044118176455));
#56096=CARTESIAN_POINT('Ctrl Pts',(15.5281660972967,73.2495166336152,14.045833883476));
#56097=CARTESIAN_POINT('Ctrl Pts',(15.5235741838923,73.2704519887471,13.9875136762749));
#56098=CARTESIAN_POINT('Ctrl Pts',(15.518982270488,73.2882255366742,13.9279868828877));
#56099=CARTESIAN_POINT('Ctrl Pts',(15.5143903570836,73.3027070635906,13.8676281335276));
#56100=CARTESIAN_POINT('Ctrl Pts',(15.5098011566025,73.3171800347551,13.807305044391));
#56101=CARTESIAN_POINT('Ctrl Pts',(15.5052119561214,73.3283647240605,13.7461514663075));
#56102=CARTESIAN_POINT('Ctrl Pts',(15.5006227556404,73.336181012075,13.6845562975226));
#56103=CARTESIAN_POINT('Ctrl Pts',(15.4960345961492,73.3439955270841,13.6229751006593));
#56104=CARTESIAN_POINT('Ctrl Pts',(15.4914464366581,73.3484430942568,13.5609530149312));
#56105=CARTESIAN_POINT('Ctrl Pts',(15.486858277167,73.34949519187,13.4988862016455));
#56106=CARTESIAN_POINT('Ctrl Pts',(15.482229235265,73.3505566641109,13.4362663472186));
#56107=CARTESIAN_POINT('Ctrl Pts',(15.477600193363,73.3481618118956,13.3736014875569));
#56108=CARTESIAN_POINT('Ctrl Pts',(15.472971151461,73.3423350717331,13.3112983997492));
#56109=CARTESIAN_POINT('Ctrl Pts',(15.4683772812649,73.3365526034514,13.2494686941073));
#56110=CARTESIAN_POINT('Ctrl Pts',(15.4637834110687,73.3273903518195,13.1879957816731));
#56111=CARTESIAN_POINT('Ctrl Pts',(15.4591895408726,73.3149240793806,13.127269517013));
#56112=CARTESIAN_POINT('Ctrl Pts',(15.4545429131177,73.3023146400532,13.0658458513937));
#56113=CARTESIAN_POINT('Ctrl Pts',(15.4498962853628,73.2863249258895,13.0051866114072));
#56114=CARTESIAN_POINT('Ctrl Pts',(15.4452496576078,73.2670851899437,12.9456795061059));
#56115=CARTESIAN_POINT('Ctrl Pts',(15.4406030298529,73.2478454539978,12.8861724008046));
#56116=CARTESIAN_POINT('Ctrl Pts',(15.4359564020979,73.2253559451803,12.8278179024466));
#56117=CARTESIAN_POINT('Ctrl Pts',(15.431309774343,73.1997959114136,12.7709805537892));
#56118=CARTESIAN_POINT('Ctrl Pts',(15.426705619554,73.1744695116935,12.7146627326055));
#56119=CARTESIAN_POINT('Ctrl Pts',(15.4221014647651,73.1460284107687,12.6596117718381));
#56120=CARTESIAN_POINT('Ctrl Pts',(15.4174973099762,73.1146219799088,12.6061935347818));
#56121=CARTESIAN_POINT('Ctrl Pts',(15.4128851028657,73.0831606215557,12.5526818732333));
#56122=CARTESIAN_POINT('Ctrl Pts',(15.4082728957552,73.0487237179752,12.5008091377367));
#56123=CARTESIAN_POINT('Ctrl Pts',(15.4036606886447,73.0115097905952,12.4509225369778));
#56124=CARTESIAN_POINT('Ctrl Pts',(15.3990687852806,72.9744596854649,12.4012555458042));
#56125=CARTESIAN_POINT('Ctrl Pts',(15.3944768819165,72.9346572372938,12.353557663944));
#56126=CARTESIAN_POINT('Ctrl Pts',(15.3898849785524,72.8923428010913,12.3081443779856));
#56127=CARTESIAN_POINT('Ctrl Pts',(15.3852957880814,72.8500533642259,12.2627579221624));
#56128=CARTESIAN_POINT('Ctrl Pts',(15.3807065976103,72.8052552276664,12.2196537557614));
#56129=CARTESIAN_POINT('Ctrl Pts',(15.3761174071393,72.758228311868,12.1791134891459));
#56130=CARTESIAN_POINT('Ctrl Pts',(15.3715292576111,72.7112120629463,12.1385824180735));
#56131=CARTESIAN_POINT('Ctrl Pts',(15.3669411080828,72.6619684226592,12.1006144229581));
#56132=CARTESIAN_POINT('Ctrl Pts',(15.3623529585546,72.6108118680941,12.0654521152545));
#56133=CARTESIAN_POINT('Ctrl Pts',(15.357723906952,72.5591992671029,12.0299763453778));
#56134=CARTESIAN_POINT('Ctrl Pts',(15.3530948553495,72.5056398879805,11.9973568613451));
#56135=CARTESIAN_POINT('Ctrl Pts',(15.348465803747,72.4504863152568,11.9677979960783));
#56136=CARTESIAN_POINT('Ctrl Pts',(15.3438719432836,72.3957520329663,11.9384638442582));
#56137=CARTESIAN_POINT('Ctrl Pts',(15.3392780828202,72.3394482025744,11.9121441018625));
#56138=CARTESIAN_POINT('Ctrl Pts',(15.3346842223568,72.2819416499901,11.8889909666837));
#56139=CARTESIAN_POINT('Ctrl Pts',(15.3300375751847,72.2237743064078,11.8655717855916));
#56140=CARTESIAN_POINT('Ctrl Pts',(15.3253909280126,72.1643769223286,11.8453926367438));
#56141=CARTESIAN_POINT('Ctrl Pts',(15.3207442808405,72.1041446427351,11.8285591121329));
#56142=CARTESIAN_POINT('Ctrl Pts',(15.3160976336684,72.0439123631416,11.811725587522));
#56143=CARTESIAN_POINT('Ctrl Pts',(15.3114509864963,71.9828457192163,11.798237740532));
#56144=CARTESIAN_POINT('Ctrl Pts',(15.3068043393242,71.9213476093244,11.7881475235598));
#56145=CARTESIAN_POINT('Ctrl Pts',(15.3022001718672,71.8604117160359,11.7781495514959));
#56146=CARTESIAN_POINT('Ctrl Pts',(15.2975960044103,71.79881131457,11.7714477650766));
#56147=CARTESIAN_POINT('Ctrl Pts',(15.2929918369534,71.7369338960352,11.7681197511351));
#56148=CARTESIAN_POINT('Ctrl Pts',(15.2883796314264,71.6749484503643,11.764785927064));
#56149=CARTESIAN_POINT('Ctrl Pts',(15.2837674258994,71.6126855166509,11.7648377959761));
#56150=CARTESIAN_POINT('Ctrl Pts',(15.2791552203724,71.550544182294,11.7683016690825));
#56151=CARTESIAN_POINT('Ctrl Pts',(15.274563304546,71.4886762158662,11.7717503041541));
#56152=CARTESIAN_POINT('Ctrl Pts',(15.2699713887197,71.4269292909023,11.7785809859631));
#56153=CARTESIAN_POINT('Ctrl Pts',(15.2653794728934,71.3656991640179,11.7887676311851));
#56154=CARTESIAN_POINT('Ctrl Pts',(15.2607902700722,71.3045052132431,11.7989482579124));
#56155=CARTESIAN_POINT('Ctrl Pts',(15.2562010672511,71.2438279543311,11.8124808326942));
#56156=CARTESIAN_POINT('Ctrl Pts',(15.2516118644299,71.1840567609523,11.8292875780976));
#56157=CARTESIAN_POINT('Ctrl Pts',(15.2470237026838,71.1242991268559,11.8460905108381));
#56158=CARTESIAN_POINT('Ctrl Pts',(15.2424355409376,71.0654476381596,11.8661660020247));
#56159=CARTESIAN_POINT('Ctrl Pts',(15.2378473791915,71.0078782486064,11.8893859256289));
#56160=CARTESIAN_POINT('Ctrl Pts',(15.2332183396177,70.9497959495882,11.9128127251212));
#56161=CARTESIAN_POINT('Ctrl Pts',(15.2285893000438,70.8930192079004,11.9394401021789));
#56162=CARTESIAN_POINT('Ctrl Pts',(15.22396026047,70.8379131137208,11.9690870231465));
#56163=CARTESIAN_POINT('Ctrl Pts',(15.2193663882507,70.7832256669776,11.9985087129915));
#56164=CARTESIAN_POINT('Ctrl Pts',(15.2147725160314,70.7301839795792,12.0309039078793));
#56165=CARTESIAN_POINT('Ctrl Pts',(15.210178643812,70.6791175554324,12.0660509008798));
#56166=CARTESIAN_POINT('Ctrl Pts',(15.205532020561,70.6274647400162,12.1016014837182));
#56167=CARTESIAN_POINT('Ctrl Pts',(15.2008853973099,70.5778332722583,12.1399671531862));
#56168=CARTESIAN_POINT('Ctrl Pts',(15.1962387740588,70.5305294428678,12.1808768575346));
#56169=CARTESIAN_POINT('Ctrl Pts',(15.1915921508077,70.4832256134773,12.2217865618831));
#56170=CARTESIAN_POINT('Ctrl Pts',(15.1869455275566,70.4382497603648,12.2652398878373));
#56171=CARTESIAN_POINT('Ctrl Pts',(15.1822989043055,70.3958677455696,12.3109296912015));
#56172=CARTESIAN_POINT('Ctrl Pts',(15.1776947235287,70.3538728500822,12.3562021617623));
#56173=CARTESIAN_POINT('Ctrl Pts',(15.173090542752,70.3142585503185,12.4038493581946));
#56174=CARTESIAN_POINT('Ctrl Pts',(15.1684863619753,70.2773035691007,12.4535911298298));
#56175=CARTESIAN_POINT('Ctrl Pts',(15.1638741581133,70.2402841914179,12.5034195797463));
#56176=CARTESIAN_POINT('Ctrl Pts',(15.1592619542512,70.2059337915272,12.5553495686052));
#56177=CARTESIAN_POINT('Ctrl Pts',(15.1546497503892,70.1744947529164,12.6090629583402));
#56178=CARTESIAN_POINT('Ctrl Pts',(15.1500578207962,70.1431939136448,12.6625402354172));
#56179=CARTESIAN_POINT('Ctrl Pts',(15.1454658912032,70.1147791748378,12.7177848420542));
#56180=CARTESIAN_POINT('Ctrl Pts',(15.1408739616102,70.0894474072078,12.77445247137));
#56181=CARTESIAN_POINT('Ctrl Pts',(15.1362847448956,70.064130605401,12.8310866218645));
#56182=CARTESIAN_POINT('Ctrl Pts',(15.131695528181,70.0418933691153,12.8891416656004));
#56183=CARTESIAN_POINT('Ctrl Pts',(15.1271063114665,70.022885951727,12.948250061086));
#56184=CARTESIAN_POINT('Ctrl Pts',(15.1225181357252,70.0038828457964,13.0073450489981));
#56185=CARTESIAN_POINT('Ctrl Pts',(15.1179299599839,69.988108259134,13.0674924315786));
#56186=CARTESIAN_POINT('Ctrl Pts',(15.1133417842426,69.9756630622344,13.1283080418545));
#56187=CARTESIAN_POINT('Ctrl Pts',(15.1087127579963,69.9631070603859,13.1896651197058));
#56188=CARTESIAN_POINT('Ctrl Pts',(15.1040837317499,69.9539401682231,13.2517018770536));
#56189=CARTESIAN_POINT('Ctrl Pts',(15.0994547055036,69.9482131515873,13.3140139840398));
#56190=CARTESIAN_POINT('Ctrl Pts',(15.094860819207,69.9425296099863,13.3758530662059));
#56191=CARTESIAN_POINT('Ctrl Pts',(15.0902669329104,69.9402338592575,13.4379628160748));
#56192=CARTESIAN_POINT('Ctrl Pts',(15.0856730466139,69.9413231041099,13.4999460931263));
#56193=CARTESIAN_POINT('Ctrl Pts',(15.0810264503927,69.9424248468802,13.5626405618899));
#56194=CARTESIAN_POINT('Ctrl Pts',(15.0763798541715,69.9469897370778,13.6252051050966));
#56195=CARTESIAN_POINT('Ctrl Pts',(15.0717332579503,69.9549610253152,13.6872346852293));
#56196=CARTESIAN_POINT('Ctrl Pts',(15.0670866617291,69.9629323135527,13.749264265362));
#56197=CARTESIAN_POINT('Ctrl Pts',(15.0624400655079,69.9743098420003,13.8107583724795));
#56198=CARTESIAN_POINT('Ctrl Pts',(15.0577934692867,69.9889844444823,13.8713257318424));
#56199=CARTESIAN_POINT('Ctrl Pts',(15.0531893714168,70.0035248312108,13.9313391345461));
#56200=CARTESIAN_POINT('Ctrl Pts',(15.048585273547,70.0213596651757,13.9906799489558));
#56201=CARTESIAN_POINT('Ctrl Pts',(15.0439811756772,70.0424093923433,14.0489610931354));
#56202=CARTESIAN_POINT('Ctrl Pts',(15.0393689614518,70.0634962271214,14.1073449785038));
#56203=CARTESIAN_POINT('Ctrl Pts',(15.0347567472264,70.087809226176,14.16466494563));
#56204=CARTESIAN_POINT('Ctrl Pts',(15.030144533001,70.1152170875011,14.2205431965559));
#56205=CARTESIAN_POINT('Ctrl Pts',(15.0255526864647,70.1425039148126,14.2761746872949));
#56206=CARTESIAN_POINT('Ctrl Pts',(15.0209608399285,70.1728581284923,14.3303766992204));
#56207=CARTESIAN_POINT('Ctrl Pts',(15.0163689933922,70.2061014787994,14.3827949399891));
#56208=CARTESIAN_POINT('Ctrl Pts',(15.0117798595527,70.2393251901385,14.4351822139586));
#56209=CARTESIAN_POINT('Ctrl Pts',(15.0071907257131,70.2754343820395,14.4857873791719));
#56210=CARTESIAN_POINT('Ctrl Pts',(15.0026015918736,70.3142056854256,14.5342821676815));
#56211=CARTESIAN_POINT('Ctrl Pts',(14.9980134986852,70.3529681968686,14.5827659593098));
#56212=CARTESIAN_POINT('Ctrl Pts',(14.9934254054969,70.3943913044572,14.6291399285655));
#56213=CARTESIAN_POINT('Ctrl Pts',(14.9888373123086,70.4382105014878,14.6731077883058));
#56214=CARTESIAN_POINT('Ctrl Pts',(14.9842082058052,70.4824214016638,14.7174686800986));
#56215=CARTESIAN_POINT('Ctrl Pts',(14.9795790993018,70.5290710975088,14.7593798349948));
#56216=CARTESIAN_POINT('Ctrl Pts',(14.9749499927984,70.5778505644227,14.7985755673648));
#56217=CARTESIAN_POINT('Ctrl Pts',(14.970356187313,70.6262580448987,14.8374723977215));
#56218=CARTESIAN_POINT('Ctrl Pts',(14.9657623818276,70.6767624744858,14.8736948247573));
#56219=CARTESIAN_POINT('Ctrl Pts',(14.9611685763422,70.7290312669044,14.9070258106954));
#56220=CARTESIAN_POINT('Ctrl Pts',(14.9565218193298,70.7819025472562,14.9407409937022));
#56221=CARTESIAN_POINT('Ctrl Pts',(14.9518750623174,70.836578670003,14.9714973752288));
#56222=CARTESIAN_POINT('Ctrl Pts',(14.9472283053051,70.8926906051386,14.9991185050504));
#56223=CARTESIAN_POINT('Ctrl Pts',(14.9425815482927,70.9488025402743,15.0267396348719));
#56224=CARTESIAN_POINT('Ctrl Pts',(14.9379347912803,71.0063497753763,15.0512253628403));
#56225=CARTESIAN_POINT('Ctrl Pts',(14.9332880342679,71.0649457963341,15.0724505462093));
#56226=CARTESIAN_POINT('Ctrl Pts',(14.9279993725813,71.1316362925666,15.0966077839939));
#56227=CARTESIAN_POINT('Ctrl Pts',(14.9227107108947,71.1999016312767,15.1166213767754));
#56228=CARTESIAN_POINT('Ctrl Pts',(14.917422049208,71.2692533052774,15.1323142000384));
#56229=CARTESIAN_POINT('Ctrl Pts',(14.9121766025752,71.3380382884026,15.1478787930909));
#56230=CARTESIAN_POINT('Ctrl Pts',(14.9069311559423,71.4078917346752,15.1591928399152));
#56231=CARTESIAN_POINT('Ctrl Pts',(14.9016857093095,71.478316607017,15.1661302943434));
#56232=CARTESIAN_POINT('Ctrl Pts',(14.8975855010802,71.5333656164401,15.171553094293));
#56233=CARTESIAN_POINT('Ctrl Pts',(14.893485292851,71.5887633394563,15.1743026527472));
#56234=CARTESIAN_POINT('Ctrl Pts',(14.8893850846217,71.6442647494568,15.1743396219082));
#56235=CARTESIAN_POINT('',(14.0956350845187,71.6466915584598,15.1743395106248));
#56236=CARTESIAN_POINT('Ctrl Pts',(14.8893850845702,71.6442647501543,15.1743396219087));
#56237=CARTESIAN_POINT('Ctrl Pts',(14.8847838848648,71.706547701914,15.174381108189));
#56238=CARTESIAN_POINT('Ctrl Pts',(14.8801826851594,71.7688576998196,15.1710041874919));
#56239=CARTESIAN_POINT('Ctrl Pts',(14.875581485454,71.8307953836467,15.1642264864305));
#56240=CARTESIAN_POINT('Ctrl Pts',(14.8709803942258,71.8927316072403,15.1574489451591));
#56241=CARTESIAN_POINT('Ctrl Pts',(14.8663793029975,71.9542950347125,15.1472708391474));
#56242=CARTESIAN_POINT('Ctrl Pts',(14.8617782117693,72.0150920328097,15.1337615924396));
#56243=CARTESIAN_POINT('Ctrl Pts',(14.8571720998765,72.0759553719816,15.1202376045772));
#56244=CARTESIAN_POINT('Ctrl Pts',(14.8525659879837,72.1360501195801,15.1033753258721));
#56245=CARTESIAN_POINT('Ctrl Pts',(14.8479598760909,72.194994496164,15.0832949901944));
#56246=CARTESIAN_POINT('Ctrl Pts',(14.8433512710408,72.2539707776611,15.0632037856025));
#56247=CARTESIAN_POINT('Ctrl Pts',(14.8387426659907,72.3117949807797,15.0398912423987));
#56248=CARTESIAN_POINT('Ctrl Pts',(14.8341340609407,72.3681050013233,15.0135259365046));
#56249=CARTESIAN_POINT('Ctrl Pts',(14.8295163898702,72.4245257946042,14.9871087649376));
#56250=CARTESIAN_POINT('Ctrl Pts',(14.8248987187997,72.4794260101098,14.9576270709721));
#56251=CARTESIAN_POINT('Ctrl Pts',(14.8202810477292,72.5324685061645,14.9252952624712));
#56252=CARTESIAN_POINT('Ctrl Pts',(14.8164482315691,72.5764954914006,14.8984588169529));
#56253=CARTESIAN_POINT('Ctrl Pts',(14.8126154154091,72.6192429818788,14.8696596754254));
#56254=CARTESIAN_POINT('Ctrl Pts',(14.8087825992491,72.6605353656926,14.839041644699));
#56255=CARTESIAN_POINT('Ctrl Pts',(14.8041783207442,72.7101390062721,14.8022608718026));
#56256=CARTESIAN_POINT('Ctrl Pts',(14.7995740422393,72.7578391002769,14.762708075234));
#56257=CARTESIAN_POINT('Ctrl Pts',(14.7949697637345,72.803310164833,14.7206074067334));
#56258=CARTESIAN_POINT('Ctrl Pts',(14.7903575720885,72.8488593782131,14.6784343819384));
#56259=CARTESIAN_POINT('Ctrl Pts',(14.7857453804425,72.8921714543769,14.6337049862599));
#56260=CARTESIAN_POINT('Ctrl Pts',(14.7811331887965,72.9329496690055,14.5866873713998));
#56261=CARTESIAN_POINT('Ctrl Pts',(14.7765411590811,72.9735496240125,14.5398752913408));
#56262=CARTESIAN_POINT('Ctrl Pts',(14.7719491293658,73.011637470106,14.4907953222569));
#56263=CARTESIAN_POINT('Ctrl Pts',(14.7673570996505,73.0469563879207,14.4397497239385));
#56264=CARTESIAN_POINT('Ctrl Pts',(14.7627677822103,73.0822544446723,14.388734275622));
#56265=CARTESIAN_POINT('Ctrl Pts',(14.7581784647701,73.114786528635,14.3357559168311));
#56266=CARTESIAN_POINT('Ctrl Pts',(14.7535891473299,73.1443373721587,14.2811483156279));
#56267=CARTESIAN_POINT('Ctrl Pts',(14.7490008704379,73.1738815155408,14.2265530957517));
#56268=CARTESIAN_POINT('Ctrl Pts',(14.7444125935458,73.2004455195007,14.1703298128512));
#56269=CARTESIAN_POINT('Ctrl Pts',(14.7398243166538,73.2238596012906,14.1128375554472));
#56270=CARTESIAN_POINT('Ctrl Pts',(14.7351953872852,73.2474811335972,14.0548359123408));
#56271=CARTESIAN_POINT('Ctrl Pts',(14.7305664579166,73.2678964206968,13.9955431691668));
#56272=CARTESIAN_POINT('Ctrl Pts',(14.725937528548,73.2849812384895,13.935347394957));
#56273=CARTESIAN_POINT('Ctrl Pts',(14.7213435412563,73.3019370893071,13.8756060163989));
#56274=CARTESIAN_POINT('Ctrl Pts',(14.7167495539647,73.315612522751,13.8149757075223));
#56275=CARTESIAN_POINT('Ctrl Pts',(14.7121555666731,73.3259372675668,13.7538473672929));
#56276=CARTESIAN_POINT('Ctrl Pts',(14.707509166266,73.336379808103,13.6920216096451));
#56277=CARTESIAN_POINT('Ctrl Pts',(14.7028627658589,73.343394642505,13.6296869111642));
#56278=CARTESIAN_POINT('Ctrl Pts',(14.6982163654517,73.3469630837017,13.5672517752208));
#56279=CARTESIAN_POINT('Ctrl Pts',(14.6935699650446,73.3505315248984,13.5048166392774));
#56280=CARTESIAN_POINT('Ctrl Pts',(14.6889235646375,73.3506536342372,13.4422815959432));
#56281=CARTESIAN_POINT('Ctrl Pts',(14.6842771642304,73.3473647645392,13.3800512597816));
#56282=CARTESIAN_POINT('Ctrl Pts',(14.6796735451174,73.3441061767993,13.3183939035797));
#56283=CARTESIAN_POINT('Ctrl Pts',(14.6750699260045,73.3374863237172,13.256791804077));
#56284=CARTESIAN_POINT('Ctrl Pts',(14.6704663068915,73.3275121922856,13.1956400026169));
#56285=CARTESIAN_POINT('Ctrl Pts',(14.6658540328215,73.3175193091552,13.1343732337361));
#56286=CARTESIAN_POINT('Ctrl Pts',(14.6612417587516,73.3041595013438,13.0735589715084));
#56287=CARTESIAN_POINT('Ctrl Pts',(14.6566294846816,73.2874923525458,13.0135927900321));
#56288=CARTESIAN_POINT('Ctrl Pts',(14.6520381171708,73.2709007527565,12.953898423827));
#56289=CARTESIAN_POINT('Ctrl Pts',(14.6474467496601,73.2510318408939,12.8950449644891));
#56290=CARTESIAN_POINT('Ctrl Pts',(14.6428553821494,73.2279956529882,12.8374133776764));
#56291=CARTESIAN_POINT('Ctrl Pts',(14.6382667260684,73.2049730690915,12.7798158251677));
#56292=CARTESIAN_POINT('Ctrl Pts',(14.6336780699874,73.1787871065311,12.7234391843144));
#56293=CARTESIAN_POINT('Ctrl Pts',(14.6290894139064,73.1495969370155,12.6686471374774));
#56294=CARTESIAN_POINT('Ctrl Pts',(14.6245017964041,73.1204133742902,12.6138674920607));
#56295=CARTESIAN_POINT('Ctrl Pts',(14.6199141789018,73.0882271932799,12.5606721760087));
#56296=CARTESIAN_POINT('Ctrl Pts',(14.6153265613995,73.0532438821944,12.5094009999132));
#56297=CARTESIAN_POINT('Ctrl Pts',(14.6106969920505,73.0179406633348,12.4576609703183));
#56298=CARTESIAN_POINT('Ctrl Pts',(14.6060674227015,72.9797891625929,12.4078809045185));
#56299=CARTESIAN_POINT('Ctrl Pts',(14.6014378533525,72.9390444113478,12.3603789058474));
#56300=CARTESIAN_POINT('Ctrl Pts',(14.5968445129989,72.8986185107977,12.3132486371493));
#56301=CARTESIAN_POINT('Ctrl Pts',(14.5922511726452,72.8556402011786,12.2683612386279));
#56302=CARTESIAN_POINT('Ctrl Pts',(14.5876578322916,72.8103964656305,12.2259911291842));
#56303=CARTESIAN_POINT('Ctrl Pts',(14.5830101484449,72.7646174545664,12.1831197418968));
#56304=CARTESIAN_POINT('Ctrl Pts',(14.5783624645983,72.7165194588078,12.1428259543845));
#56305=CARTESIAN_POINT('Ctrl Pts',(14.5737147807516,72.6664330419732,12.1053511943365));
#56306=CARTESIAN_POINT('Ctrl Pts',(14.5690670969049,72.6163466251387,12.0678764342884));
#56307=CARTESIAN_POINT('Ctrl Pts',(14.5644194130582,72.5642722641935,12.0332209438036));
#56308=CARTESIAN_POINT('Ctrl Pts',(14.5597717292116,72.5105671637858,12.0015788702464));
#56309=CARTESIAN_POINT('Ctrl Pts',(14.5551668265409,72.4573564101171,11.9702280568444));
#56310=CARTESIAN_POINT('Ctrl Pts',(14.5505619238703,72.4023343486674,11.9417113462341));
#56311=CARTESIAN_POINT('Ctrl Pts',(14.5459570211996,72.3458343412366,11.9162411483063));
#56312=CARTESIAN_POINT('Ctrl Pts',(14.5413449075743,72.2892458587566,11.8907310658349));
#56313=CARTESIAN_POINT('Ctrl Pts',(14.536732793949,72.2311752148467,11.8682773441838));
#56314=CARTESIAN_POINT('Ctrl Pts',(14.5321206803237,72.1719849151098,11.8490486858703));
#56315=CARTESIAN_POINT('Ctrl Pts',(14.5275280398947,72.1130445277594,11.8299012145065));
#56316=CARTESIAN_POINT('Ctrl Pts',(14.5229353994657,72.0529943950421,11.8139518123152));
#56317=CARTESIAN_POINT('Ctrl Pts',(14.5183427590366,71.9922130427281,11.8013192189656));
#56318=CARTESIAN_POINT('Ctrl Pts',(14.5137528376327,71.9314676753825,11.7886941046116));
#56319=CARTESIAN_POINT('Ctrl Pts',(14.5091629162287,71.8699924424387,11.7793820076052));
#56320=CARTESIAN_POINT('Ctrl Pts',(14.5045729948247,71.8081786019903,11.7734511612293));
#56321=CARTESIAN_POINT('Ctrl Pts',(14.4999841216952,71.7463788789666,11.7675216693766));
#56322=CARTESIAN_POINT('Ctrl Pts',(14.4953952485657,71.6842412064689,11.764971943071));
#56323=CARTESIAN_POINT('Ctrl Pts',(14.4908063754362,71.6221625296889,11.7658184205979));
#56324=CARTESIAN_POINT('Ctrl Pts',(14.4861780353326,71.5595499402336,11.7666721783231));
#56325=CARTESIAN_POINT('Ctrl Pts',(14.481549695229,71.4969978898257,11.7709808662977));
#56326=CARTESIAN_POINT('Ctrl Pts',(14.4769213551254,71.4349119549069,11.7787077075583));
#56327=CARTESIAN_POINT('Ctrl Pts',(14.4723267972193,71.3732791844643,11.7863781506993));
#56328=CARTESIAN_POINT('Ctrl Pts',(14.4677322393132,71.312106243243,11.7974168674359));
#56329=CARTESIAN_POINT('Ctrl Pts',(14.4631376814072,71.251780603494,11.8117362675695));
#56330=CARTESIAN_POINT('Ctrl Pts',(14.4584924502048,71.1907896333514,11.8262135961092));
#56331=CARTESIAN_POINT('Ctrl Pts',(14.4538472190024,71.1306652827134,11.8440442820284));
#56332=CARTESIAN_POINT('Ctrl Pts',(14.4492019878,71.0717907212702,11.8650865347456));
#56333=CARTESIAN_POINT('Ctrl Pts',(14.4445567565976,71.0129161598269,11.8861287874627));
#56334=CARTESIAN_POINT('Ctrl Pts',(14.4399115253952,70.9552918509495,11.9103823446695));
#56335=CARTESIAN_POINT('Ctrl Pts',(14.4352662941928,70.8992763763392,11.9376572270489));
#56336=CARTESIAN_POINT('Ctrl Pts',(14.4306615361222,70.8437489553025,11.9646944678855));
#56337=CARTESIAN_POINT('Ctrl Pts',(14.4260567780516,70.7895836007335,11.9948070939335));
#56338=CARTESIAN_POINT('Ctrl Pts',(14.4214520199811,70.7371414975494,12.0278345003689));
#56339=CARTESIAN_POINT('Ctrl Pts',(14.4168398882808,70.6846154184768,12.0609147938098));
#56340=CARTESIAN_POINT('Ctrl Pts',(14.4122277565805,70.6338185941214,12.0969190279969));
#56341=CARTESIAN_POINT('Ctrl Pts',(14.4076156248802,70.5850918980863,12.1356381432999));
#56342=CARTESIAN_POINT('Ctrl Pts',(14.4030230932803,70.5365722750922,12.1741927146136));
#56343=CARTESIAN_POINT('Ctrl Pts',(14.3984305616805,70.490105637244,12.215438844973));
#56344=CARTESIAN_POINT('Ctrl Pts',(14.3938380300807,70.4460000194499,12.2591265457297));
#56345=CARTESIAN_POINT('Ctrl Pts',(14.3892482038997,70.4019203838768,12.3027885104566));
#56346=CARTESIAN_POINT('Ctrl Pts',(14.3846583777187,70.3601993694717,12.3488888369503));
#56347=CARTESIAN_POINT('Ctrl Pts',(14.3800685515377,70.3211099353246,12.3971390303482));
#56348=CARTESIAN_POINT('Ctrl Pts',(14.3754797599858,70.2820293126359,12.4453783472886));
#56349=CARTESIAN_POINT('Ctrl Pts',(14.3708909684338,70.2455794112319,12.4957661749858));
#56350=CARTESIAN_POINT('Ctrl Pts',(14.3663021768819,70.211993149495,12.5479806745381));
#56351=CARTESIAN_POINT('Ctrl Pts',(14.3616737337395,70.1781166700228,12.6006463577894));
#56352=CARTESIAN_POINT('Ctrl Pts',(14.3570452905972,70.1471538701477,12.6551700120064));
#56353=CARTESIAN_POINT('Ctrl Pts',(14.3524168474549,70.1192980902112,12.7111931757429));
#56354=CARTESIAN_POINT('Ctrl Pts',(14.3478223372381,70.0916465318836,12.766805611772));
#56355=CARTESIAN_POINT('Ctrl Pts',(14.3432278270213,70.0670567385342,12.8238951491533));
#56356=CARTESIAN_POINT('Ctrl Pts',(14.3386333168044,70.0456696681031,12.8820903974172));
#56357=CARTESIAN_POINT('Ctrl Pts',(14.3339879071994,70.0240456651701,12.9409303504252));
#56358=CARTESIAN_POINT('Ctrl Pts',(14.3293424975943,70.0056959548617,13.0009001610863));
#56359=CARTESIAN_POINT('Ctrl Pts',(14.3246970879893,69.9907139442805,13.0616020413769));
#56360=CARTESIAN_POINT('Ctrl Pts',(14.3200516783842,69.9757319336994,13.1223039216675));
#56361=CARTESIAN_POINT('Ctrl Pts',(14.3154062687791,69.964117659956,13.1837373402832));
#56362=CARTESIAN_POINT('Ctrl Pts',(14.3107608591741,69.9559107672478,13.2454984008646));
#56363=CARTESIAN_POINT('Ctrl Pts',(14.3061611205119,69.9477845598957,13.3066522629185));
#56364=CARTESIAN_POINT('Ctrl Pts',(14.3015613818498,69.9429667228472,13.3683702260757));
#56365=CARTESIAN_POINT('Ctrl Pts',(14.2969616431876,69.9415232932443,13.4302633195206));
#56366=CARTESIAN_POINT('Ctrl Pts',(14.2923488840613,69.9400757777304,13.4923316135295));
#56367=CARTESIAN_POINT('Ctrl Pts',(14.2877361249349,69.9420219261382,13.5545755284543));
#56368=CARTESIAN_POINT('Ctrl Pts',(14.2831233658086,69.9473761995002,13.6165947084177));
#56369=CARTESIAN_POINT('Ctrl Pts',(14.2785358895706,69.9527011256771,13.6782739564746));
#56370=CARTESIAN_POINT('Ctrl Pts',(14.2739484133326,69.9613968904335,13.7397304151198));
#56371=CARTESIAN_POINT('Ctrl Pts',(14.2693609370947,69.9734256073589,13.8005699108396));
#56372=CARTESIAN_POINT('Ctrl Pts',(14.2647761653569,69.9854472328759,13.86137353925));
#56373=CARTESIAN_POINT('Ctrl Pts',(14.2601913936191,70.0007978156185,13.9215604283667));
#56374=CARTESIAN_POINT('Ctrl Pts',(14.2556066218814,70.0193879899528,13.9807443379835));
#56375=CARTESIAN_POINT('Ctrl Pts',(14.2510228753126,70.0379740074674,14.0399150138973));
#56376=CARTESIAN_POINT('Ctrl Pts',(14.2464391287438,70.0597980259357,14.0980826709205));
#56377=CARTESIAN_POINT('Ctrl Pts',(14.241855382175,70.0847207610753,14.1548760097927));
#56378=CARTESIAN_POINT('Ctrl Pts',(14.23722205234,70.1099130902232,14.2122836931091));
#56379=CARTESIAN_POINT('Ctrl Pts',(14.232588722505,70.1382714009772,14.268286646983));
#56380=CARTESIAN_POINT('Ctrl Pts',(14.22795539267,70.1696027349112,14.3225240571129));
#56381=CARTESIAN_POINT('Ctrl Pts',(14.2233658460228,70.2006379997706,14.3762489445442));
#56382=CARTESIAN_POINT('Ctrl Pts',(14.2187762993756,70.2345900042183,14.42824111596));
#56383=CARTESIAN_POINT('Ctrl Pts',(14.2141867527284,70.2712272732066,14.478178631264));
#56384=CARTESIAN_POINT('Ctrl Pts',(14.2095315312995,70.3083888084951,14.5288307346667));
#56385=CARTESIAN_POINT('Ctrl Pts',(14.2048763098707,70.3483127374649,14.5773684850226));
#56386=CARTESIAN_POINT('Ctrl Pts',(14.2002210884418,70.3907166117566,14.6234922760323));
#56387=CARTESIAN_POINT('Ctrl Pts',(14.195565867013,70.4331204860483,14.6696160670419));
#56388=CARTESIAN_POINT('Ctrl Pts',(14.1909106455841,70.4780038747041,14.7133255692536));
#56389=CARTESIAN_POINT('Ctrl Pts',(14.1862554241553,70.5250491772928,14.7543632156284));
#56390=CARTESIAN_POINT('Ctrl Pts',(14.1816850784947,70.571236732025,14.7946526480205));
#56391=CARTESIAN_POINT('Ctrl Pts',(14.1771147328342,70.6196991503876,14.8325335042692));
#56392=CARTESIAN_POINT('Ctrl Pts',(14.1725443871736,70.6701535700373,14.8677371843251));
#56393=CARTESIAN_POINT('Ctrl Pts',(14.1679804721886,70.7205369981191,14.9028913312685));
#56394=CARTESIAN_POINT('Ctrl Pts',(14.1634165572037,70.7729064546098,14.9353754743146));
#56395=CARTESIAN_POINT('Ctrl Pts',(14.1588526422187,70.8269450467072,14.9649603088479));
#56396=CARTESIAN_POINT('Ctrl Pts',(14.154293423454,70.8809280336649,14.9945147008993));
#56397=CARTESIAN_POINT('Ctrl Pts',(14.1497342046893,70.9365763011329,15.0211754531287));
#56398=CARTESIAN_POINT('Ctrl Pts',(14.1451749859246,70.9935447046724,15.0447569684092));
#56399=CARTESIAN_POINT('Ctrl Pts',(14.1406177721829,71.0504880550248,15.0683281131671));
#56400=CARTESIAN_POINT('Ctrl Pts',(14.1360605584412,71.1087499187007,15.0888225003503));
#56401=CARTESIAN_POINT('Ctrl Pts',(14.1315033446995,71.1679630181875,15.1061016973274));
#56402=CARTESIAN_POINT('Ctrl Pts',(14.1269474062919,71.227159546917,15.1233760587296));
#56403=CARTESIAN_POINT('Ctrl Pts',(14.1223914678843,71.2873062868815,15.1374368764556));
#56404=CARTESIAN_POINT('Ctrl Pts',(14.1178355294766,71.3480208531988,15.1481956020225));
#56405=CARTESIAN_POINT('Ctrl Pts',(14.1132769416049,71.4087707275143,15.1589605842275));
#56406=CARTESIAN_POINT('Ctrl Pts',(14.1087183537331,71.4700885788062,15.1664195531591));
#56407=CARTESIAN_POINT('Ctrl Pts',(14.1041597658614,71.5315834484369,15.1705353945715));
#56408=CARTESIAN_POINT('Ctrl Pts',(14.101318205431,71.5699157989656,15.1731009724268));
#56409=CARTESIAN_POINT('Ctrl Pts',(14.0984766450006,71.6083168025979,15.1743685912238));
#56410=CARTESIAN_POINT('Ctrl Pts',(14.0956350845702,71.6466915577646,15.1743395106253));
#56411=CARTESIAN_POINT('',(13.9390000020058,73.2573116306334,14.0236386281943));
#56412=CARTESIAN_POINT('Ctrl Pts',(14.0956350845187,71.6466915584598,15.1743395106248));
#56413=CARTESIAN_POINT('Ctrl Pts',(14.0899102231617,71.7240047665774,15.174280922223));
#56414=CARTESIAN_POINT('Ctrl Pts',(14.0841853618047,71.8010986838953,15.1689576896067));
#56415=CARTESIAN_POINT('Ctrl Pts',(14.0784605004477,71.8773531425193,15.1584823289793));
#56416=CARTESIAN_POINT('Ctrl Pts',(14.0728903300106,71.9515471368597,15.148290022049));
#56417=CARTESIAN_POINT('Ctrl Pts',(14.0673201595735,72.0249466919968,15.1332206059659));
#56418=CARTESIAN_POINT('Ctrl Pts',(14.0617499891365,72.0969995652456,15.1134210258695));
#56419=CARTESIAN_POINT('Ctrl Pts',(14.0571556162791,72.1564300205421,15.0970899899683));
#56420=CARTESIAN_POINT('Ctrl Pts',(14.0525612434217,72.2150920063269,15.0774984774246));
#56421=CARTESIAN_POINT('Ctrl Pts',(14.0479668705642,72.2726022507899,15.0547372565205));
#56422=CARTESIAN_POINT('Ctrl Pts',(14.0433801850032,72.3300162692153,15.0320141196502));
#56423=CARTESIAN_POINT('Ctrl Pts',(14.0387934994422,72.3862819023425,15.0061319904094));
#56424=CARTESIAN_POINT('Ctrl Pts',(14.0342068138811,72.4410305366652,14.9772315299004));
#56425=CARTESIAN_POINT('Ctrl Pts',(14.0296244126719,72.4957280311387,14.9483580648627));
#56426=CARTESIAN_POINT('Ctrl Pts',(14.0250420114626,72.5489108869029,14.9164720935188));
#56427=CARTESIAN_POINT('Ctrl Pts',(14.0204596102533,72.6002315075143,14.8817618878047));
#56428=CARTESIAN_POINT('Ctrl Pts',(14.015879802325,72.6515230846649,14.8470713253547));
#56429=CARTESIAN_POINT('Ctrl Pts',(14.0112999943968,72.7009540952428,14.8095599829552));
#56430=CARTESIAN_POINT('Ctrl Pts',(14.0067201864685,72.7482043460189,14.7694604303333));
#56431=CARTESIAN_POINT('Ctrl Pts',(14.0021412843155,72.7954452518376,14.7293688084334));
#56432=CARTESIAN_POINT('Ctrl Pts',(13.9975623821625,72.8405058661429,14.6866903225734));
#56433=CARTESIAN_POINT('Ctrl Pts',(13.9929834800095,72.883099252963,14.6416976550351));
#56434=CARTESIAN_POINT('Ctrl Pts',(13.9884005179902,72.9257304050486,14.5966650949181));
#56435=CARTESIAN_POINT('Ctrl Pts',(13.9838175559709,72.9658896065511,14.5493146232578));
#56436=CARTESIAN_POINT('Ctrl Pts',(13.9792345939516,73.0033278615039,14.4999547361663));
#56437=CARTESIAN_POINT('Ctrl Pts',(13.9746497437218,73.0407815412642,14.4505745124765));
#56438=CARTESIAN_POINT('Ctrl Pts',(13.9700648934919,73.0755117530719,14.3991836455102));
#56439=CARTESIAN_POINT('Ctrl Pts',(13.9654800432621,73.1073126056581,14.3461200654122));
#56440=CARTESIAN_POINT('Ctrl Pts',(13.9608866089702,73.1391729979194,14.292957136144));
#56441=CARTESIAN_POINT('Ctrl Pts',(13.9562931746783,73.1680928320662,14.2381156874062));
#56442=CARTESIAN_POINT('Ctrl Pts',(13.9516997403865,73.1939123920431,14.1819580094984));
#56443=CARTESIAN_POINT('Ctrl Pts',(13.9474664942596,73.2177073448659,14.1302038627333));
#56444=CARTESIAN_POINT('Ctrl Pts',(13.9432332481327,73.2388696027766,14.0773323512853));
#56445=CARTESIAN_POINT('Ctrl Pts',(13.9390000020058,73.2573116306334,14.0236386281943));
#56446=CARTESIAN_POINT('',(13.939,72.0984538423728,15.1130207093982));
#56447=CARTESIAN_POINT('Origin',(13.939,71.6454,13.47));
#56448=CARTESIAN_POINT('',(13.9729899143421,71.6451742442358,15.171860356376));
#56449=CARTESIAN_POINT('Ctrl Pts',(13.939,72.0984538423728,15.1130207093982));
#56450=CARTESIAN_POINT('Ctrl Pts',(13.9447857228067,72.0232055254717,15.1337700151793));
#56451=CARTESIAN_POINT('Ctrl Pts',(13.9505714456135,71.9465687943793,15.1493352443956));
#56452=CARTESIAN_POINT('Ctrl Pts',(13.9563571684203,71.8691762668991,15.1595854574341));
#56453=CARTESIAN_POINT('Ctrl Pts',(13.9619014045005,71.7950139785347,15.1694078431334));
#56454=CARTESIAN_POINT('Ctrl Pts',(13.9674456405806,71.720157559446,15.1743499093407));
#56455=CARTESIAN_POINT('Ctrl Pts',(13.9729898766608,71.6451744249067,15.1743399850722));
#56456=CARTESIAN_POINT('',(14.766739959622,71.6442542797994,15.1740410878602));
#56457=CARTESIAN_POINT('Ctrl Pts',(13.9729899154298,71.6451742390203,15.1717887764722));
#56458=CARTESIAN_POINT('Ctrl Pts',(14.0031617552928,71.2377257485833,15.1690257382362));
#56459=CARTESIAN_POINT('Ctrl Pts',(14.0748354068288,70.2684391229546,14.8219893666021));
#56460=CARTESIAN_POINT('Ctrl Pts',(14.1880108700375,69.6552364071702,13.2070658961577));
#56461=CARTESIAN_POINT('Ctrl Pts',(14.3125163050564,70.7660383371287,11.6669646452173));
#56462=CARTESIAN_POINT('Ctrl Pts',(14.4370217400751,72.6622260268806,11.7404213989368));
#56463=CARTESIAN_POINT('Ctrl Pts',(14.5615271750938,73.6490321077662,13.362480576396));
#56464=CARTESIAN_POINT('Ctrl Pts',(14.6714332335455,72.9363884810012,14.879191736923));
#56465=CARTESIAN_POINT('Ctrl Pts',(14.7398374803241,72.0080403161166,15.1703558387755));
#56466=CARTESIAN_POINT('Ctrl Pts',(14.7667399154298,71.6442558079889,15.1726571393383));
#56467=CARTESIAN_POINT('',(15.5604899154688,71.6456305596758,15.1743399844052));
#56468=CARTESIAN_POINT('Ctrl Pts',(14.7667399691545,71.6442539501588,15.1743396146806));
#56469=CARTESIAN_POINT('Ctrl Pts',(14.7719829711192,71.5732864489064,15.1742918939724));
#56470=CARTESIAN_POINT('Ctrl Pts',(14.7772259730839,71.5024894639145,15.1698075684678));
#56471=CARTESIAN_POINT('Ctrl Pts',(14.7824689750485,71.4323729178381,15.160974363456));
#56472=CARTESIAN_POINT('Ctrl Pts',(14.787757410458,71.3616487740059,15.1520646139503));
#56473=CARTESIAN_POINT('Ctrl Pts',(14.7930458458675,71.2916171145709,15.1387304010231));
#56474=CARTESIAN_POINT('Ctrl Pts',(14.7983342812769,71.2227823845175,15.121111500379));
#56475=CARTESIAN_POINT('Ctrl Pts',(14.8024022025617,71.1698339712652,15.1075588528763));
#56476=CARTESIAN_POINT('Ctrl Pts',(14.8064701238466,71.1175934009965,15.0914720431421));
#56477=CARTESIAN_POINT('Ctrl Pts',(14.8105380451314,71.0662816943619,15.0729338176216));
#56478=CARTESIAN_POINT('Ctrl Pts',(14.8151416958287,71.0082124355223,15.0519541798978));
#56479=CARTESIAN_POINT('Ctrl Pts',(14.819745346526,70.9511696380993,15.0277734201126));
#56480=CARTESIAN_POINT('Ctrl Pts',(14.8243489972233,70.8955293886369,15.0005126271331));
#56481=CARTESIAN_POINT('Ctrl Pts',(14.8289612673452,70.8397849638209,14.9732007937148));
#56482=CARTESIAN_POINT('Ctrl Pts',(14.8335735374672,70.78544884212,14.9427975104087));
#56483=CARTESIAN_POINT('Ctrl Pts',(14.8381858075891,70.7328823826295,14.9094743601705));
#56484=CARTESIAN_POINT('Ctrl Pts',(14.8427771879991,70.6805540050749,14.8763021358308));
#56485=CARTESIAN_POINT('Ctrl Pts',(14.847368568409,70.6299797387178,14.8402366865257));
#56486=CARTESIAN_POINT('Ctrl Pts',(14.851959948819,70.5814923562384,14.8014936579442));
#56487=CARTESIAN_POINT('Ctrl Pts',(14.856548610765,70.533033682162,14.7627735683299));
#56488=CARTESIAN_POINT('Ctrl Pts',(14.861137272711,70.4866598370754,14.7213793595562));
#56489=CARTESIAN_POINT('Ctrl Pts',(14.865725934657,70.4426728224686,14.6775687028188));
#56490=CARTESIAN_POINT('Ctrl Pts',(14.8703135510013,70.3986958310231,14.6337680290566));
#56491=CARTESIAN_POINT('Ctrl Pts',(14.8749011673457,70.3571049493374,14.5875523585866));
#56492=CARTESIAN_POINT('Ctrl Pts',(14.87948878369,70.318165917844,14.5392167819313));
#56493=CARTESIAN_POINT('Ctrl Pts',(14.8841183417283,70.2788708912493,14.4904393034657));
#56494=CARTESIAN_POINT('Ctrl Pts',(14.8887478997666,70.2422768074236,14.4395033453739));
#56495=CARTESIAN_POINT('Ctrl Pts',(14.893377457805,70.2086142824763,14.3867451322587));
#56496=CARTESIAN_POINT('Ctrl Pts',(14.89797077985,70.1752152373298,14.334399862721));
#56497=CARTESIAN_POINT('Ctrl Pts',(14.902564101895,70.1447022241691,14.2802612397332));
#56498=CARTESIAN_POINT('Ctrl Pts',(14.90715742394,70.1172547941091,14.2246834205895));
#56499=CARTESIAN_POINT('Ctrl Pts',(14.911805099975,70.0894825713773,14.1684479344682));
#56500=CARTESIAN_POINT('Ctrl Pts',(14.9164527760101,70.0648491854927,14.1107394511286));
#56501=CARTESIAN_POINT('Ctrl Pts',(14.9211004520451,70.043489991238,14.0519442923754));
#56502=CARTESIAN_POINT('Ctrl Pts',(14.9257481280801,70.0221307969833,13.9931491336223));
#56503=CARTESIAN_POINT('Ctrl Pts',(14.9303958041151,70.0040458880126,13.933267826093));
#56504=CARTESIAN_POINT('Ctrl Pts',(14.9350434801501,69.9893176493714,13.8726985020292));
#56505=CARTESIAN_POINT('Ctrl Pts',(14.9396477604633,69.9747269294693,13.8126947185755));
#56506=CARTESIAN_POINT('Ctrl Pts',(14.9442520407764,69.9633726913063,13.7517783712946));
#56507=CARTESIAN_POINT('Ctrl Pts',(14.9488563210896,69.9553616753097,13.6903299722646));
#56508=CARTESIAN_POINT('Ctrl Pts',(14.9534685125096,69.9473368947291,13.6287759921632));
#56509=CARTESIAN_POINT('Ctrl Pts',(14.9580807039295,69.9426670021147,13.5666886161985));
#56510=CARTESIAN_POINT('Ctrl Pts',(14.9626928953495,69.9414084847753,13.5044637728968));
#56511=CARTESIAN_POINT('Ctrl Pts',(14.967284925864,69.9401554686927,13.4425109281029));
#56512=CARTESIAN_POINT('Ctrl Pts',(14.9718769563785,69.9422841044234,13.3804223235053));
#56513=CARTESIAN_POINT('Ctrl Pts',(14.976468986893,69.9477983883997,13.3185945711275));
#56514=CARTESIAN_POINT('Ctrl Pts',(14.9810583047522,69.9533094149169,13.2568033423269));
#56515=CARTESIAN_POINT('Ctrl Pts',(14.9856476226114,69.9622020782475,13.1952731643083));
#56516=CARTESIAN_POINT('Ctrl Pts',(14.9902369404706,69.9744283455657,13.1343982037041));
#56517=CARTESIAN_POINT('Ctrl Pts',(14.9948252174018,69.9866518397781,13.0735370504784));
#56518=CARTESIAN_POINT('Ctrl Pts',(14.999413494333,70.0022073366833,13.0133313165563));
#56519=CARTESIAN_POINT('Ctrl Pts',(15.0040017712643,70.0209955822639,12.9541656048311));
#56520=CARTESIAN_POINT('Ctrl Pts',(15.008630699923,70.0399502900372,12.8944756901369));
#56521=CARTESIAN_POINT('Ctrl Pts',(15.0132596285817,70.0621951881863,12.8358448276789));
#56522=CARTESIAN_POINT('Ctrl Pts',(15.0178885572404,70.0875774671697,12.7786507454216));
#56523=CARTESIAN_POINT('Ctrl Pts',(15.0224825436428,70.112768143697,12.7218884024357));
#56524=CARTESIAN_POINT('Ctrl Pts',(15.0270765300451,70.1410487119256,12.666541653862));
#56525=CARTESIAN_POINT('Ctrl Pts',(15.0316705164474,70.172223086198,12.6129558843088));
#56526=CARTESIAN_POINT('Ctrl Pts',(15.0363169162344,70.2037531329355,12.5587587477854));
#56527=CARTESIAN_POINT('Ctrl Pts',(15.0409633160213,70.2382431576301,12.5063634811408));
#56528=CARTESIAN_POINT('Ctrl Pts',(15.0456097158082,70.2754461663039,12.4560959960917));
#56529=CARTESIAN_POINT('Ctrl Pts',(15.0502561155951,70.3126491749777,12.4058285110425));
#56530=CARTESIAN_POINT('Ctrl Pts',(15.054902515382,70.3525647813502,12.357689175729));
#56531=CARTESIAN_POINT('Ctrl Pts',(15.0595489151689,70.3949069468999,12.3119663391126));
#56532=CARTESIAN_POINT('Ctrl Pts',(15.0641531360115,70.4368647400483,12.2666585638487));
#56533=CARTESIAN_POINT('Ctrl Pts',(15.0687573568541,70.481370989419,12.2235445099839));
#56534=CARTESIAN_POINT('Ctrl Pts',(15.0733615776967,70.5281674762515,12.1829233420349));
#56535=CARTESIAN_POINT('Ctrl Pts',(15.0779737765505,70.5750450501797,12.1422317873378));
#56536=CARTESIAN_POINT('Ctrl Pts',(15.0825859754043,70.6242204927978,12.1040421730639));
#56537=CARTESIAN_POINT('Ctrl Pts',(15.0871981742581,70.6753949616811,12.0686203008335));
#56538=CARTESIAN_POINT('Ctrl Pts',(15.0917901472714,70.7263450155555,12.0333537638698));
#56539=CARTESIAN_POINT('Ctrl Pts',(15.0963821202846,70.7792761970361,12.0008310574532));
#56540=CARTESIAN_POINT('Ctrl Pts',(15.1009740932979,70.8338601108457,11.9712745935591));
#56541=CARTESIAN_POINT('Ctrl Pts',(15.1055633545697,70.888411790698,11.9417355839245));
#56542=CARTESIAN_POINT('Ctrl Pts',(15.1101526158415,70.944613822131,11.915159583856));
#56543=CARTESIAN_POINT('Ctrl Pts',(15.1147418771134,71.002111107896,11.8917242836261));
#56544=CARTESIAN_POINT('Ctrl Pts',(15.1193300984737,71.0595953649657,11.8682942937579));
#56545=CARTESIAN_POINT('Ctrl Pts',(15.1239183198341,71.1183738240929,11.8480037818434));
#56546=CARTESIAN_POINT('Ctrl Pts',(15.1285065411944,71.1780710663744,11.8309824578741));
#56547=CARTESIAN_POINT('Ctrl Pts',(15.1331355252772,71.238298671497,11.813809912887));
#56548=CARTESIAN_POINT('Ctrl Pts',(15.13776450936,71.2994609717384,11.799965109451));
#56549=CARTESIAN_POINT('Ctrl Pts',(15.1423934934427,71.361158667484,11.7895293217406));
#56550=CARTESIAN_POINT('Ctrl Pts',(15.1469874274447,71.4223891960973,11.7791725524921));
#56551=CARTESIAN_POINT('Ctrl Pts',(15.1515813614467,71.4841465228903,11.7721733515128));
#56552=CARTESIAN_POINT('Ctrl Pts',(15.1561752954487,71.5460344327724,11.7685590460878));
#56553=CARTESIAN_POINT('Ctrl Pts',(15.1608218045719,71.6086306167306,11.7649033768676));
#56554=CARTESIAN_POINT('Ctrl Pts',(15.1654683136951,71.6713598596993,11.7647105911223));
#56555=CARTESIAN_POINT('Ctrl Pts',(15.1701148228182,71.7338140167254,11.7679548192699));
#56556=CARTESIAN_POINT('Ctrl Pts',(15.1747613319414,71.7962681737516,11.7711990474176));
#56557=CARTESIAN_POINT('Ctrl Pts',(15.1794078410646,71.8584467244815,11.7778801707693));
#56558=CARTESIAN_POINT('Ctrl Pts',(15.1840543501877,71.9199512711816,11.787919016488));
#56559=CARTESIAN_POINT('Ctrl Pts',(15.1886584522427,71.9808944873354,11.7978662411633));
#56560=CARTESIAN_POINT('Ctrl Pts',(15.1932625542977,72.0414169105433,11.8111494280926));
#56561=CARTESIAN_POINT('Ctrl Pts',(15.1978666563527,72.1011265402971,11.8277186123965));
#56562=CARTESIAN_POINT('Ctrl Pts',(15.202478870055,72.1609413682952,11.844316988794));
#56563=CARTESIAN_POINT('Ctrl Pts',(15.2070910837572,72.2199400235554,11.8642129166003));
#56564=CARTESIAN_POINT('Ctrl Pts',(15.2117032974595,72.2777358385527,11.887304128115));
#56565=CARTESIAN_POINT('Ctrl Pts',(15.2162951457023,72.335276453249,11.9102933792346));
#56566=CARTESIAN_POINT('Ctrl Pts',(15.2208869939451,72.3916243448091,11.9364495923407));
#56567=CARTESIAN_POINT('Ctrl Pts',(15.2254788421879,72.4464127216951,11.9656219041469));
#56568=CARTESIAN_POINT('Ctrl Pts',(15.2300679768008,72.5011687204691,11.9947769760853));
#56569=CARTESIAN_POINT('Ctrl Pts',(15.2346571114137,72.5543665855262,12.0269443738947));
#56570=CARTESIAN_POINT('Ctrl Pts',(15.2392462460267,72.6056620523399,12.0619262709517));
#56571=CARTESIAN_POINT('Ctrl Pts',(15.2438343390567,72.656945876767,12.0969002282668));
#56572=CARTESIAN_POINT('Ctrl Pts',(15.2484224320868,72.7063277415258,12.1346871306779));
#56573=CARTESIAN_POINT('Ctrl Pts',(15.2530105251169,72.7534921503756,12.175045706646));
#56574=CARTESIAN_POINT('Ctrl Pts',(15.2576396301243,72.8010781517384,12.2157650392499));
#56575=CARTESIAN_POINT('Ctrl Pts',(15.2622687351318,72.8464064356783,12.25910193594));
#56576=CARTESIAN_POINT('Ctrl Pts',(15.2668978401393,72.8891886426184,12.3047684143942));
#56577=CARTESIAN_POINT('Ctrl Pts',(15.2714916431915,72.9316445887475,12.3500866363334));
#56578=CARTESIAN_POINT('Ctrl Pts',(15.2760854462438,72.9715928707069,12.3976986006646));
#56579=CARTESIAN_POINT('Ctrl Pts',(15.280679249296,73.0087918493918,12.4472891412467));
#56580=CARTESIAN_POINT('Ctrl Pts',(15.2853260052811,73.0464196220407,12.497451313772));
#56581=CARTESIAN_POINT('Ctrl Pts',(15.2899727612662,73.0812339932799,12.549637535583));
#56582=CARTESIAN_POINT('Ctrl Pts',(15.2946195172513,73.113031030015,12.6034932225671));
#56583=CARTESIAN_POINT('Ctrl Pts',(15.2992662732363,73.1448280667501,12.6573489095512));
#56584=CARTESIAN_POINT('Ctrl Pts',(15.3039130292214,73.1736075803916,12.7128735621519));
#56585=CARTESIAN_POINT('Ctrl Pts',(15.3085597852065,73.1992154713234,12.7696912704556));
#56586=CARTESIAN_POINT('Ctrl Pts',(15.3131639657683,73.2245887325911,12.8259883923568));
#56587=CARTESIAN_POINT('Ctrl Pts',(15.3177681463301,73.246948614108,12.8837775277029));
#56588=CARTESIAN_POINT('Ctrl Pts',(15.3223723268919,73.2661202331561,12.942704294121));
#56589=CARTESIAN_POINT('Ctrl Pts',(15.3269845307808,73.2853252610092,13.0017337473723));
#56590=CARTESIAN_POINT('Ctrl Pts',(15.3315967346697,73.3013306509221,13.0619043533235));
#56591=CARTESIAN_POINT('Ctrl Pts',(15.3362089385586,73.3140080727277,13.1228373072639));
#56592=CARTESIAN_POINT('Ctrl Pts',(15.3408008680718,73.3266297669858,13.1835024114678));
#56593=CARTESIAN_POINT('Ctrl Pts',(15.3453927975851,73.3359525592773,13.2449226827745));
#56594=CARTESIAN_POINT('Ctrl Pts',(15.3499847270984,73.3418995996425,13.3067090204182));
#56595=CARTESIAN_POINT('Ctrl Pts',(15.354573943784,73.3478431266055,13.3684588558289));
#56596=CARTESIAN_POINT('Ctrl Pts',(15.3591631604697,73.3504148083483,13.430573824812));
#56597=CARTESIAN_POINT('Ctrl Pts',(15.3637523771554,73.349589386739,13.4926576637407));
#56598=CARTESIAN_POINT('Ctrl Pts',(15.3683405529185,73.3487641523512,13.5547274208618));
#56599=CARTESIAN_POINT('Ctrl Pts',(15.3729287286817,73.34454335145,13.6167655550409));
#56600=CARTESIAN_POINT('Ctrl Pts',(15.3775169044448,73.3369538322894,13.6783757857026));
#56601=CARTESIAN_POINT('Ctrl Pts',(15.3821459307598,73.3292967402932,13.7405345594138));
#56602=CARTESIAN_POINT('Ctrl Pts',(15.3867749570749,73.3182106749259,13.8022572477504));
#56603=CARTESIAN_POINT('Ctrl Pts',(15.3914039833899,73.3037764025269,13.8631444303841));
#56604=CARTESIAN_POINT('Ctrl Pts',(15.3959978698321,73.2894517036023,13.9235694061282));
#56605=CARTESIAN_POINT('Ctrl Pts',(15.4005917562743,73.2718296576399,13.9831710408981));
#56606=CARTESIAN_POINT('Ctrl Pts',(15.4051856427165,73.2510395064569,14.0415738018005));
#56607=CARTESIAN_POINT('Ctrl Pts',(15.409832238968,73.2300108110877,14.1006466703395));
#56608=CARTESIAN_POINT('Ctrl Pts',(15.4144788352194,73.205741036146,14.1584924808248));
#56609=CARTESIAN_POINT('Ctrl Pts',(15.4191254314709,73.178413080281,14.2147454137404));
#56610=CARTESIAN_POINT('Ctrl Pts',(15.4237720277223,73.151085124416,14.270998346656));
#56611=CARTESIAN_POINT('Ctrl Pts',(15.4284186239738,73.1206992997734,14.3256579689713));
#56612=CARTESIAN_POINT('Ctrl Pts',(15.4330652202252,73.0874838004644,14.3783882143875));
#56613=CARTESIAN_POINT('Ctrl Pts',(15.4376693867961,73.0545716033901,14.4306369616596));
#56614=CARTESIAN_POINT('Ctrl Pts',(15.4422735533669,73.0187511318237,14.481198000377));
#56615=CARTESIAN_POINT('Ctrl Pts',(15.4468777199378,72.9802211865124,14.5297297936916));
#56616=CARTESIAN_POINT('Ctrl Pts',(15.4514899255755,72.9416239663092,14.5783463255419));
#56617=CARTESIAN_POINT('Ctrl Pts',(15.4561021312133,72.9003080344869,14.6249260610246));
#56618=CARTESIAN_POINT('Ctrl Pts',(15.460714336851,72.8565182678733,14.6691527745969));
#56619=CARTESIAN_POINT('Ctrl Pts',(15.4653062523124,72.8129211427332,14.7131849244635));
#56620=CARTESIAN_POINT('Ctrl Pts',(15.4698981677737,72.7668722415645,14.7548843308449));
#56621=CARTESIAN_POINT('Ctrl Pts',(15.4744900832351,72.7186534588276,14.7939719969526));
#56622=CARTESIAN_POINT('Ctrl Pts',(15.4790792858875,72.6704631627531,14.8330365708733));
#56623=CARTESIAN_POINT('Ctrl Pts',(15.4836684885399,72.6201059206686,14.8694921457964));
#56624=CARTESIAN_POINT('Ctrl Pts',(15.4882576911923,72.5678980969526,14.9030987742367));
#56625=CARTESIAN_POINT('Ctrl Pts',(15.4928458529655,72.5157021145166,14.9366977803425));
#56626=CARTESIAN_POINT('Ctrl Pts',(15.4974340147388,72.4616568102192,14.9674488487201));
#56627=CARTESIAN_POINT('Ctrl Pts',(15.5020221765121,72.4061073458497,14.9951554575093));
#56628=CARTESIAN_POINT('Ctrl Pts',(15.5066512164064,72.3500629648139,15.0231089176878));
#56629=CARTESIAN_POINT('Ctrl Pts',(15.5112802563007,72.2924879411894,15.0479631342202));
#56630=CARTESIAN_POINT('Ctrl Pts',(15.5159092961951,72.2337598447896,15.0695647935108));
#56631=CARTESIAN_POINT('Ctrl Pts',(15.52050316892,72.1754779102213,15.0910023433467));
#56632=CARTESIAN_POINT('Ctrl Pts',(15.5250970416448,72.1160608708911,15.1092364899732));
#56633=CARTESIAN_POINT('Ctrl Pts',(15.5296909143697,72.0558931552801,15.1241675263008));
#56634=CARTESIAN_POINT('Ctrl Pts',(15.5343375378488,71.9950345427799,15.1392700134879));
#56635=CARTESIAN_POINT('Ctrl Pts',(15.5389841613278,71.9334084238037,15.1509929319953));
#56636=CARTESIAN_POINT('Ctrl Pts',(15.5436307848069,71.8714207801692,15.1592866667714));
#56637=CARTESIAN_POINT('Ctrl Pts',(15.5482774082859,71.8094331365347,15.1675804015476));
#56638=CARTESIAN_POINT('Ctrl Pts',(15.552924031765,71.7470845016633,15.1724449735931));
#56639=CARTESIAN_POINT('Ctrl Pts',(15.557570655244,71.684781076219,15.1738849627941));
#56640=CARTESIAN_POINT('Ctrl Pts',(15.5585437419726,71.6717336156878,15.1741865224938));
#56641=CARTESIAN_POINT('Ctrl Pts',(15.5595168287012,71.6586826780926,15.1743382187369));
#56642=CARTESIAN_POINT('Ctrl Pts',(15.5604899154299,71.6456305601979,15.1743399844051));
#56643=CARTESIAN_POINT('',(16.3542399153822,71.6462368438886,15.1743397945516));
#56644=CARTESIAN_POINT('Ctrl Pts',(15.5604899154688,71.6456305596758,15.1743399844052));
#56645=CARTESIAN_POINT('Ctrl Pts',(15.5650762026696,71.5841141917248,15.1743483062154));
#56646=CARTESIAN_POINT('Ctrl Pts',(15.5696624898704,71.5224716406624,15.171021778295));
#56647=CARTESIAN_POINT('Ctrl Pts',(15.5742487770713,71.4610952352599,15.1643454751892));
#56648=CARTESIAN_POINT('Ctrl Pts',(15.5788273156343,71.399822526707,15.1576804518512));
#56649=CARTESIAN_POINT('Ctrl Pts',(15.5834058541973,71.3388155757472,15.1476769437711));
#56650=CARTESIAN_POINT('Ctrl Pts',(15.5879843927603,71.2784659257297,15.1343720199341));
#56651=CARTESIAN_POINT('Ctrl Pts',(15.5925586200818,71.2181731021245,15.1210796242739));
#56652=CARTESIAN_POINT('Ctrl Pts',(15.5971328474032,71.1585368501406,15.104492083317));
#56653=CARTESIAN_POINT('Ctrl Pts',(15.6017070747247,71.0999411665725,15.0846979583303));
#56654=CARTESIAN_POINT('Ctrl Pts',(15.6062786955914,71.0413788715929,15.0649151122954));
#56655=CARTESIAN_POINT('Ctrl Pts',(15.6108503164582,70.98385645321,15.0419294686012));
#56656=CARTESIAN_POINT('Ctrl Pts',(15.6154219373249,70.9277432952677,15.0158795844932));
#56657=CARTESIAN_POINT('Ctrl Pts',(15.6199926529081,70.8716412489911,14.9898348588473));
#56658=CARTESIAN_POINT('Ctrl Pts',(15.6245633684912,70.8169483728025,14.9607273133252));
#56659=CARTESIAN_POINT('Ctrl Pts',(15.6291340840744,70.7640126540446,14.9287430143756));
#56660=CARTESIAN_POINT('Ctrl Pts',(15.6337088025551,70.7110305757495,14.8967307045229));
#56661=CARTESIAN_POINT('Ctrl Pts',(15.6382835210358,70.6598091689236,14.8618368720041));
#56662=CARTESIAN_POINT('Ctrl Pts',(15.6428582395164,70.6106693274308,14.8242921659836));
#56663=CARTESIAN_POINT('Ctrl Pts',(15.6474348741354,70.561508903528,14.7867317342198));
#56664=CARTESIAN_POINT('Ctrl Pts',(15.6520115087544,70.5144321728164,14.7465185484755));
#56665=CARTESIAN_POINT('Ctrl Pts',(15.6565881433734,70.4697262601586,14.703923049889));
#56666=CARTESIAN_POINT('Ctrl Pts',(15.6611731743483,70.4249383294268,14.6612494050227));
#56667=CARTESIAN_POINT('Ctrl Pts',(15.6657582053233,70.3825302586924,14.6161850885475));
#56668=CARTESIAN_POINT('Ctrl Pts',(15.6703432362982,70.3427510441729,14.5690361838823));
#56669=CARTESIAN_POINT('Ctrl Pts',(15.6742541876198,70.3088200691273,14.5288189918904));
#56670=CARTESIAN_POINT('Ctrl Pts',(15.6781651389413,70.2768012186877,14.4870858181692));
#56671=CARTESIAN_POINT('Ctrl Pts',(15.6820760902628,70.2468237658147,14.4440427879575));
#56672=CARTESIAN_POINT('Ctrl Pts',(15.6866802550219,70.2115328299943,14.3933704101823));
#56673=CARTESIAN_POINT('Ctrl Pts',(15.691284419781,70.1789295745051,14.3406774457886));
#56674=CARTESIAN_POINT('Ctrl Pts',(15.6958885845401,70.1492510550151,14.2862800806223));
#56675=CARTESIAN_POINT('Ctrl Pts',(15.7005007904043,70.1195207024331,14.2317877112683));
#56676=CARTESIAN_POINT('Ctrl Pts',(15.7051129962685,70.092725642573,14.1755853749444));
#56677=CARTESIAN_POINT('Ctrl Pts',(15.7097252021328,70.0690616645609,14.118021826658));
#56678=CARTESIAN_POINT('Ctrl Pts',(15.7143171155079,70.0455018018095,14.0607115427987));
#56679=CARTESIAN_POINT('Ctrl Pts',(15.718909028883,70.0250457459363,14.0020524600338));
#56680=CARTESIAN_POINT('Ctrl Pts',(15.7235009422582,70.0078405740573,13.9424129148386));
#56681=CARTESIAN_POINT('Ctrl Pts',(15.728090142727,69.9906455670086,13.8828086047376));
#56682=CARTESIAN_POINT('Ctrl Pts',(15.7326793431958,69.9766977752377,13.8222254673645));
#56683=CARTESIAN_POINT('Ctrl Pts',(15.7372685436646,69.9660948804296,13.7610483653701));
#56684=CARTESIAN_POINT('Ctrl Pts',(15.7418567031604,69.9554943906868,13.6998851402398));
#56685=CARTESIAN_POINT('Ctrl Pts',(15.7464448626562,69.9482373778168,13.6381287175427));
#56686=CARTESIAN_POINT('Ctrl Pts',(15.751033022152,69.9443703084637,13.5761735565569));
#56687=CARTESIAN_POINT('Ctrl Pts',(15.7556620640795,69.9404687818955,13.5136663490179));
#56688=CARTESIAN_POINT('Ctrl Pts',(15.7602911060069,69.9400179785039,13.4509573647327));
#56689=CARTESIAN_POINT('Ctrl Pts',(15.7649201479344,69.9430119428877,13.3884540706023));
#56690=CARTESIAN_POINT('Ctrl Pts',(15.7695140181765,69.9459831589846,13.3264256795361));
#56691=CARTESIAN_POINT('Ctrl Pts',(15.7741078884186,69.952346866061,13.2646003691596));
#56692=CARTESIAN_POINT('Ctrl Pts',(15.7787017586607,69.9620450677426,13.2033710299972));
#56693=CARTESIAN_POINT('Ctrl Pts',(15.7833483864309,69.9718546467859,13.1414385128155));
#56694=CARTESIAN_POINT('Ctrl Pts',(15.787995014201,69.9850757024932,13.0801162666477));
#56695=CARTESIAN_POINT('Ctrl Pts',(15.7926416419712,70.0015957067538,13.0197975109959));
#56696=CARTESIAN_POINT('Ctrl Pts',(15.7972882697413,70.0181157110145,12.9594787553441));
#56697=CARTESIAN_POINT('Ctrl Pts',(15.8019348975115,70.0379344366011,12.9001639732733));
#56698=CARTESIAN_POINT('Ctrl Pts',(15.8065815252816,70.0608893599134,12.8422254647946));
#56699=CARTESIAN_POINT('Ctrl Pts',(15.8111856876317,70.0836344987306,12.7848164549592));
#56700=CARTESIAN_POINT('Ctrl Pts',(15.8157898499818,70.10954861961,12.7285316886502));
#56701=CARTESIAN_POINT('Ctrl Pts',(15.8203940123319,70.1384991038188,12.6737434303641));
#56702=CARTESIAN_POINT('Ctrl Pts',(15.8250062184972,70.1675001666843,12.6188594529017));
#56703=CARTESIAN_POINT('Ctrl Pts',(15.8296184246626,70.1995480678181,12.5654777103989));
#56704=CARTESIAN_POINT('Ctrl Pts',(15.8342306308279,70.2344602436447,12.5139540599238));
#56705=CARTESIAN_POINT('Ctrl Pts',(15.8388225417529,70.2692187942917,12.462657130639));
#56706=CARTESIAN_POINT('Ctrl Pts',(15.8434144526779,70.3068162023768,12.413202412115));
#56707=CARTESIAN_POINT('Ctrl Pts',(15.8480063636028,70.3470266736192,12.3659159719736));
#56708=CARTESIAN_POINT('Ctrl Pts',(15.8525955616132,70.3872133883956,12.3186574688018));
#56709=CARTESIAN_POINT('Ctrl Pts',(15.8571847596235,70.4300097767036,12.2735650890779));
#56710=CARTESIAN_POINT('Ctrl Pts',(15.8617739576338,70.475148982573,12.2309328541959));
#56711=CARTESIAN_POINT('Ctrl Pts',(15.8663621146672,70.5202779494261,12.188310289669));
#56712=CARTESIAN_POINT('Ctrl Pts',(15.8709502717005,70.5677483099836,12.1481471099338));
#56713=CARTESIAN_POINT('Ctrl Pts',(15.8755384287339,70.6172569178041,12.1106999455114));
#56714=CARTESIAN_POINT('Ctrl Pts',(15.8801674730311,70.6672067205304,12.0729190714796));
#56715=CARTESIAN_POINT('Ctrl Pts',(15.8847965173283,70.7192308819633,12.0379032049952));
#56716=CARTESIAN_POINT('Ctrl Pts',(15.8894255616255,70.7729864540195,12.0058724644384));
#56717=CARTESIAN_POINT('Ctrl Pts',(15.8940194294244,70.8263335329464,11.9740851281825));
#56718=CARTESIAN_POINT('Ctrl Pts',(15.8986132972232,70.8813853167274,11.9452378931465));
#56719=CARTESIAN_POINT('Ctrl Pts',(15.9032071650221,70.9377822618517,11.9194994446122));
#56720=CARTESIAN_POINT('Ctrl Pts',(15.9078537975685,70.9948269771555,11.8934653666002));
#56721=CARTESIAN_POINT('Ctrl Pts',(15.9125004301148,71.0532474624081,11.8706121550289));
#56722=CARTESIAN_POINT('Ctrl Pts',(15.9171470626612,71.1126537750681,11.8510632206844));
#56723=CARTESIAN_POINT('Ctrl Pts',(15.9217936952076,71.1720600877282,11.8315142863399));
#56724=CARTESIAN_POINT('Ctrl Pts',(15.9264403277539,71.2324516995971,11.8152697066516));
#56725=CARTESIAN_POINT('Ctrl Pts',(15.9310869603003,71.2934284890502,11.802399660866));
#56726=CARTESIAN_POINT('Ctrl Pts',(15.9356911216906,71.3538479383828,11.7896472498876));
#56727=CARTESIAN_POINT('Ctrl Pts',(15.9402952830808,71.4150807634737,11.7801574727491));
#56728=CARTESIAN_POINT('Ctrl Pts',(15.9448994444711,71.4767433933052,11.774025417461));
#56729=CARTESIAN_POINT('Ctrl Pts',(15.9495116507564,71.5385137668374,11.7678826475744));
#56730=CARTESIAN_POINT('Ctrl Pts',(15.9541238570418,71.6007149577268,11.7651094963736));
#56731=CARTESIAN_POINT('Ctrl Pts',(15.9587360633271,71.6629494823739,11.7657503553562));
#56732=CARTESIAN_POINT('Ctrl Pts',(15.9633279732294,71.7249101390122,11.7663883941876));
#56733=CARTESIAN_POINT('Ctrl Pts',(15.9679198831317,71.7869033274104,11.7704104814037));
#56734=CARTESIAN_POINT('Ctrl Pts',(15.9725117930339,71.8485325158393,11.7778085165653));
#56735=CARTESIAN_POINT('Ctrl Pts',(15.9771009900009,71.9101252932745,11.7852021809115));
#56736=CARTESIAN_POINT('Ctrl Pts',(15.9816901869678,71.971353994652,11.7959677772661));
#56737=CARTESIAN_POINT('Ctrl Pts',(15.9862793839347,72.0318261191956,11.8100452747128));
#56738=CARTESIAN_POINT('Ctrl Pts',(15.9908675399058,72.0922845264737,11.8241195788738));
#56739=CARTESIAN_POINT('Ctrl Pts',(15.9954556958768,72.1519862039588,11.8415041773498));
#56740=CARTESIAN_POINT('Ctrl Pts',(16.0000438518479,72.2105497726291,11.8620881336039));
#56741=CARTESIAN_POINT('Ctrl Pts',(16.0046728971372,72.2696352556394,11.8828555326056));
#56742=CARTESIAN_POINT('Ctrl Pts',(16.0093019424264,72.3275617374471,11.906879457176));
#56743=CARTESIAN_POINT('Ctrl Pts',(16.0139309877157,72.3839562882486,11.9339956234801));
#56744=CARTESIAN_POINT('Ctrl Pts',(16.018524854418,72.4399222667451,11.9609057195569));
#56745=CARTESIAN_POINT('Ctrl Pts',(16.0231187211203,72.4943790953525,11.9908609217262));
#56746=CARTESIAN_POINT('Ctrl Pts',(16.0277125878226,72.5469875513231,12.0236547013596));
#56747=CARTESIAN_POINT('Ctrl Pts',(16.0323592224054,72.6002002992542,12.0568251698165));
#56748=CARTESIAN_POINT('Ctrl Pts',(16.0370058569881,72.6515214953787,12.0928995509853));
#56749=CARTESIAN_POINT('Ctrl Pts',(16.0416524915709,72.7006328641361,12.1316209662255));
#56750=CARTESIAN_POINT('Ctrl Pts',(16.0462991261536,72.7497442328934,12.1703423814656));
#56751=CARTESIAN_POINT('Ctrl Pts',(16.0509457607364,72.7966454179646,12.2117104332495));
#56752=CARTESIAN_POINT('Ctrl Pts',(16.0555923953191,72.8410568939521,12.255430352946));
#56753=CARTESIAN_POINT('Ctrl Pts',(16.060196557806,72.885062431312,12.2987506551157));
#56754=CARTESIAN_POINT('Ctrl Pts',(16.064800720293,72.9267975936672,12.344551233288));
#56755=CARTESIAN_POINT('Ctrl Pts',(16.0694048827799,72.9659712349874,12.3925648748423));
#56756=CARTESIAN_POINT('Ctrl Pts',(16.0740170889281,73.0052133142713,12.4406623982043));
#56757=CARTESIAN_POINT('Ctrl Pts',(16.0786292950764,73.041884516254,12.4909803995974));
#56758=CARTESIAN_POINT('Ctrl Pts',(16.0832415012246,73.0757282696727,12.5432120649388));
#56759=CARTESIAN_POINT('Ctrl Pts',(16.0878334122674,73.109423100315,12.5952138951162));
#56760=CARTESIAN_POINT('Ctrl Pts',(16.0924253233102,73.1403150134699,12.6491121710601));
#56761=CARTESIAN_POINT('Ctrl Pts',(16.097017234353,73.1681917198803,12.7045718757035));
#56762=CARTESIAN_POINT('Ctrl Pts',(16.1016064324736,73.1960519566043,12.7599988144984));
#56763=CARTESIAN_POINT('Ctrl Pts',(16.1061956305943,73.2209002921553,12.8169849001973));
#56764=CARTESIAN_POINT('Ctrl Pts',(16.1107848287149,73.2425699523366,12.8751697898112));
#56765=CARTESIAN_POINT('Ctrl Pts',(16.1153729858509,73.264234697109,12.9333414811325));
#56766=CARTESIAN_POINT('Ctrl Pts',(16.1199611429868,73.282722021386,12.9927109612972));
#56767=CARTESIAN_POINT('Ctrl Pts',(16.1245493001227,73.2979137286391,13.05289903829));
#56768=CARTESIAN_POINT('Ctrl Pts',(16.1291783443073,73.3132408157528,13.1136234772163));
#56769=CARTESIAN_POINT('Ctrl Pts',(16.1338073884919,73.325213094183,13.1751806757362));
#56770=CARTESIAN_POINT('Ctrl Pts',(16.1384364326765,73.3337615042061,13.2371690168494));
#56771=CARTESIAN_POINT('Ctrl Pts',(16.1430303005577,73.3422449544982,13.2986863059242));
#56772=CARTESIAN_POINT('Ctrl Pts',(16.1476241684388,73.3473564086421,13.3606276905436));
#56773=CARTESIAN_POINT('Ctrl Pts',(16.1522180363199,73.3490806409208,13.4225963149988));
#56774=CARTESIAN_POINT('Ctrl Pts',(16.1568646686562,73.3508246774645,13.4852767014799));
#56775=CARTESIAN_POINT('Ctrl Pts',(16.1615113009926,73.3491031829668,13.5479844251041));
#56776=CARTESIAN_POINT('Ctrl Pts',(16.1661579333289,73.343954473631,13.6103122792496));
#56777=CARTESIAN_POINT('Ctrl Pts',(16.1708045656652,73.3388057642951,13.6726401333951));
#56778=CARTESIAN_POINT('Ctrl Pts',(16.1754511980016,73.3302299746642,13.7345876014508));
#56779=CARTESIAN_POINT('Ctrl Pts',(16.1800978303379,73.3183184105988,13.7957588480447));
#56780=CARTESIAN_POINT('Ctrl Pts',(16.1847019924617,73.3065157182112,13.8563709895367));
#56781=CARTESIAN_POINT('Ctrl Pts',(16.1893061545855,73.2913913686667,13.9164606737471));
#56782=CARTESIAN_POINT('Ctrl Pts',(16.1939103167092,73.2730072786163,13.9756375996653));
#56783=CARTESIAN_POINT('Ctrl Pts',(16.1985225229029,73.2545910691702,14.0349179153672));
#56784=CARTESIAN_POINT('Ctrl Pts',(16.2031347290965,73.2329037695676,14.0932817691944));
#56785=CARTESIAN_POINT('Ctrl Pts',(16.2077469352901,73.2080594064967,14.1503458053722));
#56786=CARTESIAN_POINT('Ctrl Pts',(16.2123388459611,73.1833243684022,14.2071587373299));
#56787=CARTESIAN_POINT('Ctrl Pts',(16.2169307566321,73.1554601710129,14.26268278935));
#56788=CARTESIAN_POINT('Ctrl Pts',(16.2215226673031,73.1246288116329,14.3165559393419));
#56789=CARTESIAN_POINT('Ctrl Pts',(16.2261118650498,73.0938156675777,14.3703972608012));
#56790=CARTESIAN_POINT('Ctrl Pts',(16.2307010627965,73.0600390895782,14.422589175253));
#56791=CARTESIAN_POINT('Ctrl Pts',(16.2352902605432,73.0235073284427,14.4727936113141));
#56792=CARTESIAN_POINT('Ctrl Pts',(16.2398784173036,72.9869838539538,14.5229866593007));
#56793=CARTESIAN_POINT('Ctrl Pts',(16.2444665740641,72.9477067356623,14.5711927142205));
#56794=CARTESIAN_POINT('Ctrl Pts',(16.2490547308245,72.9059267706146,14.6171037861344));
#56795=CARTESIAN_POINT('Ctrl Pts',(16.2536837753689,72.8637744795392,14.6634239988175));
#56796=CARTESIAN_POINT('Ctrl Pts',(16.2583128199132,72.8190748379485,14.7074077100018));
#56797=CARTESIAN_POINT('Ctrl Pts',(16.2629418644576,72.7721244789935,14.7487755018129));
#56798=CARTESIAN_POINT('Ctrl Pts',(16.2675357319639,72.725530905234,14.7898289314761));
#56799=CARTESIAN_POINT('Ctrl Pts',(16.2721295994702,72.6767211430397,14.8283057896959));
#56800=CARTESIAN_POINT('Ctrl Pts',(16.2767234669765,72.6260175940621,14.86397416397));
#56801=CARTESIAN_POINT('Ctrl Pts',(16.2813701000399,72.5747316597627,14.9000522282568));
#56802=CARTESIAN_POINT('Ctrl Pts',(16.2860167331032,72.5215085991454,14.9332565837703));
#56803=CARTESIAN_POINT('Ctrl Pts',(16.2906633661666,72.4667090186912,14.9633942317474));
#56804=CARTESIAN_POINT('Ctrl Pts',(16.2953099992299,72.411909438237,14.9935318797246));
#56805=CARTESIAN_POINT('Ctrl Pts',(16.2999566322933,72.3555338429059,15.0206026469455));
#56806=CARTESIAN_POINT('Ctrl Pts',(16.3046032653567,72.2979626314675,15.0444639873977));
#56807=CARTESIAN_POINT('Ctrl Pts',(16.3097079245347,72.2347165328731,15.0706773786592));
#56808=CARTESIAN_POINT('Ctrl Pts',(16.3148125837127,72.169816198335,15.0931062139384));
#56809=CARTESIAN_POINT('Ctrl Pts',(16.3199172428907,72.1037055186798,15.1115635495306));
#56810=CARTESIAN_POINT('Ctrl Pts',(16.3250050814713,72.037812683368,15.1299600655068));
#56811=CARTESIAN_POINT('Ctrl Pts',(16.3300929200518,71.9707177406488,15.1444110519676));
#56812=CARTESIAN_POINT('Ctrl Pts',(16.3351807586324,71.9028819957496,15.1547782813963));
#56813=CARTESIAN_POINT('Ctrl Pts',(16.3402418161921,71.8354033200608,15.1650909405033));
#56814=CARTESIAN_POINT('Ctrl Pts',(16.3453028737517,71.7671919133591,15.1713625929221));
#56815=CARTESIAN_POINT('Ctrl Pts',(16.3503639313113,71.6987191891739,15.1735057674296));
#56816=CARTESIAN_POINT('Ctrl Pts',(16.3516559260016,71.6812393650395,15.1740528803702));
#56817=CARTESIAN_POINT('Ctrl Pts',(16.3529479206919,71.663742587001,15.1743311990977));
#56818=CARTESIAN_POINT('Ctrl Pts',(16.3542399153822,71.6462368438885,15.1743397945516));
#56819=CARTESIAN_POINT('',(17.1479899153848,71.6439440199028,15.174339378094));
#56820=CARTESIAN_POINT('Ctrl Pts',(16.3542399154298,71.6462368432431,15.174339794552));
#56821=CARTESIAN_POINT('Ctrl Pts',(16.3588871624829,71.5832694690705,15.1743707119909));
#56822=CARTESIAN_POINT('Ctrl Pts',(16.363534409536,71.5203035798291,15.1709077637263));
#56823=CARTESIAN_POINT('Ctrl Pts',(16.3681816565891,71.4577458076997,15.163977786074));
#56824=CARTESIAN_POINT('Ctrl Pts',(16.3728305705312,71.3951655971534,15.1570453227556));
#56825=CARTESIAN_POINT('Ctrl Pts',(16.3774794844734,71.3329942797243,15.1466434159465));
#56826=CARTESIAN_POINT('Ctrl Pts',(16.3821283984155,71.2716314321484,15.1328505324551));
#56827=CARTESIAN_POINT('Ctrl Pts',(16.3867839971765,71.2101803490142,15.119037815745));
#56828=CARTESIAN_POINT('Ctrl Pts',(16.3914395959375,71.1495405328699,15.1018245005813));
#56829=CARTESIAN_POINT('Ctrl Pts',(16.3960951946984,71.0900985982484,15.0813395634728));
#56830=CARTESIAN_POINT('Ctrl Pts',(16.4007546246755,71.030607747277,15.0608377687644));
#56831=CARTESIAN_POINT('Ctrl Pts',(16.4054140546525,70.9723171923226,15.0370591771749));
#56832=CARTESIAN_POINT('Ctrl Pts',(16.4100734846296,70.9155929391788,15.0101806678359));
#56833=CARTESIAN_POINT('Ctrl Pts',(16.4147419584392,70.8587585857334,14.9832499880086));
#56834=CARTESIAN_POINT('Ctrl Pts',(16.4194104322488,70.803497031157,14.9532076138302));
#56835=CARTESIAN_POINT('Ctrl Pts',(16.4240789060584,70.7501483512317,14.9202756017315));
#56836=CARTESIAN_POINT('Ctrl Pts',(16.4257555041641,70.730989135747,14.9084486639885));
#56837=CARTESIAN_POINT('Ctrl Pts',(16.4274321022698,70.7120763427755,14.8962494254406));
#56838=CARTESIAN_POINT('Ctrl Pts',(16.4291087003754,70.69342469322,14.8836894464065));
#56839=CARTESIAN_POINT('Ctrl Pts',(16.4337128625557,70.642204774032,14.8491980675494));
#56840=CARTESIAN_POINT('Ctrl Pts',(16.4383170247359,70.5927605262358,14.8118512798714));
#56841=CARTESIAN_POINT('Ctrl Pts',(16.4429211869162,70.5454272604206,14.7718582133943));
#56842=CARTESIAN_POINT('Ctrl Pts',(16.4475333931028,70.49801129789,14.731795274383));
#56843=CARTESIAN_POINT('Ctrl Pts',(16.4521455992894,70.452714151242,14.6890770477523));
#56844=CARTESIAN_POINT('Ctrl Pts',(16.456757805476,70.4098444265217,14.6439579466262));
#56845=CARTESIAN_POINT('Ctrl Pts',(16.4613497162028,70.3671633448792,14.5990373866887));
#56846=CARTESIAN_POINT('Ctrl Pts',(16.4659416269297,70.3268887374615,14.5517373873812));
#56847=CARTESIAN_POINT('Ctrl Pts',(16.4705335376566,70.2892908682312,14.5023482253257));
#56848=CARTESIAN_POINT('Ctrl Pts',(16.4751227354588,70.2517152120173,14.4529882426438));
#56849=CARTESIAN_POINT('Ctrl Pts',(16.479711933261,70.2168134642751,14.4015419478507));
#56850=CARTESIAN_POINT('Ctrl Pts',(16.4843011310632,70.1848158059665,14.3483328798009));
#56851=CARTESIAN_POINT('Ctrl Pts',(16.4888892878786,70.152825405819,14.2951358813841));
#56852=CARTESIAN_POINT('Ctrl Pts',(16.4934774446941,70.1237380482417,14.2401773381916));
#56853=CARTESIAN_POINT('Ctrl Pts',(16.4980656015095,70.0977396300053,14.1838082478845));
#56854=CARTESIAN_POINT('Ctrl Pts',(16.5026946459999,70.0715095250773,14.1269368205534));
#56855=CARTESIAN_POINT('Ctrl Pts',(16.5073236904903,70.0484239391731,14.0686300418957));
#56856=CARTESIAN_POINT('Ctrl Pts',(16.5119527349807,70.0286245927657,14.0092699863355));
#56857=CARTESIAN_POINT('Ctrl Pts',(16.5165466025402,70.0089757051069,13.9503610183765));
#56858=CARTESIAN_POINT('Ctrl Pts',(16.5211404700996,69.9925633636205,13.8904152375184));
#56859=CARTESIAN_POINT('Ctrl Pts',(16.5257343376591,69.9794754969945,13.8298199353646));
#56860=CARTESIAN_POINT('Ctrl Pts',(16.530380970615,69.9662373024668,13.7685286324888));
#56861=CARTESIAN_POINT('Ctrl Pts',(16.5350276035708,69.9564005406046,13.7065733151398));
#56862=CARTESIAN_POINT('Ctrl Pts',(16.5396742365267,69.9500024138971,13.6443612934011));
#56863=CARTESIAN_POINT('Ctrl Pts',(16.5443208694825,69.9436042871896,13.5821492716623));
#56864=CARTESIAN_POINT('Ctrl Pts',(16.5489675024384,69.9406447583667,13.5196810780754));
#56865=CARTESIAN_POINT('Ctrl Pts',(16.5536141353942,69.9411068528548,13.457362587531));
#56866=CARTESIAN_POINT('Ctrl Pts',(16.5582182975238,69.9415647237395,13.3956136960519));
#56867=CARTESIAN_POINT('Ctrl Pts',(16.5628224596533,69.9453836854699,13.3337676644005));
#56868=CARTESIAN_POINT('Ctrl Pts',(16.5674266217829,69.9525746342542,13.2722195239975));
#56869=CARTESIAN_POINT('Ctrl Pts',(16.5720388279758,69.959778146551,13.2105638510776));
#56870=CARTESIAN_POINT('Ctrl Pts',(16.5766510341687,69.9703654829862,13.1492076232064));
#56871=CARTESIAN_POINT('Ctrl Pts',(16.5812632403617,69.9842950411052,13.0885486254645));
#56872=CARTESIAN_POINT('Ctrl Pts',(16.5858551510364,69.998163303699,13.0281565511301));
#56873=CARTESIAN_POINT('Ctrl Pts',(16.5904470617111,70.0153443485486,12.9684560858829));
#56874=CARTESIAN_POINT('Ctrl Pts',(16.5950389723858,70.0357454980589,12.9098328642444));
#56875=CARTESIAN_POINT('Ctrl Pts',(16.5996281701355,70.0561345944622,12.8512442775151));
#56876=CARTESIAN_POINT('Ctrl Pts',(16.6042173678851,70.0797398561651,12.7937321502646));
#56877=CARTESIAN_POINT('Ctrl Pts',(16.6088065656347,70.1064187371306,12.7376670783469));
#56878=CARTESIAN_POINT('Ctrl Pts',(16.6133947223973,70.1330915664134,12.6816147239051));
#56879=CARTESIAN_POINT('Ctrl Pts',(16.6179828791599,70.1628364126363,12.6270092307533));
#56880=CARTESIAN_POINT('Ctrl Pts',(16.6225710359226,70.195463378247,12.574199448259));
#56881=CARTESIAN_POINT('Ctrl Pts',(16.6272000804634,70.2283811020432,12.5209190465623));
#56882=CARTESIAN_POINT('Ctrl Pts',(16.6318291250043,70.2642323236069,12.4694669842057));
#56883=CARTESIAN_POINT('Ctrl Pts',(16.6364581695452,70.3027768375861,12.4201724525668));
#56884=CARTESIAN_POINT('Ctrl Pts',(16.6410520370517,70.3410284441021,12.371252519923));
#56885=CARTESIAN_POINT('Ctrl Pts',(16.6456459045582,70.3819321685111,12.3244577889898));
#56886=CARTESIAN_POINT('Ctrl Pts',(16.6502397720647,70.4252137422743,12.2800754931268));
#56887=CARTESIAN_POINT('Ctrl Pts',(16.6548864051227,70.4689924518623,12.2351834184518));
#56888=CARTESIAN_POINT('Ctrl Pts',(16.6595330381808,70.5152036032517,12.1927599238098));
#56889=CARTESIAN_POINT('Ctrl Pts',(16.6641796712388,70.5635282199637,12.1530610161586));
#56890=CARTESIAN_POINT('Ctrl Pts',(16.6688263042969,70.6118528366758,12.1133621085074));
#56891=CARTESIAN_POINT('Ctrl Pts',(16.673472937355,70.6622904542047,12.0763880509518));
#56892=CARTESIAN_POINT('Ctrl Pts',(16.678119570413,70.7144933653474,12.0423488965578));
#56893=CARTESIAN_POINT('Ctrl Pts',(16.6827237325413,70.7662191339778,12.008620865189));
#56894=CARTESIAN_POINT('Ctrl Pts',(16.6873278946696,70.8198825227819,11.9776409233246));
#56895=CARTESIAN_POINT('Ctrl Pts',(16.691932056798,70.8751602591703,11.9496363667706));
#56896=CARTESIAN_POINT('Ctrl Pts',(16.696544262991,70.9305345728899,11.9215828826463));
#56897=CARTESIAN_POINT('Ctrl Pts',(16.7011564691841,70.9875284777049,11.8965155093395));
#56898=CARTESIAN_POINT('Ctrl Pts',(16.7057686753772,71.0457874056845,11.8746193017533));
#56899=CARTESIAN_POINT('Ctrl Pts',(16.7103605860502,71.1037899714826,11.8528194460866));
#56900=CARTESIAN_POINT('Ctrl Pts',(16.7149524967232,71.1630459838935,11.8341631108941));
#56901=CARTESIAN_POINT('Ctrl Pts',(16.7195444073963,71.2231827898986,11.8187860638021));
#56902=CARTESIAN_POINT('Ctrl Pts',(16.724133605144,71.2832840667586,11.8034181015514));
#56903=CARTESIAN_POINT('Ctrl Pts',(16.7287228028918,71.3442646147717,11.7913257104668));
#56904=CARTESIAN_POINT('Ctrl Pts',(16.7333120006395,71.4057367698828,11.7825947814085));
#56905=CARTESIAN_POINT('Ctrl Pts',(16.7379001574001,71.4671949810043,11.7738658328238));
#56906=CARTESIAN_POINT('Ctrl Pts',(16.7424883141607,71.5291440758616,11.7684969034079));
#56907=CARTESIAN_POINT('Ctrl Pts',(16.7470764709212,71.5911883612235,11.766522399965));
#56908=CARTESIAN_POINT('Ctrl Pts',(16.7517055154638,71.6537855599544,11.7645303005526));
#56909=CARTESIAN_POINT('Ctrl Pts',(16.7563345600063,71.7164791315643,11.7659934791591));
#56910=CARTESIAN_POINT('Ctrl Pts',(16.7609636045489,71.7788619796757,11.7708935478961));
#56911=CARTESIAN_POINT('Ctrl Pts',(16.7655574720529,71.8407707680047,11.7757563800274));
#56912=CARTESIAN_POINT('Ctrl Pts',(16.770151339557,71.9023730372047,11.7840039215462));
#56913=CARTESIAN_POINT('Ctrl Pts',(16.774745207061,71.9632778501082,11.7955662127123));
#56914=CARTESIAN_POINT('Ctrl Pts',(16.7793918401228,72.0248822209372,11.8072613093504));
#56915=CARTESIAN_POINT('Ctrl Pts',(16.7840384731846,72.085772490495,11.8223476771256));
#56916=CARTESIAN_POINT('Ctrl Pts',(16.7886851062464,72.1455590550303,11.8407008392345));
#56917=CARTESIAN_POINT('Ctrl Pts',(16.7933317393082,72.2053456195656,11.8590540013434));
#56918=CARTESIAN_POINT('Ctrl Pts',(16.7979783723699,72.2640280031684,11.8806737159195));
#56919=CARTESIAN_POINT('Ctrl Pts',(16.8026250054317,72.3212390378092,11.9053861720626));
#56920=CARTESIAN_POINT('Ctrl Pts',(16.8072291675718,72.37792715503,11.9298727526575));
#56921=CARTESIAN_POINT('Ctrl Pts',(16.8118333297119,72.4333948401411,11.9574925286597));
#56922=CARTESIAN_POINT('Ctrl Pts',(16.816437491852,72.487274049383,11.9881015822347));
#56923=CARTESIAN_POINT('Ctrl Pts',(16.8210496980436,72.5412473923939,12.0187641136839));
#56924=CARTESIAN_POINT('Ctrl Pts',(16.8256619042352,72.5936262154243,12.0524262182956));
#56925=CARTESIAN_POINT('Ctrl Pts',(16.8302741104268,72.6440603986762,12.0888945573505));
#56926=CARTESIAN_POINT('Ctrl Pts',(16.8348660211122,72.6942726518502,12.1252024214895));
#56927=CARTESIAN_POINT('Ctrl Pts',(16.8394579317976,72.7425569150337,12.1642915990056));
#56928=CARTESIAN_POINT('Ctrl Pts',(16.844049842483,72.7885941633852,12.2059264497657));
#56929=CARTESIAN_POINT('Ctrl Pts',(16.8486390402434,72.8346042126872,12.247536702436));
#56930=CARTESIAN_POINT('Ctrl Pts',(16.8532282380037,72.8783695045443,12.2916893060575));
#56931=CARTESIAN_POINT('Ctrl Pts',(16.857817435764,72.91960429855,12.338108555931));
#56932=CARTESIAN_POINT('Ctrl Pts',(16.8624055925373,72.9608297390943,12.3845172763311));
#56933=CARTESIAN_POINT('Ctrl Pts',(16.8669937493107,72.999525484948,12.4331912429753));
#56934=CARTESIAN_POINT('Ctrl Pts',(16.871581906084,73.0354442766861,12.4838196187045));
#56935=CARTESIAN_POINT('Ctrl Pts',(16.8762109506146,73.0716831618535,12.5348991735971));
#56936=CARTESIAN_POINT('Ctrl Pts',(16.8808399951451,73.1050950208235,12.5879677374539));
#56937=CARTESIAN_POINT('Ctrl Pts',(16.8854690396756,73.1354703039202,12.6426758041884));
#56938=CARTESIAN_POINT('Ctrl Pts',(16.8900629071927,73.1656147593083,12.6969681336393));
#56939=CARTESIAN_POINT('Ctrl Pts',(16.8946567747098,73.1927684582529,12.7528746463588));
#56940=CARTESIAN_POINT('Ctrl Pts',(16.8992506422269,73.2167737667556,12.8100308183313));
#56941=CARTESIAN_POINT('Ctrl Pts',(16.9038972752642,73.2410548021018,12.8678434905477));
#56942=CARTESIAN_POINT('Ctrl Pts',(16.9085439083015,73.2621144654426,12.9269342170202));
#56943=CARTESIAN_POINT('Ctrl Pts',(16.9131905413387,73.2798413038651,12.9869094703685));
#56944=CARTESIAN_POINT('Ctrl Pts',(16.917837174376,73.2975681422877,13.0468847237168));
#56945=CARTESIAN_POINT('Ctrl Pts',(16.9224838074133,73.3119620945183,13.1077439736246));
#56946=CARTESIAN_POINT('Ctrl Pts',(16.9271304404505,73.3229652250746,13.169085142905));
#56947=CARTESIAN_POINT('Ctrl Pts',(16.9317346025836,73.3338677854115,13.2298656449451));
#56948=CARTESIAN_POINT('Ctrl Pts',(16.9363387647168,73.3414844073172,13.2913595729054));
#56949=CARTESIAN_POINT('Ctrl Pts',(16.9409429268499,73.3457317532,13.3531806323423));
#56950=CARTESIAN_POINT('Ctrl Pts',(16.9455551330423,73.3499865197386,13.4151097010669));
#56951=CARTESIAN_POINT('Ctrl Pts',(16.9501673392348,73.3508600892818,13.4773665502191));
#56952=CARTESIAN_POINT('Ctrl Pts',(16.9547795454273,73.3483202217464,13.5395525266776));
#56953=CARTESIAN_POINT('Ctrl Pts',(16.9593714561055,73.3457915306232,13.6014648604752));
#56954=CARTESIAN_POINT('Ctrl Pts',(16.9639633667837,73.3398793734571,13.6633064343219));
#56955=CARTESIAN_POINT('Ctrl Pts',(16.9685552774618,73.330603948578,13.7246811482951));
#56956=CARTESIAN_POINT('Ctrl Pts',(16.9731444752149,73.3213340036691,13.7860196017623));
#56957=CARTESIAN_POINT('Ctrl Pts',(16.9777336729679,73.3087048074216,13.8468912418622));
#56958=CARTESIAN_POINT('Ctrl Pts',(16.9823228707209,73.2927883414332,13.9069055826033));
#56959=CARTESIAN_POINT('Ctrl Pts',(16.9869110274869,73.2768754858439,13.9669063100386));
#56960=CARTESIAN_POINT('Ctrl Pts',(16.9914991842528,73.2576769711982,14.0260496342609));
#56961=CARTESIAN_POINT('Ctrl Pts',(16.9960873410188,73.2353153215806,14.0839577394278));
#56962=CARTESIAN_POINT('Ctrl Pts',(17.0007163855563,73.2127543941117,14.1423818978809));
#56963=CARTESIAN_POINT('Ctrl Pts',(17.0053454300939,73.1869738302626,14.1995482107794));
#56964=CARTESIAN_POINT('Ctrl Pts',(17.0099744746314,73.1581492185228,14.2550889360185));
#56965=CARTESIAN_POINT('Ctrl Pts',(17.0145683421411,73.1295436507266,14.3102075962668));
#56966=CARTESIAN_POINT('Ctrl Pts',(17.0191622096507,73.0979404514304,14.3637248767813));
#56967=CARTESIAN_POINT('Ctrl Pts',(17.0237560771604,73.0635564057154,14.4153080156903));
#56968=CARTESIAN_POINT('Ctrl Pts',(17.0284027102119,73.02877742201,14.4674836427953));
#56969=CARTESIAN_POINT('Ctrl Pts',(17.0330493432634,72.991153607696,14.517679977289));
#56970=CARTESIAN_POINT('Ctrl Pts',(17.0376959763149,72.9509514347238,14.5655867317975));
#56971=CARTESIAN_POINT('Ctrl Pts',(17.0423426093664,72.9107492617515,14.6134934863059));
#56972=CARTESIAN_POINT('Ctrl Pts',(17.0469892424178,72.8679691383366,14.6591103168089));
#56973=CARTESIAN_POINT('Ctrl Pts',(17.0516358754693,72.8229142261024,14.7021668243085));
#56974=CARTESIAN_POINT('Ctrl Pts',(17.0561790386785,72.7788625832488,14.7442645623095));
#56975=CARTESIAN_POINT('Ctrl Pts',(17.0607222018877,72.7324519488316,14.7840909041797));
#56976=CARTESIAN_POINT('Ctrl Pts',(17.0652653650969,72.6839488770977,14.8213663698195));
#56977=CARTESIAN_POINT('Ctrl Pts',(17.0698023105883,72.6355121860765,14.8585908207115));
#56978=CARTESIAN_POINT('Ctrl Pts',(17.0743392560797,72.5849891390917,14.8932709945406));
#56979=CARTESIAN_POINT('Ctrl Pts',(17.0788762015711,72.5326822271473,14.9251649683072));
#56980=CARTESIAN_POINT('Ctrl Pts',(17.0834086977726,72.4804266115247,14.9570276643041));
#56981=CARTESIAN_POINT('Ctrl Pts',(17.087941193974,72.4263910408378,14.9861093042422));
#56982=CARTESIAN_POINT('Ctrl Pts',(17.0924736901755,72.3709083198828,15.0122102688612));
#56983=CARTESIAN_POINT('Ctrl Pts',(17.0971000422763,72.3142766998578,15.0388517147951));
#56984=CARTESIAN_POINT('Ctrl Pts',(17.1017263943771,72.2561377765807,15.0623873233133));
#56985=CARTESIAN_POINT('Ctrl Pts',(17.1063527464778,72.1968719525397,15.0826541852369));
#56986=CARTESIAN_POINT('Ctrl Pts',(17.1108831137178,72.1388357413225,15.1025005621049));
#56987=CARTESIAN_POINT('Ctrl Pts',(17.1154134809578,72.0797194742587,15.1192124147451));
#56988=CARTESIAN_POINT('Ctrl Pts',(17.1199438481978,72.0198979852371,15.132686408994));
#56989=CARTESIAN_POINT('Ctrl Pts',(17.1246181927289,71.9581753399763,15.1465886133836));
#56990=CARTESIAN_POINT('Ctrl Pts',(17.1292925372601,71.8957024531013,15.1570434910494));
#56991=CARTESIAN_POINT('Ctrl Pts',(17.1339668817913,71.832901938976,15.1639946453517));
#56992=CARTESIAN_POINT('Ctrl Pts',(17.1386412263225,71.7701014248507,15.170945799654));
#56993=CARTESIAN_POINT('Ctrl Pts',(17.1433155708536,71.7069738919126,15.1743932231441));
#56994=CARTESIAN_POINT('Ctrl Pts',(17.1479899153848,71.6439440199028,15.174339378094));
#56995=CARTESIAN_POINT('',(17.9417399154741,71.6466202076947,15.1743395632013));
#56996=CARTESIAN_POINT('Ctrl Pts',(17.1479899154299,71.6439440192947,15.1743393780935));
#56997=CARTESIAN_POINT('Ctrl Pts',(17.154145561567,71.5609399562498,15.1742684694964));
#56998=CARTESIAN_POINT('Ctrl Pts',(17.1603012077041,71.4781926934508,15.1681301741125));
#56999=CARTESIAN_POINT('Ctrl Pts',(17.1664568538413,71.3964381367899,15.1560583697687));
#57000=CARTESIAN_POINT('Ctrl Pts',(17.1696850060568,71.3535643023719,15.1497276579196));
#57001=CARTESIAN_POINT('Ctrl Pts',(17.1729131582724,71.3109630137133,15.1417659085998));
#57002=CARTESIAN_POINT('Ctrl Pts',(17.176141310488,71.2687378943283,15.132197489395));
#57003=CARTESIAN_POINT('Ctrl Pts',(17.1807454726154,71.2085141866116,15.1185505017749));
#57004=CARTESIAN_POINT('Ctrl Pts',(17.1853496347428,71.1489140648698,15.1015993488436));
#57005=CARTESIAN_POINT('Ctrl Pts',(17.1899537968702,71.0903257587081,15.0814178298177));
#57006=CARTESIAN_POINT('Ctrl Pts',(17.1945660030634,71.0316350912098,15.0612010510718));
#57007=CARTESIAN_POINT('Ctrl Pts',(17.1991782092565,70.9739602875218,15.0377426749009));
#57008=CARTESIAN_POINT('Ctrl Pts',(17.2037904154497,70.9176810449265,15.0111683743273));
#57009=CARTESIAN_POINT('Ctrl Pts',(17.2083823261224,70.8616494531249,14.9847110111241));
#57010=CARTESIAN_POINT('Ctrl Pts',(17.212974236795,70.8070016382065,14.9551652808883));
#57011=CARTESIAN_POINT('Ctrl Pts',(17.2175661474677,70.7540945097158,14.9227041538418));
#57012=CARTESIAN_POINT('Ctrl Pts',(17.2221553452153,70.7012186390359,14.8902622050005));
#57013=CARTESIAN_POINT('Ctrl Pts',(17.2267445429629,70.6500818466847,14.8549085400333));
#57014=CARTESIAN_POINT('Ctrl Pts',(17.2313337407104,70.6010156910675,14.8168616301817));
#57015=CARTESIAN_POINT('Ctrl Pts',(17.2359218974711,70.5519606653323,14.7788233506702));
#57016=CARTESIAN_POINT('Ctrl Pts',(17.2405100542317,70.5049757442545,14.7380933500799));
#57017=CARTESIAN_POINT('Ctrl Pts',(17.2450982109923,70.4603611203596,14.6949317080314));
#57018=CARTESIAN_POINT('Ctrl Pts',(17.2497272555352,70.4153489091278,14.6513854270277));
#57019=CARTESIAN_POINT('Ctrl Pts',(17.2543563000781,70.3727498524199,14.6053642886211));
#57020=CARTESIAN_POINT('Ctrl Pts',(17.2589853446209,70.3328341851558,14.5571733152089));
#57021=CARTESIAN_POINT('Ctrl Pts',(17.2635792121255,70.2932218450562,14.5093485546732));
#57022=CARTESIAN_POINT('Ctrl Pts',(17.2681730796301,70.2562525110266,14.4593872711379));
#57023=CARTESIAN_POINT('Ctrl Pts',(17.2727669471347,70.2221481483269,14.4076187937051));
#57024=CARTESIAN_POINT('Ctrl Pts',(17.2774135801968,70.1876520599828,14.3552556990863));
#57025=CARTESIAN_POINT('Ctrl Pts',(17.2820602132588,70.1560874600736,14.3010440817876));
#57026=CARTESIAN_POINT('Ctrl Pts',(17.2867068463208,70.1276362522913,14.245350270356));
#57027=CARTESIAN_POINT('Ctrl Pts',(17.2913534793828,70.0991850445089,14.1896564589244));
#57028=CARTESIAN_POINT('Ctrl Pts',(17.2960001124449,70.0738473865819,14.1324809633711));
#57029=CARTESIAN_POINT('Ctrl Pts',(17.3006467455069,70.0517541489216,14.07420835557));
#57030=CARTESIAN_POINT('Ctrl Pts',(17.305250907637,70.0298628468088,14.0164683682541));
#57031=CARTESIAN_POINT('Ctrl Pts',(17.3098550697672,70.0110703066881,13.957422991343));
#57032=CARTESIAN_POINT('Ctrl Pts',(17.3144592318973,69.9955294663945,13.8974366127747));
#57033=CARTESIAN_POINT('Ctrl Pts',(17.3190714380902,69.9799614742565,13.8373454302971));
#57034=CARTESIAN_POINT('Ctrl Pts',(17.323683644283,69.9676567804078,13.7763104165833));
#57035=CARTESIAN_POINT('Ctrl Pts',(17.3282958504759,69.9587203683434,13.7147175019381));
#57036=CARTESIAN_POINT('Ctrl Pts',(17.3328877611508,69.9498232800003,13.653395620297));
#57037=CARTESIAN_POINT('Ctrl Pts',(17.3374796718258,69.9442649925582,13.5915212371243));
#57038=CARTESIAN_POINT('Ctrl Pts',(17.3420715825008,69.9420984755528,13.5294874139279));
#57039=CARTESIAN_POINT('Ctrl Pts',(17.3466607802506,69.9399332385372,13.4674902406439));
#57040=CARTESIAN_POINT('Ctrl Pts',(17.3512499780003,69.9411558154965,13.4053343200391));
#57041=CARTESIAN_POINT('Ctrl Pts',(17.35583917575,69.9457672432653,13.3434167158172));
#57042=CARTESIAN_POINT('Ctrl Pts',(17.3604273325126,69.9503776250044,13.2815131566273));
#57043=CARTESIAN_POINT('Ctrl Pts',(17.3650154892753,69.9583752934179,13.2198483120309));
#57044=CARTESIAN_POINT('Ctrl Pts',(17.3696036460379,69.969709274973,13.1588160838692));
#57045=CARTESIAN_POINT('Ctrl Pts',(17.3742326905785,69.9811442603399,13.0972399614319));
#57046=CARTESIAN_POINT('Ctrl Pts',(17.3788617351191,69.9959752570609,13.036308308371));
#57047=CARTESIAN_POINT('Ctrl Pts',(17.3834907796598,70.0140972796604,12.976414880479));
#57048=CARTESIAN_POINT('Ctrl Pts',(17.388084647166,70.0320815893888,12.916976594714));
#57049=CARTESIAN_POINT('Ctrl Pts',(17.3926785146721,70.0533068491446,12.8585612725601));
#57050=CARTESIAN_POINT('Ctrl Pts',(17.3972723821783,70.0776211479283,12.8015358599022));
#57051=CARTESIAN_POINT('Ctrl Pts',(17.4019190152362,70.1022147228096,12.7438554485189));
#57052=CARTESIAN_POINT('Ctrl Pts',(17.4065656482941,70.1299685313298,12.6875975644117));
#57053=CARTESIAN_POINT('Ctrl Pts',(17.411212281352,70.1606776906095,12.633116197075));
#57054=CARTESIAN_POINT('Ctrl Pts',(17.4158589144098,70.1913868498893,12.5786348297384));
#57055=CARTESIAN_POINT('Ctrl Pts',(17.4205055474677,70.2250510219201,12.5259303923793));
#57056=CARTESIAN_POINT('Ctrl Pts',(17.4251521805256,70.2614219260227,12.4753244115039));
#57057=CARTESIAN_POINT('Ctrl Pts',(17.4297563427082,70.2974603949805,12.4251809763637));
#57058=CARTESIAN_POINT('Ctrl Pts',(17.4343605048907,70.3362987518513,12.3768995283544));
#57059=CARTESIAN_POINT('Ctrl Pts',(17.4389646670733,70.3777177308449,12.3308088395402));
#57060=CARTESIAN_POINT('Ctrl Pts',(17.4435768732596,70.4192090735843,12.2846376249629));
#57061=CARTESIAN_POINT('Ctrl Pts',(17.4481890794459,70.4632898039885,12.2406652747666));
#57062=CARTESIAN_POINT('Ctrl Pts',(17.4528012856322,70.5096962092413,12.1991924869374));
#57063=CARTESIAN_POINT('Ctrl Pts',(17.45739319636,70.5558984086906,12.1579021951217));
#57064=CARTESIAN_POINT('Ctrl Pts',(17.4619851070879,70.6044054971416,12.1190898735605));
#57065=CARTESIAN_POINT('Ctrl Pts',(17.4665770178157,70.6549190851283,12.0830168015167));
#57066=CARTESIAN_POINT('Ctrl Pts',(17.4711662156183,70.7054028294192,12.0469650416352));
#57067=CARTESIAN_POINT('Ctrl Pts',(17.4757554134209,70.7578903102951,12.0136496158755));
#57068=CARTESIAN_POINT('Ctrl Pts',(17.4803446112235,70.8120511148244,11.9832907240565));
#57069=CARTESIAN_POINT('Ctrl Pts',(17.4849327680389,70.8661996338284,11.9529387186738));
#57070=CARTESIAN_POINT('Ctrl Pts',(17.4895209248543,70.9220202805256,11.9255421633639));
#57071=CARTESIAN_POINT('Ctrl Pts',(17.4941090816697,70.9791565474556,11.9012761563801));
#57072=CARTESIAN_POINT('Ctrl Pts',(17.4987381261593,71.0368019881473,11.8767939012106));
#57073=CARTESIAN_POINT('Ctrl Pts',(17.5033671706488,71.0957861455202,11.8554985051479));
#57074=CARTESIAN_POINT('Ctrl Pts',(17.5079962151384,71.1557227980214,11.8375199623082));
#57075=CARTESIAN_POINT('Ctrl Pts',(17.5125900826965,71.2152039812526,11.8196780416092));
#57076=CARTESIAN_POINT('Ctrl Pts',(17.5171839502547,71.2756227198441,11.8051028014983));
#57077=CARTESIAN_POINT('Ctrl Pts',(17.5217778178128,71.3365892191394,11.7938703101418));
#57078=CARTESIAN_POINT('Ctrl Pts',(17.5264244507681,71.3982559827556,11.7825088018165));
#57079=CARTESIAN_POINT('Ctrl Pts',(17.5310710837234,71.4604826448642,11.7745674065155));
#57080=CARTESIAN_POINT('Ctrl Pts',(17.5357177166786,71.5228609497408,11.7700708789007));
#57081=CARTESIAN_POINT('Ctrl Pts',(17.5403643496339,71.5852392546174,11.7655743512858));
#57082=CARTESIAN_POINT('Ctrl Pts',(17.5450109825892,71.647768671106,11.7645226378518));
#57083=CARTESIAN_POINT('Ctrl Pts',(17.5496576155444,71.7100440314096,11.7668863852335));
#57084=CARTESIAN_POINT('Ctrl Pts',(17.5542617775941,71.7717501858019,11.7692285276179));
#57085=CARTESIAN_POINT('Ctrl Pts',(17.5588659396438,71.8334508596207,11.774933159723));
#57086=CARTESIAN_POINT('Ctrl Pts',(17.5634701016935,71.8947508729253,11.7839991169126));
#57087=CARTESIAN_POINT('Ctrl Pts',(17.5680823078964,71.9561579864345,11.7930809136726));
#57088=CARTESIAN_POINT('Ctrl Pts',(17.5726945140993,72.0171625250871,11.8055358197998));
#57089=CARTESIAN_POINT('Ctrl Pts',(17.5773067203022,72.0773681587226,11.8213101124075));
#57090=CARTESIAN_POINT('Ctrl Pts',(17.5818986308978,72.1373088627685,11.8370149916295));
#57091=CARTESIAN_POINT('Ctrl Pts',(17.5864905414935,72.1964571786997,11.8560100030348));
#57092=CARTESIAN_POINT('Ctrl Pts',(17.5910824520891,72.2544304800156,11.878190743207));
#57093=CARTESIAN_POINT('Ctrl Pts',(17.5956716497601,72.3123695304044,11.9003583788827));
#57094=CARTESIAN_POINT('Ctrl Pts',(17.6002608474311,72.3691344701657,11.9257078297304));
#57095=CARTESIAN_POINT('Ctrl Pts',(17.6048500451021,72.4243592263726,11.9540853060779));
#57096=CARTESIAN_POINT('Ctrl Pts',(17.6094382017868,72.4795714557233,11.9824563454469));
#57097=CARTESIAN_POINT('Ctrl Pts',(17.6140263584714,72.5332437443721,12.0138538146624));
#57098=CARTESIAN_POINT('Ctrl Pts',(17.618614515156,72.585033200847,12.048077258264));
#57099=CARTESIAN_POINT('Ctrl Pts',(17.6232435597733,72.6372841855461,12.0826056883673));
#57100=CARTESIAN_POINT('Ctrl Pts',(17.6278726043905,72.6876181564677,12.1200104517166));
#57101=CARTESIAN_POINT('Ctrl Pts',(17.6325016490078,72.7357134062617,12.1600414083926));
#57102=CARTESIAN_POINT('Ctrl Pts',(17.6370955164387,72.7834431690703,12.1997681605215));
#57103=CARTESIAN_POINT('Ctrl Pts',(17.6416893838697,72.8289677814321,12.2420809370951));
#57104=CARTESIAN_POINT('Ctrl Pts',(17.6462832513006,72.8720085140621,12.2866968313951));
#57105=CARTESIAN_POINT('Ctrl Pts',(17.650929884511,72.9155436183387,12.3318251898606));
#57106=CARTESIAN_POINT('Ctrl Pts',(17.6555765177215,72.9565370577431,12.37930951984));
#57107=CARTESIAN_POINT('Ctrl Pts',(17.6602231509319,72.9947426792337,12.4288231804356));
#57108=CARTESIAN_POINT('Ctrl Pts',(17.6648697841423,73.0329483007243,12.4783368410311));
#57109=CARTESIAN_POINT('Ctrl Pts',(17.6695164173527,73.0683658554946,12.5298793599239));
#57110=CARTESIAN_POINT('Ctrl Pts',(17.6741630505631,73.1007959998186,12.583096781316));
#57111=CARTESIAN_POINT('Ctrl Pts',(17.6787672126947,73.132929726682,12.6358277857267));
#57112=CARTESIAN_POINT('Ctrl Pts',(17.6833713748263,73.1622575108099,12.6904116401468));
#57113=CARTESIAN_POINT('Ctrl Pts',(17.6879755369578,73.1885620280686,12.7465182858378));
#57114=CARTESIAN_POINT('Ctrl Pts',(17.6925877431505,73.214912502689,12.8027229570269));
#57115=CARTESIAN_POINT('Ctrl Pts',(17.6971999493432,73.2382288299098,12.8604553332266));
#57116=CARTESIAN_POINT('Ctrl Pts',(17.7018121555359,73.2583368619122,12.9193553640644));
#57117=CARTESIAN_POINT('Ctrl Pts',(17.7064040662101,73.2783564106775,12.9779962116365));
#57118=CARTESIAN_POINT('Ctrl Pts',(17.7109959768843,73.2951956498906,13.03779398638));
#57119=CARTESIAN_POINT('Ctrl Pts',(17.7155878875585,73.3087302479811,13.0983720654324));
#57120=CARTESIAN_POINT('Ctrl Pts',(17.7201770853067,73.3222568497568,13.158914354623));
#57121=CARTESIAN_POINT('Ctrl Pts',(17.7247662830548,73.3324825720767,13.2202355398255));
#57122=CARTESIAN_POINT('Ctrl Pts',(17.729355480803,73.3393333950186,13.2819455162975));
#57123=CARTESIAN_POINT('Ctrl Pts',(17.7339436375632,73.3461826639582,13.3436414948236));
#57124=CARTESIAN_POINT('Ctrl Pts',(17.7385317943235,73.3496584977824,13.4057255856276));
#57125=CARTESIAN_POINT('Ctrl Pts',(17.7431199510837,73.3497385816819,13.4678012297476));
#57126=CARTESIAN_POINT('Ctrl Pts',(17.7477489956252,73.3498193792564,13.530430066684));
#57127=CARTESIAN_POINT('Ctrl Pts',(17.7523780401667,73.346443567122,13.5930497816456));
#57128=CARTESIAN_POINT('Ctrl Pts',(17.7570070847083,73.3396419485777,13.6552540290513));
#57129=CARTESIAN_POINT('Ctrl Pts',(17.7616009522102,73.3328920168994,13.7169855738816));
#57130=CARTESIAN_POINT('Ctrl Pts',(17.766194819712,73.3227683069389,13.778307446046));
#57131=CARTESIAN_POINT('Ctrl Pts',(17.7707886872139,73.30935267667,13.8388310255427));
#57132=CARTESIAN_POINT('Ctrl Pts',(17.7754353202753,73.2957829533114,13.9000497841081));
#57133=CARTESIAN_POINT('Ctrl Pts',(17.7800819533366,73.2788453317756,13.9604512774611));
#57134=CARTESIAN_POINT('Ctrl Pts',(17.7847285863979,73.2586761210118,14.0196498821734));
#57135=CARTESIAN_POINT('Ctrl Pts',(17.7893752194593,73.2385069102479,14.0788484868857));
#57136=CARTESIAN_POINT('Ctrl Pts',(17.7940218525206,73.2151063665341,14.1368437346505));
#57137=CARTESIAN_POINT('Ctrl Pts',(17.7986684855819,73.188659425232,14.1932739329139));
#57138=CARTESIAN_POINT('Ctrl Pts',(17.8032726480834,73.1624542108728,14.2491883551123));
#57139=CARTESIAN_POINT('Ctrl Pts',(17.8078768105848,73.1331545058933,14.3037872928552));
#57140=CARTESIAN_POINT('Ctrl Pts',(17.8124809730863,73.1009153932975,14.3567072659418));
#57141=CARTESIAN_POINT('Ctrl Pts',(17.8170931792327,73.0686199577599,14.4097196922112));
#57142=CARTESIAN_POINT('Ctrl Pts',(17.8217053853791,73.0333750087894,14.461046798619));
#57143=CARTESIAN_POINT('Ctrl Pts',(17.8263175915256,72.9953844801837,14.5103445289244));
#57144=CARTESIAN_POINT('Ctrl Pts',(17.8309095025744,72.9575611213583,14.559425334353));
#57145=CARTESIAN_POINT('Ctrl Pts',(17.8355014136231,72.9170165837424,14.606494165908));
#57146=CARTESIAN_POINT('Ctrl Pts',(17.8400933246719,72.8739961339218,14.6512393387085));
#57147=CARTESIAN_POINT('Ctrl Pts',(17.8446825227953,72.8310011008107,14.6959580758239));
#57148=CARTESIAN_POINT('Ctrl Pts',(17.8492717209188,72.7855334073483,14.7383555119124));
#57149=CARTESIAN_POINT('Ctrl Pts',(17.8538609190422,72.7378773502305,14.7781544537375));
#57150=CARTESIAN_POINT('Ctrl Pts',(17.8584490761777,72.690232103145,14.8179443677942));
#57151=CARTESIAN_POINT('Ctrl Pts',(17.8630372333132,72.6403998672494,14.8551366331016));
#57152=CARTESIAN_POINT('Ctrl Pts',(17.8676253904487,72.5886988809515,14.8894935916712));
#57153=CARTESIAN_POINT('Ctrl Pts',(17.872254434628,72.5365371649029,14.9241567198923));
#57154=CARTESIAN_POINT('Ctrl Pts',(17.8768834788074,72.482473643401,14.9559334375672));
#57155=CARTESIAN_POINT('Ctrl Pts',(17.8815125229867,72.4268640547575,14.9846249590978));
#57156=CARTESIAN_POINT('Ctrl Pts',(17.8861063908595,72.371677045778,15.0130984525181));
#57157=CARTESIAN_POINT('Ctrl Pts',(17.8907002587324,72.3149678786595,15.0385333196578));
#57158=CARTESIAN_POINT('Ctrl Pts',(17.8952941266052,72.2571057184215,15.0607831246435));
#57159=CARTESIAN_POINT('Ctrl Pts',(17.8999407589378,72.1985789623117,15.0832884874666));
#57160=CARTESIAN_POINT('Ctrl Pts',(17.9045873912704,72.1388730591315,15.1025349754775));
#57161=CARTESIAN_POINT('Ctrl Pts',(17.909234023603,72.078384754109,15.1184231975768));
#57162=CARTESIAN_POINT('Ctrl Pts',(17.9138806559356,72.0178964490865,15.134311419676));
#57163=CARTESIAN_POINT('Ctrl Pts',(17.9185272882681,71.9566262741602,15.1468413308028));
#57164=CARTESIAN_POINT('Ctrl Pts',(17.9231739206007,71.894977887111,15.1559672932371));
#57165=CARTESIAN_POINT('Ctrl Pts',(17.9293625855438,71.8128708503543,15.1681217999306));
#57166=CARTESIAN_POINT('Ctrl Pts',(17.9355512504868,71.7298551795929,15.1742799717883));
#57167=CARTESIAN_POINT('Ctrl Pts',(17.9417399154298,71.6466202082904,15.1743395632009));
#57168=CARTESIAN_POINT('',(18.7354899154876,71.6451863826151,15.1743399866129));
#57169=CARTESIAN_POINT('Ctrl Pts',(17.9417399154741,71.6466202076947,15.1743395632013));
#57170=CARTESIAN_POINT('Ctrl Pts',(17.9462717923975,71.585668346648,15.1743832011778));
#57171=CARTESIAN_POINT('Ctrl Pts',(17.950803669321,71.5245990262305,15.1711528932889));
#57172=CARTESIAN_POINT('Ctrl Pts',(17.9553355462444,71.4637980963487,15.1646373016638));
#57173=CARTESIAN_POINT('Ctrl Pts',(17.9598626640451,71.4030610161902,15.1581285523472));
#57174=CARTESIAN_POINT('Ctrl Pts',(17.9643897818458,71.3425922856912,15.1483414059901));
#57175=CARTESIAN_POINT('Ctrl Pts',(17.9689168996465,71.2827767009868,15.1353165400646));
#57176=CARTESIAN_POINT('Ctrl Pts',(17.9734410287427,71.2230006052276,15.1223002728717));
#57177=CARTESIAN_POINT('Ctrl Pts',(17.9779651578389,71.1638773111853,15.1060506318105));
#57178=CARTESIAN_POINT('Ctrl Pts',(17.9824892869351,71.1057832030213,15.0866596883755));
#57179=CARTESIAN_POINT('Ctrl Pts',(17.9870121931421,71.0477047979148,15.0672739863861));
#57180=CARTESIAN_POINT('Ctrl Pts',(17.9915350993491,70.9906555229741,15.0447488323605));
#57181=CARTESIAN_POINT('Ctrl Pts',(17.9960580055561,70.9349961577852,15.0192260056449));
#57182=CARTESIAN_POINT('Ctrl Pts',(18.0005845415412,70.87929212416,14.9936826960374));
#57183=CARTESIAN_POINT('Ctrl Pts',(18.0051110775263,70.8249807064607,14.9651371243569));
#57184=CARTESIAN_POINT('Ctrl Pts',(18.0096376135114,70.7724008933841,14.9337784652904));
#57185=CARTESIAN_POINT('Ctrl Pts',(18.0141659003803,70.7198007422072,14.9024076765582));
#57186=CARTESIAN_POINT('Ctrl Pts',(18.0186941872493,70.6689339652024,14.8682219251408));
#57187=CARTESIAN_POINT('Ctrl Pts',(18.0232224741182,70.6201104803191,14.8314537217374));
#57188=CARTESIAN_POINT('Ctrl Pts',(18.0277588628083,70.5711996425019,14.7946197342047));
#57189=CARTESIAN_POINT('Ctrl Pts',(18.0322952514984,70.5243397990785,14.7551944049274));
#57190=CARTESIAN_POINT('Ctrl Pts',(18.0368316401885,70.4798068340605,14.7134498008023));
#57191=CARTESIAN_POINT('Ctrl Pts',(18.0404475453321,70.4443101012468,14.6801756395501));
#57192=CARTESIAN_POINT('Ctrl Pts',(18.0440634504758,70.4102911126563,14.6454287521193));
#57193=CARTESIAN_POINT('Ctrl Pts',(18.0476793556195,70.3778711177324,14.6093618249781));
#57194=CARTESIAN_POINT('Ctrl Pts',(18.0522835180563,70.3365904654751,14.5634375032501));
#57195=CARTESIAN_POINT('Ctrl Pts',(18.0568876804932,70.2977272769018,14.5151760381375));
#57196=CARTESIAN_POINT('Ctrl Pts',(18.06149184293,70.2615558534696,14.4648619068562));
#57197=CARTESIAN_POINT('Ctrl Pts',(18.0661040490845,70.225321236629,14.4144598741006));
#57198=CARTESIAN_POINT('Ctrl Pts',(18.070716255239,70.1917881761899,14.3619983451011));
#57199=CARTESIAN_POINT('Ctrl Pts',(18.0753284613936,70.161194047235,14.3077992154312));
#57200=CARTESIAN_POINT('Ctrl Pts',(18.0799203723543,70.1307345423091,14.2538385794021));
#57201=CARTESIAN_POINT('Ctrl Pts',(18.0845122833151,70.1031884329188,14.1981560322717));
#57202=CARTESIAN_POINT('Ctrl Pts',(18.0891041942758,70.0787471739964,14.1410989184725));
#57203=CARTESIAN_POINT('Ctrl Pts',(18.0936933923027,70.0543203551446,14.0840755144241));
#57204=CARTESIAN_POINT('Ctrl Pts',(18.0982825903297,70.0329949481222,14.0256796195907));
#57205=CARTESIAN_POINT('Ctrl Pts',(18.1028717883566,70.0149154324902,13.9662810803491));
#57206=CARTESIAN_POINT('Ctrl Pts',(18.1074599453874,69.9968400179464,13.906896014845));
#57207=CARTESIAN_POINT('Ctrl Pts',(18.1120481024182,69.9820091803124,13.8465092415604));
#57208=CARTESIAN_POINT('Ctrl Pts',(18.116636259449,69.9705177620195,13.7855064571404));
#57209=CARTESIAN_POINT('Ctrl Pts',(18.1212653037147,69.958923938269,13.7239600480877));
#57210=CARTESIAN_POINT('Ctrl Pts',(18.1258943479805,69.9507294795822,13.661787102663));
#57211=CARTESIAN_POINT('Ctrl Pts',(18.1305233922463,69.9459788150061,13.599392703017));
#57212=CARTESIAN_POINT('Ctrl Pts',(18.1351172599958,69.9412642511498,13.5374724439251));
#57213=CARTESIAN_POINT('Ctrl Pts',(18.1397111277453,69.9399412755248,13.4753345999021));
#57214=CARTESIAN_POINT('Ctrl Pts',(18.1443049954948,69.9420008739233,13.4133762162947));
#57215=CARTESIAN_POINT('Ctrl Pts',(18.1489516280187,69.9440841286939,13.3507061839613));
#57216=CARTESIAN_POINT('Ctrl Pts',(18.1535982605426,69.949628127205,13.2882202924725));
#57217=CARTESIAN_POINT('Ctrl Pts',(18.1582448930665,69.9585697815553,13.2263226523824));
#57218=CARTESIAN_POINT('Ctrl Pts',(18.1628915255904,69.9675114359056,13.1644250122922));
#57219=CARTESIAN_POINT('Ctrl Pts',(18.1675381581143,69.9798505802848,13.1031161310414));
#57220=CARTESIAN_POINT('Ctrl Pts',(18.1721847906382,69.9954719295671,13.0427855362965));
#57221=CARTESIAN_POINT('Ctrl Pts',(18.176788955474,70.0109505082331,12.9830063302976));
#57222=CARTESIAN_POINT('Ctrl Pts',(18.1813931203098,70.0297126859196,12.9239512599727));
#57223=CARTESIAN_POINT('Ctrl Pts',(18.1859972851456,70.051672849213,12.8660061221797));
#57224=CARTESIAN_POINT('Ctrl Pts',(18.1906094910002,70.0736713651922,12.8079597851546));
#57225=CARTESIAN_POINT('Ctrl Pts',(18.1952216968549,70.0988789650903,12.7510277683002));
#57226=CARTESIAN_POINT('Ctrl Pts',(18.1998339027095,70.1271584465421,12.69558575623));
#57227=CARTESIAN_POINT('Ctrl Pts',(18.2044258161163,70.1553135059884,12.640387673892));
#57228=CARTESIAN_POINT('Ctrl Pts',(18.2090177295231,70.1865132661784,12.5866669785811));
#57229=CARTESIAN_POINT('Ctrl Pts',(18.2136096429299,70.2205739447844,12.5347751350724));
#57230=CARTESIAN_POINT('Ctrl Pts',(18.2181988434134,70.2546145001867,12.4829139495009));
#57231=CARTESIAN_POINT('Ctrl Pts',(18.2227880438968,70.2915123441123,12.4328798960513));
#57232=CARTESIAN_POINT('Ctrl Pts',(18.2273772443803,70.3310389880981,12.3849977115267));
#57233=CARTESIAN_POINT('Ctrl Pts',(18.2319654038738,70.3705566660694,12.3371263883432));
#57234=CARTESIAN_POINT('Ctrl Pts',(18.2365535633674,70.4127016372396,12.2914063557475));
#57235=CARTESIAN_POINT('Ctrl Pts',(18.2411417228609,70.4572047813951,12.2481297294375));
#57236=CARTESIAN_POINT('Ctrl Pts',(18.2457707647606,70.5021044670432,12.2044674904182));
#57237=CARTESIAN_POINT('Ctrl Pts',(18.2503998066603,70.5494042079811,12.1632928081916));
#57238=CARTESIAN_POINT('Ctrl Pts',(18.2550288485599,70.5987908775215,12.1248664823354));
#57239=CARTESIAN_POINT('Ctrl Pts',(18.2596227187584,70.6478023045769,12.0867321217026));
#57240=CARTESIAN_POINT('Ctrl Pts',(18.2642165889569,70.6988686009911,12.0513047425673));
#57241=CARTESIAN_POINT('Ctrl Pts',(18.2688104591553,70.7516538167364,12.0187961564612));
#57242=CARTESIAN_POINT('Ctrl Pts',(18.2734570869056,70.8050452356688,11.9859142308087));
#57243=CARTESIAN_POINT('Ctrl Pts',(18.2781037146559,70.8601948474178,11.9560188353314));
#57244=CARTESIAN_POINT('Ctrl Pts',(18.2827503424062,70.916730944274,11.9292806086677));
#57245=CARTESIAN_POINT('Ctrl Pts',(18.2873969701565,70.9732670411301,11.902542382004));
#57246=CARTESIAN_POINT('Ctrl Pts',(18.2920435979068,71.0311891085112,11.8789614662436));
#57247=CARTESIAN_POINT('Ctrl Pts',(18.296690225657,71.0901087614014,11.8586569341274));
#57248=CARTESIAN_POINT('Ctrl Pts',(18.3012943804412,71.1484898533054,11.8385379976199));
#57249=CARTESIAN_POINT('Ctrl Pts',(18.3058985352253,71.2080811556222,11.821556207845));
#57250=CARTESIAN_POINT('Ctrl Pts',(18.3105026900094,71.2685137839003,11.8078533110119));
#57251=CARTESIAN_POINT('Ctrl Pts',(18.3151148971205,71.3290521043859,11.7941264488234));
#57252=CARTESIAN_POINT('Ctrl Pts',(18.3197271042316,71.3904342281563,11.7836901707823));
#57253=CARTESIAN_POINT('Ctrl Pts',(18.3243393113427,71.4522711997435,11.7766376341398));
#57254=CARTESIAN_POINT('Ctrl Pts',(18.3289312147021,71.5138359540407,11.7696161440116));
#57255=CARTESIAN_POINT('Ctrl Pts',(18.3335231180614,71.5758510573455,11.7659487512926));
#57256=CARTESIAN_POINT('Ctrl Pts',(18.3381150214207,71.6379220157181,11.7656764053294));
#57257=CARTESIAN_POINT('Ctrl Pts',(18.342704211887,71.6999563026153,11.7654042202679));
#57258=CARTESIAN_POINT('Ctrl Pts',(18.3472934023533,71.762045872943,11.7685231062559));
#57259=CARTESIAN_POINT('Ctrl Pts',(18.3518825928196,71.823793817313,11.7750219819878));
#57260=CARTESIAN_POINT('Ctrl Pts',(18.3564707423432,71.8855277557106,11.7815193836128));
#57261=CARTESIAN_POINT('Ctrl Pts',(18.3610588918667,71.9469197178515,11.7913951994893));
#57262=CARTESIAN_POINT('Ctrl Pts',(18.3656470413903,72.0075775420149,11.8045864586656));
#57263=CARTESIAN_POINT('Ctrl Pts',(18.3702760929974,72.0687761138982,11.8178953142678));
#57264=CARTESIAN_POINT('Ctrl Pts',(18.3749051446046,72.129226873885,11.8345789426527));
#57265=CARTESIAN_POINT('Ctrl Pts',(18.3795341962117,72.1885394510549,11.8545203893865));
#57266=CARTESIAN_POINT('Ctrl Pts',(18.3841280566705,72.2474011199443,11.8743102365123));
#57267=CARTESIAN_POINT('Ctrl Pts',(18.3887219171293,72.3051413956357,11.8973082953942));
#57268=CARTESIAN_POINT('Ctrl Pts',(18.3933157775881,72.3613981403934,11.9233515271552));
#57269=CARTESIAN_POINT('Ctrl Pts',(18.3979624247694,72.4183013151414,11.9496940141633));
#57270=CARTESIAN_POINT('Ctrl Pts',(18.4026090719507,72.4736861697953,11.9791518683659));
#57271=CARTESIAN_POINT('Ctrl Pts',(18.407255719132,72.5272051290434,12.011509496091));
#57272=CARTESIAN_POINT('Ctrl Pts',(18.4119023663132,72.5807240882916,12.0438671238161));
#57273=CARTESIAN_POINT('Ctrl Pts',(18.4165490134945,72.6323767494258,12.0791241745914));
#57274=CARTESIAN_POINT('Ctrl Pts',(18.4211956606758,72.6818493101953,12.1170226672277));
#57275=CARTESIAN_POINT('Ctrl Pts',(18.4257998281339,72.7308695920193,12.1545746912353));
#57276=CARTESIAN_POINT('Ctrl Pts',(18.430403995592,72.7779433012867,12.1948684785823));
#57277=CARTESIAN_POINT('Ctrl Pts',(18.43500816305,72.8227485102806,12.2376748314913));
#57278=CARTESIAN_POINT('Ctrl Pts',(18.4396203685769,72.8676319413103,12.2805559167839));
#57279=CARTESIAN_POINT('Ctrl Pts',(18.4442325741038,72.9102385090048,12.3259580752481));
#57280=CARTESIAN_POINT('Ctrl Pts',(18.4488447796306,72.9502757042091,12.3736085406367));
#57281=CARTESIAN_POINT('Ctrl Pts',(18.453436695458,72.990136770519,12.4210493853528));
#57282=CARTESIAN_POINT('Ctrl Pts',(18.4580286112853,73.0274506743401,12.4707184253993));
#57283=CARTESIAN_POINT('Ctrl Pts',(18.4626205271126,73.0619653640192,12.5223094360176));
#57284=CARTESIAN_POINT('Ctrl Pts',(18.4672097299348,73.0964596616579,12.5738699655283));
#57285=CARTESIAN_POINT('Ctrl Pts',(18.4717989327569,73.1281577436136,12.6273497928535));
#57286=CARTESIAN_POINT('Ctrl Pts',(18.4763881355791,73.1568495958325,12.6824119383474));
#57287=CARTESIAN_POINT('Ctrl Pts',(18.4809762973261,73.1855349392146,12.7374615928207));
#57288=CARTESIAN_POINT('Ctrl Pts',(18.4855644590732,73.211215172838,12.7940924030778));
#57289=CARTESIAN_POINT('Ctrl Pts',(18.4901526208202,73.2337261595506,12.8519426834936));
#57290=CARTESIAN_POINT('Ctrl Pts',(18.4947816603931,73.2564377059305,12.9103083759232));
#57291=CARTESIAN_POINT('Ctrl Pts',(18.4994106999659,73.2759230296784,12.9699149004168));
#57292=CARTESIAN_POINT('Ctrl Pts',(18.5040397395388,73.2920639842587,13.0303722500284));
#57293=CARTESIAN_POINT('Ctrl Pts',(18.5086336117589,73.3080823141274,13.0903702981142));
#57294=CARTESIAN_POINT('Ctrl Pts',(18.5132274839791,73.3208068662135,13.1512057732044));
#57295=CARTESIAN_POINT('Ctrl Pts',(18.5178213561992,73.3301735030541,13.2124867401343));
#57296=CARTESIAN_POINT('Ctrl Pts',(18.5224679794484,73.3396476961586,13.2744713909966));
#57297=CARTESIAN_POINT('Ctrl Pts',(18.5271146026976,73.3456862965543,13.3369113020137));
#57298=CARTESIAN_POINT('Ctrl Pts',(18.5317612259469,73.3482770197843,13.3993976552055));
#57299=CARTESIAN_POINT('Ctrl Pts',(18.5364078491961,73.3508677430143,13.4618840083973));
#57300=CARTESIAN_POINT('Ctrl Pts',(18.5410544724453,73.3500106587655,13.524416274497));
#57301=CARTESIAN_POINT('Ctrl Pts',(18.5457010956945,73.3457474705212,13.5865903730673));
#57302=CARTESIAN_POINT('Ctrl Pts',(18.5503052764862,73.3415232224227,13.6481965707345));
#57303=CARTESIAN_POINT('Ctrl Pts',(18.5549094572779,73.333938189835,13.7096946632185));
#57304=CARTESIAN_POINT('Ctrl Pts',(18.5595136380695,73.3230055995048,13.7706896874024));
#57305=CARTESIAN_POINT('Ctrl Pts',(18.5641258419297,73.3120539584629,13.8317909991711));
#57306=CARTESIAN_POINT('Ctrl Pts',(18.5687380457898,73.2977430700227,13.8923869741468));
#57307=CARTESIAN_POINT('Ctrl Pts',(18.57335024965,73.2801387287715,13.9520831092813));
#57308=CARTESIAN_POINT('Ctrl Pts',(18.5779421792581,73.2626117724025,14.0115168330985));
#57309=CARTESIAN_POINT('Ctrl Pts',(18.5825341088662,73.2418203745654,14.0700581154847));
#57310=CARTESIAN_POINT('Ctrl Pts',(18.5871260384743,73.2178805692773,14.1273276921333));
#57311=CARTESIAN_POINT('Ctrl Pts',(18.5917152552039,73.1939549074511,14.1845634343347));
#57312=CARTESIAN_POINT('Ctrl Pts',(18.5963044719336,73.1668847223054,14.2405284937931));
#57313=CARTESIAN_POINT('Ctrl Pts',(18.6008936886632,73.1368349058593,14.2948616594219));
#57314=CARTESIAN_POINT('Ctrl Pts',(18.6054818644196,73.1067919056215,14.3491825006437));
#57315=CARTESIAN_POINT('Ctrl Pts',(18.6100700401759,73.0737708615674,14.4018717394724));
#57316=CARTESIAN_POINT('Ctrl Pts',(18.6146582159323,73.037982602253,14.4525927597444));
#57317=CARTESIAN_POINT('Ctrl Pts',(18.619287242164,73.0018757048819,14.5037653707796));
#57318=CARTESIAN_POINT('Ctrl Pts',(18.6239162683958,72.9629523455289,14.5529340929907));
#57319=CARTESIAN_POINT('Ctrl Pts',(18.6285452946276,72.9214723610863,14.5997850082523));
#57320=CARTESIAN_POINT('Ctrl Pts',(18.633139180939,72.880307260007,14.6462802682752));
#57321=CARTESIAN_POINT('Ctrl Pts',(18.6377330672504,72.8366246183834,14.6904924650606));
#57322=CARTESIAN_POINT('Ctrl Pts',(18.6423269535618,72.7907157191772,14.7321516307503));
#57323=CARTESIAN_POINT('Ctrl Pts',(18.6469735497538,72.7442800649696,14.7742887903423));
#57324=CARTESIAN_POINT('Ctrl Pts',(18.6516201459457,72.6955671421928,14.8138136103111));
#57325=CARTESIAN_POINT('Ctrl Pts',(18.6562667421376,72.6449109413609,14.8504900266572));
#57326=CARTESIAN_POINT('Ctrl Pts',(18.6609133383295,72.594254740529,14.8871664430032));
#57327=CARTESIAN_POINT('Ctrl Pts',(18.6655599345214,72.5416557412991,14.9209942214633));
#57328=CARTESIAN_POINT('Ctrl Pts',(18.6702065307133,72.4874738068746,14.9517849167054));
#57329=CARTESIAN_POINT('Ctrl Pts',(18.6749930460121,72.4316603366847,14.9835027866795));
#57330=CARTESIAN_POINT('Ctrl Pts',(18.6797795613109,72.373961918635,15.0121150505961));
#57331=CARTESIAN_POINT('Ctrl Pts',(18.6845660766097,72.3147425716321,15.0374040185609));
#57332=CARTESIAN_POINT('Ctrl Pts',(18.6893401544225,72.2556771027128,15.0626272745899));
#57333=CARTESIAN_POINT('Ctrl Pts',(18.6941142322353,72.1950989810462,15.0845442444087));
#57334=CARTESIAN_POINT('Ctrl Pts',(18.698888310048,72.1333960632559,15.1029833672903));
#57335=CARTESIAN_POINT('Ctrl Pts',(18.7036549356628,72.0717894619435,15.121393707232));
#57336=CARTESIAN_POINT('Ctrl Pts',(18.7084215612776,72.009061981251,15.1363368575986));
#57337=CARTESIAN_POINT('Ctrl Pts',(18.7131881868923,71.9456203696711,15.1476896510483));
#57338=CARTESIAN_POINT('Ctrl Pts',(18.717946530032,71.8822889940553,15.1590227179163));
#57339=CARTESIAN_POINT('Ctrl Pts',(18.7227048731716,71.8182463977651,15.1667777619715));
#57340=CARTESIAN_POINT('Ctrl Pts',(18.7274632163113,71.7539115768951,15.1708821456173));
#57341=CARTESIAN_POINT('Ctrl Pts',(18.7301387826841,71.7177367827973,15.173189997435));
#57342=CARTESIAN_POINT('Ctrl Pts',(18.732814349057,71.6814698195352,15.1743445342645));
#57343=CARTESIAN_POINT('Ctrl Pts',(18.7354899154298,71.6451863833987,15.174339986613));
#57344=CARTESIAN_POINT('Ctrl Pts',(18.7354899154876,71.6451863826151,15.1743399866129));
#57345=CARTESIAN_POINT('Ctrl Pts',(18.7404250863413,71.5782603820836,15.1743315982882));
#57346=CARTESIAN_POINT('Ctrl Pts',(18.745360257195,71.5114232487074,15.1703765618724));
#57347=CARTESIAN_POINT('Ctrl Pts',(18.7502954280487,71.4451369577199,15.1625334707168));
#57348=CARTESIAN_POINT('Ctrl Pts',(18.7551622095479,71.3797692320236,15.1547990655536));
#57349=CARTESIAN_POINT('Ctrl Pts',(18.7600289910471,71.3149375632485,15.1432838780447));
#57350=CARTESIAN_POINT('Ctrl Pts',(18.7648957725463,71.2510718358305,15.1280953333698));
#57351=CARTESIAN_POINT('Ctrl Pts',(18.7698651380773,71.185859920216,15.1125866382732));
#57352=CARTESIAN_POINT('Ctrl Pts',(18.7748345036083,71.1216555675429,15.0932481155449));
#57353=CARTESIAN_POINT('Ctrl Pts',(18.7798038691392,71.0588960841977,15.0702462286625));
#57354=CARTESIAN_POINT('Ctrl Pts',(18.7847732346702,70.9961366008525,15.0472443417801));
#57355=CARTESIAN_POINT('Ctrl Pts',(18.7897426002011,70.9348223677971,15.0205793412336));
#57356=CARTESIAN_POINT('Ctrl Pts',(18.7947119657321,70.8753642096513,14.9904669405094));
#57357=CARTESIAN_POINT('Ctrl Pts',(18.799316195139,70.8202748831543,14.962567121093));
#57358=CARTESIAN_POINT('Ctrl Pts',(18.803920424546,70.7665949169974,14.9316143274008));
#57359=CARTESIAN_POINT('Ctrl Pts',(18.8085246539529,70.7146828958061,14.8977746697434));
#57360=CARTESIAN_POINT('Ctrl Pts',(18.8131368517362,70.6626810323236,14.8638764469925));
#57361=CARTESIAN_POINT('Ctrl Pts',(18.8177490495194,70.6124537165645,14.8270815477019));
#57362=CARTESIAN_POINT('Ctrl Pts',(18.8223612473027,70.564338610821,14.7876043064693));
#57363=CARTESIAN_POINT('Ctrl Pts',(18.8269532238489,70.5164344559088,14.7483001451194));
#57364=CARTESIAN_POINT('Ctrl Pts',(18.8315452003952,70.4706244396919,14.70633741437));
#57365=CARTESIAN_POINT('Ctrl Pts',(18.8361371769414,70.4272126232424,14.6619707843351));
#57366=CARTESIAN_POINT('Ctrl Pts',(18.8407264398518,70.3838264610755,14.6176303728315));
#57367=CARTESIAN_POINT('Ctrl Pts',(18.8453157027621,70.3428360420209,14.5708892411813));
#57368=CARTESIAN_POINT('Ctrl Pts',(18.8499049656725,70.3045097605242,14.5220400188578));
#57369=CARTESIAN_POINT('Ctrl Pts',(18.8544931867798,70.2661921794301,14.4732018857371));
#57370=CARTESIAN_POINT('Ctrl Pts',(18.8590814078871,70.2305378478503,14.4222570110851));
#57371=CARTESIAN_POINT('Ctrl Pts',(18.8636696289945,70.1977746077564,14.3695307439613));
#57372=CARTESIAN_POINT('Ctrl Pts',(18.8682986099742,70.1647203124902,14.3163360783301));
#57373=CARTESIAN_POINT('Ctrl Pts',(18.8729275909539,70.1346090361727,14.2613286395754));
#57374=CARTESIAN_POINT('Ctrl Pts',(18.8775565719336,70.1076286077453,14.204870043452));
#57375=CARTESIAN_POINT('Ctrl Pts',(18.8821505010633,70.0808524821512,14.1488389665277));
#57376=CARTESIAN_POINT('Ctrl Pts',(18.8867444301931,70.0571600946983,14.0913791310703));
#57377=CARTESIAN_POINT('Ctrl Pts',(18.8913383593228,70.0366865554042,14.0328640055793));
#57378=CARTESIAN_POINT('Ctrl Pts',(18.8959848662275,70.0159786953117,13.9736791712154));
#57379=CARTESIAN_POINT('Ctrl Pts',(18.9006313731322,69.9985639957566,13.9134152439124));
#57380=CARTESIAN_POINT('Ctrl Pts',(18.9052778800368,69.9845296933773,13.8524717769704));
#57381=CARTESIAN_POINT('Ctrl Pts',(18.9099243869415,69.9704953909979,13.7915283100284));
#57382=CARTESIAN_POINT('Ctrl Pts',(18.9145708938462,69.9598415146185,13.7299058363891));
#57383=CARTESIAN_POINT('Ctrl Pts',(18.9192174007509,69.9526013703753,13.6680091794354));
#57384=CARTESIAN_POINT('Ctrl Pts',(18.9238216793447,69.945427025897,13.6066750507048));
#57385=CARTESIAN_POINT('Ctrl Pts',(18.9284259579385,69.9415762144442,13.5448293225974));
#57386=CARTESIAN_POINT('Ctrl Pts',(18.9330302365323,69.941108538074,13.4828626749172));
#57387=CARTESIAN_POINT('Ctrl Pts',(18.9376424281672,69.9406400579421,13.4207895296351));
#57388=CARTESIAN_POINT('Ctrl Pts',(18.9422546198021,69.9435664584075,13.3585955513503));
#57389=CARTESIAN_POINT('Ctrl Pts',(18.946866811437,69.9498955848858,13.2966806014082));
#57390=CARTESIAN_POINT('Ctrl Pts',(18.9514588412422,69.95619704409,13.2350363077556));
#57391=CARTESIAN_POINT('Ctrl Pts',(18.9560508710474,69.965871517759,13.1736691171281));
#57392=CARTESIAN_POINT('Ctrl Pts',(18.9606429008527,69.9788746679288,13.1129731758468));
#57393=CARTESIAN_POINT('Ctrl Pts',(18.9652322183829,69.9918701378089,13.0523130845251));
#57394=CARTESIAN_POINT('Ctrl Pts',(18.9698215359132,70.0081902789825,12.992323951191));
#57395=CARTESIAN_POINT('Ctrl Pts',(18.9744108534434,70.027739409392,12.9333911581107));
#57396=CARTESIAN_POINT('Ctrl Pts',(18.9789991304254,70.047284107375,12.8744717270197));
#57397=CARTESIAN_POINT('Ctrl Pts',(18.9835874074075,70.0700561811619,12.8166086417205));
#57398=CARTESIAN_POINT('Ctrl Pts',(18.9881756843895,70.0959102736314,12.7601715534875));
#57399=CARTESIAN_POINT('Ctrl Pts',(18.9928046136712,70.1219934342932,12.7032344306163));
#57400=CARTESIAN_POINT('Ctrl Pts',(18.9974335429529,70.1512133108252,12.647749189379));
#57401=CARTESIAN_POINT('Ctrl Pts',(19.0020624722345,70.1833722265965,12.5940721345927));
#57402=CARTESIAN_POINT('Ctrl Pts',(19.006656459615,70.2152883878152,12.5408002660236));
#57403=CARTESIAN_POINT('Ctrl Pts',(19.0112504469955,70.2500990333393,12.4893097723984));
#57404=CARTESIAN_POINT('Ctrl Pts',(19.015844434376,70.2875674718241,12.4399195851646));
#57405=CARTESIAN_POINT('Ctrl Pts',(19.0204908346083,70.3254633881294,12.3899659047496));
#57406=CARTESIAN_POINT('Ctrl Pts',(19.0251372348405,70.3660777959415,12.342161175751));
#57407=CARTESIAN_POINT('Ctrl Pts',(19.0297836350728,70.4091258464664,12.2967988011834));
#57408=CARTESIAN_POINT('Ctrl Pts',(19.0344300353051,70.4521738969912,12.2514364266159));
#57409=CARTESIAN_POINT('Ctrl Pts',(19.0390764355373,70.4976551619854,12.2085167248299));
#57410=CARTESIAN_POINT('Ctrl Pts',(19.0437228357696,70.5452506138259,12.1682910602978));
#57411=CARTESIAN_POINT('Ctrl Pts',(19.0483264546595,70.5924078345151,12.1284357702152));
#57412=CARTESIAN_POINT('Ctrl Pts',(19.0529300735493,70.641826949787,12.0910674439044));
#57413=CARTESIAN_POINT('Ctrl Pts',(19.0575336924392,70.6932153353122,12.0564515572739));
#57414=CARTESIAN_POINT('Ctrl Pts',(19.0621459665371,70.7447003355176,12.0217705897349));
#57415=CARTESIAN_POINT('Ctrl Pts',(19.066758240635,70.7981616585012,11.9898527893657));
#57416=CARTESIAN_POINT('Ctrl Pts',(19.0713705147328,70.8532702678118,11.9609256734728));
#57417=CARTESIAN_POINT('Ctrl Pts',(19.0759618820208,70.9081290773066,11.9321296802541));
#57418=CARTESIAN_POINT('Ctrl Pts',(19.0805532493088,70.9646198330223,11.906297577776));
#57419=CARTESIAN_POINT('Ctrl Pts',(19.0851446165967,71.0223895875124,11.883610116796));
#57420=CARTESIAN_POINT('Ctrl Pts',(19.0897332724557,71.0801252261114,11.8609360538814));
#57421=CARTESIAN_POINT('Ctrl Pts',(19.0943219283147,71.1391378942585,11.841403134612));
#57422=CARTESIAN_POINT('Ctrl Pts',(19.0989105841737,71.1990535842303,11.8251444705599));
#57423=CARTESIAN_POINT('Ctrl Pts',(19.1034982014551,71.2589557131298,11.8088894864275));
#57424=CARTESIAN_POINT('Ctrl Pts',(19.1080858187364,71.3197599685948,11.7959074186996));
#57425=CARTESIAN_POINT('Ctrl Pts',(19.1126734360178,71.3810780140583,11.7862812814048));
#57426=CARTESIAN_POINT('Ctrl Pts',(19.1173030055821,71.4429567933031,11.7765671161841));
#57427=CARTESIAN_POINT('Ctrl Pts',(19.1219325751463,71.5053582945914,11.770270688795));
#57428=CARTESIAN_POINT('Ctrl Pts',(19.1265621447105,71.5678760653021,11.7674240471718));
#57429=CARTESIAN_POINT('Ctrl Pts',(19.1311554848484,71.6299045933452,11.7645996823912));
#57430=CARTESIAN_POINT('Ctrl Pts',(19.1357488249864,71.6920470637278,11.7651712377844));
#57431=CARTESIAN_POINT('Ctrl Pts',(19.1403421651244,71.7539069697206,11.769117560464));
#57432=CARTESIAN_POINT('Ctrl Pts',(19.1449898494017,71.8164987447354,11.7731105723726));
#57433=CARTESIAN_POINT('Ctrl Pts',(19.149637533679,71.8788006939132,11.780558684302));
#57434=CARTESIAN_POINT('Ctrl Pts',(19.1542852179564,71.9404105001401,11.791386393357));
#57435=CARTESIAN_POINT('Ctrl Pts',(19.1589329022337,72.0020203063669,11.802214102412));
#57436=CARTESIAN_POINT('Ctrl Pts',(19.1635805865111,72.0629374665644,11.8164212268768));
#57437=CARTESIAN_POINT('Ctrl Pts',(19.1682282707884,72.1227758668436,11.8338804697225));
#57438=CARTESIAN_POINT('Ctrl Pts',(19.1728331735793,72.1820634604063,11.851179001918));
#57439=CARTESIAN_POINT('Ctrl Pts',(19.1774380763701,72.240526620572,11.8717384059336));
#57440=CARTESIAN_POINT('Ctrl Pts',(19.1820429791609,72.2977822570827,11.8954612655626));
#57441=CARTESIAN_POINT('Ctrl Pts',(19.1866550927712,72.3551275502217,11.9192212728288));
#57442=CARTESIAN_POINT('Ctrl Pts',(19.1912672063814,72.4112610313227,11.9461545520894));
#57443=CARTESIAN_POINT('Ctrl Pts',(19.1958793199917,72.465811495844,11.9761125165907));
#57444=CARTESIAN_POINT('Ctrl Pts',(19.2004719605371,72.5201316397738,12.0059439938812));
#57445=CARTESIAN_POINT('Ctrl Pts',(19.2050646010825,72.5728816480386,12.0387744470168));
#57446=CARTESIAN_POINT('Ctrl Pts',(19.2096572416279,72.6237157481518,12.0744093965212));
#57447=CARTESIAN_POINT('Ctrl Pts',(19.2142471631464,72.6745197524455,12.110023248711));
#57448=CARTESIAN_POINT('Ctrl Pts',(19.218837084665,72.7234096838212,12.1484380138804));
#57449=CARTESIAN_POINT('Ctrl Pts',(19.2234270061836,72.7700678497869,12.1894153431906));
#57450=CARTESIAN_POINT('Ctrl Pts',(19.2280158794259,72.8167153596549,12.2303833138297));
#57451=CARTESIAN_POINT('Ctrl Pts',(19.2326047526681,72.8611317355008,12.2739123520018));
#57452=CARTESIAN_POINT('Ctrl Pts',(19.2371936259103,72.9030331290775,12.3197244902865));
#57453=CARTESIAN_POINT('Ctrl Pts',(19.2418219659017,72.9452948969125,12.3659306373128));
#57454=CARTESIAN_POINT('Ctrl Pts',(19.2464503058931,72.9849978358667,12.414458981884));
#57455=CARTESIAN_POINT('Ctrl Pts',(19.2510786458845,73.0218909603376,12.4649888201075));
#57456=CARTESIAN_POINT('Ctrl Pts',(19.2556732038974,73.0585148040855,12.5151498440448));
#57457=CARTESIAN_POINT('Ctrl Pts',(19.2602677619103,73.0923694824295,12.5672827792031));
#57458=CARTESIAN_POINT('Ctrl Pts',(19.2648623199231,73.1232534334683,12.6210453105224));
#57459=CARTESIAN_POINT('Ctrl Pts',(19.2695075509038,73.1544780008302,12.6754007839727));
#57460=CARTESIAN_POINT('Ctrl Pts',(19.2741527818845,73.1826656578134,12.7314215526223));
#57461=CARTESIAN_POINT('Ctrl Pts',(19.2787980128652,73.2076572814218,12.7887313142051));
#57462=CARTESIAN_POINT('Ctrl Pts',(19.2834432438458,73.2326489050301,12.846041075788));
#57463=CARTESIAN_POINT('Ctrl Pts',(19.2880884748265,73.254444369023,12.9046393130213));
#57464=CARTESIAN_POINT('Ctrl Pts',(19.2927337058072,73.2729365026424,12.9641346343478));
#57465=CARTESIAN_POINT('Ctrl Pts',(19.297338464396,73.2912675202953,13.0231115922232));
#57466=CARTESIAN_POINT('Ctrl Pts',(19.3019432229847,73.3064248298589,13.0832024627714));
#57467=CARTESIAN_POINT('Ctrl Pts',(19.3065479815735,73.3182780745141,13.1440340763056));
#57468=CARTESIAN_POINT('Ctrl Pts',(19.311160113209,73.330150298346,13.2049630921949));
#57469=CARTESIAN_POINT('Ctrl Pts',(19.3157722448445,73.3387076718679,13.2666347506746));
#57470=CARTESIAN_POINT('Ctrl Pts',(19.32038437648,73.343869055285,13.328657494577));
#57471=CARTESIAN_POINT('Ctrl Pts',(19.3249769086041,73.3490085051144,13.3904166693586));
#57472=CARTESIAN_POINT('Ctrl Pts',(19.3295694407281,73.3507806986223,13.4525234472179));
#57473=CARTESIAN_POINT('Ctrl Pts',(19.3341619728522,73.3491568095592,13.5145821655008));
#57474=CARTESIAN_POINT('Ctrl Pts',(19.3387517995581,73.3475338771141,13.5766043255676));
#57475=CARTESIAN_POINT('Ctrl Pts',(19.343341626264,73.3425188430167,13.6385779763424));
#57476=CARTESIAN_POINT('Ctrl Pts',(19.3479314529699,73.3341349614926,13.7001066392624));
#57477=CARTESIAN_POINT('Ctrl Pts',(19.3525202450466,73.3257529698456,13.7616214325192));
#57478=CARTESIAN_POINT('Ctrl Pts',(19.3571090371233,73.3140037072191,13.8226909349592));
#57479=CARTESIAN_POINT('Ctrl Pts',(19.3616978292,73.2989621474886,13.882925005289));
#57480=CARTESIAN_POINT('Ctrl Pts',(19.3663262718355,73.2837906175528,13.9436795425534));
#57481=CARTESIAN_POINT('Ctrl Pts',(19.370954714471,73.2652697138045,14.0035836244977));
#57482=CARTESIAN_POINT('Ctrl Pts',(19.3755831571065,73.243528201611,14.0622508647656));
#57483=CARTESIAN_POINT('Ctrl Pts',(19.3801776678416,73.2219460801423,14.120488005514));
#57484=CARTESIAN_POINT('Ctrl Pts',(19.3847721785767,73.1971906715339,14.1775059306295));
#57485=CARTESIAN_POINT('Ctrl Pts',(19.3893666893118,73.1694360388153,14.2329475656899));
#57486=CARTESIAN_POINT('Ctrl Pts',(19.3940120978975,73.1413739411171,14.2890033815022));
#57487=CARTESIAN_POINT('Ctrl Pts',(19.3986575064832,73.110246008635,14.3434472988074));
#57488=CARTESIAN_POINT('Ctrl Pts',(19.4033029150688,73.076278106149,14.3959388105827));
#57489=CARTESIAN_POINT('Ctrl Pts',(19.4079483236545,73.0423102036631,14.4484303223581));
#57490=CARTESIAN_POINT('Ctrl Pts',(19.4125937322402,73.0055026928797,14.4989690376699));
#57491=CARTESIAN_POINT('Ctrl Pts',(19.4172391408259,72.9661227118731,14.5472494390542));
#57492=CARTESIAN_POINT('Ctrl Pts',(19.4219058397656,72.9265622486294,14.5957511141574));
#57493=CARTESIAN_POINT('Ctrl Pts',(19.4265725387052,72.8842352513501,14.6421822266909));
#57494=CARTESIAN_POINT('Ctrl Pts',(19.4312392376448,72.8393915776516,14.6862067867337));
#57495=CARTESIAN_POINT('Ctrl Pts',(19.4357752167816,72.7958040287347,14.7289981663452));
#57496=CARTESIAN_POINT('Ctrl Pts',(19.4403111959183,72.7498393319997,14.7695156363342));
#57497=CARTESIAN_POINT('Ctrl Pts',(19.4448471750551,72.7017686549099,14.8074827477481));
#57498=CARTESIAN_POINT('Ctrl Pts',(19.4493789194439,72.6537428561569,14.8454144134201));
#57499=CARTESIAN_POINT('Ctrl Pts',(19.4539106638327,72.6036153791354,14.8808001147534));
#57500=CARTESIAN_POINT('Ctrl Pts',(19.4584424082216,72.5516925959545,14.9134017341399));
#57501=CARTESIAN_POINT('Ctrl Pts',(19.4629716795609,72.4997981479139,14.9459855622717));
#57502=CARTESIAN_POINT('Ctrl Pts',(19.4675009509002,72.4461107770265,14.9757880429932));
#57503=CARTESIAN_POINT('Ctrl Pts',(19.4720302222396,72.3909663220636,15.0026140071801));
#57504=CARTESIAN_POINT('Ctrl Pts',(19.4765587783873,72.33583057465,15.0294357354305));
#57505=CARTESIAN_POINT('Ctrl Pts',(19.481087334535,72.2792386699189,15.0532816536205));
#57506=CARTESIAN_POINT('Ctrl Pts',(19.4856158906827,72.221549564604,15.0740032776795));
#57507=CARTESIAN_POINT('Ctrl Pts',(19.4901480107099,72.1638150591632,15.0947412092257));
#57508=CARTESIAN_POINT('Ctrl Pts',(19.4946801307371,72.1049821223312,15.1123497644502));
#57509=CARTESIAN_POINT('Ctrl Pts',(19.4992122507643,72.0454266369115,15.1267297683573));
#57510=CARTESIAN_POINT('Ctrl Pts',(19.5037465866609,71.9858420332909,15.1411168030164));
#57511=CARTESIAN_POINT('Ctrl Pts',(19.5082809225576,71.9255346914762,15.1522720511605));
#57512=CARTESIAN_POINT('Ctrl Pts',(19.5128152584543,71.8648895078128,15.1601476833579));
#57513=CARTESIAN_POINT('Ctrl Pts',(19.5173562582881,71.8041551962814,15.1680348900657));
#57514=CARTESIAN_POINT('Ctrl Pts',(19.5218972581218,71.7430825723748,15.1726328329929));
#57515=CARTESIAN_POINT('Ctrl Pts',(19.5264382579556,71.6820588908945,15.1739457037472));
#57516=CARTESIAN_POINT('Ctrl Pts',(19.5273721437628,71.6695089785131,15.1742157040574));
#57517=CARTESIAN_POINT('Ctrl Pts',(19.5283060295701,71.6569611230376,15.174346939252));
#57518=CARTESIAN_POINT('Ctrl Pts',(19.5292399153773,71.6444186650849,15.1743397174806));
#57519=CARTESIAN_POINT('Origin',(21.26284859951,71.6454,13.47));
#57520=CARTESIAN_POINT('',(13.939,70.3906268762381,13.2739275442987));
#57521=CARTESIAN_POINT('Ctrl Pts',(13.939,70.3906268762381,13.2739275442987));
#57522=CARTESIAN_POINT('Ctrl Pts',(13.939476998378,70.3913557976579,13.2692627840007));
#57523=CARTESIAN_POINT('Ctrl Pts',(13.9399552893779,70.3921107122386,13.2646022132722));
#57524=CARTESIAN_POINT('Ctrl Pts',(13.9417487187488,70.3950313405543,13.2471871084459));
#57525=CARTESIAN_POINT('Ctrl Pts',(13.9430715863859,70.3973657981373,13.2344624073896));
#57526=CARTESIAN_POINT('Ctrl Pts',(13.950929094055,70.4123016062837,13.1595193368332));
#57527=CARTESIAN_POINT('Ctrl Pts',(13.9576152221227,70.4293582572828,13.0982868263952));
#57528=CARTESIAN_POINT('Ctrl Pts',(13.9724334320229,70.477206094675,12.9658055514468));
#57529=CARTESIAN_POINT('Ctrl Pts',(13.9805257607193,70.5100971774642,12.8955603370341));
#57530=CARTESIAN_POINT('Ctrl Pts',(13.9915151991299,70.5644934030398,12.8025722603859));
#57531=CARTESIAN_POINT('Ctrl Pts',(13.9945760543604,70.5807325852423,12.7769613699378));
#57532=CARTESIAN_POINT('Ctrl Pts',(13.9999561130953,70.6111811584152,12.7325413362383));
#57533=CARTESIAN_POINT('Ctrl Pts',(14.0022870448487,70.6250256515042,12.7135013133656));
#57534=CARTESIAN_POINT('Ctrl Pts',(14.0074424274966,70.6570574216567,12.6719294521042));
#57535=CARTESIAN_POINT('Ctrl Pts',(14.0102556756569,70.6755022934806,12.6496120495138));
#57536=CARTESIAN_POINT('Ctrl Pts',(14.0192439504941,70.7373428187729,12.5797925150066));
#57537=CARTESIAN_POINT('Ctrl Pts',(14.0253074478497,70.7835894852584,12.5349484414327));
#57538=CARTESIAN_POINT('Ctrl Pts',(14.0364660638293,70.8747173866202,12.4591151619936));
#57539=CARTESIAN_POINT('Ctrl Pts',(14.0415533847315,70.9185697641717,12.4271400924489));
#57540=CARTESIAN_POINT('Ctrl Pts',(14.0489162665172,70.9835928044448,12.3858264743385));
#57541=CARTESIAN_POINT('Ctrl Pts',(14.0511133230423,71.0031832515459,12.3741083681617));
#57542=CARTESIAN_POINT('Ctrl Pts',(14.0551429109317,71.0392651346352,12.3538255569822));
#57543=CARTESIAN_POINT('Ctrl Pts',(14.0569665926813,71.0556493201144,12.3450827300574));
#57544=CARTESIAN_POINT('Ctrl Pts',(14.060168130926,71.0844074382759,12.3305378698528));
#57545=CARTESIAN_POINT('Ctrl Pts',(14.0615366605854,71.09669384579,12.3245707853382));
#57546=CARTESIAN_POINT('Ctrl Pts',(14.0646364920111,71.1245061322962,12.3116134381408));
#57547=CARTESIAN_POINT('Ctrl Pts',(14.0663729254254,71.1400801522094,12.3047353950554));
#57548=CARTESIAN_POINT('Ctrl Pts',(14.0744847022017,71.2129275096061,12.2742982535752));
#57549=CARTESIAN_POINT('Ctrl Pts',(14.0809988379883,71.2717322723212,12.2546375391324));
#57550=CARTESIAN_POINT('Ctrl Pts',(14.094817689829,71.3991004994873,12.2221737653857));
#57551=CARTESIAN_POINT('Ctrl Pts',(14.1020964281858,71.4677780606284,12.2105608141454));
#57552=CARTESIAN_POINT('Ctrl Pts',(14.1127095020675,71.5708939392687,12.2017329677886));
#57553=CARTESIAN_POINT('Ctrl Pts',(14.1161534156613,71.6048236442353,12.2001943015546));
#57554=CARTESIAN_POINT('Ctrl Pts',(14.1219322244582,71.6624682015945,12.199893744023));
#57555=CARTESIAN_POINT('Ctrl Pts',(14.1242866410912,71.6861587520721,12.2004330910749));
#57556=CARTESIAN_POINT('Ctrl Pts',(14.129233621627,71.7362907908017,12.2029793813775));
#57557=CARTESIAN_POINT('Ctrl Pts',(14.1318200410207,71.7627127605111,12.2051520480678));
#57558=CARTESIAN_POINT('Ctrl Pts',(14.1394804903234,71.8413684315128,12.2141062568121));
#57559=CARTESIAN_POINT('Ctrl Pts',(14.1444814921371,71.8932710306063,12.2233108213533));
#57560=CARTESIAN_POINT('Ctrl Pts',(14.1561100063329,72.0131234493128,12.2523501508562));
#57561=CARTESIAN_POINT('Ctrl Pts',(14.1626863094704,72.080276432895,12.2746870134236));
#57562=CARTESIAN_POINT('Ctrl Pts',(14.1718438106433,72.1687837321241,12.3125776534399));
#57563=CARTESIAN_POINT('Ctrl Pts',(14.1742991986238,72.1920346943366,12.3233756953006));
#57564=CARTESIAN_POINT('Ctrl Pts',(14.1787329944899,72.2328957851856,12.343877344785));
#57565=CARTESIAN_POINT('Ctrl Pts',(14.1806991170041,72.2506325212958,12.353309818221));
#57566=CARTESIAN_POINT('Ctrl Pts',(14.1840219139556,72.2798553649482,12.3697513011343));
#57567=CARTESIAN_POINT('Ctrl Pts',(14.1853652962686,72.2914670310747,12.3765293086549));
#57568=CARTESIAN_POINT('Ctrl Pts',(14.1885093415771,72.3181556937138,12.3926816262207));
#57569=CARTESIAN_POINT('Ctrl Pts',(14.1903170640238,72.3331463424182,12.4021891777416));
#57570=CARTESIAN_POINT('Ctrl Pts',(14.1999026649965,72.4109359804507,12.4538432557881));
#57571=CARTESIAN_POINT('Ctrl Pts',(14.2078959440174,72.4700710441466,12.5012196510443));
#57572=CARTESIAN_POINT('Ctrl Pts',(14.2231252894692,72.5746573522342,12.6015610383273));
#57573=CARTESIAN_POINT('Ctrl Pts',(14.2303453761543,72.6206749140444,12.6535762450275));
#57574=CARTESIAN_POINT('Ctrl Pts',(14.2403516348131,72.6795543263118,12.7322590956993));
#57575=CARTESIAN_POINT('Ctrl Pts',(14.2432679300762,72.6960912186791,12.7560076203112));
#57576=CARTESIAN_POINT('Ctrl Pts',(14.2484630925337,72.7243694762793,12.7997312344215));
#57577=CARTESIAN_POINT('Ctrl Pts',(14.250751702894,72.7364024727295,12.8195008625732));
#57578=CARTESIAN_POINT('Ctrl Pts',(14.2558792756512,72.7623467479083,12.8648733801021));
#57579=CARTESIAN_POINT('Ctrl Pts',(14.258705844717,72.7759311862742,12.8906488022976));
#57580=CARTESIAN_POINT('Ctrl Pts',(14.2686398840895,72.8209087482662,12.9836093670273));
#57581=CARTESIAN_POINT('Ctrl Pts',(14.2755845575386,72.8472953411638,13.0530512168687));
#57582=CARTESIAN_POINT('Ctrl Pts',(14.28715814635,72.8808496167928,13.1717043784891));
#57583=CARTESIAN_POINT('Ctrl Pts',(14.2917711345339,72.8914669442238,13.2197353572991));
#57584=CARTESIAN_POINT('Ctrl Pts',(14.2978697489013,72.9016036510804,13.2827368088897));
#57585=CARTESIAN_POINT('Ctrl Pts',(14.299278560386,72.9036823773703,13.2972558893892));
#57586=CARTESIAN_POINT('Ctrl Pts',(14.3027574150405,72.9081629635459,13.3329466215874));
#57587=CARTESIAN_POINT('Ctrl Pts',(14.3048374149227,72.9102841614885,13.3541475287875));
#57588=CARTESIAN_POINT('Ctrl Pts',(14.3082685839507,72.9128682565807,13.3887386111822));
#57589=CARTESIAN_POINT('Ctrl Pts',(14.3096033497845,72.9136542410914,13.4021005592649));
#57590=CARTESIAN_POINT('Ctrl Pts',(14.3126726160277,72.9149641551614,13.4325819493954));
#57591=CARTESIAN_POINT('Ctrl Pts',(14.3144130745964,72.9153532090717,13.4497023981396));
#57592=CARTESIAN_POINT('Ctrl Pts',(14.3248101507675,72.9156070120017,13.5511864250937));
#57593=CARTESIAN_POINT('Ctrl Pts',(14.3337446112976,72.9074116815241,13.6353516107536));
#57594=CARTESIAN_POINT('Ctrl Pts',(14.3475118905944,72.8817789309105,13.7640485312999));
#57595=CARTESIAN_POINT('Ctrl Pts',(14.3523974580923,72.8700830549755,13.8094845992648));
#57596=CARTESIAN_POINT('Ctrl Pts',(14.3609273465335,72.8449901256348,13.88855013499));
#57597=CARTESIAN_POINT('Ctrl Pts',(14.3645946079188,72.8326199289611,13.9224490717668));
#57598=CARTESIAN_POINT('Ctrl Pts',(14.3706134829778,72.8096907104379,13.9778355819002));
#57599=CARTESIAN_POINT('Ctrl Pts',(14.37298948397,72.7999391051427,13.9996314606053));
#57600=CARTESIAN_POINT('Ctrl Pts',(14.3778780368709,72.7784425396652,14.0442586614366));
#57601=CARTESIAN_POINT('Ctrl Pts',(14.3803863398905,72.7666081996359,14.0670350094066));
#57602=CARTESIAN_POINT('Ctrl Pts',(14.3877972090109,72.7293203403296,14.1337739436212));
#57603=CARTESIAN_POINT('Ctrl Pts',(14.3926311014853,72.7019105305642,14.176587453146));
#57604=CARTESIAN_POINT('Ctrl Pts',(14.4043910868289,72.6285931422274,14.2772604595145));
#57605=CARTESIAN_POINT('Ctrl Pts',(14.4112487358363,72.5800728314809,14.3329738710421));
#57606=CARTESIAN_POINT('Ctrl Pts',(14.4207331854241,72.5082585172442,14.4022300067908));
#57607=CARTESIAN_POINT('Ctrl Pts',(14.4232252252988,72.4889717219042,14.4197179130659));
#57608=CARTESIAN_POINT('Ctrl Pts',(14.4277150060949,72.4537204885764,14.4497600036826));
#57609=CARTESIAN_POINT('Ctrl Pts',(14.42969994994,72.4379662802958,14.4625473282464));
#57610=CARTESIAN_POINT('Ctrl Pts',(14.4330455211469,72.4112423228979,14.4831966366446));
#57611=CARTESIAN_POINT('Ctrl Pts',(14.4343924570854,72.4004415118038,14.4912708527554));
#57612=CARTESIAN_POINT('Ctrl Pts',(14.4375382312067,72.3751393129469,14.5095648985649));
#57613=CARTESIAN_POINT('Ctrl Pts',(14.4393440192259,72.3605499510892,14.5196547398217));
#57614=CARTESIAN_POINT('Ctrl Pts',(14.4450144134697,72.314454345255,14.550126941652));
#57615=CARTESIAN_POINT('Ctrl Pts',(14.4489252220712,72.2822548807986,14.5694194668465));
#57616=CARTESIAN_POINT('Ctrl Pts',(14.4606935507246,72.183510131956,14.6227888442584));
#57617=CARTESIAN_POINT('Ctrl Pts',(14.4685870075198,72.1147529250637,14.6524526405009));
#57618=CARTESIAN_POINT('Ctrl Pts',(14.4786179771461,72.0229660970368,14.6827755300108));
#57619=CARTESIAN_POINT('Ctrl Pts',(14.4808805828867,72.0019732119006,14.6891129198592));
#57620=CARTESIAN_POINT('Ctrl Pts',(14.4865726092809,71.9484246744597,14.7037765500435));
#57621=CARTESIAN_POINT('Ctrl Pts',(14.4899797250469,71.9156811933941,14.7113609980156));
#57622=CARTESIAN_POINT('Ctrl Pts',(14.4957087608353,71.8595260038556,14.7220403916426));
#57623=CARTESIAN_POINT('Ctrl Pts',(14.4980497315057,71.8362607082174,14.7257975405665));
#57624=CARTESIAN_POINT('Ctrl Pts',(14.5029753891358,71.78670588571,14.732391005023));
#57625=CARTESIAN_POINT('Ctrl Pts',(14.505553845302,71.7604049151202,14.735058304044));
#57626=CARTESIAN_POINT('Ctrl Pts',(14.5132157729235,71.6813994141478,14.7405858389996));
#57627=CARTESIAN_POINT('Ctrl Pts',(14.5182254565731,71.6285779875919,14.7409848913599));
#57628=CARTESIAN_POINT('Ctrl Pts',(14.529824973741,71.5057116099575,14.7342489296445));
#57629=CARTESIAN_POINT('Ctrl Pts',(14.5363650344652,71.4359891878249,14.724585298081));
#57630=CARTESIAN_POINT('Ctrl Pts',(14.5454766825696,71.3425039421267,14.703615192929));
#57631=CARTESIAN_POINT('Ctrl Pts',(14.5479232462942,71.3177564210438,14.6972741822677));
#57632=CARTESIAN_POINT('Ctrl Pts',(14.5523417557301,71.2739797623426,14.6846390401184));
#57633=CARTESIAN_POINT('Ctrl Pts',(14.554301469331,71.2548763502391,14.6786323284445));
#57634=CARTESIAN_POINT('Ctrl Pts',(14.5576174455032,71.2231984630154,14.6678424829587));
#57635=CARTESIAN_POINT('Ctrl Pts',(14.5589605428977,71.2105438049429,14.6633066625323));
#57636=CARTESIAN_POINT('Ctrl Pts',(14.5621121806618,71.181275133035,14.6522884864969));
#57637=CARTESIAN_POINT('Ctrl Pts',(14.5639279465121,71.1647227730529,14.6456560898091));
#57638=CARTESIAN_POINT('Ctrl Pts',(14.5747662048084,71.0675590798907,14.6043287054158));
#57639=CARTESIAN_POINT('Ctrl Pts',(14.5840732617276,70.9905855644922,14.5617040993972));
#57640=CARTESIAN_POINT('Ctrl Pts',(14.5985102655584,70.8775755894171,14.482843207685));
#57641=CARTESIAN_POINT('Ctrl Pts',(14.6037099770511,70.8382498734026,14.4517920767621));
#57642=CARTESIAN_POINT('Ctrl Pts',(14.6120892722629,70.777065610681,14.3973133377009));
#57643=CARTESIAN_POINT('Ctrl Pts',(14.6153132949853,70.7540788900329,14.3752412753103));
#57644=CARTESIAN_POINT('Ctrl Pts',(14.6208409854466,70.7157045775444,14.335513026184));
#57645=CARTESIAN_POINT('Ctrl Pts',(14.6231601180174,70.6999311093351,14.3182541683687));
#57646=CARTESIAN_POINT('Ctrl Pts',(14.6254746131335,70.6845474582352,14.3004591583989));
#57647=CARTESIAN_POINT('Ctrl Pts',(14.6254887977793,70.6844531914697,14.3003500779552));
#57648=CARTESIAN_POINT('Ctrl Pts',(14.625502981677,70.6843589433682,14.3002409815638));
#57649=CARTESIAN_POINT('',(13.939,71.5396994937916,12.2044063041452));
#57650=CARTESIAN_POINT('Origin',(13.939,71.6454,13.47));
#57651=CARTESIAN_POINT('Ctrl Pts',(13.939,71.5396994937916,12.2044063041452));
#57652=CARTESIAN_POINT('Ctrl Pts',(13.9400008803869,71.5497265306615,12.2035688609149));
#57653=CARTESIAN_POINT('Ctrl Pts',(13.9409965869167,71.5597636455021,12.2028505703803));
#57654=CARTESIAN_POINT('Ctrl Pts',(13.9432202349612,71.5822983601624,12.2015069062696));
#57655=CARTESIAN_POINT('Ctrl Pts',(13.9444455907093,71.5947989547552,12.2009467657048));
#57656=CARTESIAN_POINT('Ctrl Pts',(13.9506098604098,71.6580160501178,12.1990497182328));
#57657=CARTESIAN_POINT('Ctrl Pts',(13.9554545208499,71.7087770568631,12.200567738032));
#57658=CARTESIAN_POINT('Ctrl Pts',(13.9662009801399,71.8212239847597,12.2106947988583));
#57659=CARTESIAN_POINT('Ctrl Pts',(13.9720824475883,71.882636162236,12.2208074072765));
#57660=CARTESIAN_POINT('Ctrl Pts',(13.9817260512219,71.9802087958434,12.2443314486371));
#57661=CARTESIAN_POINT('Ctrl Pts',(13.9854258910078,72.0169316314597,12.2549592481323));
#57662=CARTESIAN_POINT('Ctrl Pts',(13.9917230728597,72.077750086069,12.2755754712658));
#57663=CARTESIAN_POINT('Ctrl Pts',(13.9942936017168,72.1021193940872,12.284679905866));
#57664=CARTESIAN_POINT('Ctrl Pts',(13.9998426320644,72.1536153711263,12.305742678006));
#57665=CARTESIAN_POINT('Ctrl Pts',(14.0028263940625,72.1806367620649,12.3179152654874));
#57666=CARTESIAN_POINT('Ctrl Pts',(14.0137538928216,72.2769737338574,12.3654337747251));
#57667=CARTESIAN_POINT('Ctrl Pts',(14.021863947909,72.3434172847856,12.406177269604));
#57668=CARTESIAN_POINT('Ctrl Pts',(14.036212249074,72.4523557827846,12.4875976380237));
#57669=CARTESIAN_POINT('Ctrl Pts',(14.0423891403232,72.4965542068884,12.5256330654351));
#57670=CARTESIAN_POINT('Ctrl Pts',(14.0510067894361,72.5550641423249,12.5834406702947));
#57671=CARTESIAN_POINT('Ctrl Pts',(14.053507207594,72.5716609151176,12.600795071267));
#57672=CARTESIAN_POINT('Ctrl Pts',(14.0579761760335,72.6007134927342,12.6329518170708));
#57673=CARTESIAN_POINT('Ctrl Pts',(14.0599528001752,72.6133422534691,12.6475880141916));
#57674=CARTESIAN_POINT('Ctrl Pts',(14.0631257389503,72.6332926317608,12.6718062465998));
#57675=CARTESIAN_POINT('Ctrl Pts',(14.0643351086155,72.6408199704038,12.6812134225529));
#57676=CARTESIAN_POINT('Ctrl Pts',(14.0672300116217,72.6586585761863,12.7041691858446));
#57677=CARTESIAN_POINT('Ctrl Pts',(14.0689063732077,72.6688335190671,12.7178206847786));
#57678=CARTESIAN_POINT('Ctrl Pts',(14.078504766024,72.7260097741151,12.7978423042603));
#57679=CARTESIAN_POINT('Ctrl Pts',(14.0860899837725,72.7668322900115,12.8684119441173));
#57680=CARTESIAN_POINT('Ctrl Pts',(14.0997941559012,72.8274880950476,13.0012270457913));
#57681=CARTESIAN_POINT('Ctrl Pts',(14.105872946104,72.8498137862941,13.0619974288209));
#57682=CARTESIAN_POINT('Ctrl Pts',(14.1147712391621,72.8749865554666,13.1509543112505));
#57683=CARTESIAN_POINT('Ctrl Pts',(14.1174706324221,72.8816765490075,13.1779498911137));
#57684=CARTESIAN_POINT('Ctrl Pts',(14.1223875197292,72.892126759165,13.2269568674093));
#57685=CARTESIAN_POINT('Ctrl Pts',(14.1245938427866,72.8962028054639,13.2488897171881));
#57686=CARTESIAN_POINT('Ctrl Pts',(14.1296011449077,72.9040695909924,13.2984534208844));
#57687=CARTESIAN_POINT('Ctrl Pts',(14.1324115332915,72.9075317672287,13.3261234877943));
#57688=CARTESIAN_POINT('Ctrl Pts',(14.1444616756825,72.9183506254904,13.4439556617656));
#57689=CARTESIAN_POINT('Ctrl Pts',(14.1539650803249,72.9169724666146,13.5346343529476));
#57690=CARTESIAN_POINT('Ctrl Pts',(14.1696416569437,72.8989361470008,13.6819139638364));
#57691=CARTESIAN_POINT('Ctrl Pts',(14.1757614372814,72.8879576214181,13.7389098685731));
#57692=CARTESIAN_POINT('Ctrl Pts',(14.1836996253696,72.868263149876,13.8133164786309));
#57693=CARTESIAN_POINT('Ctrl Pts',(14.185641568696,72.8629934675486,13.8315615894252));
#57694=CARTESIAN_POINT('Ctrl Pts',(14.1888797281759,72.853418461148,13.8621241638884));
#57695=CARTESIAN_POINT('Ctrl Pts',(14.190186696673,72.8493296742341,13.8745038336191));
#57696=CARTESIAN_POINT('Ctrl Pts',(14.193207982358,72.8393558708374,13.9032094224017));
#57697=CARTESIAN_POINT('Ctrl Pts',(14.1949142433418,72.8333257001578,13.9194815566024));
#57698=CARTESIAN_POINT('Ctrl Pts',(14.2044541483894,72.7974459037967,14.0105293213565));
#57699=CARTESIAN_POINT('Ctrl Pts',(14.2119715930869,72.7608672484061,14.0824698321661));
#57700=CARTESIAN_POINT('Ctrl Pts',(14.2258300667714,72.6817886474242,14.207084965997));
#57701=CARTESIAN_POINT('Ctrl Pts',(14.2321347133448,72.6414408122528,14.2607569624196));
#57702=CARTESIAN_POINT('Ctrl Pts',(14.2413760835527,72.5778898376136,14.3326701905974));
#57703=CARTESIAN_POINT('Ctrl Pts',(14.2441863162849,72.5579966393668,14.3536878558472));
#57704=CARTESIAN_POINT('Ctrl Pts',(14.2491069800615,72.5223217491232,14.3888891395435));
#57705=CARTESIAN_POINT('Ctrl Pts',(14.2512026364407,72.5068696091555,14.4033911213357));
#57706=CARTESIAN_POINT('Ctrl Pts',(14.2561982192381,72.4694811707387,14.436761107742));
#57707=CARTESIAN_POINT('Ctrl Pts',(14.2591108893377,72.4472497530191,14.4552783632821));
#57708=CARTESIAN_POINT('Ctrl Pts',(14.2685636822047,72.3738376899391,14.5122948091277));
#57709=CARTESIAN_POINT('Ctrl Pts',(14.2752077046584,72.320378634547,14.5476831949409));
#57710=CARTESIAN_POINT('Ctrl Pts',(14.2876182528634,72.216925635022,14.6054408468038));
#57711=CARTESIAN_POINT('Ctrl Pts',(14.2933541963639,72.1677019373563,14.6289082780757));
#57712=CARTESIAN_POINT('Ctrl Pts',(14.3014093983787,72.0958859899463,14.6576386417937));
#57713=CARTESIAN_POINT('Ctrl Pts',(14.3037785183152,72.0744220921676,14.6655598591436));
#57714=CARTESIAN_POINT('Ctrl Pts',(14.3080342100415,72.0351404441845,14.6788623640315));
#57715=CARTESIAN_POINT('Ctrl Pts',(14.3099276650795,72.0173959500412,14.6844401891772));
#57716=CARTESIAN_POINT('Ctrl Pts',(14.3131770104863,71.9864162551457,14.6934355267851));
#57717=CARTESIAN_POINT('Ctrl Pts',(14.3145411934125,71.9732384615798,14.6970324255393));
#57718=CARTESIAN_POINT('Ctrl Pts',(14.3175782115732,71.9435299424688,14.7046285430537));
#57719=CARTESIAN_POINT('Ctrl Pts',(14.3192451068933,71.926972523221,14.7085096355793));
#57720=CARTESIAN_POINT('Ctrl Pts',(14.3271482062558,71.8474837798943,14.7254652170998));
#57721=CARTESIAN_POINT('Ctrl Pts',(14.3331979919213,71.7836893620083,14.7340844309566));
#57722=CARTESIAN_POINT('Ctrl Pts',(14.3444979591608,71.6636846004003,14.7410989367819));
#57723=CARTESIAN_POINT('Ctrl Pts',(14.3497369986247,71.6077103466657,14.740671386377));
#57724=CARTESIAN_POINT('Ctrl Pts',(14.3568506587739,71.5331155157879,14.7351675053485));
#57725=CARTESIAN_POINT('Ctrl Pts',(14.3586543682143,71.5143165029657,14.7333580941724));
#57726=CARTESIAN_POINT('Ctrl Pts',(14.3634092330661,71.4651675094903,14.7275187235973));
#57727=CARTESIAN_POINT('Ctrl Pts',(14.3663757765885,71.4349129264901,14.7228096161121));
#57728=CARTESIAN_POINT('Ctrl Pts',(14.3716716545472,71.3818618108209,14.7125764566566));
#57729=CARTESIAN_POINT('Ctrl Pts',(14.373985987621,71.3589920675168,14.7075051295526));
#57730=CARTESIAN_POINT('Ctrl Pts',(14.3791448312527,71.3087960301523,14.6949083860453));
#57731=CARTESIAN_POINT('Ctrl Pts',(14.3819972942167,71.2815560669788,14.6870949260919));
#57732=CARTESIAN_POINT('Ctrl Pts',(14.3938257027312,71.1708725190663,14.6512991507506));
#57733=CARTESIAN_POINT('Ctrl Pts',(14.4030355071996,71.0902009327151,14.6155965882369));
#57734=CARTESIAN_POINT('Ctrl Pts',(14.4167055282893,70.9774699565543,14.5509861125811));
#57735=CARTESIAN_POINT('Ctrl Pts',(14.4211189102001,70.9421110317391,14.5283225226393));
#57736=CARTESIAN_POINT('Ctrl Pts',(14.4283525036214,70.8854675647898,14.4879216300232));
#57737=CARTESIAN_POINT('Ctrl Pts',(14.431198690521,70.8635233793001,14.4711648481963));
#57738=CARTESIAN_POINT('Ctrl Pts',(14.4354711688423,70.8309739097779,14.4445860537232));
#57739=CARTESIAN_POINT('Ctrl Pts',(14.4369258536208,70.8199623305819,14.4352774579565));
#57740=CARTESIAN_POINT('Ctrl Pts',(14.4398774101789,70.7977382021212,14.4158318144448));
#57741=CARTESIAN_POINT('Ctrl Pts',(14.4413729012027,70.78654333058,14.405678174897));
#57742=CARTESIAN_POINT('Ctrl Pts',(14.4460738804801,70.7516443729712,14.3728708181603));
#57743=CARTESIAN_POINT('Ctrl Pts',(14.4492324740128,70.7286325727925,14.3494958189013));
#57744=CARTESIAN_POINT('Ctrl Pts',(14.4534224657446,70.6990405148412,14.3170112305496));
#57745=CARTESIAN_POINT('Ctrl Pts',(14.4544813502127,70.6916433897297,14.3086730545474));
#57746=CARTESIAN_POINT('Ctrl Pts',(14.4555370852546,70.6843589127286,14.3002409460971));
#57747=CARTESIAN_POINT('Origin',(13.939,71.6454,13.47));
#57748=CARTESIAN_POINT('',(13.939,73.264582312878,14.0019995049462));
#57749=CARTESIAN_POINT('',(13.939,71.6454,15.17434));
#57750=CARTESIAN_POINT('Origin',(13.939,71.6454,13.47));
#57751=CARTESIAN_POINT('Ctrl Pts',(13.939,73.264582312878,14.0019995049462));
#57752=CARTESIAN_POINT('Ctrl Pts',(13.939,73.2646272474247,14.001763711796));
#57753=CARTESIAN_POINT('Ctrl Pts',(13.939,73.2646721268292,14.0015279088845));
#57754=CARTESIAN_POINT('Ctrl Pts',(13.939,73.2647169510781,14.0012920962225));
#57755=CARTESIAN_POINT('Ctrl Pts',(13.939,73.2768225083756,13.9376068419289));
#57756=CARTESIAN_POINT('Ctrl Pts',(13.939,73.2849096414707,13.8732097073678));
#57757=CARTESIAN_POINT('Ctrl Pts',(13.939,73.2890848141171,13.8084486550991));
#57758=CARTESIAN_POINT('Ctrl Pts',(13.939,73.2919053719335,13.7646990170269));
#57759=CARTESIAN_POINT('Ctrl Pts',(13.939,73.2929394569106,13.7207833483898));
#57760=CARTESIAN_POINT('Ctrl Pts',(13.939,73.2922072227446,13.6768133865707));
#57761=CARTESIAN_POINT('Ctrl Pts',(13.939,73.2919437584807,13.6609926093361));
#57762=CARTESIAN_POINT('Ctrl Pts',(13.939,73.2914514204789,13.6451624680941));
#57763=CARTESIAN_POINT('Ctrl Pts',(13.939,73.2907312164348,13.6293359597415));
#57764=CARTESIAN_POINT('Ctrl Pts',(13.939,73.2878331555803,13.5656509739393));
#57765=CARTESIAN_POINT('Ctrl Pts',(13.939,73.2812563477203,13.5021534078011));
#57766=CARTESIAN_POINT('Ctrl Pts',(13.939,73.2710875752043,13.4391836479786));
#57767=CARTESIAN_POINT('Ctrl Pts',(13.939,73.2642723599941,13.3969806717347));
#57768=CARTESIAN_POINT('Ctrl Pts',(13.939,73.2558426578812,13.3550150867301));
#57769=CARTESIAN_POINT('Ctrl Pts',(13.939,73.2458136086189,13.3133965701029));
#57770=CARTESIAN_POINT('Ctrl Pts',(13.939,73.2421720474416,13.298284831149));
#57771=CARTESIAN_POINT('Ctrl Pts',(13.939,73.2383195470336,13.2832189194597));
#57772=CARTESIAN_POINT('Ctrl Pts',(13.939,73.2342565785196,13.2682043412823));
#57773=CARTESIAN_POINT('Ctrl Pts',(13.939,73.2311876368406,13.2568631594338));
#57774=CARTESIAN_POINT('Ctrl Pts',(13.939,73.2279985968259,13.2455515851929));
#57775=CARTESIAN_POINT('Ctrl Pts',(13.939,73.2246937617167,13.2342850968275));
#57776=CARTESIAN_POINT('Ctrl Pts',(13.939,73.2073554594815,13.1751772218635));
#57777=CARTESIAN_POINT('Ctrl Pts',(13.939,73.1868086540449,13.1172137677125));
#57778=CARTESIAN_POINT('Ctrl Pts',(13.939,73.1631328660133,13.0607036923316));
#57779=CARTESIAN_POINT('Ctrl Pts',(13.939,73.1400618824897,13.0056371823474));
#57780=CARTESIAN_POINT('Ctrl Pts',(13.939,73.1140190789678,12.9519500056349));
#57781=CARTESIAN_POINT('Ctrl Pts',(13.939,73.0850424472804,12.8999613856181));
#57782=CARTESIAN_POINT('Ctrl Pts',(13.939,73.0669043859958,12.867418860105));
#57783=CARTESIAN_POINT('Ctrl Pts',(13.939,73.0476161236673,12.8355425667648));
#57784=CARTESIAN_POINT('Ctrl Pts',(13.939,73.027181258192,12.804419590393));
#57785=CARTESIAN_POINT('Ctrl Pts',(13.939,73.0087993152631,12.776423282997));
#57786=CARTESIAN_POINT('Ctrl Pts',(13.939,72.989489497977,12.7490365884417));
#57787=CARTESIAN_POINT('Ctrl Pts',(13.939,72.9692519295121,12.7223284864005));
#57788=CARTESIAN_POINT('Ctrl Pts',(13.939,72.9625477153461,12.7134807418526));
#57789=CARTESIAN_POINT('Ctrl Pts',(13.939,72.9557464912283,12.7047139507404));
#57790=CARTESIAN_POINT('Ctrl Pts',(13.939,72.9488522064473,12.6960346929813));
#57791=CARTESIAN_POINT('Ctrl Pts',(13.939,72.9134703517828,12.6514922572707));
#57792=CARTESIAN_POINT('Ctrl Pts',(13.939,72.8756104083326,12.6092130013336));
#57793=CARTESIAN_POINT('Ctrl Pts',(13.939,72.8353120313341,12.5694808059632));
#57794=CARTESIAN_POINT('Ctrl Pts',(13.939,72.827878568635,12.5621517814655));
#57795=CARTESIAN_POINT('Ctrl Pts',(13.939,72.8203620597672,12.5549095428167));
#57796=CARTESIAN_POINT('Ctrl Pts',(13.939,72.8127626542197,12.547756041847));
#57797=CARTESIAN_POINT('Ctrl Pts',(13.939,72.7704332554513,12.5079103732296));
#57798=CARTESIAN_POINT('Ctrl Pts',(13.939,72.7255327909401,12.4708137762423));
#57799=CARTESIAN_POINT('Ctrl Pts',(13.939,72.6783705863321,12.4365867468974));
#57800=CARTESIAN_POINT('Ctrl Pts',(13.939,72.6372143500213,12.4067184292553));
#57801=CARTESIAN_POINT('Ctrl Pts',(13.939,72.5943349481246,12.3790360565908));
#57802=CARTESIAN_POINT('Ctrl Pts',(13.939,72.5499374525507,12.3536521712294));
#57803=CARTESIAN_POINT('Ctrl Pts',(13.939,72.5412850963492,12.3487052611597));
#57804=CARTESIAN_POINT('Ctrl Pts',(13.939,72.5325771207947,12.3438469827975));
#57805=CARTESIAN_POINT('Ctrl Pts',(13.939,72.5238247169746,12.3390831285424));
#57806=CARTESIAN_POINT('Ctrl Pts',(13.939,72.4744815389255,12.3122260829191));
#57807=CARTESIAN_POINT('Ctrl Pts',(13.939,72.4236416082651,12.2883166978516));
#57808=CARTESIAN_POINT('Ctrl Pts',(13.939,72.3715973046636,12.2674409134596));
#57809=CARTESIAN_POINT('Ctrl Pts',(13.939,72.3205033306167,12.2469463211196));
#57810=CARTESIAN_POINT('Ctrl Pts',(13.939,72.2682474285401,12.2293756434533));
#57811=CARTESIAN_POINT('Ctrl Pts',(13.939,72.2151072058468,12.2148592018594));
#57812=CARTESIAN_POINT('Ctrl Pts',(13.939,72.1624130772386,12.2004646208525));
#57813=CARTESIAN_POINT('Ctrl Pts',(13.939,72.1088484048521,12.1890732539501));
#57814=CARTESIAN_POINT('Ctrl Pts',(13.939,72.054700628375,12.1808599598466));
#57815=CARTESIAN_POINT('Ctrl Pts',(13.939,72.0424424009615,12.1790005958342));
#57816=CARTESIAN_POINT('Ctrl Pts',(13.939,72.0301516559131,12.1773041064647));
#57817=CARTESIAN_POINT('Ctrl Pts',(13.939,72.0178560360339,12.1757754217218));
#57818=CARTESIAN_POINT('Ctrl Pts',(13.939,71.964717139225,12.1691687909376));
#57819=CARTESIAN_POINT('Ctrl Pts',(13.939,71.9113917654875,12.1656763501367));
#57820=CARTESIAN_POINT('Ctrl Pts',(13.939,71.8581433977227,12.1654083282307));
#57821=CARTESIAN_POINT('Ctrl Pts',(13.939,71.8048950299579,12.1651403063247));
#57822=CARTESIAN_POINT('Ctrl Pts',(13.939,71.7517225988644,12.1680967638079));
#57823=CARTESIAN_POINT('Ctrl Pts',(13.939,71.6989120037461,12.1744397176796));
#57824=CARTESIAN_POINT('Ctrl Pts',(13.939,71.649362220586,12.1803910232506));
#57825=CARTESIAN_POINT('Ctrl Pts',(13.939,71.6001304926346,12.1893240715038));
#57826=CARTESIAN_POINT('Ctrl Pts',(13.939,71.5514831449858,12.2014131145448));
#57827=CARTESIAN_POINT('Ctrl Pts',(13.939,71.5475513741415,12.2023901739172));
#57828=CARTESIAN_POINT('Ctrl Pts',(13.939,71.5436234399984,12.2033878695024));
#57829=CARTESIAN_POINT('Ctrl Pts',(13.939,71.5396994937916,12.2044063041452));
#57830=CARTESIAN_POINT('',(13.9383731125779,70.3876696333693,13.2861333242433));
#57831=CARTESIAN_POINT('Ctrl Pts',(13.939,70.3906268762381,13.2739275442987));
#57832=CARTESIAN_POINT('Ctrl Pts',(13.938791037526,70.3899833170529,13.2780460257359));
#57833=CARTESIAN_POINT('Ctrl Pts',(13.9385820750519,70.3893600348717,13.282167675683));
#57834=CARTESIAN_POINT('Ctrl Pts',(13.9383731125779,70.3887570599105,13.2862922943282));
#57835=CARTESIAN_POINT('Ctrl Pts',(13.939,70.3865728200509,13.2860385524592));
#57836=CARTESIAN_POINT('Ctrl Pts',(13.939,70.3847141156884,13.2916947947257));
#57837=CARTESIAN_POINT('Ctrl Pts',(13.939,70.3828997146351,13.2973636743118));
#57838=CARTESIAN_POINT('Ctrl Pts',(13.939,70.3811298896707,13.3030447680062));
#57839=CARTESIAN_POINT('Ctrl Pts',(13.939,70.3662097964106,13.3509378927181));
#57840=CARTESIAN_POINT('Ctrl Pts',(13.939,70.3544544690838,13.3996961009194));
#57841=CARTESIAN_POINT('Ctrl Pts',(13.939,70.3457112817141,13.449041204321));
#57842=CARTESIAN_POINT('Ctrl Pts',(13.939,70.3408256769823,13.4766147493539));
#57843=CARTESIAN_POINT('Ctrl Pts',(13.939,70.3368812979427,13.5043722152326));
#57844=CARTESIAN_POINT('Ctrl Pts',(13.939,70.333856942926,13.5322692423113));
#57845=CARTESIAN_POINT('Ctrl Pts',(13.939,70.3322585732646,13.5470128029982));
#57846=CARTESIAN_POINT('Ctrl Pts',(13.939,70.3309172432249,13.5617953885959));
#57847=CARTESIAN_POINT('Ctrl Pts',(13.939,70.3298302731433,13.5766107087285));
#57848=CARTESIAN_POINT('Ctrl Pts',(13.939,70.3288771678923,13.5896014613277));
#57849=CARTESIAN_POINT('Ctrl Pts',(13.939,70.3281203298447,13.6026083266247));
#57850=CARTESIAN_POINT('Ctrl Pts',(13.939,70.3275573847283,13.6156237951177));
#57851=CARTESIAN_POINT('Ctrl Pts',(13.939,70.3252516912663,13.6689321545626));
#57852=CARTESIAN_POINT('Ctrl Pts',(13.939,70.3261938157966,13.7223984126338));
#57853=CARTESIAN_POINT('Ctrl Pts',(13.939,70.3302344908111,13.7757255847281));
#57854=CARTESIAN_POINT('Ctrl Pts',(13.939,70.3325695397501,13.8065426032142));
#57855=CARTESIAN_POINT('Ctrl Pts',(13.939,70.3359402122064,13.8373137478591));
#57856=CARTESIAN_POINT('Ctrl Pts',(13.939,70.3403248092368,13.8679850719421));
#57857=CARTESIAN_POINT('Ctrl Pts',(13.939,70.3424557006452,13.8828911763162));
#57858=CARTESIAN_POINT('Ctrl Pts',(13.939,70.3448269839794,13.897777514839));
#57859=CARTESIAN_POINT('Ctrl Pts',(13.939,70.3474313892361,13.9126111345666));
#57860=CARTESIAN_POINT('Ctrl Pts',(13.939,70.3570334545961,13.9673005442813));
#57861=CARTESIAN_POINT('Ctrl Pts',(13.939,70.3698086876566,14.0213395656395));
#57862=CARTESIAN_POINT('Ctrl Pts',(13.939,70.3855940774027,14.0744222844327));
#57863=CARTESIAN_POINT('Ctrl Pts',(13.939,70.4017665627473,14.1288067187448));
#57864=CARTESIAN_POINT('Ctrl Pts',(13.939,70.42109845679,14.1821884755046));
#57865=CARTESIAN_POINT('Ctrl Pts',(13.939,70.4434662797082,14.2342555993515));
#57866=CARTESIAN_POINT('Ctrl Pts',(13.939,70.4574328955107,14.2667666540649));
#57867=CARTESIAN_POINT('Ctrl Pts',(13.939,70.4725842111556,14.2987654365004));
#57868=CARTESIAN_POINT('Ctrl Pts',(13.939,70.4889004546343,14.3301761874657));
#57869=CARTESIAN_POINT('Ctrl Pts',(13.939,70.4970056681847,14.3457797082568));
#57870=CARTESIAN_POINT('Ctrl Pts',(13.939,70.5053984703826,14.3612381077738));
#57871=CARTESIAN_POINT('Ctrl Pts',(13.939,70.5140771559869,14.3765419403879));
#57872=CARTESIAN_POINT('Ctrl Pts',(13.939,70.519061925058,14.385331989361));
#57873=CARTESIAN_POINT('Ctrl Pts',(13.939,70.5241422137917,14.3940730469123));
#57874=CARTESIAN_POINT('Ctrl Pts',(13.939,70.5293138507803,14.4027567437645));
#57875=CARTESIAN_POINT('Ctrl Pts',(13.939,70.5595344952892,14.4535002348824));
#57876=CARTESIAN_POINT('Ctrl Pts',(13.939,70.5927791867216,14.5021351404274));
#57877=CARTESIAN_POINT('Ctrl Pts',(13.939,70.6288939100955,14.5483354328417));
#57878=CARTESIAN_POINT('Ctrl Pts',(13.939,70.6410781382509,14.5639222863749));
#57879=CARTESIAN_POINT('Ctrl Pts',(13.939,70.6535894795825,14.5792320742092));
#57880=CARTESIAN_POINT('Ctrl Pts',(13.939,70.6664233505904,14.5942522878267));
#57881=CARTESIAN_POINT('Ctrl Pts',(13.939,70.7032143579353,14.6373109089695));
#57882=CARTESIAN_POINT('Ctrl Pts',(13.939,70.7426523252183,14.6779915147634));
#57883=CARTESIAN_POINT('Ctrl Pts',(13.939,70.7844391127293,14.7162612897989));
#57884=CARTESIAN_POINT('Ctrl Pts',(13.939,70.8065815217405,14.7365400683813));
#57885=CARTESIAN_POINT('Ctrl Pts',(13.939,70.8293842670646,14.7561415704296));
#57886=CARTESIAN_POINT('Ctrl Pts',(13.939,70.8528080216974,14.7750580958749));
#57887=CARTESIAN_POINT('Ctrl Pts',(13.939,70.8661058911497,14.7857971720737));
#57888=CARTESIAN_POINT('Ctrl Pts',(13.939,70.8796039668997,14.7963154462813));
#57889=CARTESIAN_POINT('Ctrl Pts',(13.939,70.8932954851338,14.8066111791164));
#57890=CARTESIAN_POINT('Ctrl Pts',(13.939,70.9051906076058,14.8155560602405));
#57891=CARTESIAN_POINT('Ctrl Pts',(13.939,70.9172363806852,14.8243360470071));
#57892=CARTESIAN_POINT('Ctrl Pts',(13.939,70.9294017561649,14.8329314829181));
#57893=CARTESIAN_POINT('Ctrl Pts',(13.939,70.9781285705973,14.8673593730641));
#57894=CARTESIAN_POINT('Ctrl Pts',(13.939,71.0288346774935,14.898879998854));
#57895=CARTESIAN_POINT('Ctrl Pts',(13.939,71.0811731191553,14.9274712503634));
#57896=CARTESIAN_POINT('Ctrl Pts',(13.939,71.1349695972786,14.9568589926711));
#57897=CARTESIAN_POINT('Ctrl Pts',(13.939,71.1904912389686,14.9831525457031));
#57898=CARTESIAN_POINT('Ctrl Pts',(13.939,71.2474094103809,15.0062985260324));
#57899=CARTESIAN_POINT('Ctrl Pts',(13.939,71.3043094664642,15.0294371396975));
#57900=CARTESIAN_POINT('Ctrl Pts',(13.939,71.362606078278,15.0494307474303));
#57901=CARTESIAN_POINT('Ctrl Pts',(13.939,71.4220064371697,15.0661879181898));
#57902=CARTESIAN_POINT('Ctrl Pts',(13.939,71.4337420948756,15.0694986123307));
#57903=CARTESIAN_POINT('Ctrl Pts',(13.939,71.4455209214723,15.0726828426826));
#57904=CARTESIAN_POINT('Ctrl Pts',(13.939,71.4573407739189,15.0757396982053));
#57905=CARTESIAN_POINT('Ctrl Pts',(13.939,71.4688100974538,15.0787058997842));
#57906=CARTESIAN_POINT('Ctrl Pts',(13.939,71.480309797296,15.0815499878697));
#57907=CARTESIAN_POINT('Ctrl Pts',(13.939,71.4918315190228,15.0842702463551));
#57908=CARTESIAN_POINT('Ctrl Pts',(13.939,71.5542915564786,15.0990169526999));
#57909=CARTESIAN_POINT('Ctrl Pts',(13.939,71.6174513748119,15.1101419723292));
#57910=CARTESIAN_POINT('Ctrl Pts',(13.939,71.6809583817784,15.1175988679018));
#57911=CARTESIAN_POINT('Ctrl Pts',(13.939,71.7446039751982,15.1250720360836));
#57912=CARTESIAN_POINT('Ctrl Pts',(13.939,71.8085992672762,15.1288616146105));
#57913=CARTESIAN_POINT('Ctrl Pts',(13.939,71.8726203928869,15.1288794736354));
#57914=CARTESIAN_POINT('Ctrl Pts',(13.939,71.936077962909,15.1288971754536));
#57915=CARTESIAN_POINT('Ctrl Pts',(13.939,71.9995619530363,15.1252097402554));
#57916=CARTESIAN_POINT('Ctrl Pts',(13.939,72.0627722128131,15.1176831531631));
#57917=CARTESIAN_POINT('Ctrl Pts',(13.939,72.0746764434834,15.1162656897763));
#57918=CARTESIAN_POINT('Ctrl Pts',(13.939,72.0865709835791,15.1147119119096));
#57919=CARTESIAN_POINT('Ctrl Pts',(13.939,72.0984538423728,15.1130207093982));
#57920=CARTESIAN_POINT('Origin',(13.939,71.6454,13.47));
#57921=CARTESIAN_POINT('Ctrl Pts',(20.0410482168728,70.5240746963012,14.0615191344664));
#57922=CARTESIAN_POINT('Ctrl Pts',(19.9995464051999,70.7184011759149,14.4298980863427));
#57923=CARTESIAN_POINT('Ctrl Pts',(19.9165427818541,71.4952528988591,14.9541982817824));
#57924=CARTESIAN_POINT('Ctrl Pts',(19.7920373468353,72.80183948703,14.4146995872025));
#57925=CARTESIAN_POINT('Ctrl Pts',(19.6675319118165,73.0706439666114,13.0280142869573));
#57926=CARTESIAN_POINT('Ctrl Pts',(19.5430264767976,72.0647777602789,12.0377159341111));
#57927=CARTESIAN_POINT('Ctrl Pts',(19.418521041779,70.6828821695164,12.3292652371603));
#57928=CARTESIAN_POINT('Ctrl Pts',(19.2940156067602,70.1629367914403,13.6421861630661));
#57929=CARTESIAN_POINT('Ctrl Pts',(19.1695101717414,70.969967751209,14.8008798288961));
#57930=CARTESIAN_POINT('Ctrl Pts',(19.0450047367226,72.3817240944507,14.7681945331265));
#57931=CARTESIAN_POINT('Ctrl Pts',(18.9204993017039,73.1342796795863,13.5733292463045));
#57932=CARTESIAN_POINT('Ctrl Pts',(18.7959938666851,72.5539885107806,12.2859722028927));
#57933=CARTESIAN_POINT('Ctrl Pts',(18.6714884316663,71.1603094218454,12.0585666918175));
#57934=CARTESIAN_POINT('Ctrl Pts',(18.5469829966475,70.2008934572389,13.094696140498));
#57935=CARTESIAN_POINT('Ctrl Pts',(18.4224775616288,70.5346156866825,14.4668010991402));
#57936=CARTESIAN_POINT('Ctrl Pts',(18.29797212661,71.8627267685966,14.9465579232634));
#57937=CARTESIAN_POINT('Ctrl Pts',(18.1734666915911,72.996283760724,14.1044815120698));
#57938=CARTESIAN_POINT('Ctrl Pts',(18.0489612565725,72.9205130945634,12.6944095214458));
#57939=CARTESIAN_POINT('Ctrl Pts',(17.9244558215537,71.7032452653328,11.9786556757229));
#57940=CARTESIAN_POINT('Ctrl Pts',(17.7999503865349,70.4341936928937,12.5979717898819));
#57941=CARTESIAN_POINT('Ctrl Pts',(17.6754449515162,70.249428994792,13.9979383523494));
#57942=CARTESIAN_POINT('Ctrl Pts',(17.5509395164974,71.3143548597143,14.9252879647334));
#57943=CARTESIAN_POINT('Ctrl Pts',(17.4264340814786,72.6756364317002,14.5498457460373));
#57944=CARTESIAN_POINT('Ctrl Pts',(17.3019286464598,73.114637581328,13.207712230478));
#57945=CARTESIAN_POINT('Ctrl Pts',(17.177423211441,72.2383590324684,12.1003819768889));
#57946=CARTESIAN_POINT('Ctrl Pts',(17.0529177764223,70.8312562074884,12.2191507571731));
#57947=CARTESIAN_POINT('Ctrl Pts',(16.9284123414035,70.1529849983377,13.4576952863166));
#57948=CARTESIAN_POINT('Ctrl Pts',(16.8039069063848,70.8107421999714,14.7072551476021));
#57949=CARTESIAN_POINT('Ctrl Pts',(16.6794014713659,72.2156954121601,14.8492088628255));
#57950=CARTESIAN_POINT('Ctrl Pts',(16.5548960363472,73.1101130998516,13.756477705172));
#57951=CARTESIAN_POINT('Ctrl Pts',(16.4303906013284,72.6933014657471,12.4072881560414));
#57952=CARTESIAN_POINT('Ctrl Pts',(16.3058851663097,71.3383954419374,12.0094514206671));
#57953=CARTESIAN_POINT('Ctrl Pts',(16.1813797312908,70.2583237181736,12.9191158869499));
#57954=CARTESIAN_POINT('Ctrl Pts',(16.0568742962721,70.4199798494693,14.3219386262802));
#57955=CARTESIAN_POINT('Ctrl Pts',(15.9323688612533,71.6786473483666,14.9620953750271));
#57956=CARTESIAN_POINT('Ctrl Pts',(15.8078634262346,72.9075512918229,14.2665097869431));
#57957=CARTESIAN_POINT('Ctrl Pts',(15.6833579912158,73.006561990935,12.857878884914));
#57958=CARTESIAN_POINT('Ctrl Pts',(15.558852556197,71.8870431132129,11.9972261450596));
#57959=CARTESIAN_POINT('Ctrl Pts',(15.4343471211782,70.5512033220584,12.4550193257908));
#57960=CARTESIAN_POINT('Ctrl Pts',(15.3098416861595,70.1948999249935,13.8214347519347));
#57961=CARTESIAN_POINT('Ctrl Pts',(15.1853362511407,71.1371063372083,14.8732435492854));
#57962=CARTESIAN_POINT('Ctrl Pts',(15.060830816122,72.5343350401052,14.6688469993707));
#57963=CARTESIAN_POINT('Ctrl Pts',(14.9363253811032,73.1357954317769,13.3912365894174));
#57964=CARTESIAN_POINT('Ctrl Pts',(14.8118199460844,72.4029999040765,12.1841181131174));
#57965=CARTESIAN_POINT('Ctrl Pts',(14.6873145110655,70.992063963973,12.1281739071278));
#57966=CARTESIAN_POINT('Ctrl Pts',(14.5628090760468,70.1658546328295,13.2733737564971));
#57967=CARTESIAN_POINT('Ctrl Pts',(14.4383036410281,70.6644547802432,14.5947496730614));
#57968=CARTESIAN_POINT('Ctrl Pts',(14.3137982060093,72.0405920319688,14.9089214685884));
#57969=CARTESIAN_POINT('Ctrl Pts',(14.1892927709905,73.064211602503,13.9355998645035));
#57970=CARTESIAN_POINT('Ctrl Pts',(14.0647765398672,72.8150660685469,12.5440178827245));
#57971=CARTESIAN_POINT('Ctrl Pts',(13.9817621204168,71.954707782371,12.1718579782255));
#57972=CARTESIAN_POINT('Ctrl Pts',(13.9402495126393,71.5395603852097,12.2066460152216));
#57973=CARTESIAN_POINT('Ctrl Pts',(19.9566236618974,70.3947393463692,14.1297458426261));
#57974=CARTESIAN_POINT('Ctrl Pts',(19.9151218502245,70.6114797349164,14.5406141778164));
#57975=CARTESIAN_POINT('Ctrl Pts',(19.8321182268787,71.4779347059999,15.1253879477157));
#57976=CARTESIAN_POINT('Ctrl Pts',(19.7076127918599,72.935224959771,14.5236626608872));
#57977=CARTESIAN_POINT('Ctrl Pts',(19.5831073568411,73.2350337530116,12.9770349889135));
#57978=CARTESIAN_POINT('Ctrl Pts',(19.4586019218224,72.1131494229894,11.8725141320536));
#57979=CARTESIAN_POINT('Ctrl Pts',(19.3340964868036,70.5718639128065,12.1976911709685));
#57980=CARTESIAN_POINT('Ctrl Pts',(19.2095910517848,69.9919472514666,13.6620463745321));
#57981=CARTESIAN_POINT('Ctrl Pts',(19.085085616766,70.8920623780184,14.954385513482));
#57982=CARTESIAN_POINT('Ctrl Pts',(18.9605801817473,72.4666528248602,14.9179302464542));
#57983=CARTESIAN_POINT('Ctrl Pts',(18.8360747467285,73.3060093049954,13.5852473972504));
#57984=CARTESIAN_POINT('Ctrl Pts',(18.7115693117097,72.6587864785055,12.1494046529026));
#57985=CARTESIAN_POINT('Ctrl Pts',(18.587063876691,71.1043583437171,11.8957698475678));
#57986=CARTESIAN_POINT('Ctrl Pts',(18.4625584416722,70.0342818962844,13.0514080279053));
#57987=CARTESIAN_POINT('Ctrl Pts',(18.3380530066534,70.4064961504623,14.5817736397085));
#57988=CARTESIAN_POINT('Ctrl Pts',(18.2135475716346,71.8877935655138,15.1168663387342));
#57989=CARTESIAN_POINT('Ctrl Pts',(18.0890421366159,73.152096728945,14.1776635655901));
#57990=CARTESIAN_POINT('Ctrl Pts',(17.9645367015971,73.0675865599923,12.6049517471346));
#57991=CARTESIAN_POINT('Ctrl Pts',(17.8400312665783,71.7099172253868,11.8066417744819));
#57992=CARTESIAN_POINT('Ctrl Pts',(17.7155258315596,70.2944913326127,12.4973907423177));
#57993=CARTESIAN_POINT('Ctrl Pts',(17.5910203965408,70.0884155958631,14.0588315573082));
#57994=CARTESIAN_POINT('Ctrl Pts',(17.466514961522,71.2761716144768,15.0931430711416));
#57995=CARTESIAN_POINT('Ctrl Pts',(17.3420095265032,72.7944654539002,14.674396781295));
#57996=CARTESIAN_POINT('Ctrl Pts',(17.2175040914845,73.284101657531,13.1774595639752));
#57997=CARTESIAN_POINT('Ctrl Pts',(17.0929986564657,72.3067518206332,11.9424081706189));
#57998=CARTESIAN_POINT('Ctrl Pts',(16.9684932214469,70.7373516358605,12.0748759209596));
#57999=CARTESIAN_POINT('Ctrl Pts',(16.8439877864282,69.9808476035539,13.456276042102));
#58000=CARTESIAN_POINT('Ctrl Pts',(16.7194823514094,70.7144715118097,14.8499620203914));
#58001=CARTESIAN_POINT('Ctrl Pts',(16.5949769163906,72.2814741442132,15.0082888909979));
#58002=CARTESIAN_POINT('Ctrl Pts',(16.4704714813718,73.2790553155443,13.7895204752976));
#58003=CARTESIAN_POINT('Ctrl Pts',(16.3459660463531,72.8141679995884,12.2847133708637));
#58004=CARTESIAN_POINT('Ctrl Pts',(16.2214606113343,71.3029850736735,11.8409895470452));
#58005=CARTESIAN_POINT('Ctrl Pts',(16.0969551763155,70.0983362500405,12.8555760833815));
#58006=CARTESIAN_POINT('Ctrl Pts',(15.9724497412967,70.278638043073,14.4202025109772));
#58007=CARTESIAN_POINT('Ctrl Pts',(15.847944306278,71.682482147618,15.1341959035932));
#58008=CARTESIAN_POINT('Ctrl Pts',(15.7234388712592,73.0531297233953,14.3583804258011));
#58009=CARTESIAN_POINT('Ctrl Pts',(15.5989334362404,73.1635604657141,12.7872759132704));
#58010=CARTESIAN_POINT('Ctrl Pts',(15.4744280012216,71.9149145939534,11.8273541897304));
#58011=CARTESIAN_POINT('Ctrl Pts',(15.3499225662029,70.4249970286936,12.3379499256443));
#58012=CARTESIAN_POINT('Ctrl Pts',(15.2254171311841,70.0275970609997,13.8619697656991));
#58013=CARTESIAN_POINT('Ctrl Pts',(15.1009116961653,71.07847898034,15.0350957744051));
#58014=CARTESIAN_POINT('Ctrl Pts',(14.9764062611466,72.636866146912,14.8071238184768));
#58015=CARTESIAN_POINT('Ctrl Pts',(14.8519008261278,73.3076998863273,13.3821518989748));
#58016=CARTESIAN_POINT('Ctrl Pts',(14.727395391109,72.4903826184226,12.0358025589579));
#58017=CARTESIAN_POINT('Ctrl Pts',(14.6028899560903,70.9167072012529,11.9734056639631));
#58018=CARTESIAN_POINT('Ctrl Pts',(14.4783845210715,69.9952016410777,13.2506945893318));
#58019=CARTESIAN_POINT('Ctrl Pts',(14.3538790860527,70.5513110806915,14.7244799949148));
#58020=CARTESIAN_POINT('Ctrl Pts',(14.2293736510339,72.0861740763376,15.0748888386734));
#58021=CARTESIAN_POINT('Ctrl Pts',(14.1048682160152,73.2278594703359,13.9893028543541));
#58022=CARTESIAN_POINT('Ctrl Pts',(13.9803519848918,72.9499771151273,12.4372137102212));
#58023=CARTESIAN_POINT('Ctrl Pts',(13.8973375654414,71.9903838079969,12.0221283216363));
#58024=CARTESIAN_POINT('Ctrl Pts',(13.8558249576639,71.5273526845803,12.0609288632316));
#58025=CARTESIAN_POINT('Ctrl Pts',(19.8721991069221,70.2654039964372,14.1979725507859));
#58026=CARTESIAN_POINT('Ctrl Pts',(19.8306972952492,70.5045582939178,14.6513302692902));
#58027=CARTESIAN_POINT('Ctrl Pts',(19.7476936719033,71.4606165131408,15.296577613649));
#58028=CARTESIAN_POINT('Ctrl Pts',(19.6231882368845,73.0686104325118,14.6326257345719));
#58029=CARTESIAN_POINT('Ctrl Pts',(19.4986828018657,73.3994235394119,12.9260556908696));
#58030=CARTESIAN_POINT('Ctrl Pts',(19.374177366847,72.1615210857001,11.707312329996));
#58031=CARTESIAN_POINT('Ctrl Pts',(19.2496719318282,70.4608456560965,12.0661171047766));
#58032=CARTESIAN_POINT('Ctrl Pts',(19.1251664968095,69.8209577114928,13.681906585998));
#58033=CARTESIAN_POINT('Ctrl Pts',(19.0006610617907,70.8141570048277,15.1078911980679));
#58034=CARTESIAN_POINT('Ctrl Pts',(18.8761556267719,72.5515815552696,15.0676659597819));
#58035=CARTESIAN_POINT('Ctrl Pts',(18.7516501917531,73.4777389304046,13.5971655481964));
#58036=CARTESIAN_POINT('Ctrl Pts',(18.6271447567344,72.7635844462302,12.0128371029124));
#58037=CARTESIAN_POINT('Ctrl Pts',(18.5026393217156,71.048407265589,11.7329730033181));
#58038=CARTESIAN_POINT('Ctrl Pts',(18.3781338866968,69.8676703353299,13.0081199153126));
#58039=CARTESIAN_POINT('Ctrl Pts',(18.253628451678,70.278376614242,14.696746180277));
#58040=CARTESIAN_POINT('Ctrl Pts',(18.1291230166593,71.912860362431,15.2871747542049));
#58041=CARTESIAN_POINT('Ctrl Pts',(18.0046175816405,73.3079096971661,14.2508456191104));
#58042=CARTESIAN_POINT('Ctrl Pts',(17.8801121466217,73.2146600254213,12.5154939728233));
#58043=CARTESIAN_POINT('Ctrl Pts',(17.7556067116029,71.7165891854406,11.6346278732409));
#58044=CARTESIAN_POINT('Ctrl Pts',(17.6311012765842,70.1547889723317,12.3968096947535));
#58045=CARTESIAN_POINT('Ctrl Pts',(17.5065958415654,69.9274021969343,14.119724762267));
#58046=CARTESIAN_POINT('Ctrl Pts',(17.3820904065466,71.2379883692392,15.2609981775499));
#58047=CARTESIAN_POINT('Ctrl Pts',(17.2575849715279,72.9132944761003,14.7989478165527));
#58048=CARTESIAN_POINT('Ctrl Pts',(17.1330795365091,73.4535657337339,13.1472068974724));
#58049=CARTESIAN_POINT('Ctrl Pts',(17.0085741014903,72.375144608798,11.7844343643487));
#58050=CARTESIAN_POINT('Ctrl Pts',(16.8840686664715,70.6434470642325,11.9306010847461));
#58051=CARTESIAN_POINT('Ctrl Pts',(16.7595632314528,69.8087102087702,13.4548567978873));
#58052=CARTESIAN_POINT('Ctrl Pts',(16.635057796434,70.618200823648,14.9926688931807));
#58053=CARTESIAN_POINT('Ctrl Pts',(16.5105523614152,72.3472528762663,15.1673689191704));
#58054=CARTESIAN_POINT('Ctrl Pts',(16.3860469263965,73.4479975312372,13.8225632454232));
#58055=CARTESIAN_POINT('Ctrl Pts',(16.2615414913777,72.9350345334297,12.1621385856859));
#58056=CARTESIAN_POINT('Ctrl Pts',(16.1370360563589,71.2675747054093,11.6725276734234));
#58057=CARTESIAN_POINT('Ctrl Pts',(16.0125306213401,69.9383487819074,12.7920362798131));
#58058=CARTESIAN_POINT('Ctrl Pts',(15.8880251863214,70.1372962366768,14.5184663956743));
#58059=CARTESIAN_POINT('Ctrl Pts',(15.7635197513026,71.6863169468695,15.3062964321592));
#58060=CARTESIAN_POINT('Ctrl Pts',(15.6390143162838,73.1987081549679,14.4502510646592));
#58061=CARTESIAN_POINT('Ctrl Pts',(15.514508881265,73.3205589404931,12.7166729416266));
#58062=CARTESIAN_POINT('Ctrl Pts',(15.3900034462463,71.9427860746941,11.6574822344012));
#58063=CARTESIAN_POINT('Ctrl Pts',(15.2654980112275,70.2987907353288,12.2208805254978));
#58064=CARTESIAN_POINT('Ctrl Pts',(15.1409925762087,69.8602941970061,13.9025047794634));
#58065=CARTESIAN_POINT('Ctrl Pts',(15.01648714119,71.0198516234718,15.1969479995249));
#58066=CARTESIAN_POINT('Ctrl Pts',(14.8919817061712,72.7393972537189,14.9454006375828));
#58067=CARTESIAN_POINT('Ctrl Pts',(14.7674762711524,73.4796043408778,13.3730672085322));
#58068=CARTESIAN_POINT('Ctrl Pts',(14.6429708361336,72.5777653327687,11.8874870047984));
#58069=CARTESIAN_POINT('Ctrl Pts',(14.5184654011149,70.841350438533,11.8186374207984));
#58070=CARTESIAN_POINT('Ctrl Pts',(14.3939599660961,69.8245486493257,13.2280154221665));
#58071=CARTESIAN_POINT('Ctrl Pts',(14.2694545310773,70.4381673811397,14.8542103167684));
#58072=CARTESIAN_POINT('Ctrl Pts',(14.1449490960586,72.1317561207064,15.2408562087582));
#58073=CARTESIAN_POINT('Ctrl Pts',(14.0204436610398,73.3915073381686,14.0430058442048));
#58074=CARTESIAN_POINT('Ctrl Pts',(13.8959274299164,73.0848881617078,12.3304095377178));
#58075=CARTESIAN_POINT('Ctrl Pts',(13.8129130104661,72.0260598336227,11.872398665047));
#58076=CARTESIAN_POINT('Ctrl Pts',(13.7714004026886,71.5151449839512,11.9152117112416));
#58077=CARTESIAN_POINT('Ctrl Pts',(19.7877745519467,70.1360686465052,14.2661992589458));
#58078=CARTESIAN_POINT('Ctrl Pts',(19.7462727402738,70.3976368529192,14.762046360764));
#58079=CARTESIAN_POINT('Ctrl Pts',(19.6632691169279,71.4432983202816,15.4677672795824));
#58080=CARTESIAN_POINT('Ctrl Pts',(19.5387636819092,73.2019959052528,14.7415888082566));
#58081=CARTESIAN_POINT('Ctrl Pts',(19.4142582468904,73.5638133258121,12.8750763928258));
#58082=CARTESIAN_POINT('Ctrl Pts',(19.2897528118716,72.2098927484105,11.5421105279385));
#58083=CARTESIAN_POINT('Ctrl Pts',(19.1652473768528,70.3498273993866,11.9345430385847));
#58084=CARTESIAN_POINT('Ctrl Pts',(19.0407419418341,69.649968171519,13.701766797464));
#58085=CARTESIAN_POINT('Ctrl Pts',(18.9162365068153,70.7362516316372,15.2613968826537));
#58086=CARTESIAN_POINT('Ctrl Pts',(18.7917310717965,72.636510285679,15.2174016731096));
#58087=CARTESIAN_POINT('Ctrl Pts',(18.6672256367778,73.6494685558138,13.6090836991424));
#58088=CARTESIAN_POINT('Ctrl Pts',(18.542720201759,72.868382413955,11.8762695529223));
#58089=CARTESIAN_POINT('Ctrl Pts',(18.4182147667402,70.9924561874607,11.5701761590684));
#58090=CARTESIAN_POINT('Ctrl Pts',(18.2937093317214,69.7010587743754,12.9648318027199));
#58091=CARTESIAN_POINT('Ctrl Pts',(18.1692038967027,70.1502570780218,14.8117187208453));
#58092=CARTESIAN_POINT('Ctrl Pts',(18.0446984616839,71.9379271593483,15.4574831696756));
#58093=CARTESIAN_POINT('Ctrl Pts',(17.9201930266651,73.4637226653873,14.3240276726307));
#58094=CARTESIAN_POINT('Ctrl Pts',(17.7956875916463,73.3617334908503,12.4260361985122));
#58095=CARTESIAN_POINT('Ctrl Pts',(17.6711821566276,71.7232611454946,11.4626139719998));
#58096=CARTESIAN_POINT('Ctrl Pts',(17.5466767216088,70.0150866120508,12.2962286471894));
#58097=CARTESIAN_POINT('Ctrl Pts',(17.42217128659,69.7663887980055,14.1806179672258));
#58098=CARTESIAN_POINT('Ctrl Pts',(17.2976658515713,71.1998051240017,15.4288532839581));
#58099=CARTESIAN_POINT('Ctrl Pts',(17.1731604165525,73.0321234983004,14.9234988518104));
#58100=CARTESIAN_POINT('Ctrl Pts',(17.0486549815337,73.6230298099368,13.1169542309696));
#58101=CARTESIAN_POINT('Ctrl Pts',(16.9241495465149,72.4435373969628,11.6264605580787));
#58102=CARTESIAN_POINT('Ctrl Pts',(16.7996441114962,70.5495424926045,11.7863262485325));
#58103=CARTESIAN_POINT('Ctrl Pts',(16.6751386764774,69.6365728139866,13.4534375536726));
#58104=CARTESIAN_POINT('Ctrl Pts',(16.5506332414586,70.5219301354863,15.1353757659699));
#58105=CARTESIAN_POINT('Ctrl Pts',(16.4261278064399,72.4130316083195,15.3264489473428));
#58106=CARTESIAN_POINT('Ctrl Pts',(16.3016223714211,73.61693974693,13.8556060155489));
#58107=CARTESIAN_POINT('Ctrl Pts',(16.1771169364023,73.0559010672711,12.0395638005081));
#58108=CARTESIAN_POINT('Ctrl Pts',(16.0526115013835,71.2321643371453,11.5040657998015));
#58109=CARTESIAN_POINT('Ctrl Pts',(15.9281060663648,69.7783613137743,12.7284964762447));
#58110=CARTESIAN_POINT('Ctrl Pts',(15.803600631346,69.9959544302804,14.6167302803713));
#58111=CARTESIAN_POINT('Ctrl Pts',(15.6790951963272,71.690151746121,15.4783969607253));
#58112=CARTESIAN_POINT('Ctrl Pts',(15.5545897613085,73.3442865865404,14.5421217035174));
#58113=CARTESIAN_POINT('Ctrl Pts',(15.4300843262897,73.477557415272,12.646069969983));
#58114=CARTESIAN_POINT('Ctrl Pts',(15.3055788912709,71.9706575554347,11.487610279072));
#58115=CARTESIAN_POINT('Ctrl Pts',(15.1810734562521,70.172584441964,12.1038111253513));
#58116=CARTESIAN_POINT('Ctrl Pts',(15.0565680212334,69.6929913330123,13.9430397932278));
#58117=CARTESIAN_POINT('Ctrl Pts',(14.9320625862146,70.9612242666035,15.3588002246446));
#58118=CARTESIAN_POINT('Ctrl Pts',(14.8075571511958,72.8419283605258,15.0836774566888));
#58119=CARTESIAN_POINT('Ctrl Pts',(14.6830517161771,73.6515087954282,13.3639825180896));
#58120=CARTESIAN_POINT('Ctrl Pts',(14.5585462811583,72.6651480471149,11.7391714506388));
#58121=CARTESIAN_POINT('Ctrl Pts',(14.4340408461395,70.7659936758129,11.6638691776337));
#58122=CARTESIAN_POINT('Ctrl Pts',(14.3095354111207,69.6538956575739,13.2053362550011));
#58123=CARTESIAN_POINT('Ctrl Pts',(14.185029976102,70.3250236815881,14.9839406386219));
#58124=CARTESIAN_POINT('Ctrl Pts',(14.0605245410832,72.1773381650751,15.4068235788432));
#58125=CARTESIAN_POINT('Ctrl Pts',(13.9360191060644,73.5551552060015,14.0967088340556));
#58126=CARTESIAN_POINT('Ctrl Pts',(13.811502874941,73.2197992082883,12.2236053652145));
#58127=CARTESIAN_POINT('Ctrl Pts',(13.7284884554907,72.0617358592485,11.7226690084578));
#58128=CARTESIAN_POINT('Ctrl Pts',(13.6869758477133,71.5029372833219,11.7694945592516));
#58129=CARTESIAN_POINT('Ctrl Pts',(13.939,73.2573116306334,14.0236386281943));
#58130=CARTESIAN_POINT('Ctrl Pts',(13.939,73.2597351913816,14.0164255871116));
#58131=CARTESIAN_POINT('Ctrl Pts',(13.939,73.2621587521298,14.0092125460289));
#58132=CARTESIAN_POINT('Ctrl Pts',(13.939,73.264582312878,14.0019995049462));
#58133=CARTESIAN_POINT('',(19.7896276022603,72.6408167039313,14.2604548813054));
#58134=CARTESIAN_POINT('Ctrl Pts',(19.789,72.641620209933,14.2612225008607));
#58135=CARTESIAN_POINT('Ctrl Pts',(19.789,72.6387719444729,14.266450811799));
#58136=CARTESIAN_POINT('Ctrl Pts',(19.7890000000001,72.6358841274372,14.2716554974063));
#58137=CARTESIAN_POINT('Ctrl Pts',(19.789,72.6329568803625,14.2768360690663));
#58138=CARTESIAN_POINT('Ctrl Pts',(19.789,72.6082794067475,14.3205096699577));
#58139=CARTESIAN_POINT('Ctrl Pts',(19.789,72.5808040359192,14.3624698284424));
#58140=CARTESIAN_POINT('Ctrl Pts',(19.789,72.5508379984757,14.4026372192824));
#58141=CARTESIAN_POINT('Ctrl Pts',(19.789,72.5340932826451,14.4250823472557));
#58142=CARTESIAN_POINT('Ctrl Pts',(19.789,72.516569904339,14.4469676385987));
#58143=CARTESIAN_POINT('Ctrl Pts',(19.789,72.4983147064114,14.4682781592601));
#58144=CARTESIAN_POINT('Ctrl Pts',(19.789,72.4886668022326,14.4795408068717));
#58145=CARTESIAN_POINT('Ctrl Pts',(19.789,72.4788144131649,14.4906428946705));
#58146=CARTESIAN_POINT('Ctrl Pts',(19.789,72.4687639579593,14.5015820667859));
#58147=CARTESIAN_POINT('Ctrl Pts',(19.789,72.4599513410421,14.5111739440961));
#58148=CARTESIAN_POINT('Ctrl Pts',(19.789,72.4509925607107,14.5206338520356));
#58149=CARTESIAN_POINT('Ctrl Pts',(19.789,72.4418947144233,14.5299583775618));
#58150=CARTESIAN_POINT('Ctrl Pts',(19.789,72.4045912780145,14.5681912553245));
#58151=CARTESIAN_POINT('Ctrl Pts',(19.789,72.3649432494347,14.6041609037284));
#58152=CARTESIAN_POINT('Ctrl Pts',(19.789,72.3232702684491,14.637772358608));
#58153=CARTESIAN_POINT('Ctrl Pts',(19.789,72.2992595261045,14.657138287415));
#58154=CARTESIAN_POINT('Ctrl Pts',(19.789,72.274575549839,14.6757211293625));
#58155=CARTESIAN_POINT('Ctrl Pts',(19.789,72.2492721984787,14.6934998632628));
#58156=CARTESIAN_POINT('Ctrl Pts',(19.789,72.2369517511987,14.7021565012948));
#58157=CARTESIAN_POINT('Ctrl Pts',(19.789,72.2244810608313,14.7106244461823));
#58158=CARTESIAN_POINT('Ctrl Pts',(19.789,72.2118891168812,14.7188864255039));
#58159=CARTESIAN_POINT('Ctrl Pts',(19.789,72.1656012648316,14.7492573736266));
#58160=CARTESIAN_POINT('Ctrl Pts',(19.789,72.1176239693264,14.7768870422043));
#58161=CARTESIAN_POINT('Ctrl Pts',(19.789,72.0682888938632,14.801685512822));
#58162=CARTESIAN_POINT('Ctrl Pts',(19.789,72.0175949058287,14.8271670462132));
#58163=CARTESIAN_POINT('Ctrl Pts',(19.789,71.965466663248,14.8496601676798));
#58164=CARTESIAN_POINT('Ctrl Pts',(19.789,71.9122161490832,14.8690412852909));
#58165=CARTESIAN_POINT('Ctrl Pts',(19.789,71.878811941916,14.881199118468));
#58166=CARTESIAN_POINT('Ctrl Pts',(19.789,71.8449651868027,14.892131784855));
#58167=CARTESIAN_POINT('Ctrl Pts',(19.789,71.8107455960956,14.9018012949587));
#58168=CARTESIAN_POINT('Ctrl Pts',(19.789,71.7938250741778,14.9065825665714));
#58169=CARTESIAN_POINT('Ctrl Pts',(19.789,71.7768133199693,14.9110548975236));
#58170=CARTESIAN_POINT('Ctrl Pts',(19.789,71.7597183837639,14.9152130609202));
#58171=CARTESIAN_POINT('Ctrl Pts',(19.789,71.7498995878967,14.9176013797231));
#58172=CARTESIAN_POINT('Ctrl Pts',(19.789,71.7400510664113,14.9198865455108));
#58173=CARTESIAN_POINT('Ctrl Pts',(19.789,71.7301817745093,14.9220658655007));
#58174=CARTESIAN_POINT('Ctrl Pts',(19.789,71.6725102077602,14.9348008012503));
#58175=CARTESIAN_POINT('Ctrl Pts',(19.789,71.6143038238963,14.9438881407692));
#58176=CARTESIAN_POINT('Ctrl Pts',(19.789,71.5559056616475,14.9492168055038));
#58177=CARTESIAN_POINT('Ctrl Pts',(19.789,71.5362035607306,14.9510145656783));
#58178=CARTESIAN_POINT('Ctrl Pts',(19.789,71.5164792954917,14.9523842178932));
#58179=CARTESIAN_POINT('Ctrl Pts',(19.789,71.4967451192257,14.9533205346688));
#58180=CARTESIAN_POINT('Ctrl Pts',(19.789,71.4401728765432,14.9560046872345));
#58181=CARTESIAN_POINT('Ctrl Pts',(19.789,71.3835204002696,14.9551314660335));
#58182=CARTESIAN_POINT('Ctrl Pts',(19.789,71.3270157996704,14.9508956287317));
#58183=CARTESIAN_POINT('Ctrl Pts',(19.789,71.2970745678256,14.9486511002267));
#58184=CARTESIAN_POINT('Ctrl Pts',(19.789,71.2671745497408,14.945461559463));
#58185=CARTESIAN_POINT('Ctrl Pts',(19.789,71.2373482913903,14.9413503873858));
#58186=CARTESIAN_POINT('Ctrl Pts',(19.789,71.2204156653886,14.9390164392789));
#58187=CARTESIAN_POINT('Ctrl Pts',(19.789,71.2035067992762,14.9363853860378));
#58188=CARTESIAN_POINT('Ctrl Pts',(19.789,71.1866275930246,14.9334609646543));
#58189=CARTESIAN_POINT('Ctrl Pts',(19.789,71.1719630215258,14.9309202417179));
#58190=CARTESIAN_POINT('Ctrl Pts',(19.789,71.1573154150842,14.928156812882));
#58191=CARTESIAN_POINT('Ctrl Pts',(19.789,71.1427203611893,14.9251798379043));
#58192=CARTESIAN_POINT('Ctrl Pts',(19.789,71.084427289372,14.9132897128372));
#58193=CARTESIAN_POINT('Ctrl Pts',(19.789,71.0268925829723,14.8979855977678));
#58194=CARTESIAN_POINT('Ctrl Pts',(19.789,70.9703678600636,14.8795032122604));
#58195=CARTESIAN_POINT('Ctrl Pts',(19.789,70.9120325610004,14.8604288067527));
#58196=CARTESIAN_POINT('Ctrl Pts',(19.789,70.8547720822423,14.8379693077407));
#58197=CARTESIAN_POINT('Ctrl Pts',(19.789,70.7988513813129,14.812328463574));
#58198=CARTESIAN_POINT('Ctrl Pts',(19.789,70.7429306803836,14.7866876194072));
#58199=CARTESIAN_POINT('Ctrl Pts',(19.789,70.6883487124932,14.7578651502859));
#58200=CARTESIAN_POINT('Ctrl Pts',(19.789,70.6353738709878,14.7260125179742));
#58201=CARTESIAN_POINT('Ctrl Pts',(19.789,70.6249237878694,14.7197291078547));
#58202=CARTESIAN_POINT('Ctrl Pts',(19.789,70.614536282974,14.7133276283047));
#58203=CARTESIAN_POINT('Ctrl Pts',(19.789,70.6042134878844,14.7068090168181));
#58204=CARTESIAN_POINT('Ctrl Pts',(19.789,70.5941967736294,14.7004836884516));
#58205=CARTESIAN_POINT('Ctrl Pts',(19.789,70.5842482301542,14.6940525900351));
#58206=CARTESIAN_POINT('Ctrl Pts',(19.789,70.5743748300446,14.6875206335784));
#58207=CARTESIAN_POINT('Ctrl Pts',(19.789,70.5206424546419,14.6519728453245));
#58208=CARTESIAN_POINT('Ctrl Pts',(19.789,70.4690864887003,14.6134113895555));
#58209=CARTESIAN_POINT('Ctrl Pts',(19.789,70.419985490651,14.5720639021248));
#58210=CARTESIAN_POINT('Ctrl Pts',(19.789,70.3709118097536,14.5307394182099));
#58211=CARTESIAN_POINT('Ctrl Pts',(19.789,70.324289270061,14.4866316356991));
#58212=CARTESIAN_POINT('Ctrl Pts',(19.789,70.2804049653145,14.4399165596753));
#58213=CARTESIAN_POINT('Ctrl Pts',(19.789,70.2371769561625,14.3939001138058));
#58214=CARTESIAN_POINT('Ctrl Pts',(19.789,70.1966048791055,14.3453533038319));
#58215=CARTESIAN_POINT('Ctrl Pts',(19.789,70.1589874472662,14.294401015779));
#58216=CARTESIAN_POINT('Ctrl Pts',(19.789,70.1518669431078,14.2847563919645));
#58217=CARTESIAN_POINT('Ctrl Pts',(19.789,70.1448523993543,14.275025465843));
#58218=CARTESIAN_POINT('Ctrl Pts',(19.789,70.1379459883857,14.2652089275579));
#58219=CARTESIAN_POINT('Ctrl Pts',(19.7896276022603,72.6399620111973,14.2597761745477));
#58220=CARTESIAN_POINT('Ctrl Pts',(19.7894184015068,72.6425467167479,14.2565212650763));
#58221=CARTESIAN_POINT('Ctrl Pts',(19.7892092007534,72.6451154436252,14.2532536670299));
#58222=CARTESIAN_POINT('Ctrl Pts',(19.789,72.647668068024,14.249973537897));
#58223=CARTESIAN_POINT('Origin',(19.789,71.6454,13.47));
#58224=CARTESIAN_POINT('',(19.789,70.1487787364881,12.6545862220908));
#58225=CARTESIAN_POINT('',(19.789,71.6454,15.17434));
#58226=CARTESIAN_POINT('Origin',(19.789,71.6454,13.47));
#58227=CARTESIAN_POINT('Ctrl Pts',(19.789,70.1487787364881,12.6545862220908));
#58228=CARTESIAN_POINT('Ctrl Pts',(19.789,70.1489198244377,12.6543919049109));
#58229=CARTESIAN_POINT('Ctrl Pts',(19.789,70.1490609573038,12.6541976212514));
#58230=CARTESIAN_POINT('Ctrl Pts',(19.789,70.149202135088,12.6540033711292));
#58231=CARTESIAN_POINT('Ctrl Pts',(19.789,70.1879762118368,12.6006531277364));
#58232=CARTESIAN_POINT('Ctrl Pts',(19.789,70.2301358263451,12.5498286668655));
#58233=CARTESIAN_POINT('Ctrl Pts',(19.789,70.2753374488553,12.5016996841948));
#58234=CARTESIAN_POINT('Ctrl Pts',(19.789,70.3045799803949,12.4705633396221));
#58235=CARTESIAN_POINT('Ctrl Pts',(19.789,70.3350964259176,12.4405560547994));
#58236=CARTESIAN_POINT('Ctrl Pts',(19.789,70.3667987628524,12.4117351475176));
#58237=CARTESIAN_POINT('Ctrl Pts',(19.789,70.3785067074331,12.401091339589));
#58238=CARTESIAN_POINT('Ctrl Pts',(19.789,70.3903782324118,12.3906078824228));
#58239=CARTESIAN_POINT('Ctrl Pts',(19.789,70.4024031776679,12.3802929434665));
#58240=CARTESIAN_POINT('Ctrl Pts',(19.789,70.4508048825224,12.3387741988632));
#58241=CARTESIAN_POINT('Ctrl Pts',(19.789,70.5015910097002,12.3000658874002));
#58242=CARTESIAN_POINT('Ctrl Pts',(19.789,70.5544538397869,12.2643380655472));
#58243=CARTESIAN_POINT('Ctrl Pts',(19.789,70.5898575003643,12.2404101813234));
#58244=CARTESIAN_POINT('Ctrl Pts',(19.789,70.6261931205748,12.2178201212625));
#58245=CARTESIAN_POINT('Ctrl Pts',(19.789,70.6633705338864,12.1966318922625));
#58246=CARTESIAN_POINT('Ctrl Pts',(19.789,70.67687546201,12.1889351354356));
#58247=CARTESIAN_POINT('Ctrl Pts',(19.789,70.690491471705,12.1814234606844));
#58248=CARTESIAN_POINT('Ctrl Pts',(19.789,70.7042142283386,12.174100295955));
#58249=CARTESIAN_POINT('Ctrl Pts',(19.789,70.7145797303758,12.1685687339702));
#58250=CARTESIAN_POINT('Ctrl Pts',(19.789,70.7250059162256,12.1631449583535));
#58251=CARTESIAN_POINT('Ctrl Pts',(19.789,70.7354785604031,12.157836434949));
#58252=CARTESIAN_POINT('Ctrl Pts',(19.789,70.7903722896243,12.1300111177326));
#58253=CARTESIAN_POINT('Ctrl Pts',(19.789,70.8466272484881,12.1053018562078));
#58254=CARTESIAN_POINT('Ctrl Pts',(19.789,70.903964603326,12.0838618819254));
#58255=CARTESIAN_POINT('Ctrl Pts',(19.789,70.9598880709669,12.0629505979745));
#58256=CARTESIAN_POINT('Ctrl Pts',(19.789,71.0168421988663,12.0451493184059));
#58257=CARTESIAN_POINT('Ctrl Pts',(19.789,71.0745683658387,12.0306489624154));
#58258=CARTESIAN_POINT('Ctrl Pts',(19.789,71.1107541019409,12.0215593920736));
#58259=CARTESIAN_POINT('Ctrl Pts',(19.789,71.147243151667,12.0137678679056));
#58260=CARTESIAN_POINT('Ctrl Pts',(19.789,71.183969313623,12.0073316554369));
#58261=CARTESIAN_POINT('Ctrl Pts',(19.789,71.2169581642735,12.0015504019494));
#58262=CARTESIAN_POINT('Ctrl Pts',(19.789,71.2501383400913,11.9968627522112));
#58263=CARTESIAN_POINT('Ctrl Pts',(19.789,71.2834594960917,11.9933158611134));
#58264=CARTESIAN_POINT('Ctrl Pts',(19.789,71.2944980578517,11.9921408545669));
#58265=CARTESIAN_POINT('Ctrl Pts',(19.789,71.3055440776528,11.9910919794509));
#58266=CARTESIAN_POINT('Ctrl Pts',(19.789,71.3165900557996,11.9901708649002));
#58267=CARTESIAN_POINT('Ctrl Pts',(19.789,71.373278300547,11.9854436812687));
#58268=CARTESIAN_POINT('Ctrl Pts',(19.789,71.4300147845701,11.9840721766392));
#58269=CARTESIAN_POINT('Ctrl Pts',(19.789,71.4865655032522,11.9862218894224));
#58270=CARTESIAN_POINT('Ctrl Pts',(19.789,71.4969969079928,11.9866184276918));
#58271=CARTESIAN_POINT('Ctrl Pts',(19.789,71.5074219568044,11.9871349167772));
#58272=CARTESIAN_POINT('Ctrl Pts',(19.789,71.5178391251249,11.9877725845906));
#58273=CARTESIAN_POINT('Ctrl Pts',(19.789,71.5747021515476,11.9912533502463));
#58274=CARTESIAN_POINT('Ctrl Pts',(19.789,71.6313325553251,11.998341595826));
#58275=CARTESIAN_POINT('Ctrl Pts',(19.789,71.6874486199552,12.0089024886782));
#58276=CARTESIAN_POINT('Ctrl Pts',(19.789,71.7385648764786,12.0185224310549));
#58277=CARTESIAN_POINT('Ctrl Pts',(19.789,71.789254587842,12.0310247112241));
#58278=CARTESIAN_POINT('Ctrl Pts',(19.789,71.8392799419038,12.0463316703637));
#58279=CARTESIAN_POINT('Ctrl Pts',(19.789,71.8488104716665,12.0492478602117));
#58280=CARTESIAN_POINT('Ctrl Pts',(19.789,71.8583145157961,12.0522652805629));
#58281=CARTESIAN_POINT('Ctrl Pts',(19.789,71.8677801889141,12.055379744509));
#58282=CARTESIAN_POINT('Ctrl Pts',(19.789,71.9211107347488,12.0729269448148));
#58283=CARTESIAN_POINT('Ctrl Pts',(19.789,71.9733200814847,12.0935796656819));
#58284=CARTESIAN_POINT('Ctrl Pts',(19.789,72.024145868163,12.1171840112806));
#58285=CARTESIAN_POINT('Ctrl Pts',(19.789,72.0745282756665,12.1405824441733));
#58286=CARTESIAN_POINT('Ctrl Pts',(19.789,72.1235519535232,12.1668820916441));
#58287=CARTESIAN_POINT('Ctrl Pts',(19.789,72.1709238057524,12.1959669353727));
#58288=CARTESIAN_POINT('Ctrl Pts',(19.789,72.2170798876667,12.2243053339456));
#58289=CARTESIAN_POINT('Ctrl Pts',(19.789,72.2616683576994,12.2552886122479));
#58290=CARTESIAN_POINT('Ctrl Pts',(19.789,72.3043729294909,12.288829428407));
#58291=CARTESIAN_POINT('Ctrl Pts',(19.789,72.3141234565815,12.2964876397619));
#58292=CARTESIAN_POINT('Ctrl Pts',(19.789,72.3237775801607,12.304281098163));
#58293=CARTESIAN_POINT('Ctrl Pts',(19.789,72.3333127754152,12.3121930388631));
#58294=CARTESIAN_POINT('Ctrl Pts',(19.789,72.3739413221764,12.3459050546245));
#58295=CARTESIAN_POINT('Ctrl Pts',(19.789,72.4124882882934,12.3818224635262));
#58296=CARTESIAN_POINT('Ctrl Pts',(19.789,72.4487040921249,12.4198334708158));
#58297=CARTESIAN_POINT('Ctrl Pts',(19.789,72.4859547374258,12.4589306162682));
#58298=CARTESIAN_POINT('Ctrl Pts',(19.789,72.5207400586359,12.5002434669381));
#58299=CARTESIAN_POINT('Ctrl Pts',(19.789,72.5527331601959,12.5436703974697));
#58300=CARTESIAN_POINT('Ctrl Pts',(19.789,72.5823338904573,12.5838499610027));
#58301=CARTESIAN_POINT('Ctrl Pts',(19.789,72.6095441962068,12.6258399981718));
#58302=CARTESIAN_POINT('Ctrl Pts',(19.789,72.63405470443,12.6695658026545));
#58303=CARTESIAN_POINT('Ctrl Pts',(19.789,72.6360356770569,12.673099781672));
#58304=CARTESIAN_POINT('Ctrl Pts',(19.789,72.6379989859775,12.6766450988997));
#58305=CARTESIAN_POINT('Ctrl Pts',(19.789,72.6399444526778,12.6802017145829));
#58306=CARTESIAN_POINT('Origin',(19.789,71.6454,13.47));
#58307=CARTESIAN_POINT('Ctrl Pts',(20.040973809758,72.9819445553179,12.4091675667597));
#58308=CARTESIAN_POINT('Ctrl Pts',(19.999461202279,72.633355430368,11.9699615052754));
#58309=CARTESIAN_POINT('Ctrl Pts',(19.9164467831271,71.4752515269709,11.4692823470277));
#58310=CARTESIAN_POINT('Ctrl Pts',(19.7919305523022,69.8808452508188,12.5077823363638));
#58311=CARTESIAN_POINT('Ctrl Pts',(19.6674251172834,69.8699348774273,14.4089112278554));
#58312=CARTESIAN_POINT('Ctrl Pts',(19.5429196822646,71.4466435928667,15.4688729946812));
#58313=CARTESIAN_POINT('Ctrl Pts',(19.4184142472458,73.202158953221,14.7397343798463));
#58314=CARTESIAN_POINT('Ctrl Pts',(19.2939088122271,73.563614891359,12.8737593469291));
#58315=CARTESIAN_POINT('Ctrl Pts',(19.1694033772083,72.2080713563702,11.5416219660584));
#58316=CARTESIAN_POINT('Ctrl Pts',(19.0448979421895,70.3487144949671,11.9357554795025));
#58317=CARTESIAN_POINT('Ctrl Pts',(18.9203925071708,69.6502169789121,13.7033818367937));
#58318=CARTESIAN_POINT('Ctrl Pts',(18.795887072152,70.7378073584978,15.2620730044683));
#58319=CARTESIAN_POINT('Ctrl Pts',(18.6713816371332,72.6378980052588,15.2164825479556));
#58320=CARTESIAN_POINT('Ctrl Pts',(18.5468762021145,73.6494862177602,13.6074171356146));
#58321=CARTESIAN_POINT('Ctrl Pts',(18.4223707670957,72.8669944998988,11.8753352416511));
#58322=CARTESIAN_POINT('Ctrl Pts',(18.2978653320769,70.9909148234652,11.5708164984104));
#58323=CARTESIAN_POINT('Ctrl Pts',(18.1733598970581,69.7007390850565,12.9664706197299));
#58324=CARTESIAN_POINT('Ctrl Pts',(18.0488544620394,70.1514475657618,14.8128903622671));
#58325=CARTESIAN_POINT('Ctrl Pts',(17.9243490270206,71.9395609525946,15.4571380645241));
#58326=CARTESIAN_POINT('Ctrl Pts',(17.7998435920018,73.4643377264577,14.3224751075195));
#58327=CARTESIAN_POINT('Ctrl Pts',(17.675338156983,73.3607789380809,12.4246658804603));
#58328=CARTESIAN_POINT('Ctrl Pts',(17.5508327219643,71.7215916392195,11.4626527092184));
#58329=CARTESIAN_POINT('Ctrl Pts',(17.4263272869455,70.0141966499276,12.2976417212453));
#58330=CARTESIAN_POINT('Ctrl Pts',(17.3018218519267,69.7670751170318,14.1821403964886));
#58331=CARTESIAN_POINT('Ctrl Pts',(17.177316416908,71.2014533072286,15.4291221611814));
#58332=CARTESIAN_POINT('Ctrl Pts',(17.0528109818892,73.0332580794223,14.9222734795421));
#58333=CARTESIAN_POINT('Ctrl Pts',(16.9283055468704,73.6226350938871,13.1153315752696));
#58334=CARTESIAN_POINT('Ctrl Pts',(16.8038001118517,72.4419667407709,11.6258932417151));
#58335=CARTESIAN_POINT('Ctrl Pts',(16.6792946768329,70.5482019652493,11.7873221393186));
#58336=CARTESIAN_POINT('Ctrl Pts',(16.5547892418141,69.6366624746966,13.4551051186589));
#58337=CARTESIAN_POINT('Ctrl Pts',(16.4302838067953,70.5233697144127,15.1362221790386));
#58338=CARTESIAN_POINT('Ctrl Pts',(16.3057783717766,72.4145323853567,15.3257164914074));
#58339=CARTESIAN_POINT('Ctrl Pts',(16.1812729367578,73.6171581900668,13.853950389472));
#58340=CARTESIAN_POINT('Ctrl Pts',(16.056767501739,73.0546416597839,12.0384671509735));
#58341=CARTESIAN_POINT('Ctrl Pts',(15.9322620667202,71.2305544421676,11.5045098412908));
#58342=CARTESIAN_POINT('Ctrl Pts',(15.8077566317015,69.7778422804962,12.7300837376931));
#58343=CARTESIAN_POINT('Ctrl Pts',(15.6832511966827,69.9969905948197,14.6180397431827));
#58344=CARTESIAN_POINT('Ctrl Pts',(15.5587457616639,71.6918161520591,15.4782565459948));
#58345=CARTESIAN_POINT('Ctrl Pts',(15.4342403266452,73.345087948424,14.5406567682313));
#58346=CARTESIAN_POINT('Ctrl Pts',(15.3097348916264,73.476780975954,12.6445926450108));
#58347=CARTESIAN_POINT('Ctrl Pts',(15.1852294566076,71.9689930174075,11.4874416489449));
#58348=CARTESIAN_POINT('Ctrl Pts',(15.0607240215888,70.1715328997075,12.1051050809465));
#58349=CARTESIAN_POINT('Ctrl Pts',(14.9362185865701,69.6934717153363,13.9446319828763));
#58350=CARTESIAN_POINT('Ctrl Pts',(14.8117131515513,70.9628523308878,15.3592775276433));
#58351=CARTESIAN_POINT('Ctrl Pts',(14.6872077165325,72.8431530960336,15.0825876121152));
#58352=CARTESIAN_POINT('Ctrl Pts',(14.5627022815138,73.6514248701469,13.3623521753633));
#58353=CARTESIAN_POINT('Ctrl Pts',(14.438196846495,72.6634403331674,11.7383559146618));
#58354=CARTESIAN_POINT('Ctrl Pts',(14.3136914114762,70.7649881924949,11.6648114379736));
#58355=CARTESIAN_POINT('Ctrl Pts',(14.1891859764574,69.6528597290574,13.2067518969809));
#58356=CARTESIAN_POINT('Ctrl Pts',(14.0646805414387,70.3282556438409,14.9854666458723));
#58357=CARTESIAN_POINT('Ctrl Pts',(13.9816769180928,71.5585834209095,15.2639982872471));
#58358=CARTESIAN_POINT('Ctrl Pts',(13.9401751064199,72.0989948849057,15.1149828251624));
#58359=CARTESIAN_POINT('Ctrl Pts',(19.9565660471403,72.8674323206533,12.5000573856227));
#58360=CARTESIAN_POINT('Ctrl Pts',(19.9150534396612,72.5487095548299,12.0984815455766));
#58361=CARTESIAN_POINT('Ctrl Pts',(19.8320390205094,71.4898294785953,11.6406994901849));
#58362=CARTESIAN_POINT('Ctrl Pts',(19.7075227896845,70.0320284693002,12.5902230559481));
#58363=CARTESIAN_POINT('Ctrl Pts',(19.5830173546657,70.0220528730047,14.3284673530698));
#58364=CARTESIAN_POINT('Ctrl Pts',(19.458511919647,71.4636726101519,15.2976138978402));
#58365=CARTESIAN_POINT('Ctrl Pts',(19.3340064846282,73.0687792272267,14.6309462959114));
#58366=CARTESIAN_POINT('Ctrl Pts',(19.2095010496094,73.3992664056296,12.9248439511118));
#58367=CARTESIAN_POINT('Ctrl Pts',(19.0849956145907,72.1598628966198,11.706841207771));
#58368=CARTESIAN_POINT('Ctrl Pts',(18.9604901795719,70.459811692773,12.0672062178001));
#58369=CARTESIAN_POINT('Ctrl Pts',(18.8359847445531,69.82115992683,13.6833861878982));
#58370=CARTESIAN_POINT('Ctrl Pts',(18.7114793095343,70.8155679248255,15.1085320816407));
#58371=CARTESIAN_POINT('Ctrl Pts',(18.5869738745156,72.5528629317702,15.0668477164242));
#58372=CARTESIAN_POINT('Ctrl Pts',(18.4624684394968,73.4777804632882,13.5956435338909));
#58373=CARTESIAN_POINT('Ctrl Pts',(18.337963004478,72.7623309363231,12.0119626547013));
#58374=CARTESIAN_POINT('Ctrl Pts',(18.2134575694592,71.0469896919175,11.7335344159986));
#58375=CARTESIAN_POINT('Ctrl Pts',(18.0889521344405,69.8673534086486,13.0096119234183));
#58376=CARTESIAN_POINT('Ctrl Pts',(17.9644466994217,70.2794461656189,14.6978344326455));
#58377=CARTESIAN_POINT('Ctrl Pts',(17.8399412644029,71.9143578810632,15.2868843910119));
#58378=CARTESIAN_POINT('Ctrl Pts',(17.7154358293842,73.3084950925974,14.2494368917941));
#58379=CARTESIAN_POINT('Ctrl Pts',(17.5909303943654,73.2138089962899,12.5142278374661));
#58380=CARTESIAN_POINT('Ctrl Pts',(17.4664249593466,71.7150637050516,11.6346378653441));
#58381=CARTESIAN_POINT('Ctrl Pts',(17.3419195243278,70.1539546101586,12.3980868323294));
#58382=CARTESIAN_POINT('Ctrl Pts',(17.2174140893091,69.9280059134793,14.121125754012));
#58383=CARTESIAN_POINT('Ctrl Pts',(17.0929086542903,71.2394896956594,15.2612688294198));
#58384=CARTESIAN_POINT('Ctrl Pts',(16.9684032192715,72.9143494134601,14.7978458420012));
#58385=CARTESIAN_POINT('Ctrl Pts',(16.8438977842528,73.4532298853908,13.1457187955978));
#58386=CARTESIAN_POINT('Ctrl Pts',(16.719392349234,72.3737186324814,11.7838923035579));
#58387=CARTESIAN_POINT('Ctrl Pts',(16.5948869142152,70.6422075098673,11.9314903238213));
#58388=CARTESIAN_POINT('Ctrl Pts',(16.4703814791964,69.8087667430968,13.4563812797421));
#58389=CARTESIAN_POINT('Ctrl Pts',(16.3458760441777,70.6195028323494,14.9934638815989));
#58390=CARTESIAN_POINT('Ctrl Pts',(16.2213706091589,72.3486347930544,15.1667227328458));
#58391=CARTESIAN_POINT('Ctrl Pts',(16.0968651741401,73.4482222307946,13.8210543540021));
#58392=CARTESIAN_POINT('Ctrl Pts',(15.9723597391213,72.9339008950991,12.1611177763384));
#58393=CARTESIAN_POINT('Ctrl Pts',(15.8478543041026,71.2660975085615,11.6729087692499));
#58394=CARTESIAN_POINT('Ctrl Pts',(15.7233488690838,69.9378505697632,12.7934781560268));
#58395=CARTESIAN_POINT('Ctrl Pts',(15.598843434065,70.1382227324828,14.5196781914091));
#58396=CARTESIAN_POINT('Ctrl Pts',(15.4743379990463,71.6878393169617,15.3061934868572));
#58397=CARTESIAN_POINT('Ctrl Pts',(15.3498325640275,73.1994623765476,14.4489252216837));
#58398=CARTESIAN_POINT('Ctrl Pts',(15.2253271290087,73.3198722315023,12.7153117544878));
#58399=CARTESIAN_POINT('Ctrl Pts',(15.1008216939899,71.9412682704863,11.6573029425538));
#58400=CARTESIAN_POINT('Ctrl Pts',(14.9763162589712,70.2978106317753,12.222046313202));
#58401=CARTESIAN_POINT('Ctrl Pts',(14.8518108239524,69.8607086913822,13.9039665454345));
#58402=CARTESIAN_POINT('Ctrl Pts',(14.7273053889336,71.0213315327552,15.197408332388));
#58403=CARTESIAN_POINT('Ctrl Pts',(14.6027999539149,72.7405322121599,14.9444246078808));
#58404=CARTESIAN_POINT('Ctrl Pts',(14.4782945188961,73.4795530161492,13.3715752071784));
#58405=CARTESIAN_POINT('Ctrl Pts',(14.3537890838773,72.5762168484989,11.8867194189437));
#58406=CARTESIAN_POINT('Ctrl Pts',(14.2292836488585,70.8404199639996,11.8194760732872));
#58407=CARTESIAN_POINT('Ctrl Pts',(14.1047782138398,69.8235762518826,13.2293064227002));
#58408=CARTESIAN_POINT('Ctrl Pts',(13.980272778821,70.4411057115768,14.8556247550891));
#58409=CARTESIAN_POINT('Ctrl Pts',(13.8972691554751,71.5660216768494,15.1102924103725));
#58410=CARTESIAN_POINT('Ctrl Pts',(13.8557673438022,72.0601318603277,14.9740442694332));
#58411=CARTESIAN_POINT('Ctrl Pts',(19.8721582845226,72.7529200859888,12.5909472044855));
#58412=CARTESIAN_POINT('Ctrl Pts',(19.8306456770436,72.4640636792919,12.2270015858779));
#58413=CARTESIAN_POINT('Ctrl Pts',(19.7476312578916,71.5044074302198,11.812116633342));
#58414=CARTESIAN_POINT('Ctrl Pts',(19.6231150270668,70.1832116877817,12.6726637755322));
#58415=CARTESIAN_POINT('Ctrl Pts',(19.4986095920481,70.1741708685821,14.2480234782843));
#58416=CARTESIAN_POINT('Ctrl Pts',(19.3741041570293,71.4807016274368,15.126354800999));
#58417=CARTESIAN_POINT('Ctrl Pts',(19.2495987220105,72.9353995012324,14.5221582119765));
#58418=CARTESIAN_POINT('Ctrl Pts',(19.1250932869917,73.2349179199001,12.9759285552946));
#58419=CARTESIAN_POINT('Ctrl Pts',(19.000587851973,72.1116544368694,11.8720604494837));
#58420=CARTESIAN_POINT('Ctrl Pts',(18.8760824169542,70.5709088905788,12.1986569560976));
#58421=CARTESIAN_POINT('Ctrl Pts',(18.7515769819354,69.9921028747479,13.6633905390027));
#58422=CARTESIAN_POINT('Ctrl Pts',(18.6270715469167,70.8933284911529,14.9549911588131));
#58423=CARTESIAN_POINT('Ctrl Pts',(18.5025661118979,72.4678278582817,14.917212884893));
#58424=CARTESIAN_POINT('Ctrl Pts',(18.3780606768791,73.3060747088162,13.583869932167));
#58425=CARTESIAN_POINT('Ctrl Pts',(18.2535552418603,72.6576673727473,12.1485900677515));
#58426=CARTESIAN_POINT('Ctrl Pts',(18.1290498068416,71.1030645603695,11.8962523335869));
#58427=CARTESIAN_POINT('Ctrl Pts',(18.0045443718228,70.0339677322408,13.0527532271067));
#58428=CARTESIAN_POINT('Ctrl Pts',(17.880038936804,70.407444765476,14.5827785030239));
#58429=CARTESIAN_POINT('Ctrl Pts',(17.7555335017852,71.8891548095317,15.1166307174996));
#58430=CARTESIAN_POINT('Ctrl Pts',(17.6310280667665,73.1526524587371,14.1763986760686));
#58431=CARTESIAN_POINT('Ctrl Pts',(17.5065226317477,73.0668390544988,12.6037897944718));
#58432=CARTESIAN_POINT('Ctrl Pts',(17.382017196729,71.7085357708834,11.8066230214698));
#58433=CARTESIAN_POINT('Ctrl Pts',(17.2575117617102,70.2937125703898,12.4985319434135));
#58434=CARTESIAN_POINT('Ctrl Pts',(17.1330063266914,70.0889367099268,14.0601111115353));
#58435=CARTESIAN_POINT('Ctrl Pts',(17.0085008916726,71.2775260840903,15.0934154976583));
#58436=CARTESIAN_POINT('Ctrl Pts',(16.8839954566538,72.795440747498,14.6734182044602));
#58437=CARTESIAN_POINT('Ctrl Pts',(16.7594900216351,73.2838246768945,13.1761060159259));
#58438=CARTESIAN_POINT('Ctrl Pts',(16.6349845866163,72.3054705241918,11.9418913654007));
#58439=CARTESIAN_POINT('Ctrl Pts',(16.5104791515975,70.7362130544855,12.0756585083241));
#58440=CARTESIAN_POINT('Ctrl Pts',(16.3859737165788,69.9808710114968,13.4576574408253));
#58441=CARTESIAN_POINT('Ctrl Pts',(16.26146828156,70.715635950286,14.8507055841594));
#58442=CARTESIAN_POINT('Ctrl Pts',(16.1369628465412,72.2827372007522,15.0077289742842));
#58443=CARTESIAN_POINT('Ctrl Pts',(16.0124574115224,73.2792862715224,13.7881583185323));
#58444=CARTESIAN_POINT('Ctrl Pts',(15.8879519765037,72.8131601304144,12.2837684017033));
#58445=CARTESIAN_POINT('Ctrl Pts',(15.7634465414849,71.3016405749555,11.8413076972089));
#58446=CARTESIAN_POINT('Ctrl Pts',(15.6389411064661,70.0978588590303,12.8568725743605));
#58447=CARTESIAN_POINT('Ctrl Pts',(15.5144356714473,70.2794548701458,14.4213166396355));
#58448=CARTESIAN_POINT('Ctrl Pts',(15.3899302364286,71.6838624818643,15.1341304277197));
#58449=CARTESIAN_POINT('Ctrl Pts',(15.2654248014098,73.0538368046712,14.3571936751363));
#58450=CARTESIAN_POINT('Ctrl Pts',(15.140919366391,73.1629634870506,12.7860308639648));
#58451=CARTESIAN_POINT('Ctrl Pts',(15.0164139313723,71.913543523565,11.8271642361628));
#58452=CARTESIAN_POINT('Ctrl Pts',(14.8919084963535,70.4240883638431,12.3389875454574));
#58453=CARTESIAN_POINT('Ctrl Pts',(14.7674030613347,70.0279456674279,13.8633011079927));
#58454=CARTESIAN_POINT('Ctrl Pts',(14.6428976263159,71.0798107346226,15.0355391371328));
#58455=CARTESIAN_POINT('Ctrl Pts',(14.5183921912972,72.6379113282863,14.8062616036466));
#58456=CARTESIAN_POINT('Ctrl Pts',(14.3938867562784,73.3076811621513,13.3807982389934));
#58457=CARTESIAN_POINT('Ctrl Pts',(14.2693813212596,72.4889933638302,12.0350829232256));
#58458=CARTESIAN_POINT('Ctrl Pts',(14.1448758862409,70.9158517355042,11.9741407086008));
#58459=CARTESIAN_POINT('Ctrl Pts',(14.0203704512221,69.9942927747077,13.2518609484195));
#58460=CARTESIAN_POINT('Ctrl Pts',(13.8958650162033,70.5539557793127,14.7257828643058));
#58461=CARTESIAN_POINT('Ctrl Pts',(13.8128613928575,71.5734599327894,14.956586533498));
#58462=CARTESIAN_POINT('Ctrl Pts',(13.7713595811846,72.0212688357496,14.833105713704));
#58463=CARTESIAN_POINT('Ctrl Pts',(19.7877505219048,72.6384078513241,12.6818370233485));
#58464=CARTESIAN_POINT('Ctrl Pts',(19.7462379144259,72.3794178037539,12.3555216261791));
#58465=CARTESIAN_POINT('Ctrl Pts',(19.6632234952739,71.5189853818442,11.983533776499));
#58466=CARTESIAN_POINT('Ctrl Pts',(19.5387072644491,70.3343949062631,12.7551044951164));
#58467=CARTESIAN_POINT('Ctrl Pts',(19.4142018294303,70.3262888641596,14.1675796034986));
#58468=CARTESIAN_POINT('Ctrl Pts',(19.2896963944115,71.4977306447218,14.9550957041578));
#58469=CARTESIAN_POINT('Ctrl Pts',(19.1651909593927,72.8020197752382,14.4133701280415));
#58470=CARTESIAN_POINT('Ctrl Pts',(19.040685524374,73.0705694341706,13.0270131594774));
#58471=CARTESIAN_POINT('Ctrl Pts',(18.9161800893552,72.063445977119,12.0372796911963));
#58472=CARTESIAN_POINT('Ctrl Pts',(18.7916746543364,70.6820060883847,12.3301076943952));
#58473=CARTESIAN_POINT('Ctrl Pts',(18.6671692193177,70.1630458226657,13.6433948901071));
#58474=CARTESIAN_POINT('Ctrl Pts',(18.5426637842989,70.9710890574806,14.8014502359854));
#58475=CARTESIAN_POINT('Ctrl Pts',(18.4181583492801,72.3827927847929,14.7675780533616));
#58476=CARTESIAN_POINT('Ctrl Pts',(18.2936529142613,73.1343689543444,13.5720963304433));
#58477=CARTESIAN_POINT('Ctrl Pts',(18.1691474792426,72.5530038091715,12.2852174808017));
#58478=CARTESIAN_POINT('Ctrl Pts',(18.0446420442238,71.1591394288216,12.058970251175));
#58479=CARTESIAN_POINT('Ctrl Pts',(17.920136609205,70.200582055833,13.0958945307951));
#58480=CARTESIAN_POINT('Ctrl Pts',(17.7956311741862,70.535443365333,14.4677225734024));
#58481=CARTESIAN_POINT('Ctrl Pts',(17.6711257391675,71.8639517380003,14.9463770439872));
#58482=CARTESIAN_POINT('Ctrl Pts',(17.5466203041487,72.9968098248767,14.1033604603431));
#58483=CARTESIAN_POINT('Ctrl Pts',(17.4221148691299,72.9198691127078,12.6933517514775));
#58484=CARTESIAN_POINT('Ctrl Pts',(17.2976094341112,71.7020078367154,11.9786081775955));
#58485=CARTESIAN_POINT('Ctrl Pts',(17.1731039990924,70.4334705306209,12.5989770544976));
#58486=CARTESIAN_POINT('Ctrl Pts',(17.0485985640736,70.2498675063742,13.9990964690587));
#58487=CARTESIAN_POINT('Ctrl Pts',(16.9240931290549,71.3155624725212,14.9255621658968));
#58488=CARTESIAN_POINT('Ctrl Pts',(16.7995876940361,72.6765320815356,14.5489905669191));
#58489=CARTESIAN_POINT('Ctrl Pts',(16.6750822590173,73.1144194683981,13.2064932362542));
#58490=CARTESIAN_POINT('Ctrl Pts',(16.5505768239985,72.2372224159023,12.0998904272434));
#58491=CARTESIAN_POINT('Ctrl Pts',(16.4260713889798,70.8302185991034,12.219826692827));
#58492=CARTESIAN_POINT('Ctrl Pts',(16.301565953961,70.152975279897,13.4589336019084));
#58493=CARTESIAN_POINT('Ctrl Pts',(16.1770605189422,70.8117690682227,14.7079472867197));
#58494=CARTESIAN_POINT('Ctrl Pts',(16.0525550839235,72.21683960845,14.8487352157226));
#58495=CARTESIAN_POINT('Ctrl Pts',(15.9280496489047,73.11035031225,13.7552622830624));
#58496=CARTESIAN_POINT('Ctrl Pts',(15.8035442138859,72.6924193657298,12.4064190270683));
#58497=CARTESIAN_POINT('Ctrl Pts',(15.6790387788671,71.3371836413492,12.009706625168));
#58498=CARTESIAN_POINT('Ctrl Pts',(15.5545333438484,70.2578671482972,12.9202669926942));
#58499=CARTESIAN_POINT('Ctrl Pts',(15.4300279088296,70.4206870078087,14.322955087862));
#58500=CARTESIAN_POINT('Ctrl Pts',(15.3055224738108,71.679885646767,14.962067368582));
#58501=CARTESIAN_POINT('Ctrl Pts',(15.181017038792,72.9082112327946,14.2654621285887));
#58502=CARTESIAN_POINT('Ctrl Pts',(15.0565116037733,73.0060547425988,12.8567499734418));
#58503=CARTESIAN_POINT('Ctrl Pts',(14.9320061687545,71.8858187766437,11.9970255297717));
#58504=CARTESIAN_POINT('Ctrl Pts',(14.8075007337357,70.5503660959109,12.4559287777128));
#58505=CARTESIAN_POINT('Ctrl Pts',(14.6829952987169,70.1951826434738,13.8226356705509));
#58506=CARTESIAN_POINT('Ctrl Pts',(14.5584898636982,71.1382899364899,14.8736699418776));
#58507=CARTESIAN_POINT('Ctrl Pts',(14.4339844286794,72.5352904444127,14.6680985994122));
#58508=CARTESIAN_POINT('Ctrl Pts',(14.3094789936606,73.1358093081533,13.3900212708084));
#58509=CARTESIAN_POINT('Ctrl Pts',(14.1849735586419,72.4017698791616,12.1834464275074));
#58510=CARTESIAN_POINT('Ctrl Pts',(14.0604681236231,70.9912835070088,12.1288053439144));
#58511=CARTESIAN_POINT('Ctrl Pts',(13.9359626886043,70.165009297533,13.2744154741389));
#58512=CARTESIAN_POINT('Ctrl Pts',(13.8114572535856,70.6668058470485,14.5959409735227));
#58513=CARTESIAN_POINT('Ctrl Pts',(13.7284536302397,71.5808981887293,14.8028806566234));
#58514=CARTESIAN_POINT('Ctrl Pts',(13.6869518185668,71.9824058111716,14.6921671579748));
#58515=CARTESIAN_POINT('Ctrl Pts',(19.789,70.1379689624582,12.6747475226976));
#58516=CARTESIAN_POINT('Ctrl Pts',(19.789,70.1415722204682,12.668027089162));
#58517=CARTESIAN_POINT('Ctrl Pts',(19.789,70.1451754784782,12.6613066556264));
#58518=CARTESIAN_POINT('Ctrl Pts',(19.789,70.1487787364881,12.6545862220908));
#58519=CARTESIAN_POINT('Origin',(19.789,71.6454,13.47));
#58520=CARTESIAN_POINT('',(19.939,71.6454,15.32434));
#58521=CARTESIAN_POINT('Origin',(19.939,71.6454,13.47));
#58522=CARTESIAN_POINT('Origin',(19.789,71.6454,15.32434));
#58523=CARTESIAN_POINT('Origin',(19.939,71.6454,13.47));
#58524=CARTESIAN_POINT('',(19.939,71.6454,16.3402));
#58525=CARTESIAN_POINT('Origin',(19.939,71.6454,13.47));
#58526=CARTESIAN_POINT('Origin',(13.764,71.6454,13.47));
#58527=CARTESIAN_POINT('',(13.589,71.6454,14.82434));
#58528=CARTESIAN_POINT('',(13.764,71.6454,14.99934));
#58529=CARTESIAN_POINT('Origin',(13.589,71.6454,13.47));
#58530=CARTESIAN_POINT('Origin',(13.589,71.6454,13.47));
#58531=CARTESIAN_POINT('Origin',(23.4442,74.795221247026,13.8629302123578));
#58532=CARTESIAN_POINT('',(20.539,74.4795530928687,13.9234581415991));
#58533=CARTESIAN_POINT('',(23.1442,74.4795530928687,13.9234581415991));
#58534=CARTESIAN_POINT('',(19.939,74.4795530928687,13.9234581415991));
#58535=CARTESIAN_POINT('',(20.539,74.3538182823342,13.9475672182196));
#58536=CARTESIAN_POINT('',(20.539,74.3538182823342,13.9475672182196));
#58537=CARTESIAN_POINT('',(23.2642,74.3538182823342,13.9475672182196));
#58538=CARTESIAN_POINT('',(23.4442,74.3538182823342,13.9475672182196));
#58539=CARTESIAN_POINT('Ctrl Pts',(23.1442,74.4795530928687,13.9234581415991));
#58540=CARTESIAN_POINT('Ctrl Pts',(23.2056581248801,74.4153434186117,13.935770053868));
#58541=CARTESIAN_POINT('Ctrl Pts',(23.2642,74.3538182823342,13.9475672182196));
#58542=CARTESIAN_POINT('Origin',(23.4442,74.3538182823342,13.9475672182196));
#58543=CARTESIAN_POINT('',(23.1442,74.4637245661282,14.0132261775339));
#58544=CARTESIAN_POINT('',(20.539,74.4637245661282,14.0132261775339));
#58545=CARTESIAN_POINT('',(19.939,74.4637245661282,14.0132261775339));
#58546=CARTESIAN_POINT('Ctrl Pts',(23.2642,74.3538182823342,13.9475672182196));
#58547=CARTESIAN_POINT('Ctrl Pts',(23.2056581248809,74.4075981310439,13.9796957624344));
#58548=CARTESIAN_POINT('Ctrl Pts',(23.1442,74.4637245661282,14.0132261775339));
#58549=CARTESIAN_POINT('',(20.539,74.7396538301726,14.1780686933217));
#58550=CARTESIAN_POINT('Origin',(20.539,74.5606279104667,13.9840333355296));
#58551=CARTESIAN_POINT('Origin',(20.539,71.6454,13.47));
#58552=CARTESIAN_POINT('Origin',(23.2942,71.6454,13.47));
#58553=CARTESIAN_POINT('',(23.2642,71.6454,16.2202));
#58554=CARTESIAN_POINT('',(23.1442,71.5998235737076,16.3398381190176));
#58555=CARTESIAN_POINT('Ctrl Pts',(23.2642,71.6454,16.2202));
#58556=CARTESIAN_POINT('Ctrl Pts',(23.2056581248805,71.6230983332878,16.2787418751195));
#58557=CARTESIAN_POINT('Ctrl Pts',(23.1442,71.5998235737076,16.3398381190176));
#58558=CARTESIAN_POINT('',(23.1442,71.1919418584009,16.3041530928687));
#58559=CARTESIAN_POINT('Origin',(23.1442,71.6454,13.47));
#58560=CARTESIAN_POINT('',(23.2642,71.1678327817804,16.1784182823342));
#58561=CARTESIAN_POINT('Ctrl Pts',(23.1442,71.1919418584009,16.3041530928687));
#58562=CARTESIAN_POINT('Ctrl Pts',(23.2056581248803,71.179629946132,16.2399434186114));
#58563=CARTESIAN_POINT('Ctrl Pts',(23.2642,71.1678327817804,16.1784182823342));
#58564=CARTESIAN_POINT('',(23.1442,71.1021738224661,16.2883245661282));
#58565=CARTESIAN_POINT('Ctrl Pts',(23.2642,71.1678327817804,16.1784182823342));
#58566=CARTESIAN_POINT('Ctrl Pts',(23.2056581248806,71.1357042375654,16.2321981310442));
#58567=CARTESIAN_POINT('Ctrl Pts',(23.1442,71.1021738224661,16.2883245661282));
#58568=CARTESIAN_POINT('',(23.1442,70.7066853866809,16.1823537591437));
#58569=CARTESIAN_POINT('Origin',(23.1442,71.6454,13.47));
#58570=CARTESIAN_POINT('',(23.2642,70.7047762018258,16.0543426456854));
#58571=CARTESIAN_POINT('Ctrl Pts',(23.1442,70.7066853866809,16.1823537591438));
#58572=CARTESIAN_POINT('Ctrl Pts',(23.2056581248804,70.7057104129475,16.1169816329876));
#58573=CARTESIAN_POINT('Ctrl Pts',(23.2642,70.7047762018258,16.0543426456854));
#58574=CARTESIAN_POINT('',(23.1442,70.6210297237434,16.1511776474381));
#58575=CARTESIAN_POINT('Ctrl Pts',(23.2642,70.7047762018258,16.0543426456854));
#58576=CARTESIAN_POINT('Ctrl Pts',(23.2056581248808,70.6637969896664,16.1017263944966));
#58577=CARTESIAN_POINT('Ctrl Pts',(23.1442,70.6210297237434,16.1511776474381));
#58578=CARTESIAN_POINT('',(23.1442,70.2499512834741,15.9781409289644));
#58579=CARTESIAN_POINT('Origin',(23.1442,71.6454,13.47));
#58580=CARTESIAN_POINT('',(23.2642,70.2703,15.851743065488));
#58581=CARTESIAN_POINT('Ctrl Pts',(23.1442,70.2499512834741,15.9781409289644));
#58582=CARTESIAN_POINT('Ctrl Pts',(23.2056581248808,70.2603428723598,15.9135926498824));
#58583=CARTESIAN_POINT('Ctrl Pts',(23.2642,70.2703,15.851743065488));
#58584=CARTESIAN_POINT('',(23.1442,70.1710105975083,15.932564502672));
#58585=CARTESIAN_POINT('Ctrl Pts',(23.2642,70.2703,15.851743065488));
#58586=CARTESIAN_POINT('Ctrl Pts',(23.2056581248807,70.2217152525209,15.8912909831704));
#58587=CARTESIAN_POINT('Ctrl Pts',(23.1442,70.1710105975083,15.932564502672));
#58588=CARTESIAN_POINT('',(23.1442,69.8356171833879,15.697719505839));
#58589=CARTESIAN_POINT('Origin',(23.1442,71.6454,13.47));
#58590=CARTESIAN_POINT('',(23.2642,69.8776055158401,15.5767754274658));
#58591=CARTESIAN_POINT('Ctrl Pts',(23.1442,69.8356171833879,15.697719505839));
#58592=CARTESIAN_POINT('Ctrl Pts',(23.2056581248802,69.8570595917225,15.6359563406292));
#58593=CARTESIAN_POINT('Ctrl Pts',(23.2642,69.8776055158401,15.5767754274658));
#58594=CARTESIAN_POINT('',(23.1442,69.7657900471908,15.6391275816099));
#58595=CARTESIAN_POINT('Ctrl Pts',(23.2642,69.8776055158401,15.5767754274658));
#58596=CARTESIAN_POINT('Ctrl Pts',(23.2056581248808,69.8228914560086,15.6072858705527));
#58597=CARTESIAN_POINT('Ctrl Pts',(23.1442,69.7657900471908,15.6391275816099));
#58598=CARTESIAN_POINT('',(23.1442,69.4762724183901,15.3496099528092));
#58599=CARTESIAN_POINT('Origin',(23.1442,71.6454,13.47));
#58600=CARTESIAN_POINT('',(23.2642,69.5386245725342,15.2377944841599));
#58601=CARTESIAN_POINT('Ctrl Pts',(23.1442,69.4762724183901,15.3496099528092));
#58602=CARTESIAN_POINT('Ctrl Pts',(23.20565812488,69.5081141294468,15.2925085439922));
#58603=CARTESIAN_POINT('Ctrl Pts',(23.2642,69.5386245725342,15.2377944841599));
#58604=CARTESIAN_POINT('',(23.1442,69.417680494161,15.2797828166121));
#58605=CARTESIAN_POINT('Ctrl Pts',(23.2642,69.5386245725342,15.2377944841599));
#58606=CARTESIAN_POINT('Ctrl Pts',(23.2056581248812,69.4794436593718,15.2583404082771));
#58607=CARTESIAN_POINT('Ctrl Pts',(23.1442,69.417680494161,15.2797828166121));
#58608=CARTESIAN_POINT('',(23.1442,69.182835497328,14.9443894024917));
#58609=CARTESIAN_POINT('Origin',(23.1442,71.6454,13.47));
#58610=CARTESIAN_POINT('',(23.2642,69.263656934512,14.8451));
#58611=CARTESIAN_POINT('Ctrl Pts',(23.1442,69.182835497328,14.9443894024917));
#58612=CARTESIAN_POINT('Ctrl Pts',(23.2056581248801,69.2241090168292,14.8936847474796));
#58613=CARTESIAN_POINT('Ctrl Pts',(23.2642,69.263656934512,14.8451));
#58614=CARTESIAN_POINT('',(23.1442,69.1372590710356,14.8654487165258));
#58615=CARTESIAN_POINT('Ctrl Pts',(23.2642,69.263656934512,14.8451));
#58616=CARTESIAN_POINT('Ctrl Pts',(23.2056581248811,69.2018073501179,14.8550571276402));
#58617=CARTESIAN_POINT('Ctrl Pts',(23.1442,69.1372590710356,14.8654487165258));
#58618=CARTESIAN_POINT('',(23.1442,68.9642223525619,14.4943702762566));
#58619=CARTESIAN_POINT('Origin',(23.1442,71.6454,13.47));
#58620=CARTESIAN_POINT('',(23.2642,69.0610573543146,14.4106237981742));
#58621=CARTESIAN_POINT('Ctrl Pts',(23.1442,68.9642223525618,14.4943702762566));
#58622=CARTESIAN_POINT('Ctrl Pts',(23.2056581248796,69.0136736055024,14.4516030103345));
#58623=CARTESIAN_POINT('Ctrl Pts',(23.2642,69.0610573543146,14.4106237981742));
#58624=CARTESIAN_POINT('',(23.1442,68.9330462408563,14.4087146133191));
#58625=CARTESIAN_POINT('Ctrl Pts',(23.2642,69.0610573543146,14.4106237981742));
#58626=CARTESIAN_POINT('Ctrl Pts',(23.2056581248797,68.9984183670117,14.4096895870525));
#58627=CARTESIAN_POINT('Ctrl Pts',(23.1442,68.9330462408562,14.4087146133191));
#58628=CARTESIAN_POINT('',(23.1442,68.8270754338718,14.0132261775338));
#58629=CARTESIAN_POINT('Origin',(23.1442,71.6454,13.47));
#58630=CARTESIAN_POINT('',(23.2642,68.9369817176658,13.9475672182196));
#58631=CARTESIAN_POINT('Ctrl Pts',(23.1442,68.8270754338717,14.0132261775338));
#58632=CARTESIAN_POINT('Ctrl Pts',(23.2056581248802,68.8832018689555,13.9796957624347));
#58633=CARTESIAN_POINT('Ctrl Pts',(23.2642,68.9369817176658,13.9475672182196));
#58634=CARTESIAN_POINT('',(23.1442,68.8112469071312,13.9234581415991));
#58635=CARTESIAN_POINT('Ctrl Pts',(23.2642,68.9369817176658,13.9475672182196));
#58636=CARTESIAN_POINT('Ctrl Pts',(23.2056581248804,68.8754565813886,13.935770053868));
#58637=CARTESIAN_POINT('Ctrl Pts',(23.1442,68.8112469071312,13.9234581415991));
#58638=CARTESIAN_POINT('',(23.1442,68.7755618809824,13.5155764262924));
#58639=CARTESIAN_POINT('Origin',(23.1442,71.6454,13.47));
#58640=CARTESIAN_POINT('',(23.2642,68.8952,13.47));
#58641=CARTESIAN_POINT('Ctrl Pts',(23.1442,68.7755618809824,13.5155764262924));
#58642=CARTESIAN_POINT('Ctrl Pts',(23.2056581248812,68.8366581248812,13.4923016667119));
#58643=CARTESIAN_POINT('Ctrl Pts',(23.2642,68.8952,13.47));
#58644=CARTESIAN_POINT('',(23.1442,68.7755618809824,13.4244235737076));
#58645=CARTESIAN_POINT('Ctrl Pts',(23.2642,68.8952,13.47));
#58646=CARTESIAN_POINT('Ctrl Pts',(23.2056581248805,68.8366581248805,13.4476983332878));
#58647=CARTESIAN_POINT('Ctrl Pts',(23.1442,68.7755618809824,13.4244235737076));
#58648=CARTESIAN_POINT('',(23.1442,68.8112469071312,13.0165418584009));
#58649=CARTESIAN_POINT('Origin',(23.1442,71.6454,13.47));
#58650=CARTESIAN_POINT('',(23.2642,68.9369817176658,12.9924327817804));
#58651=CARTESIAN_POINT('Ctrl Pts',(23.1442,68.8112469071312,13.0165418584009));
#58652=CARTESIAN_POINT('Ctrl Pts',(23.20565812488,68.8754565813883,13.0042299461321));
#58653=CARTESIAN_POINT('Ctrl Pts',(23.2642,68.9369817176658,12.9924327817804));
#58654=CARTESIAN_POINT('',(23.1442,68.8270754338718,12.9267738224661));
#58655=CARTESIAN_POINT('Ctrl Pts',(23.2642,68.9369817176658,12.9924327817804));
#58656=CARTESIAN_POINT('Ctrl Pts',(23.2056581248801,68.8832018689554,12.9603042375652));
#58657=CARTESIAN_POINT('Ctrl Pts',(23.1442,68.8270754338718,12.9267738224661));
#58658=CARTESIAN_POINT('',(23.1442,68.9330462408563,12.5312853866809));
#58659=CARTESIAN_POINT('Origin',(23.1442,71.6454,13.47));
#58660=CARTESIAN_POINT('',(23.2642,69.0610573543146,12.5293762018258));
#58661=CARTESIAN_POINT('Ctrl Pts',(23.1442,68.9330462408562,12.5312853866809));
#58662=CARTESIAN_POINT('Ctrl Pts',(23.2056581248799,68.9984183670118,12.5303104129475));
#58663=CARTESIAN_POINT('Ctrl Pts',(23.2642,69.0610573543146,12.5293762018258));
#58664=CARTESIAN_POINT('',(23.1442,68.9642223525618,12.4456297237434));
#58665=CARTESIAN_POINT('Ctrl Pts',(23.2642,69.0610573543146,12.5293762018258));
#58666=CARTESIAN_POINT('Ctrl Pts',(23.2056581248799,69.0136736055026,12.4883969896657));
#58667=CARTESIAN_POINT('Ctrl Pts',(23.1442,68.9642223525618,12.4456297237434));
#58668=CARTESIAN_POINT('',(23.1442,69.1372590710356,12.0745512834741));
#58669=CARTESIAN_POINT('Origin',(23.1442,71.6454,13.47));
#58670=CARTESIAN_POINT('',(23.2642,69.263656934512,12.0949));
#58671=CARTESIAN_POINT('Ctrl Pts',(23.1442,69.1372590710356,12.0745512834741));
#58672=CARTESIAN_POINT('Ctrl Pts',(23.2056581248798,69.2018073501165,12.0849428723596));
#58673=CARTESIAN_POINT('Ctrl Pts',(23.2642,69.263656934512,12.0949));
#58674=CARTESIAN_POINT('',(23.1442,69.182835497328,11.9956105975083));
#58675=CARTESIAN_POINT('Ctrl Pts',(23.2642,69.263656934512,12.0949));
#58676=CARTESIAN_POINT('Ctrl Pts',(23.2056581248803,69.2241090168293,12.0463152525206));
#58677=CARTESIAN_POINT('Ctrl Pts',(23.1442,69.182835497328,11.9956105975083));
#58678=CARTESIAN_POINT('',(23.1442,69.417680494161,11.6602171833879));
#58679=CARTESIAN_POINT('Origin',(23.1442,71.6454,13.47));
#58680=CARTESIAN_POINT('',(23.2642,69.5386245725342,11.7022055158401));
#58681=CARTESIAN_POINT('Ctrl Pts',(23.1442,69.417680494161,11.6602171833879));
#58682=CARTESIAN_POINT('Ctrl Pts',(23.2056581248803,69.479443659371,11.6816595917226));
#58683=CARTESIAN_POINT('Ctrl Pts',(23.2642,69.5386245725342,11.7022055158401));
#58684=CARTESIAN_POINT('',(23.1442,69.4762724183901,11.5903900471908));
#58685=CARTESIAN_POINT('Ctrl Pts',(23.2642,69.5386245725342,11.7022055158401));
#58686=CARTESIAN_POINT('Ctrl Pts',(23.2056581248804,69.508114129447,11.6474914560082));
#58687=CARTESIAN_POINT('Ctrl Pts',(23.1442,69.4762724183901,11.5903900471908));
#58688=CARTESIAN_POINT('',(23.1442,69.7657900471908,11.3008724183901));
#58689=CARTESIAN_POINT('Origin',(23.1442,71.6454,13.47));
#58690=CARTESIAN_POINT('',(23.2642,69.8776055158401,11.3632245725342));
#58691=CARTESIAN_POINT('Ctrl Pts',(23.1442,69.7657900471908,11.3008724183901));
#58692=CARTESIAN_POINT('Ctrl Pts',(23.2056581248811,69.8228914560089,11.3327141294474));
#58693=CARTESIAN_POINT('Ctrl Pts',(23.2642,69.8776055158401,11.3632245725342));
#58694=CARTESIAN_POINT('',(23.1442,69.8356171833879,11.242280494161));
#58695=CARTESIAN_POINT('Ctrl Pts',(23.2642,69.8776055158401,11.3632245725342));
#58696=CARTESIAN_POINT('Ctrl Pts',(23.2056581248796,69.8570595917223,11.3040436593702));
#58697=CARTESIAN_POINT('Ctrl Pts',(23.1442,69.8356171833879,11.242280494161));
#58698=CARTESIAN_POINT('',(23.1442,70.1710105975083,11.007435497328));
#58699=CARTESIAN_POINT('Origin',(23.1442,71.6454,13.47));
#58700=CARTESIAN_POINT('',(23.2642,70.2703,11.0882569345121));
#58701=CARTESIAN_POINT('Ctrl Pts',(23.1442,70.1710105975083,11.007435497328));
#58702=CARTESIAN_POINT('Ctrl Pts',(23.2056581248807,70.2217152525209,11.0487090168296));
#58703=CARTESIAN_POINT('Ctrl Pts',(23.2642,70.2703,11.0882569345121));
#58704=CARTESIAN_POINT('',(23.1442,70.2499512834741,10.9618590710356));
#58705=CARTESIAN_POINT('Ctrl Pts',(23.2642,70.2703,11.0882569345121));
#58706=CARTESIAN_POINT('Ctrl Pts',(23.205658124881,70.2603428723598,11.0264073501178));
#58707=CARTESIAN_POINT('Ctrl Pts',(23.1442,70.2499512834741,10.9618590710356));
#58708=CARTESIAN_POINT('',(23.1442,70.6210297237434,10.7888223525619));
#58709=CARTESIAN_POINT('Origin',(23.1442,71.6454,13.47));
#58710=CARTESIAN_POINT('',(23.2642,70.7047762018258,10.8856573543146));
#58711=CARTESIAN_POINT('Ctrl Pts',(23.1442,70.6210297237434,10.7888223525619));
#58712=CARTESIAN_POINT('Ctrl Pts',(23.2056581248802,70.6637969896659,10.8382736055029));
#58713=CARTESIAN_POINT('Ctrl Pts',(23.2642,70.7047762018258,10.8856573543146));
#58714=CARTESIAN_POINT('',(23.1442,70.7066853866809,10.7576462408563));
#58715=CARTESIAN_POINT('Ctrl Pts',(23.2642,70.7047762018258,10.8856573543146));
#58716=CARTESIAN_POINT('Ctrl Pts',(23.2056581248805,70.7057104129475,10.8230183670125));
#58717=CARTESIAN_POINT('Ctrl Pts',(23.1442,70.7066853866809,10.7576462408562));
#58718=CARTESIAN_POINT('',(23.1442,71.1021738224661,10.6516754338718));
#58719=CARTESIAN_POINT('Origin',(23.1442,71.6454,13.47));
#58720=CARTESIAN_POINT('',(23.2642,71.1678327817804,10.7615817176658));
#58721=CARTESIAN_POINT('Ctrl Pts',(23.1442,71.1021738224662,10.6516754338718));
#58722=CARTESIAN_POINT('Ctrl Pts',(23.2056581248805,71.1357042375654,10.7078018689558));
#58723=CARTESIAN_POINT('Ctrl Pts',(23.2642,71.1678327817804,10.7615817176658));
#58724=CARTESIAN_POINT('',(23.1442,71.1919418584009,10.6358469071313));
#58725=CARTESIAN_POINT('Ctrl Pts',(23.2642,71.1678327817804,10.7615817176658));
#58726=CARTESIAN_POINT('Ctrl Pts',(23.2056581248808,71.1796299461319,10.7000565813891));
#58727=CARTESIAN_POINT('Ctrl Pts',(23.1442,71.1919418584009,10.6358469071313));
#58728=CARTESIAN_POINT('',(23.1442,71.5998235737076,10.6001618809824));
#58729=CARTESIAN_POINT('Origin',(23.1442,71.6454,13.47));
#58730=CARTESIAN_POINT('',(23.2642,71.6454,10.7198));
#58731=CARTESIAN_POINT('Ctrl Pts',(23.1442,71.5998235737076,10.6001618809824));
#58732=CARTESIAN_POINT('Ctrl Pts',(23.2056581248805,71.6230983332878,10.6612581248805));
#58733=CARTESIAN_POINT('Ctrl Pts',(23.2642,71.6454,10.7198));
#58734=CARTESIAN_POINT('',(23.1442,71.6909764262924,10.6001618809824));
#58735=CARTESIAN_POINT('Ctrl Pts',(23.2642,71.6454,10.7198));
#58736=CARTESIAN_POINT('Ctrl Pts',(23.2056581248811,71.667701666712,10.6612581248811));
#58737=CARTESIAN_POINT('Ctrl Pts',(23.1442,71.6909764262924,10.6001618809824));
#58738=CARTESIAN_POINT('',(23.1442,72.0988581415992,10.6358469071313));
#58739=CARTESIAN_POINT('Origin',(23.1442,71.6454,13.47));
#58740=CARTESIAN_POINT('',(23.2642,72.1229672182196,10.7615817176658));
#58741=CARTESIAN_POINT('Ctrl Pts',(23.1442,72.0988581415992,10.6358469071313));
#58742=CARTESIAN_POINT('Ctrl Pts',(23.2056581248808,72.1111700538681,10.7000565813891));
#58743=CARTESIAN_POINT('Ctrl Pts',(23.2642,72.1229672182196,10.7615817176658));
#58744=CARTESIAN_POINT('',(23.1442,72.1886261775339,10.6516754338718));
#58745=CARTESIAN_POINT('Ctrl Pts',(23.2642,72.1229672182196,10.7615817176658));
#58746=CARTESIAN_POINT('Ctrl Pts',(23.2056581248801,72.1550957624348,10.7078018689554));
#58747=CARTESIAN_POINT('Ctrl Pts',(23.1442,72.1886261775339,10.6516754338718));
#58748=CARTESIAN_POINT('',(23.1442,72.5841146133191,10.7576462408563));
#58749=CARTESIAN_POINT('Origin',(23.1442,71.6454,13.47));
#58750=CARTESIAN_POINT('',(23.2642,72.5860237981743,10.8856573543146));
#58751=CARTESIAN_POINT('Ctrl Pts',(23.1442,72.5841146133191,10.7576462408563));
#58752=CARTESIAN_POINT('Ctrl Pts',(23.2056581248803,72.5850895870525,10.8230183670123));
#58753=CARTESIAN_POINT('Ctrl Pts',(23.2642,72.5860237981742,10.8856573543146));
#58754=CARTESIAN_POINT('',(23.1442,72.6697702762566,10.7888223525619));
#58755=CARTESIAN_POINT('Ctrl Pts',(23.2642,72.5860237981743,10.8856573543146));
#58756=CARTESIAN_POINT('Ctrl Pts',(23.2056581248806,72.6270030103338,10.8382736055032));
#58757=CARTESIAN_POINT('Ctrl Pts',(23.1442,72.6697702762566,10.7888223525619));
#58758=CARTESIAN_POINT('',(23.1442,73.0408487165258,10.9618590710356));
#58759=CARTESIAN_POINT('Origin',(23.1442,71.6454,13.47));
#58760=CARTESIAN_POINT('',(23.2642,73.0205,11.088256934512));
#58761=CARTESIAN_POINT('Ctrl Pts',(23.1442,73.0408487165258,10.9618590710356));
#58762=CARTESIAN_POINT('Ctrl Pts',(23.2056581248806,73.0304571276402,11.0264073501174));
#58763=CARTESIAN_POINT('Ctrl Pts',(23.2642,73.0205,11.088256934512));
#58764=CARTESIAN_POINT('',(23.1442,73.1197894024917,11.007435497328));
#58765=CARTESIAN_POINT('Ctrl Pts',(23.2642,73.0205,11.088256934512));
#58766=CARTESIAN_POINT('Ctrl Pts',(23.2056581248807,73.0690847474791,11.0487090168296));
#58767=CARTESIAN_POINT('Ctrl Pts',(23.1442,73.1197894024917,11.007435497328));
#58768=CARTESIAN_POINT('',(23.1442,73.4551828166121,11.242280494161));
#58769=CARTESIAN_POINT('Origin',(23.1442,71.6454,13.47));
#58770=CARTESIAN_POINT('',(23.2642,73.4131944841599,11.3632245725342));
#58771=CARTESIAN_POINT('Ctrl Pts',(23.1442,73.4551828166121,11.242280494161));
#58772=CARTESIAN_POINT('Ctrl Pts',(23.2056581248799,73.4337404082776,11.3040436593706));
#58773=CARTESIAN_POINT('Ctrl Pts',(23.2642,73.4131944841599,11.3632245725342));
#58774=CARTESIAN_POINT('',(23.1442,73.5250099528092,11.3008724183901));
#58775=CARTESIAN_POINT('Ctrl Pts',(23.2642,73.4131944841599,11.3632245725342));
#58776=CARTESIAN_POINT('Ctrl Pts',(23.2056581248809,73.4679085439913,11.3327141294473));
#58777=CARTESIAN_POINT('Ctrl Pts',(23.1442,73.5250099528091,11.3008724183901));
#58778=CARTESIAN_POINT('',(23.1442,73.8145275816099,11.5903900471908));
#58779=CARTESIAN_POINT('Origin',(23.1442,71.6454,13.47));
#58780=CARTESIAN_POINT('',(23.2642,73.7521754274658,11.7022055158401));
#58781=CARTESIAN_POINT('Ctrl Pts',(23.1442,73.8145275816099,11.5903900471908));
#58782=CARTESIAN_POINT('Ctrl Pts',(23.2056581248799,73.7826858705532,11.6474914560077));
#58783=CARTESIAN_POINT('Ctrl Pts',(23.2642,73.7521754274658,11.7022055158401));
#58784=CARTESIAN_POINT('',(23.1442,73.873119505839,11.6602171833879));
#58785=CARTESIAN_POINT('Ctrl Pts',(23.2642,73.7521754274658,11.7022055158401));
#58786=CARTESIAN_POINT('Ctrl Pts',(23.2056581248803,73.811356340629,11.6816595917226));
#58787=CARTESIAN_POINT('Ctrl Pts',(23.1442,73.873119505839,11.6602171833879));
#58788=CARTESIAN_POINT('',(23.1442,74.107964502672,11.9956105975083));
#58789=CARTESIAN_POINT('Origin',(23.1442,71.6454,13.47));
#58790=CARTESIAN_POINT('',(23.2642,74.027143065488,12.0949));
#58791=CARTESIAN_POINT('Ctrl Pts',(23.1442,74.107964502672,11.9956105975083));
#58792=CARTESIAN_POINT('Ctrl Pts',(23.20565812488,74.0666909831708,12.0463152525204));
#58793=CARTESIAN_POINT('Ctrl Pts',(23.2642,74.027143065488,12.0949));
#58794=CARTESIAN_POINT('',(23.1442,74.1535409289644,12.0745512834741));
#58795=CARTESIAN_POINT('Ctrl Pts',(23.2642,74.0271430654879,12.0949));
#58796=CARTESIAN_POINT('Ctrl Pts',(23.2056581248806,74.0889926498826,12.0849428723598));
#58797=CARTESIAN_POINT('Ctrl Pts',(23.1442,74.1535409289644,12.0745512834741));
#58798=CARTESIAN_POINT('',(23.1442,74.3265776474381,12.4456297237434));
#58799=CARTESIAN_POINT('Origin',(23.1442,71.6454,13.47));
#58800=CARTESIAN_POINT('',(23.2642,74.2297426456854,12.5293762018257));
#58801=CARTESIAN_POINT('Ctrl Pts',(23.1442,74.3265776474381,12.4456297237434));
#58802=CARTESIAN_POINT('Ctrl Pts',(23.2056581248805,74.2771263944969,12.4883969896661));
#58803=CARTESIAN_POINT('Ctrl Pts',(23.2642,74.2297426456854,12.5293762018257));
#58804=CARTESIAN_POINT('',(23.1442,74.3577537591437,12.5312853866809));
#58805=CARTESIAN_POINT('Ctrl Pts',(23.2642,74.2297426456854,12.5293762018257));
#58806=CARTESIAN_POINT('Ctrl Pts',(23.2056581248808,74.2923816329872,12.5303104129475));
#58807=CARTESIAN_POINT('Ctrl Pts',(23.1442,74.3577537591437,12.5312853866809));
#58808=CARTESIAN_POINT('',(23.1442,74.4637245661282,12.9267738224661));
#58809=CARTESIAN_POINT('Origin',(23.1442,71.6454,13.47));
#58810=CARTESIAN_POINT('',(23.2642,74.3538182823342,12.9924327817804));
#58811=CARTESIAN_POINT('Ctrl Pts',(23.1442,74.4637245661282,12.9267738224661));
#58812=CARTESIAN_POINT('Ctrl Pts',(23.2056581248812,74.4075981310436,12.9603042375658));
#58813=CARTESIAN_POINT('Ctrl Pts',(23.2642,74.3538182823342,12.9924327817804));
#58814=CARTESIAN_POINT('',(23.1442,74.4795530928687,13.0165418584009));
#58815=CARTESIAN_POINT('Ctrl Pts',(23.2642,74.3538182823342,12.9924327817804));
#58816=CARTESIAN_POINT('Ctrl Pts',(23.2056581248806,74.4153434186111,13.0042299461319));
#58817=CARTESIAN_POINT('Ctrl Pts',(23.1442,74.4795530928687,13.0165418584009));
#58818=CARTESIAN_POINT('',(23.1442,74.5152381190176,13.4244235737076));
#58819=CARTESIAN_POINT('Origin',(23.1442,71.6454,13.47));
#58820=CARTESIAN_POINT('',(23.2642,74.3956,13.47));
#58821=CARTESIAN_POINT('Ctrl Pts',(23.1442,74.5152381190176,13.4244235737076));
#58822=CARTESIAN_POINT('Ctrl Pts',(23.2056581248811,74.4541418751189,13.447698333288));
#58823=CARTESIAN_POINT('Ctrl Pts',(23.2642,74.3956,13.47));
#58824=CARTESIAN_POINT('',(23.1442,74.5152381190176,13.5155764262924));
#58825=CARTESIAN_POINT('Ctrl Pts',(23.2642,74.3956,13.47));
#58826=CARTESIAN_POINT('Ctrl Pts',(23.2056581248807,74.4541418751193,13.4923016667121));
#58827=CARTESIAN_POINT('Ctrl Pts',(23.1442,74.5152381190176,13.5155764262924));
#58828=CARTESIAN_POINT('Origin',(23.1442,71.6454,13.47));
#58829=CARTESIAN_POINT('',(23.1442,74.3577537591437,14.4087146133191));
#58830=CARTESIAN_POINT('Origin',(23.1442,71.6454,13.47));
#58831=CARTESIAN_POINT('',(23.2642,74.2297426456854,14.4106237981743));
#58832=CARTESIAN_POINT('Ctrl Pts',(23.1442,74.3577537591437,14.4087146133191));
#58833=CARTESIAN_POINT('Ctrl Pts',(23.2056581248805,74.2923816329875,14.4096895870525));
#58834=CARTESIAN_POINT('Ctrl Pts',(23.2642,74.2297426456854,14.4106237981743));
#58835=CARTESIAN_POINT('',(23.1442,74.3265776474381,14.4943702762566));
#58836=CARTESIAN_POINT('Ctrl Pts',(23.2642,74.2297426456854,14.4106237981743));
#58837=CARTESIAN_POINT('Ctrl Pts',(23.20565812488,74.2771263944972,14.4516030103342));
#58838=CARTESIAN_POINT('Ctrl Pts',(23.1442,74.3265776474381,14.4943702762567));
#58839=CARTESIAN_POINT('',(23.1442,74.1535409289644,14.8654487165258));
#58840=CARTESIAN_POINT('Origin',(23.1442,71.6454,13.47));
#58841=CARTESIAN_POINT('',(23.2642,74.0271430654879,14.8451));
#58842=CARTESIAN_POINT('Ctrl Pts',(23.1442,74.1535409289644,14.8654487165259));
#58843=CARTESIAN_POINT('Ctrl Pts',(23.2056581248803,74.0889926498829,14.8550571276403));
#58844=CARTESIAN_POINT('Ctrl Pts',(23.2642,74.0271430654879,14.8451));
#58845=CARTESIAN_POINT('',(23.1442,74.107964502672,14.9443894024917));
#58846=CARTESIAN_POINT('Ctrl Pts',(23.2642,74.0271430654879,14.8451));
#58847=CARTESIAN_POINT('Ctrl Pts',(23.2056581248802,74.0666909831707,14.8936847474795));
#58848=CARTESIAN_POINT('Ctrl Pts',(23.1442,74.107964502672,14.9443894024917));
#58849=CARTESIAN_POINT('',(23.1442,73.873119505839,15.2797828166121));
#58850=CARTESIAN_POINT('Origin',(23.1442,71.6454,13.47));
#58851=CARTESIAN_POINT('',(23.2642,73.7521754274658,15.2377944841599));
#58852=CARTESIAN_POINT('Ctrl Pts',(23.1442,73.873119505839,15.2797828166121));
#58853=CARTESIAN_POINT('Ctrl Pts',(23.2056581248798,73.8113563406296,15.2583404082776));
#58854=CARTESIAN_POINT('Ctrl Pts',(23.2642,73.7521754274658,15.2377944841599));
#58855=CARTESIAN_POINT('',(23.1442,73.8145275816099,15.3496099528092));
#58856=CARTESIAN_POINT('Ctrl Pts',(23.2642,73.7521754274658,15.2377944841599));
#58857=CARTESIAN_POINT('Ctrl Pts',(23.2056581248795,73.7826858705534,15.2925085439927));
#58858=CARTESIAN_POINT('Ctrl Pts',(23.1442,73.8145275816099,15.3496099528092));
#58859=CARTESIAN_POINT('',(23.1442,73.5250099528092,15.6391275816099));
#58860=CARTESIAN_POINT('Origin',(23.1442,71.6454,13.47));
#58861=CARTESIAN_POINT('',(23.2642,73.4131944841599,15.5767754274658));
#58862=CARTESIAN_POINT('Ctrl Pts',(23.1442,73.5250099528092,15.6391275816099));
#58863=CARTESIAN_POINT('Ctrl Pts',(23.2056581248799,73.4679085439923,15.6072858705533));
#58864=CARTESIAN_POINT('Ctrl Pts',(23.2642,73.4131944841599,15.5767754274658));
#58865=CARTESIAN_POINT('',(23.1442,73.4551828166121,15.697719505839));
#58866=CARTESIAN_POINT('Ctrl Pts',(23.2642,73.4131944841599,15.5767754274658));
#58867=CARTESIAN_POINT('Ctrl Pts',(23.2056581248798,73.4337404082776,15.6359563406295));
#58868=CARTESIAN_POINT('Ctrl Pts',(23.1442,73.4551828166121,15.697719505839));
#58869=CARTESIAN_POINT('',(23.1442,73.1197894024917,15.932564502672));
#58870=CARTESIAN_POINT('Origin',(23.1442,71.6454,13.47));
#58871=CARTESIAN_POINT('',(23.2642,73.0205,15.8517430654879));
#58872=CARTESIAN_POINT('Ctrl Pts',(23.1442,73.1197894024917,15.932564502672));
#58873=CARTESIAN_POINT('Ctrl Pts',(23.2056581248807,73.0690847474791,15.8912909831704));
#58874=CARTESIAN_POINT('Ctrl Pts',(23.2642,73.0205,15.8517430654879));
#58875=CARTESIAN_POINT('',(23.1442,73.0408487165259,15.9781409289644));
#58876=CARTESIAN_POINT('Ctrl Pts',(23.2642,73.0205,15.8517430654879));
#58877=CARTESIAN_POINT('Ctrl Pts',(23.2056581248811,73.0304571276402,15.9135926498821));
#58878=CARTESIAN_POINT('Ctrl Pts',(23.1442,73.0408487165259,15.9781409289644));
#58879=CARTESIAN_POINT('',(23.1442,72.6697702762566,16.1511776474381));
#58880=CARTESIAN_POINT('Origin',(23.1442,71.6454,13.47));
#58881=CARTESIAN_POINT('',(23.2642,72.5860237981742,16.0543426456854));
#58882=CARTESIAN_POINT('Ctrl Pts',(23.1442,72.6697702762566,16.1511776474381));
#58883=CARTESIAN_POINT('Ctrl Pts',(23.2056581248799,72.6270030103342,16.1017263944973));
#58884=CARTESIAN_POINT('Ctrl Pts',(23.2642,72.5860237981742,16.0543426456854));
#58885=CARTESIAN_POINT('',(23.1442,72.5841146133191,16.1823537591437));
#58886=CARTESIAN_POINT('Ctrl Pts',(23.2642,72.5860237981742,16.0543426456854));
#58887=CARTESIAN_POINT('Ctrl Pts',(23.2056581248803,72.5850895870525,16.1169816329877));
#58888=CARTESIAN_POINT('Ctrl Pts',(23.1442,72.5841146133191,16.1823537591438));
#58889=CARTESIAN_POINT('',(23.1442,72.1886261775338,16.2883245661282));
#58890=CARTESIAN_POINT('Origin',(23.1442,71.6454,13.47));
#58891=CARTESIAN_POINT('',(23.2642,72.1229672182196,16.1784182823342));
#58892=CARTESIAN_POINT('Ctrl Pts',(23.1442,72.1886261775338,16.2883245661282));
#58893=CARTESIAN_POINT('Ctrl Pts',(23.2056581248799,72.1550957624349,16.2321981310448));
#58894=CARTESIAN_POINT('Ctrl Pts',(23.2642,72.1229672182196,16.1784182823342));
#58895=CARTESIAN_POINT('',(23.1442,72.0988581415991,16.3041530928687));
#58896=CARTESIAN_POINT('Ctrl Pts',(23.2642,72.1229672182196,16.1784182823342));
#58897=CARTESIAN_POINT('Ctrl Pts',(23.2056581248806,72.1111700538681,16.2399434186111));
#58898=CARTESIAN_POINT('Ctrl Pts',(23.1442,72.0988581415991,16.3041530928687));
#58899=CARTESIAN_POINT('',(23.1442,71.6909764262924,16.3398381190176));
#58900=CARTESIAN_POINT('Origin',(23.1442,71.6454,13.47));
#58901=CARTESIAN_POINT('Ctrl Pts',(23.1442,71.6909764262924,16.3398381190176));
#58902=CARTESIAN_POINT('Ctrl Pts',(23.2056581248802,71.6677016667123,16.2787418751198));
#58903=CARTESIAN_POINT('Ctrl Pts',(23.2642,71.6454,16.2202));
#58904=CARTESIAN_POINT('',(23.4442,71.6454,16.0402));
#58905=CARTESIAN_POINT('',(23.2942,71.6454,16.1902));
#58906=CARTESIAN_POINT('Origin',(23.4442,71.6454,13.47));
#58907=CARTESIAN_POINT('Origin',(23.4442,74.6791367693476,14.4039214390453));
#58908=CARTESIAN_POINT('',(20.539,74.3577537591437,14.4087146133191));
#58909=CARTESIAN_POINT('',(19.939,74.3577537591437,14.4087146133191));
#58910=CARTESIAN_POINT('',(20.539,74.2297426456854,14.4106237981743));
#58911=CARTESIAN_POINT('',(20.539,74.2297426456854,14.4106237981743));
#58912=CARTESIAN_POINT('',(23.4442,74.2297426456854,14.4106237981743));
#58913=CARTESIAN_POINT('Origin',(23.4442,74.2297426456854,14.4106237981743));
#58914=CARTESIAN_POINT('',(20.539,74.3265776474381,14.4943702762566));
#58915=CARTESIAN_POINT('',(19.939,74.3265776474381,14.4943702762566));
#58916=CARTESIAN_POINT('',(20.539,74.5696903234834,14.7046230776968));
#58917=CARTESIAN_POINT('Origin',(20.539,74.4270780960504,14.4824480282726));
#58918=CARTESIAN_POINT('Origin',(20.539,71.6454,13.47));
#58919=CARTESIAN_POINT('Origin',(23.4442,74.4708737350774,14.9165359353945));
#58920=CARTESIAN_POINT('',(20.539,74.1535409289644,14.8654487165258));
#58921=CARTESIAN_POINT('',(19.939,74.1535409289644,14.8654487165258));
#58922=CARTESIAN_POINT('',(20.539,74.0271430654879,14.8451));
#58923=CARTESIAN_POINT('',(20.539,74.0271430654879,14.8451));
#58924=CARTESIAN_POINT('',(23.4442,74.0271430654879,14.8451));
#58925=CARTESIAN_POINT('Origin',(23.4442,74.0271430654879,14.8451));
#58926=CARTESIAN_POINT('',(20.539,74.107964502672,14.9443894024917));
#58927=CARTESIAN_POINT('',(19.939,74.107964502672,14.9443894024917));
#58928=CARTESIAN_POINT('',(20.539,74.3108737350774,15.1936640646055));
#58929=CARTESIAN_POINT('Origin',(20.539,74.2090084002827,14.9501));
#58930=CARTESIAN_POINT('Origin',(20.539,71.6454,13.47));
#58931=CARTESIAN_POINT('Origin',(23.4442,74.1767601111256,15.3851981693292));
#58932=CARTESIAN_POINT('',(20.539,73.873119505839,15.2797828166121));
#58933=CARTESIAN_POINT('',(19.939,73.873119505839,15.2797828166121));
#58934=CARTESIAN_POINT('',(20.539,73.7521754274658,15.2377944841599));
#58935=CARTESIAN_POINT('',(20.539,73.7521754274658,15.2377944841599));
#58936=CARTESIAN_POINT('',(23.4442,73.7521754274658,15.2377944841599));
#58937=CARTESIAN_POINT('Origin',(23.4442,73.7521754274658,15.2377944841599));
#58938=CARTESIAN_POINT('',(20.539,73.8145275816099,15.3496099528092));
#58939=CARTESIAN_POINT('',(19.939,73.8145275816099,15.3496099528092));
#58940=CARTESIAN_POINT('',(20.539,73.9710680760259,15.6303323911273));
#58941=CARTESIAN_POINT('Origin',(20.539,73.9130447605208,15.3727798821941));
#58942=CARTESIAN_POINT('Origin',(20.539,71.6454,13.47));
#58943=CARTESIAN_POINT('Origin',(23.4442,73.8057323911273,15.7956680760259));
#58944=CARTESIAN_POINT('',(20.539,73.5250099528092,15.6391275816099));
#58945=CARTESIAN_POINT('',(19.939,73.5250099528092,15.6391275816099));
#58946=CARTESIAN_POINT('',(20.539,73.4131944841599,15.5767754274658));
#58947=CARTESIAN_POINT('',(20.539,73.4131944841599,15.5767754274658));
#58948=CARTESIAN_POINT('',(23.4442,73.4131944841599,15.5767754274658));
#58949=CARTESIAN_POINT('Origin',(23.4442,73.4131944841599,15.5767754274658));
#58950=CARTESIAN_POINT('',(20.539,73.4551828166121,15.697719505839));
#58951=CARTESIAN_POINT('',(19.939,73.4551828166121,15.697719505839));
#58952=CARTESIAN_POINT('',(20.539,73.5605981693292,16.0013601111256));
#58953=CARTESIAN_POINT('Origin',(20.539,73.5481798821941,15.7376447605208));
#58954=CARTESIAN_POINT('Origin',(20.539,71.6454,13.47));
#58955=CARTESIAN_POINT('Origin',(23.4442,73.3690640646055,16.1354737350774));
#58956=CARTESIAN_POINT('',(20.539,73.1197894024917,15.932564502672));
#58957=CARTESIAN_POINT('',(19.939,73.1197894024917,15.932564502672));
#58958=CARTESIAN_POINT('',(20.539,73.0205,15.8517430654879));
#58959=CARTESIAN_POINT('',(20.539,73.0205,15.8517430654879));
#58960=CARTESIAN_POINT('',(23.4442,73.0205,15.8517430654879));
#58961=CARTESIAN_POINT('Origin',(23.4442,73.0205,15.8517430654879));
#58962=CARTESIAN_POINT('',(20.539,73.0408487165258,15.9781409289644));
#58963=CARTESIAN_POINT('',(19.939,73.0408487165259,15.9781409289644));
#58964=CARTESIAN_POINT('',(20.539,73.0919359353945,16.2954737350774));
#58965=CARTESIAN_POINT('Origin',(20.539,73.1255,16.0336084002827));
#58966=CARTESIAN_POINT('Origin',(20.539,71.6454,13.47));
#58967=CARTESIAN_POINT('Origin',(23.4442,72.8800230776968,16.3942903234834));
#58968=CARTESIAN_POINT('',(20.539,72.6697702762566,16.1511776474381));
#58969=CARTESIAN_POINT('',(19.939,72.6697702762566,16.1511776474381));
#58970=CARTESIAN_POINT('',(20.539,72.5860237981742,16.0543426456854));
#58971=CARTESIAN_POINT('',(20.539,72.5860237981742,16.0543426456854));
#58972=CARTESIAN_POINT('',(23.4442,72.5860237981742,16.0543426456854));
#58973=CARTESIAN_POINT('Origin',(23.4442,72.5860237981742,16.0543426456854));
#58974=CARTESIAN_POINT('',(20.539,72.5841146133191,16.1823537591437));
#58975=CARTESIAN_POINT('',(19.939,72.5841146133191,16.1823537591437));
#58976=CARTESIAN_POINT('',(20.539,72.5793214390453,16.5037367693476));
#58977=CARTESIAN_POINT('Origin',(20.539,72.6578480282726,16.2516780960504));
#58978=CARTESIAN_POINT('Origin',(20.539,71.6454,13.47));
#58979=CARTESIAN_POINT('Origin',(23.4442,72.3534686933216,16.5642538301726));
#58980=CARTESIAN_POINT('',(20.539,72.1886261775338,16.2883245661282));
#58981=CARTESIAN_POINT('',(19.939,72.1886261775338,16.2883245661282));
#58982=CARTESIAN_POINT('',(20.539,72.1229672182196,16.1784182823342));
#58983=CARTESIAN_POINT('',(20.539,72.1229672182196,16.1784182823342));
#58984=CARTESIAN_POINT('',(23.4442,72.1229672182196,16.1784182823342));
#58985=CARTESIAN_POINT('Origin',(23.4442,72.1229672182196,16.1784182823342));
#58986=CARTESIAN_POINT('',(20.539,72.0988581415991,16.3041530928687));
#58987=CARTESIAN_POINT('',(19.939,72.0988581415991,16.3041530928687));
#58988=CARTESIAN_POINT('',(20.539,72.0383302123577,16.619821247026));
#58989=CARTESIAN_POINT('Origin',(20.539,72.1594333355296,16.3852279104667));
#58990=CARTESIAN_POINT('Origin',(20.539,71.6454,13.47));
#58991=CARTESIAN_POINT('Origin',(23.4442,71.8054,16.6402));
#58992=CARTESIAN_POINT('',(20.539,71.6909764262924,16.3398381190176));
#58993=CARTESIAN_POINT('',(19.939,71.6909764262924,16.3398381190176));
#58994=CARTESIAN_POINT('',(20.539,71.6454,16.2202));
#58995=CARTESIAN_POINT('',(20.539,71.6454,16.2202));
#58996=CARTESIAN_POINT('',(23.4442,71.6454,16.2202));
#58997=CARTESIAN_POINT('Origin',(23.4442,71.6454,16.2202));
#58998=CARTESIAN_POINT('',(20.539,71.5998235737076,16.3398381190176));
#58999=CARTESIAN_POINT('',(19.939,71.5998235737076,16.3398381190176));
#59000=CARTESIAN_POINT('',(20.539,71.4854,16.6402));
#59001=CARTESIAN_POINT('Origin',(20.539,71.6454,16.4302));
#59002=CARTESIAN_POINT('',(20.539,71.6454,16.3402));
#59003=CARTESIAN_POINT('Origin',(20.539,71.6454,13.47));
#59004=CARTESIAN_POINT('Origin',(20.539,71.6454,13.47));
#59005=CARTESIAN_POINT('Origin',(23.4442,71.2524697876423,16.619821247026));
#59006=CARTESIAN_POINT('',(20.539,71.1919418584009,16.3041530928687));
#59007=CARTESIAN_POINT('',(19.939,71.1919418584009,16.3041530928687));
#59008=CARTESIAN_POINT('',(20.539,71.1678327817804,16.1784182823342));
#59009=CARTESIAN_POINT('',(20.539,71.1678327817804,16.1784182823342));
#59010=CARTESIAN_POINT('',(23.4442,71.1678327817804,16.1784182823342));
#59011=CARTESIAN_POINT('Origin',(23.4442,71.1678327817804,16.1784182823342));
#59012=CARTESIAN_POINT('',(20.539,71.1021738224661,16.2883245661282));
#59013=CARTESIAN_POINT('',(19.939,71.1021738224661,16.2883245661282));
#59014=CARTESIAN_POINT('',(20.539,70.9373313066783,16.5642538301726));
#59015=CARTESIAN_POINT('Origin',(20.539,71.1313666644703,16.3852279104667));
#59016=CARTESIAN_POINT('Origin',(20.539,71.6454,13.47));
#59017=CARTESIAN_POINT('Origin',(23.4442,70.7114785609547,16.5037367693476));
#59018=CARTESIAN_POINT('',(20.539,70.7066853866809,16.1823537591438));
#59019=CARTESIAN_POINT('',(19.939,70.7066853866809,16.1823537591437));
#59020=CARTESIAN_POINT('',(20.539,70.7047762018258,16.0543426456854));
#59021=CARTESIAN_POINT('',(20.539,70.7047762018258,16.0543426456854));
#59022=CARTESIAN_POINT('',(23.4442,70.7047762018258,16.0543426456854));
#59023=CARTESIAN_POINT('Origin',(23.4442,70.7047762018258,16.0543426456854));
#59024=CARTESIAN_POINT('',(20.539,70.6210297237434,16.1511776474381));
#59025=CARTESIAN_POINT('',(19.939,70.6210297237434,16.1511776474381));
#59026=CARTESIAN_POINT('',(20.539,70.4107769223032,16.3942903234834));
#59027=CARTESIAN_POINT('Origin',(20.539,70.6329519717274,16.2516780960504));
#59028=CARTESIAN_POINT('Origin',(20.539,71.6454,13.47));
#59029=CARTESIAN_POINT('Origin',(23.4442,70.1988640646055,16.2954737350774));
#59030=CARTESIAN_POINT('',(20.539,70.2499512834741,15.9781409289644));
#59031=CARTESIAN_POINT('',(19.939,70.2499512834741,15.9781409289644));
#59032=CARTESIAN_POINT('',(20.539,70.2703,15.851743065488));
#59033=CARTESIAN_POINT('',(20.539,70.2703,15.851743065488));
#59034=CARTESIAN_POINT('',(23.4442,70.2703,15.851743065488));
#59035=CARTESIAN_POINT('Origin',(23.4442,70.2703,15.851743065488));
#59036=CARTESIAN_POINT('',(20.539,70.1710105975083,15.932564502672));
#59037=CARTESIAN_POINT('',(19.939,70.1710105975083,15.932564502672));
#59038=CARTESIAN_POINT('',(20.539,69.9217359353945,16.1354737350774));
#59039=CARTESIAN_POINT('Origin',(20.539,70.1653,16.0336084002827));
#59040=CARTESIAN_POINT('Origin',(20.539,71.6454,13.47));
#59041=CARTESIAN_POINT('Origin',(23.4442,69.7302018306708,16.0013601111256));
#59042=CARTESIAN_POINT('',(20.539,69.8356171833879,15.697719505839));
#59043=CARTESIAN_POINT('',(19.939,69.8356171833879,15.697719505839));
#59044=CARTESIAN_POINT('',(20.539,69.8776055158401,15.5767754274658));
#59045=CARTESIAN_POINT('',(20.539,69.8776055158401,15.5767754274658));
#59046=CARTESIAN_POINT('',(23.4442,69.8776055158401,15.5767754274658));
#59047=CARTESIAN_POINT('Origin',(23.4442,69.8776055158401,15.5767754274658));
#59048=CARTESIAN_POINT('',(20.539,69.7657900471908,15.6391275816099));
#59049=CARTESIAN_POINT('',(19.939,69.7657900471908,15.6391275816099));
#59050=CARTESIAN_POINT('',(20.539,69.4850676088727,15.7956680760259));
#59051=CARTESIAN_POINT('Origin',(20.539,69.7426201178059,15.7376447605208));
#59052=CARTESIAN_POINT('Origin',(20.539,71.6454,13.47));
#59053=CARTESIAN_POINT('Origin',(23.4442,69.3197319239741,15.6303323911273));
#59054=CARTESIAN_POINT('',(20.539,69.4762724183901,15.3496099528092));
#59055=CARTESIAN_POINT('',(19.939,69.4762724183901,15.3496099528092));
#59056=CARTESIAN_POINT('',(20.539,69.5386245725342,15.2377944841599));
#59057=CARTESIAN_POINT('',(20.539,69.5386245725342,15.2377944841599));
#59058=CARTESIAN_POINT('',(23.4442,69.5386245725342,15.2377944841599));
#59059=CARTESIAN_POINT('Origin',(23.4442,69.5386245725342,15.2377944841599));
#59060=CARTESIAN_POINT('',(20.539,69.417680494161,15.2797828166121));
#59061=CARTESIAN_POINT('',(19.939,69.417680494161,15.2797828166121));
#59062=CARTESIAN_POINT('',(20.539,69.1140398888744,15.3851981693292));
#59063=CARTESIAN_POINT('Origin',(20.539,69.3777552394792,15.3727798821941));
#59064=CARTESIAN_POINT('Origin',(20.539,71.6454,13.47));
#59065=CARTESIAN_POINT('Origin',(23.4442,68.9799262649226,15.1936640646055));
#59066=CARTESIAN_POINT('',(20.539,69.182835497328,14.9443894024917));
#59067=CARTESIAN_POINT('',(19.939,69.182835497328,14.9443894024917));
#59068=CARTESIAN_POINT('',(20.539,69.263656934512,14.8451));
#59069=CARTESIAN_POINT('',(20.539,69.263656934512,14.8451));
#59070=CARTESIAN_POINT('',(23.4442,69.263656934512,14.8451));
#59071=CARTESIAN_POINT('Origin',(23.4442,69.263656934512,14.8451));
#59072=CARTESIAN_POINT('',(20.539,69.1372590710356,14.8654487165258));
#59073=CARTESIAN_POINT('',(19.939,69.1372590710356,14.8654487165258));
#59074=CARTESIAN_POINT('',(20.539,68.8199262649226,14.9165359353945));
#59075=CARTESIAN_POINT('Origin',(20.539,69.0817915997173,14.9501));
#59076=CARTESIAN_POINT('Origin',(20.539,71.6454,13.47));
#59077=CARTESIAN_POINT('Origin',(23.4442,68.7211096765166,14.7046230776968));
#59078=CARTESIAN_POINT('',(20.539,68.9642223525619,14.4943702762566));
#59079=CARTESIAN_POINT('',(19.939,68.9642223525619,14.4943702762566));
#59080=CARTESIAN_POINT('',(20.539,69.0610573543146,14.4106237981742));
#59081=CARTESIAN_POINT('',(20.539,69.0610573543146,14.4106237981742));
#59082=CARTESIAN_POINT('',(23.4442,69.0610573543146,14.4106237981742));
#59083=CARTESIAN_POINT('Origin',(23.4442,69.0610573543146,14.4106237981742));
#59084=CARTESIAN_POINT('',(20.539,68.9330462408563,14.4087146133191));
#59085=CARTESIAN_POINT('',(19.939,68.9330462408563,14.4087146133191));
#59086=CARTESIAN_POINT('',(20.539,68.6116632306524,14.4039214390453));
#59087=CARTESIAN_POINT('Origin',(20.539,68.8637219039496,14.4824480282726));
#59088=CARTESIAN_POINT('Origin',(20.539,71.6454,13.47));
#59089=CARTESIAN_POINT('Origin',(23.4442,68.5511461698274,14.1780686933217));
#59090=CARTESIAN_POINT('',(20.539,68.8270754338718,14.0132261775339));
#59091=CARTESIAN_POINT('',(19.939,68.8270754338718,14.0132261775338));
#59092=CARTESIAN_POINT('',(20.539,68.9369817176658,13.9475672182196));
#59093=CARTESIAN_POINT('',(20.539,68.9369817176658,13.9475672182196));
#59094=CARTESIAN_POINT('',(23.4442,68.9369817176658,13.9475672182196));
#59095=CARTESIAN_POINT('Origin',(23.4442,68.9369817176658,13.9475672182196));
#59096=CARTESIAN_POINT('',(20.539,68.8112469071312,13.9234581415991));
#59097=CARTESIAN_POINT('',(19.939,68.8112469071312,13.9234581415991));
#59098=CARTESIAN_POINT('',(20.539,68.495578752974,13.8629302123577));
#59099=CARTESIAN_POINT('Origin',(20.539,68.7301720895333,13.9840333355296));
#59100=CARTESIAN_POINT('Origin',(20.539,71.6454,13.47));
#59101=CARTESIAN_POINT('Origin',(23.4442,68.4752,13.63));
#59102=CARTESIAN_POINT('',(20.539,68.7755618809824,13.5155764262924));
#59103=CARTESIAN_POINT('',(19.939,68.7755618809824,13.5155764262924));
#59104=CARTESIAN_POINT('',(20.539,68.8952,13.47));
#59105=CARTESIAN_POINT('',(20.539,68.8952,13.47));
#59106=CARTESIAN_POINT('',(23.4442,68.8952,13.47));
#59107=CARTESIAN_POINT('Origin',(23.4442,68.8952,13.47));
#59108=CARTESIAN_POINT('',(20.539,68.7755618809824,13.4244235737076));
#59109=CARTESIAN_POINT('',(19.939,68.7755618809824,13.4244235737076));
#59110=CARTESIAN_POINT('',(20.539,68.4752,13.31));
#59111=CARTESIAN_POINT('Origin',(20.539,68.6852,13.47));
#59112=CARTESIAN_POINT('Origin',(20.539,71.6454,13.47));
#59113=CARTESIAN_POINT('Origin',(23.4442,68.495578752974,13.0770697876423));
#59114=CARTESIAN_POINT('',(20.539,68.8112469071312,13.0165418584009));
#59115=CARTESIAN_POINT('',(19.939,68.8112469071312,13.0165418584009));
#59116=CARTESIAN_POINT('',(20.539,68.9369817176658,12.9924327817804));
#59117=CARTESIAN_POINT('',(20.539,68.9369817176658,12.9924327817804));
#59118=CARTESIAN_POINT('',(23.4442,68.9369817176658,12.9924327817804));
#59119=CARTESIAN_POINT('Origin',(23.4442,68.9369817176658,12.9924327817804));
#59120=CARTESIAN_POINT('',(20.539,68.8270754338718,12.9267738224661));
#59121=CARTESIAN_POINT('',(19.939,68.8270754338718,12.9267738224661));
#59122=CARTESIAN_POINT('',(20.539,68.5511461698274,12.7619313066783));
#59123=CARTESIAN_POINT('Origin',(20.539,68.7301720895333,12.9559666644704));
#59124=CARTESIAN_POINT('Origin',(20.539,71.6454,13.47));
#59125=CARTESIAN_POINT('Origin',(23.4442,68.6116632306524,12.5360785609547));
#59126=CARTESIAN_POINT('',(20.539,68.9330462408563,12.5312853866809));
#59127=CARTESIAN_POINT('',(19.939,68.9330462408563,12.5312853866809));
#59128=CARTESIAN_POINT('',(20.539,69.0610573543146,12.5293762018258));
#59129=CARTESIAN_POINT('',(20.539,69.0610573543146,12.5293762018258));
#59130=CARTESIAN_POINT('',(23.4442,69.0610573543146,12.5293762018258));
#59131=CARTESIAN_POINT('Origin',(23.4442,69.0610573543146,12.5293762018258));
#59132=CARTESIAN_POINT('',(20.539,68.9642223525618,12.4456297237434));
#59133=CARTESIAN_POINT('',(19.939,68.9642223525618,12.4456297237434));
#59134=CARTESIAN_POINT('',(20.539,68.7211096765166,12.2353769223032));
#59135=CARTESIAN_POINT('Origin',(20.539,68.8637219039495,12.4575519717274));
#59136=CARTESIAN_POINT('Origin',(20.539,71.6454,13.47));
#59137=CARTESIAN_POINT('Origin',(23.4442,68.8199262649226,12.0234640646055));
#59138=CARTESIAN_POINT('',(20.539,69.1372590710356,12.0745512834741));
#59139=CARTESIAN_POINT('',(19.939,69.1372590710356,12.0745512834741));
#59140=CARTESIAN_POINT('',(20.539,69.263656934512,12.0949));
#59141=CARTESIAN_POINT('',(20.539,69.263656934512,12.0949));
#59142=CARTESIAN_POINT('',(23.4442,69.263656934512,12.0949));
#59143=CARTESIAN_POINT('Origin',(23.4442,69.263656934512,12.0949));
#59144=CARTESIAN_POINT('',(20.539,69.182835497328,11.9956105975083));
#59145=CARTESIAN_POINT('',(19.939,69.182835497328,11.9956105975083));
#59146=CARTESIAN_POINT('',(20.539,68.9799262649226,11.7463359353945));
#59147=CARTESIAN_POINT('Origin',(20.539,69.0817915997173,11.9899));
#59148=CARTESIAN_POINT('Origin',(20.539,71.6454,13.47));
#59149=CARTESIAN_POINT('Origin',(23.4442,69.1140398888744,11.5548018306708));
#59150=CARTESIAN_POINT('',(20.539,69.417680494161,11.6602171833879));
#59151=CARTESIAN_POINT('',(19.939,69.417680494161,11.6602171833879));
#59152=CARTESIAN_POINT('',(20.539,69.5386245725342,11.7022055158401));
#59153=CARTESIAN_POINT('',(20.539,69.5386245725342,11.7022055158401));
#59154=CARTESIAN_POINT('',(23.4442,69.5386245725342,11.7022055158401));
#59155=CARTESIAN_POINT('Origin',(23.4442,69.5386245725342,11.7022055158401));
#59156=CARTESIAN_POINT('',(20.539,69.4762724183901,11.5903900471908));
#59157=CARTESIAN_POINT('',(19.939,69.4762724183901,11.5903900471908));
#59158=CARTESIAN_POINT('',(20.539,69.3197319239741,11.3096676088727));
#59159=CARTESIAN_POINT('Origin',(20.539,69.3777552394792,11.5672201178059));
#59160=CARTESIAN_POINT('Origin',(20.539,71.6454,13.47));
#59161=CARTESIAN_POINT('Origin',(23.4442,69.4850676088727,11.1443319239741));
#59162=CARTESIAN_POINT('',(20.539,69.7657900471908,11.3008724183901));
#59163=CARTESIAN_POINT('',(19.939,69.7657900471908,11.3008724183901));
#59164=CARTESIAN_POINT('',(20.539,69.8776055158401,11.3632245725342));
#59165=CARTESIAN_POINT('',(20.539,69.8776055158401,11.3632245725342));
#59166=CARTESIAN_POINT('',(23.4442,69.8776055158401,11.3632245725342));
#59167=CARTESIAN_POINT('Origin',(23.4442,69.8776055158401,11.3632245725342));
#59168=CARTESIAN_POINT('',(20.539,69.8356171833879,11.242280494161));
#59169=CARTESIAN_POINT('',(19.939,69.8356171833879,11.242280494161));
#59170=CARTESIAN_POINT('',(20.539,69.7302018306708,10.9386398888744));
#59171=CARTESIAN_POINT('Origin',(20.539,69.7426201178059,11.2023552394792));
#59172=CARTESIAN_POINT('Origin',(20.539,71.6454,13.47));
#59173=CARTESIAN_POINT('Origin',(23.4442,69.9217359353945,10.8045262649226));
#59174=CARTESIAN_POINT('',(20.539,70.1710105975083,11.007435497328));
#59175=CARTESIAN_POINT('',(19.939,70.1710105975083,11.007435497328));
#59176=CARTESIAN_POINT('',(20.539,70.2703,11.0882569345121));
#59177=CARTESIAN_POINT('',(20.539,70.2703,11.0882569345121));
#59178=CARTESIAN_POINT('',(23.4442,70.2703,11.0882569345121));
#59179=CARTESIAN_POINT('Origin',(23.4442,70.2703,11.0882569345121));
#59180=CARTESIAN_POINT('',(20.539,70.2499512834742,10.9618590710356));
#59181=CARTESIAN_POINT('',(19.939,70.2499512834741,10.9618590710356));
#59182=CARTESIAN_POINT('',(20.539,70.1988640646055,10.6445262649226));
#59183=CARTESIAN_POINT('Origin',(20.539,70.1653,10.9063915997173));
#59184=CARTESIAN_POINT('Origin',(20.539,71.6454,13.47));
#59185=CARTESIAN_POINT('Origin',(23.4442,70.4107769223032,10.5457096765166));
#59186=CARTESIAN_POINT('',(20.539,70.6210297237433,10.7888223525619));
#59187=CARTESIAN_POINT('',(19.939,70.6210297237434,10.7888223525619));
#59188=CARTESIAN_POINT('',(20.539,70.7047762018258,10.8856573543146));
#59189=CARTESIAN_POINT('',(20.539,70.7047762018258,10.8856573543146));
#59190=CARTESIAN_POINT('',(23.4442,70.7047762018258,10.8856573543146));
#59191=CARTESIAN_POINT('Origin',(23.4442,70.7047762018258,10.8856573543146));
#59192=CARTESIAN_POINT('',(20.539,70.7066853866809,10.7576462408563));
#59193=CARTESIAN_POINT('',(19.939,70.7066853866809,10.7576462408563));
#59194=CARTESIAN_POINT('',(20.539,70.7114785609547,10.4362632306524));
#59195=CARTESIAN_POINT('Origin',(20.539,70.6329519717274,10.6883219039496));
#59196=CARTESIAN_POINT('Origin',(20.539,71.6454,13.47));
#59197=CARTESIAN_POINT('Origin',(23.4442,70.9373313066783,10.3757461698274));
#59198=CARTESIAN_POINT('',(20.539,71.1021738224661,10.6516754338718));
#59199=CARTESIAN_POINT('',(19.939,71.1021738224661,10.6516754338718));
#59200=CARTESIAN_POINT('',(20.539,71.1678327817804,10.7615817176658));
#59201=CARTESIAN_POINT('',(20.539,71.1678327817804,10.7615817176658));
#59202=CARTESIAN_POINT('',(23.4442,71.1678327817804,10.7615817176658));
#59203=CARTESIAN_POINT('Origin',(23.4442,71.1678327817804,10.7615817176658));
#59204=CARTESIAN_POINT('',(20.539,71.1919418584009,10.6358469071313));
#59205=CARTESIAN_POINT('',(19.939,71.1919418584009,10.6358469071313));
#59206=CARTESIAN_POINT('',(20.539,71.2524697876422,10.320178752974));
#59207=CARTESIAN_POINT('Origin',(20.539,71.1313666644703,10.5547720895333));
#59208=CARTESIAN_POINT('Origin',(20.539,71.6454,13.47));
#59209=CARTESIAN_POINT('Origin',(23.4442,71.4854,10.2998));
#59210=CARTESIAN_POINT('',(20.539,71.5998235737076,10.6001618809824));
#59211=CARTESIAN_POINT('',(19.939,71.5998235737076,10.6001618809824));
#59212=CARTESIAN_POINT('',(20.539,71.6454,10.7198));
#59213=CARTESIAN_POINT('',(20.539,71.6454,10.7198));
#59214=CARTESIAN_POINT('',(23.4442,71.6454,10.7198));
#59215=CARTESIAN_POINT('Origin',(23.4442,71.6454,10.7198));
#59216=CARTESIAN_POINT('',(20.539,71.6909764262924,10.6001618809824));
#59217=CARTESIAN_POINT('',(19.939,71.6909764262924,10.6001618809824));
#59218=CARTESIAN_POINT('',(20.539,71.8054,10.2998));
#59219=CARTESIAN_POINT('Origin',(20.539,71.6454,10.5098));
#59220=CARTESIAN_POINT('Origin',(20.539,71.6454,13.47));
#59221=CARTESIAN_POINT('Origin',(23.4442,72.0383302123577,10.320178752974));
#59222=CARTESIAN_POINT('',(20.539,72.0988581415991,10.6358469071313));
#59223=CARTESIAN_POINT('',(19.939,72.0988581415992,10.6358469071313));
#59224=CARTESIAN_POINT('',(20.539,72.1229672182196,10.7615817176658));
#59225=CARTESIAN_POINT('',(20.539,72.1229672182196,10.7615817176658));
#59226=CARTESIAN_POINT('',(23.4442,72.1229672182196,10.7615817176658));
#59227=CARTESIAN_POINT('Origin',(23.4442,72.1229672182196,10.7615817176658));
#59228=CARTESIAN_POINT('',(20.539,72.1886261775339,10.6516754338718));
#59229=CARTESIAN_POINT('',(19.939,72.1886261775339,10.6516754338718));
#59230=CARTESIAN_POINT('',(20.539,72.3534686933216,10.3757461698274));
#59231=CARTESIAN_POINT('Origin',(20.539,72.1594333355297,10.5547720895333));
#59232=CARTESIAN_POINT('Origin',(20.539,71.6454,13.47));
#59233=CARTESIAN_POINT('Origin',(23.4442,72.5793214390453,10.4362632306524));
#59234=CARTESIAN_POINT('',(20.539,72.5841146133191,10.7576462408563));
#59235=CARTESIAN_POINT('',(19.939,72.5841146133191,10.7576462408563));
#59236=CARTESIAN_POINT('',(20.539,72.5860237981743,10.8856573543146));
#59237=CARTESIAN_POINT('',(20.539,72.5860237981743,10.8856573543146));
#59238=CARTESIAN_POINT('',(23.4442,72.5860237981743,10.8856573543146));
#59239=CARTESIAN_POINT('Origin',(23.4442,72.5860237981743,10.8856573543146));
#59240=CARTESIAN_POINT('',(20.539,72.6697702762566,10.7888223525619));
#59241=CARTESIAN_POINT('',(19.939,72.6697702762566,10.7888223525619));
#59242=CARTESIAN_POINT('',(20.539,72.8800230776968,10.5457096765166));
#59243=CARTESIAN_POINT('Origin',(20.539,72.6578480282726,10.6883219039496));
#59244=CARTESIAN_POINT('Origin',(20.539,71.6454,13.47));
#59245=CARTESIAN_POINT('Origin',(23.4442,73.0919359353945,10.6445262649226));
#59246=CARTESIAN_POINT('',(20.539,73.0408487165258,10.9618590710356));
#59247=CARTESIAN_POINT('',(19.939,73.0408487165258,10.9618590710356));
#59248=CARTESIAN_POINT('',(20.539,73.0205,11.088256934512));
#59249=CARTESIAN_POINT('',(20.539,73.0205,11.088256934512));
#59250=CARTESIAN_POINT('',(23.4442,73.0205,11.088256934512));
#59251=CARTESIAN_POINT('Origin',(23.4442,73.0205,11.088256934512));
#59252=CARTESIAN_POINT('',(20.539,73.1197894024917,11.007435497328));
#59253=CARTESIAN_POINT('',(19.939,73.1197894024917,11.007435497328));
#59254=CARTESIAN_POINT('',(20.539,73.3690640646055,10.8045262649226));
#59255=CARTESIAN_POINT('Origin',(20.539,73.1255,10.9063915997173));
#59256=CARTESIAN_POINT('Origin',(20.539,71.6454,13.47));
#59257=CARTESIAN_POINT('Origin',(23.4442,73.5605981693292,10.9386398888744));
#59258=CARTESIAN_POINT('',(20.539,73.4551828166121,11.242280494161));
#59259=CARTESIAN_POINT('',(19.939,73.4551828166121,11.242280494161));
#59260=CARTESIAN_POINT('',(20.539,73.4131944841599,11.3632245725342));
#59261=CARTESIAN_POINT('',(20.539,73.4131944841599,11.3632245725342));
#59262=CARTESIAN_POINT('',(23.4442,73.4131944841599,11.3632245725342));
#59263=CARTESIAN_POINT('Origin',(23.4442,73.4131944841599,11.3632245725342));
#59264=CARTESIAN_POINT('',(20.539,73.5250099528092,11.3008724183901));
#59265=CARTESIAN_POINT('',(19.939,73.5250099528092,11.3008724183901));
#59266=CARTESIAN_POINT('',(20.539,73.8057323911273,11.1443319239741));
#59267=CARTESIAN_POINT('Origin',(20.539,73.5481798821941,11.2023552394792));
#59268=CARTESIAN_POINT('Origin',(20.539,71.6454,13.47));
#59269=CARTESIAN_POINT('Origin',(23.4442,73.9710680760259,11.3096676088727));
#59270=CARTESIAN_POINT('',(20.539,73.8145275816099,11.5903900471908));
#59271=CARTESIAN_POINT('',(19.939,73.8145275816099,11.5903900471908));
#59272=CARTESIAN_POINT('',(20.539,73.7521754274658,11.7022055158401));
#59273=CARTESIAN_POINT('',(20.539,73.7521754274658,11.7022055158401));
#59274=CARTESIAN_POINT('',(23.4442,73.7521754274658,11.7022055158401));
#59275=CARTESIAN_POINT('Origin',(23.4442,73.7521754274658,11.7022055158401));
#59276=CARTESIAN_POINT('',(20.539,73.873119505839,11.6602171833879));
#59277=CARTESIAN_POINT('',(19.939,73.873119505839,11.6602171833879));
#59278=CARTESIAN_POINT('',(20.539,74.1767601111256,11.5548018306708));
#59279=CARTESIAN_POINT('Origin',(20.539,73.9130447605208,11.5672201178059));
#59280=CARTESIAN_POINT('Origin',(20.539,71.6454,13.47));
#59281=CARTESIAN_POINT('Origin',(23.4442,74.3108737350774,11.7463359353945));
#59282=CARTESIAN_POINT('',(20.539,74.107964502672,11.9956105975083));
#59283=CARTESIAN_POINT('',(19.939,74.107964502672,11.9956105975083));
#59284=CARTESIAN_POINT('',(20.539,74.027143065488,12.0949));
#59285=CARTESIAN_POINT('',(20.539,74.027143065488,12.0949));
#59286=CARTESIAN_POINT('',(23.4442,74.027143065488,12.0949));
#59287=CARTESIAN_POINT('Origin',(23.4442,74.027143065488,12.0949));
#59288=CARTESIAN_POINT('',(20.539,74.1535409289644,12.0745512834741));
#59289=CARTESIAN_POINT('',(19.939,74.1535409289644,12.0745512834741));
#59290=CARTESIAN_POINT('',(20.539,74.4708737350774,12.0234640646055));
#59291=CARTESIAN_POINT('Origin',(20.539,74.2090084002827,11.9899));
#59292=CARTESIAN_POINT('Origin',(20.539,71.6454,13.47));
#59293=CARTESIAN_POINT('Origin',(23.4442,74.5696903234834,12.2353769223032));
#59294=CARTESIAN_POINT('',(20.539,74.3265776474381,12.4456297237434));
#59295=CARTESIAN_POINT('',(19.939,74.3265776474381,12.4456297237434));
#59296=CARTESIAN_POINT('',(20.539,74.2297426456854,12.5293762018257));
#59297=CARTESIAN_POINT('',(20.539,74.2297426456854,12.5293762018257));
#59298=CARTESIAN_POINT('',(23.4442,74.2297426456854,12.5293762018257));
#59299=CARTESIAN_POINT('Origin',(23.4442,74.2297426456854,12.5293762018257));
#59300=CARTESIAN_POINT('',(20.539,74.3577537591437,12.5312853866809));
#59301=CARTESIAN_POINT('',(19.939,74.3577537591437,12.5312853866809));
#59302=CARTESIAN_POINT('',(20.539,74.6791367693476,12.5360785609547));
#59303=CARTESIAN_POINT('Origin',(20.539,74.4270780960504,12.4575519717274));
#59304=CARTESIAN_POINT('Origin',(20.539,71.6454,13.47));
#59305=CARTESIAN_POINT('Origin',(23.4442,74.7396538301726,12.7619313066783));
#59306=CARTESIAN_POINT('',(20.539,74.4637245661282,12.9267738224661));
#59307=CARTESIAN_POINT('',(19.939,74.4637245661282,12.9267738224661));
#59308=CARTESIAN_POINT('',(20.539,74.3538182823342,12.9924327817804));
#59309=CARTESIAN_POINT('',(20.539,74.3538182823342,12.9924327817804));
#59310=CARTESIAN_POINT('',(23.4442,74.3538182823342,12.9924327817804));
#59311=CARTESIAN_POINT('Origin',(23.4442,74.3538182823342,12.9924327817804));
#59312=CARTESIAN_POINT('',(20.539,74.4795530928687,13.0165418584009));
#59313=CARTESIAN_POINT('',(19.939,74.4795530928687,13.0165418584009));
#59314=CARTESIAN_POINT('',(20.539,74.795221247026,13.0770697876423));
#59315=CARTESIAN_POINT('Origin',(20.539,74.5606279104667,12.9559666644704));
#59316=CARTESIAN_POINT('Origin',(20.539,71.6454,13.47));
#59317=CARTESIAN_POINT('Origin',(23.4442,74.8156,13.31));
#59318=CARTESIAN_POINT('',(20.539,74.5152381190176,13.4244235737076));
#59319=CARTESIAN_POINT('',(19.939,74.5152381190176,13.4244235737076));
#59320=CARTESIAN_POINT('',(20.539,74.3956,13.47));
#59321=CARTESIAN_POINT('',(20.539,74.3956,13.47));
#59322=CARTESIAN_POINT('',(23.4442,74.3956,13.47));
#59323=CARTESIAN_POINT('Origin',(23.4442,74.3956,13.47));
#59324=CARTESIAN_POINT('',(20.539,74.5152381190176,13.5155764262924));
#59325=CARTESIAN_POINT('',(19.939,74.5152381190176,13.5155764262924));
#59326=CARTESIAN_POINT('',(20.539,74.8156,13.63));
#59327=CARTESIAN_POINT('Origin',(20.539,74.6056,13.47));
#59328=CARTESIAN_POINT('Origin',(20.539,71.6454,13.47));
#59329=CARTESIAN_POINT('Origin',(19.939,71.6454,13.47));
#59330=CARTESIAN_POINT('',(19.939,71.6454,16.3402));
#59331=CARTESIAN_POINT('Origin',(23.4442,71.6454,13.47));
#59332=CARTESIAN_POINT('',(23.4442,72.4473756082962,14.8590625));
#59333=CARTESIAN_POINT('',(23.4442,73.2493512165924,13.47));
#59334=CARTESIAN_POINT('',(23.4442,72.6478695103703,14.511796875));
#59335=CARTESIAN_POINT('',(23.4442,72.4473756082962,12.0809375));
#59336=CARTESIAN_POINT('',(23.4442,73.0488573145184,13.122734375));
#59337=CARTESIAN_POINT('',(23.4442,70.8434243917038,12.0809375));
#59338=CARTESIAN_POINT('',(23.4442,72.0463878041481,12.0809375));
#59339=CARTESIAN_POINT('',(23.4442,70.0414487834076,13.47));
#59340=CARTESIAN_POINT('',(23.4442,70.6429304896297,12.428203125));
#59341=CARTESIAN_POINT('',(23.4442,70.8434243917038,14.8590625));
#59342=CARTESIAN_POINT('',(23.4442,70.2419426854816,13.817265625));
#59343=CARTESIAN_POINT('',(23.4442,71.2444121958519,14.8590625));
#59344=CARTESIAN_POINT('Origin',(21.6442,71.6454,13.47));
#59345=CARTESIAN_POINT('',(21.6442,72.4473756082962,14.8590625));
#59346=CARTESIAN_POINT('',(21.6442,73.2493512165924,13.47));
#59347=CARTESIAN_POINT('',(21.6442,73.2493512165924,13.47));
#59348=CARTESIAN_POINT('Origin',(21.6442,71.6454,13.47));
#59349=CARTESIAN_POINT('Origin',(21.6442,71.6454,13.47));
#59350=CARTESIAN_POINT('',(21.6442,72.4473756082962,12.0809375));
#59351=CARTESIAN_POINT('',(21.6442,72.4473756082962,12.0809375));
#59352=CARTESIAN_POINT('Origin',(21.6442,71.6454,13.47));
#59353=CARTESIAN_POINT('Origin',(21.6442,71.6454,13.47));
#59354=CARTESIAN_POINT('',(21.6442,70.8434243917038,12.0809375));
#59355=CARTESIAN_POINT('',(21.6442,70.8434243917038,12.0809375));
#59356=CARTESIAN_POINT('Origin',(21.6442,71.6454,13.47));
#59357=CARTESIAN_POINT('Origin',(21.6442,71.6454,13.47));
#59358=CARTESIAN_POINT('',(21.6442,70.0414487834076,13.47));
#59359=CARTESIAN_POINT('',(21.6442,70.0414487834076,13.47));
#59360=CARTESIAN_POINT('Origin',(21.6442,71.6454,13.47));
#59361=CARTESIAN_POINT('Origin',(21.6442,71.6454,13.47));
#59362=CARTESIAN_POINT('',(21.6442,70.8434243917038,14.8590625));
#59363=CARTESIAN_POINT('',(21.6442,70.8434243917038,14.8590625));
#59364=CARTESIAN_POINT('Origin',(21.6442,71.6454,13.47));
#59365=CARTESIAN_POINT('Origin',(21.6442,71.6454,13.47));
#59366=CARTESIAN_POINT('',(21.6442,72.4473756082962,14.8590625));
#59367=CARTESIAN_POINT('Origin',(21.6442,71.6454,13.47));
#59368=CARTESIAN_POINT('Origin',(21.1623244395541,71.6454,13.47));
#59369=CARTESIAN_POINT('',(20.6804488791083,71.6454,13.47));
#59370=CARTESIAN_POINT('',(21.1623244395541,70.8434243917038,13.47));
#59371=CARTESIAN_POINT('Origin',(23.4442,72.4473756082962,14.8590625));
#59372=CARTESIAN_POINT('',(23.4442,72.4473756082962,14.8590625));
#59373=CARTESIAN_POINT('',(23.4442,73.2493512165924,13.47));
#59374=CARTESIAN_POINT('Origin',(23.4442,70.8434243917038,14.8590625));
#59375=CARTESIAN_POINT('',(23.4442,70.8434243917038,14.8590625));
#59376=CARTESIAN_POINT('Origin',(23.4442,70.0414487834076,13.47));
#59377=CARTESIAN_POINT('',(23.4442,70.0414487834076,13.47));
#59378=CARTESIAN_POINT('Origin',(23.4442,70.8434243917038,12.0809375));
#59379=CARTESIAN_POINT('',(23.4442,70.8434243917038,12.0809375));
#59380=CARTESIAN_POINT('Origin',(23.4442,72.4473756082962,12.0809375));
#59381=CARTESIAN_POINT('',(23.4442,72.4473756082962,12.0809375));
#59382=CARTESIAN_POINT('Origin',(23.4442,73.2493512165924,13.47));
#59383=CARTESIAN_POINT('',(0.,0.,0.));
#59384=CARTESIAN_POINT('Origin',(-17.98,42.93984859951,7.87));
#59385=CARTESIAN_POINT('',(-18.810359785549,40.8943234078509,8.83093840933902));
#59386=CARTESIAN_POINT('',(-18.810359785549,41.063821643627,8.83093840933902));
#59387=CARTESIAN_POINT('',(-18.810359785549,42.93984859951,8.83093840933902));
#59388=CARTESIAN_POINT('',(-18.7697008138552,41.466,6.8753781499502));
#59389=CARTESIAN_POINT('Ctrl Pts',(-18.7697008138552,41.466,6.87537814995019));
#59390=CARTESIAN_POINT('Ctrl Pts',(-18.7662893129558,41.4655640034933,6.87266951748195));
#59391=CARTESIAN_POINT('Ctrl Pts',(-18.7628639760175,41.4651280069866,6.86997851593477));
#59392=CARTESIAN_POINT('Ctrl Pts',(-18.7594249204986,41.4646920104799,6.86730523422837));
#59393=CARTESIAN_POINT('Ctrl Pts',(-18.7203639216068,41.4597399360012,6.83694194023791));
#59394=CARTESIAN_POINT('Ctrl Pts',(-18.6794401066147,41.4547878615226,6.80879775765171));
#59395=CARTESIAN_POINT('Ctrl Pts',(-18.636935323112,41.449835787044,6.78310718962369));
#59396=CARTESIAN_POINT('Ctrl Pts',(-18.5945093211734,41.4448928911128,6.75746423842754));
#59397=CARTESIAN_POINT('Ctrl Pts',(-18.5505086271947,41.4399499951817,6.7342661620788));
#59398=CARTESIAN_POINT('Ctrl Pts',(-18.5052459638554,41.4350070992505,6.71370562681746));
#59399=CARTESIAN_POINT('Ctrl Pts',(-18.4600296773934,41.4300692678927,6.69316615822235));
#59400=CARTESIAN_POINT('Ctrl Pts',(-18.4135544770867,41.4251314365349,6.67525910546274));
#59401=CARTESIAN_POINT('Ctrl Pts',(-18.3661578415816,41.420193605177,6.66013136193015));
#59402=CARTESIAN_POINT('Ctrl Pts',(-18.3187896931452,41.415258741632,6.64501271071101));
#59403=CARTESIAN_POINT('Ctrl Pts',(-18.2705017267598,41.4103238780869,6.63267022523192));
#59404=CARTESIAN_POINT('Ctrl Pts',(-18.2216491507329,41.4053890145419,6.62320182549457));
#59405=CARTESIAN_POINT('Ctrl Pts',(-18.1728052452749,41.400455026858,6.61373510625023));
#59406=CARTESIAN_POINT('Ctrl Pts',(-18.1233974659279,41.3955210391741,6.60714156320865));
#59407=CARTESIAN_POINT('Ctrl Pts',(-18.0737913182603,41.3905870514902,6.60346804674379));
#59408=CARTESIAN_POINT('Ctrl Pts',(-18.0241380309588,41.3856483751461,6.59979103941682));
#59409=CARTESIAN_POINT('Ctrl Pts',(-17.9742865454902,41.3807096988019,6.59903963882925));
#59410=CARTESIAN_POINT('Ctrl Pts',(-17.9246057785493,41.3757710224578,6.60120865378508));
#59411=CARTESIAN_POINT('Ctrl Pts',(-17.874898993866,41.3708297597363,6.60337880465075));
#59412=CARTESIAN_POINT('Ctrl Pts',(-17.8253636504628,41.3658884970149,6.60847236140719));
#59413=CARTESIAN_POINT('Ctrl Pts',(-17.7763634063757,41.3609472342934,6.61643223647977));
#59414=CARTESIAN_POINT('Ctrl Pts',(-17.7272731594248,41.3559968955397,6.62440673212346));
#59415=CARTESIAN_POINT('Ctrl Pts',(-17.6787205076998,41.351046556786,6.63525793527213));
#59416=CARTESIAN_POINT('Ctrl Pts',(-17.6310571840911,41.3460962180323,6.648878011325));
#59417=CARTESIAN_POINT('Ctrl Pts',(-17.607174645919,41.3436157646081,6.65570258757383));
#59418=CARTESIAN_POINT('Ctrl Pts',(-17.5835151218471,41.341135311184,6.66322156449435));
#59419=CARTESIAN_POINT('Ctrl Pts',(-17.5601209284272,41.3386548577598,6.67141685092141));
#59420=CARTESIAN_POINT('Ctrl Pts',(-17.513378656745,41.3336988404369,6.68779126904351));
#59421=CARTESIAN_POINT('Ctrl Pts',(-17.4674961099178,41.3287428231139,6.70693891537748));
#59422=CARTESIAN_POINT('Ctrl Pts',(-17.4228233946656,41.3237868057909,6.72874883112083));
#59423=CARTESIAN_POINT('Ctrl Pts',(-17.3782304368162,41.3188396368011,6.75051980805726));
#59424=CARTESIAN_POINT('Ctrl Pts',(-17.3348435128803,41.3138924678114,6.77494338870558));
#59425=CARTESIAN_POINT('Ctrl Pts',(-17.292994156614,41.3089452988216,6.80186004140209));
#59426=CARTESIAN_POINT('Ctrl Pts',(-17.2511859440286,41.3040029935803,6.82875023132198));
#59427=CARTESIAN_POINT('Ctrl Pts',(-17.2109127631429,41.299060688339,6.85812834631362));
#59428=CARTESIAN_POINT('Ctrl Pts',(-17.1724809489868,41.2941183830976,6.88978931741652));
#59429=CARTESIAN_POINT('Ctrl Pts',(-17.1340707187855,41.2891788535383,6.92143250718429));
#59430=CARTESIAN_POINT('Ctrl Pts',(-17.0975002268711,41.2842393239789,6.95535566624437));
#59431=CARTESIAN_POINT('Ctrl Pts',(-17.0630441374719,41.2792997944195,6.99131237281081));
#59432=CARTESIAN_POINT('Ctrl Pts',(-17.0285928762913,41.2743609570202,7.02726404088209));
#59433=CARTESIAN_POINT('Ctrl Pts',(-16.9962558059207,41.2694221196208,7.06524829586063));
#59434=CARTESIAN_POINT('Ctrl Pts',(-16.9662701561303,41.2644832822215,7.10498248147644));
#59435=CARTESIAN_POINT('Ctrl Pts',(-16.936254577797,41.2595395153907,7.14475632560514));
#59436=CARTESIAN_POINT('Ctrl Pts',(-16.9085954342255,41.2545957485599,7.18628315017448));
#59437=CARTESIAN_POINT('Ctrl Pts',(-16.8834880035964,41.249651981729,7.2292493138958));
#59438=CARTESIAN_POINT('Ctrl Pts',(-16.858366704078,41.244705484051,7.27223921134671));
#59439=CARTESIAN_POINT('Ctrl Pts',(-16.8358001717748,41.2397589863731,7.3166695440082));
#59440=CARTESIAN_POINT('Ctrl Pts',(-16.8159371695144,41.2348124886951,7.36220306550568));
#59441=CARTESIAN_POINT('Ctrl Pts',(-16.7960370638932,41.2298567511406,7.40782164195374));
#59442=CARTESIAN_POINT('Ctrl Pts',(-16.7788507563306,41.2249010135861,7.45454700763435));
#59443=CARTESIAN_POINT('Ctrl Pts',(-16.7644778697622,41.2199452760317,7.50202452404801));
#59444=CARTESIAN_POINT('Ctrl Pts',(-16.7573939362051,41.2175027523677,7.52542466500993));
#59445=CARTESIAN_POINT('Ctrl Pts',(-16.7509926544444,41.2150602287038,7.54900732953798));
#59446=CARTESIAN_POINT('Ctrl Pts',(-16.7452813598676,41.2126177050399,7.57272928211886));
#59447=CARTESIAN_POINT('Ctrl Pts',(-16.7337241625274,41.2076750904343,7.62073228451796));
#59448=CARTESIAN_POINT('Ctrl Pts',(-16.7249444346566,41.2027324758287,7.6695186469948));
#59449=CARTESIAN_POINT('Ctrl Pts',(-16.7190403175229,41.1977898612231,7.71873639179467));
#59450=CARTESIAN_POINT('Ctrl Pts',(-16.7131472161953,41.1928564684676,7.76786230692452));
#59451=CARTESIAN_POINT('Ctrl Pts',(-16.7101191501758,41.1879230757122,7.81741746730105));
#59452=CARTESIAN_POINT('Ctrl Pts',(-16.7100034521229,41.1829896829568,7.86703885491932));
#59453=CARTESIAN_POINT('Ctrl Pts',(-16.7098878732781,41.1780613732669,7.91660911570106));
#59454=CARTESIAN_POINT('Ctrl Pts',(-16.7126787239308,41.173133063577,7.96624492202012));
#59455=CARTESIAN_POINT('Ctrl Pts',(-16.7183714388613,41.1682047538871,8.01557944126555));
#59456=CARTESIAN_POINT('Ctrl Pts',(-16.7240607256338,41.1632794120298,8.06488425121812));
#59457=CARTESIAN_POINT('Ctrl Pts',(-16.7326483523484,41.1583540701725,8.11388758879785));
#59458=CARTESIAN_POINT('Ctrl Pts',(-16.7440778190009,41.1534287283153,8.16222656024821));
#59459=CARTESIAN_POINT('Ctrl Pts',(-16.75550529592,41.1485042439011,8.21055711646151));
#59460=CARTESIAN_POINT('Ctrl Pts',(-16.7697735035174,41.143579759487,8.25822300200199));
#59461=CARTESIAN_POINT('Ctrl Pts',(-16.7867751539815,41.1386552750728,8.30487293183669));
#59462=CARTESIAN_POINT('Ctrl Pts',(-16.8037933529312,41.1337259974324,8.35156826818565));
#59463=CARTESIAN_POINT('Ctrl Pts',(-16.8235501176279,41.1287967197919,8.39724515755078));
#59464=CARTESIAN_POINT('Ctrl Pts',(-16.8458893229295,41.1238674421515,8.44157061869431));
#59465=CARTESIAN_POINT('Ctrl Pts',(-16.8682404570172,41.1189355323538,8.48591974894088));
#59466=CARTESIAN_POINT('Ctrl Pts',(-16.893176501586,41.1140036225562,8.52891553834176));
#59467=CARTESIAN_POINT('Ctrl Pts',(-16.9204962178153,41.1090717127586,8.57025119459823));
#59468=CARTESIAN_POINT('Ctrl Pts',(-16.9478672195076,41.1041305446189,8.61166444749786));
#59469=CARTESIAN_POINT('Ctrl Pts',(-16.9776304941512,41.0991893764792,8.65141090734916));
#59470=CARTESIAN_POINT('Ctrl Pts',(-17.0095434900046,41.0942482083395,8.68921557737121));
#59471=CARTESIAN_POINT('Ctrl Pts',(-17.0260509141496,41.0916923229996,8.70877054881862));
#59472=CARTESIAN_POINT('Ctrl Pts',(-17.0431328973853,41.0891364376597,8.72780655956598));
#59473=CARTESIAN_POINT('Ctrl Pts',(-17.0607521808746,41.0865805523198,8.74628959085061));
#59474=CARTESIAN_POINT('Ctrl Pts',(-17.0948672620246,41.0816317565397,8.78207709109475));
#59475=CARTESIAN_POINT('Ctrl Pts',(-17.1311506442264,41.0766829607596,8.81594838736544));
#59476=CARTESIAN_POINT('Ctrl Pts',(-17.1693586351461,41.0717341649795,8.84763008218228));
#59477=CARTESIAN_POINT('Ctrl Pts',(-17.207496297458,41.0667944783388,8.8792534612009));
#59478=CARTESIAN_POINT('Ctrl Pts',(-17.247551124006,41.0618547916982,8.90869488560116));
#59479=CARTESIAN_POINT('Ctrl Pts',(-17.2892426818714,41.0569151050575,8.93571775224576));
#59480=CARTESIAN_POINT('Ctrl Pts',(-17.3308918826817,41.0519804369527,8.96271316467397));
#59481=CARTESIAN_POINT('Ctrl Pts',(-17.3741740654164,41.047045768848,8.9872945872446));
#59482=CARTESIAN_POINT('Ctrl Pts',(-17.4187775382754,41.0421111007432,9.00926702245602));
#59483=CARTESIAN_POINT('Ctrl Pts',(-17.463354659789,41.0371793479976,9.03122647654302));
#59484=CARTESIAN_POINT('Ctrl Pts',(-17.5092510345198,41.032247595252,9.05057975520432));
#59485=CARTESIAN_POINT('Ctrl Pts',(-17.5561301971801,41.0273158425064,9.06717767697926));
#59486=CARTESIAN_POINT('Ctrl Pts',(-17.6030015944308,41.0223849066926,9.08377284935221));
#59487=CARTESIAN_POINT('Ctrl Pts',(-17.6508549400012,41.0174539708789,9.09761338913787));
#59488=CARTESIAN_POINT('Ctrl Pts',(-17.6993360470047,41.0125230350651,9.1085991060424));
#59489=CARTESIAN_POINT('Ctrl Pts',(-17.7478643829505,41.0075872956712,9.11959552492597));
#59490=CARTESIAN_POINT('Ctrl Pts',(-17.7970211658719,41.0026515562773,9.12773144782443));
#59491=CARTESIAN_POINT('Ctrl Pts',(-17.8464411553264,40.9977158168833,9.13295765368814));
#59492=CARTESIAN_POINT('Ctrl Pts',(-17.895887655359,40.9927774297894,9.13818666306801));
#59493=CARTESIAN_POINT('Ctrl Pts',(-17.9455970953375,40.9878390426955,9.14050282159945));
#59494=CARTESIAN_POINT('Ctrl Pts',(-17.9952018021158,40.9829006556016,9.13990901454098));
#59495=CARTESIAN_POINT('Ctrl Pts',(-18.0448989824159,40.977953062324,9.13931410050226));
#59496=CARTESIAN_POINT('Ctrl Pts',(-18.0944904931126,40.9730054690463,9.13579843234562));
#59497=CARTESIAN_POINT('Ctrl Pts',(-18.1436129898443,40.9680578757686,9.12941684503353));
#59498=CARTESIAN_POINT('Ctrl Pts',(-18.1684823091492,40.965553050379,9.12618602935649));
#59499=CARTESIAN_POINT('Ctrl Pts',(-18.1932315680045,40.9630482249894,9.12222146616022));
#59500=CARTESIAN_POINT('Ctrl Pts',(-18.2178149117059,40.9605433995999,9.11753519700661));
#59501=CARTESIAN_POINT('Ctrl Pts',(-18.266382885828,40.9555947524109,9.10827679010531));
#59502=CARTESIAN_POINT('Ctrl Pts',(-18.3145163539881,40.950646105222,9.09615754486093));
#59503=CARTESIAN_POINT('Ctrl Pts',(-18.3618534959181,40.9456974580331,9.08123404330258));
#59504=CARTESIAN_POINT('Ctrl Pts',(-18.4091054333049,40.9407577181674,9.06633740331808));
#59505=CARTESIAN_POINT('Ctrl Pts',(-18.4555633687124,40.9358179783017,9.04864667986656));
#59506=CARTESIAN_POINT('Ctrl Pts',(-18.5008764485329,40.930878238436,9.02826928016062));
#59507=CARTESIAN_POINT('Ctrl Pts',(-18.5461422178815,40.925943656053,9.0079131560863));
#59508=CARTESIAN_POINT('Ctrl Pts',(-18.5902650016222,40.9210090736699,8.98487613439213));
#59509=CARTESIAN_POINT('Ctrl Pts',(-18.632911998898,40.9160744912869,8.95931442737852));
#59510=CARTESIAN_POINT('Ctrl Pts',(-18.6755365947284,40.9111425009217,8.93376614731687));
#59511=CARTESIAN_POINT('Ctrl Pts',(-18.7166864689408,40.9062105105565,8.90569608701138));
#59512=CARTESIAN_POINT('Ctrl Pts',(-18.7560538356799,40.9012785201913,8.87530614447863));
#59513=CARTESIAN_POINT('Ctrl Pts',(-18.7745591744945,40.8989601494112,8.86102080538415));
#59514=CARTESIAN_POINT('Ctrl Pts',(-18.7926710403453,40.896641778631,8.84622349164109));
#59515=CARTESIAN_POINT('Ctrl Pts',(-18.810359785549,40.8943234078509,8.83093840933902));
#59516=CARTESIAN_POINT('',(-17.1902017145829,41.466,6.87545554732221));
#59517=CARTESIAN_POINT('Origin',(-17.98,41.466,7.87));
#59518=CARTESIAN_POINT('Ctrl Pts',(-17.1902017145829,41.466,6.8754555473222));
#59519=CARTESIAN_POINT('Ctrl Pts',(-17.1488581735048,41.46074845197,6.90828772266504));
#59520=CARTESIAN_POINT('Ctrl Pts',(-17.1095277389328,41.45549690394,6.94373146166701));
#59521=CARTESIAN_POINT('Ctrl Pts',(-17.0725391330082,41.45024535591,6.98150983411271));
#59522=CARTESIAN_POINT('Ctrl Pts',(-17.0369268116997,41.4451892092633,7.0178825360412));
#59523=CARTESIAN_POINT('Ctrl Pts',(-17.0034854613723,41.4401330626166,7.05641875636496));
#59524=CARTESIAN_POINT('Ctrl Pts',(-16.9724723315806,41.43507691597,7.0968324907438));
#59525=CARTESIAN_POINT('Ctrl Pts',(-16.9414666942878,41.4300219908438,7.13723646152047));
#59526=CARTESIAN_POINT('Ctrl Pts',(-16.912888425032,41.4249670657176,7.17951663961273));
#59527=CARTESIAN_POINT('Ctrl Pts',(-16.8869538267822,41.4199121405914,7.22335476247492));
#59528=CARTESIAN_POINT('Ctrl Pts',(-16.8610166860104,41.414856719901,7.26719718304738));
#59529=CARTESIAN_POINT('Ctrl Pts',(-16.8377239906499,41.4098012992106,7.31259740987186));
#59530=CARTESIAN_POINT('Ctrl Pts',(-16.8172469983271,41.4047458785202,7.35921094657329));
#59531=CARTESIAN_POINT('Ctrl Pts',(-16.7967610431176,41.3996882450457,7.40584488626361));
#59532=CARTESIAN_POINT('Ctrl Pts',(-16.7790934417601,41.3946306115713,7.45369272028221));
#59533=CARTESIAN_POINT('Ctrl Pts',(-16.7643672089986,41.3895729780968,7.50239026476135));
#59534=CARTESIAN_POINT('Ctrl Pts',(-16.7496177628025,41.3845073721119,7.55116457274716));
#59535=CARTESIAN_POINT('Ctrl Pts',(-16.7378190830481,41.379441766127,7.60079077170885));
#59536=CARTESIAN_POINT('Ctrl Pts',(-16.7290438642617,41.3743761601421,7.65089101693723));
#59537=CARTESIAN_POINT('Ctrl Pts',(-16.7202606764508,41.3693059539371,7.70103675961648));
#59538=CARTESIAN_POINT('Ctrl Pts',(-16.7145064743903,41.364235747732,7.75165689655593));
#59539=CARTESIAN_POINT('Ctrl Pts',(-16.711802087889,41.3591655415269,7.80236823440583));
#59540=CARTESIAN_POINT('Ctrl Pts',(-16.7090922072103,41.3540850347923,7.85318259639535));
#59541=CARTESIAN_POINT('Ctrl Pts',(-16.7094445054123,41.3490045280577,7.9040880169369));
#59542=CARTESIAN_POINT('Ctrl Pts',(-16.7128277501521,41.3439240213231,7.95470235661039));
#59543=CARTESIAN_POINT('Ctrl Pts',(-16.7137070339155,41.3426036299754,7.96785670118008));
#59544=CARTESIAN_POINT('Ctrl Pts',(-16.7147907711315,41.3412832386277,7.9809914252611));
#59545=CARTESIAN_POINT('Ctrl Pts',(-16.716077846963,41.33996284728,7.99409992369983));
#59546=CARTESIAN_POINT('Ctrl Pts',(-16.7208583168536,41.3350586365668,8.04278763934462));
#59547=CARTESIAN_POINT('Ctrl Pts',(-16.7284689095781,41.3301544258535,8.09132687279746));
#59548=CARTESIAN_POINT('Ctrl Pts',(-16.7388931309886,41.3252502151403,8.13935801397516));
#59549=CARTESIAN_POINT('Ctrl Pts',(-16.7492957772868,41.3203561547196,8.1872897446339));
#59550=CARTESIAN_POINT('Ctrl Pts',(-16.7625003926254,41.3154620942988,8.23471492660863));
#59551=CARTESIAN_POINT('Ctrl Pts',(-16.7784387857867,41.3105680338781,8.28127928284587));
#59552=CARTESIAN_POINT('Ctrl Pts',(-16.7943588359799,41.3056796058692,8.32779004970989));
#59553=CARTESIAN_POINT('Ctrl Pts',(-16.8130062614727,41.3007911778603,8.3734414244914));
#59554=CARTESIAN_POINT('Ctrl Pts',(-16.8342624010277,41.2959027498514,8.4178917359307));
#59555=CARTESIAN_POINT('Ctrl Pts',(-16.8555035418765,41.2910177712033,8.46231068244799));
#59556=CARTESIAN_POINT('Ctrl Pts',(-16.8793495130331,41.2861327925552,8.5055297396731));
#59557=CARTESIAN_POINT('Ctrl Pts',(-16.9056336178924,41.2812478139072,8.54722734513384));
#59558=CARTESIAN_POINT('Ctrl Pts',(-16.9319108774696,41.276364107475,8.58891409110851));
#59559=CARTESIAN_POINT('Ctrl Pts',(-16.9606247132791,41.2714804010429,8.62907969843351));
#59560=CARTESIAN_POINT('Ctrl Pts',(-16.9915639654444,41.2665966946107,8.66742974962811));
#59561=CARTESIAN_POINT('Ctrl Pts',(-17.022531549917,41.2617085159737,8.70581491949443));
#59562=CARTESIAN_POINT('Ctrl Pts',(-17.0557282686084,41.2568203373368,8.74238077681579));
#59563=CARTESIAN_POINT('Ctrl Pts',(-17.0909025557302,41.2519321586998,8.77686588567053));
#59564=CARTESIAN_POINT('Ctrl Pts',(-17.1260939629179,41.2470416008835,8.81136777915358));
#59565=CARTESIAN_POINT('Ctrl Pts',(-17.1632644324539,41.2421510430671,8.84378654025613));
#59566=CARTESIAN_POINT('Ctrl Pts',(-17.2021281422095,41.2372604852507,8.87390008111241));
#59567=CARTESIAN_POINT('Ctrl Pts',(-17.2410661571624,41.2323605769666,8.90407119734194));
#59568=CARTESIAN_POINT('Ctrl Pts',(-17.2817034113001,41.2274606686825,8.93192798131612));
#59569=CARTESIAN_POINT('Ctrl Pts',(-17.3237252953702,41.2225607603984,8.95729182470168));
#59570=CARTESIAN_POINT('Ctrl Pts',(-17.3484102292207,41.2196824051189,8.97219131838266));
#59571=CARTESIAN_POINT('Ctrl Pts',(-17.373572487103,41.2168040498395,8.98623143042253));
#59572=CARTESIAN_POINT('Ctrl Pts',(-17.3991449984387,41.21392569456,8.99938366694457));
#59573=CARTESIAN_POINT('Ctrl Pts',(-17.4431413364607,41.2089736157375,9.02201148930331));
#59574=CARTESIAN_POINT('Ctrl Pts',(-17.4885586565541,41.204021536915,9.04211435978455));
#59575=CARTESIAN_POINT('Ctrl Pts',(-17.5350766527608,41.1990694580926,9.05951385661602));
#59576=CARTESIAN_POINT('Ctrl Pts',(-17.5815084299456,41.1941265577263,9.07688110425956));
#59577=CARTESIAN_POINT('Ctrl Pts',(-17.6290363287014,41.1891836573601,9.09155472662279));
#59578=CARTESIAN_POINT('Ctrl Pts',(-17.6773174249779,41.1842407569939,9.10340312095356));
#59579=CARTESIAN_POINT('Ctrl Pts',(-17.725549052196,41.1793029211487,9.11523937535886));
#59580=CARTESIAN_POINT('Ctrl Pts',(-17.7745318204545,41.1743650853034,9.12425600303587));
#59581=CARTESIAN_POINT('Ctrl Pts',(-17.8239069283246,41.1694272494582,9.13037095847807));
#59582=CARTESIAN_POINT('Ctrl Pts',(-17.8732523604535,41.1644923813825,9.1364822386709));
#59583=CARTESIAN_POINT('Ctrl Pts',(-17.9229891232676,41.1595575133068,9.13969523465749));
#59584=CARTESIAN_POINT('Ctrl Pts',(-17.9727500344444,41.154622645231,9.1399793061304));
#59585=CARTESIAN_POINT('Ctrl Pts',(-18.0225021141912,41.1496886529821,9.14026332718707));
#59586=CARTESIAN_POINT('Ctrl Pts',(-18.0722777871663,41.1447546607332,9.137619453456));
#59587=CARTESIAN_POINT('Ctrl Pts',(-18.1217091818159,41.1398206684844,9.13206913748378));
#59588=CARTESIAN_POINT('Ctrl Pts',(-18.1711875501415,41.1348819875603,9.12651354715616));
#59589=CARTESIAN_POINT('Ctrl Pts',(-18.2203204424377,41.1299433066362,9.11804606179781));
#59590=CARTESIAN_POINT('Ctrl Pts',(-18.2687462450927,41.1250046257122,9.10673991038733));
#59591=CARTESIAN_POINT('Ctrl Pts',(-18.3171974083899,41.1200633583959,9.09542783793383));
#59592=CARTESIAN_POINT('Ctrl Pts',(-18.3649402195001,41.1151220910796,9.08127429396082));
#59593=CARTESIAN_POINT('Ctrl Pts',(-18.4116278165976,41.1101808237633,9.0644025401594));
#59594=CARTESIAN_POINT('Ctrl Pts',(-18.4584011683509,41.105230480446,9.04749979672621));
#59595=CARTESIAN_POINT('Ctrl Pts',(-18.504114934574,41.1002801371287,9.02786909389845));
#59596=CARTESIAN_POINT('Ctrl Pts',(-18.5484433448027,41.0953297938114,9.0056813654144));
#59597=CARTESIAN_POINT('Ctrl Pts',(-18.5706545228201,41.0928493764876,8.99456398979415));
#59598=CARTESIAN_POINT('Ctrl Pts',(-18.5925182992269,41.0903689591638,8.98280535865674));
#59599=CARTESIAN_POINT('Ctrl Pts',(-18.6139964278095,41.08788854184,8.9704310653216));
#59600=CARTESIAN_POINT('Ctrl Pts',(-18.6568995557085,41.0829338428644,8.9457130882606));
#59601=CARTESIAN_POINT('Ctrl Pts',(-18.6984463437109,41.0779791438888,8.9184297097546));
#59602=CARTESIAN_POINT('Ctrl Pts',(-18.7383134522219,41.0730244449132,8.88875448866707));
#59603=CARTESIAN_POINT('Ctrl Pts',(-18.7629963562215,41.0699568444845,8.87038168309808));
#59604=CARTESIAN_POINT('Ctrl Pts',(-18.7870357913132,41.0668892440557,8.85109298601484));
#59605=CARTESIAN_POINT('Ctrl Pts',(-18.810359785549,41.063821643627,8.83093840933902));
#59606=CARTESIAN_POINT('Origin',(-17.98,42.93984859951,7.87));
#59607=CARTESIAN_POINT('',(-18.810359785549,40.1006362902583,8.83093840933902));
#59608=CARTESIAN_POINT('',(-18.8103597856021,40.2713186493562,8.83093840929314));
#59609=CARTESIAN_POINT('',(-18.810359785549,42.93984859951,8.83093840933902));
#59610=CARTESIAN_POINT('',(-19.2499997814169,40.7859014005834,7.87074511808734));
#59611=CARTESIAN_POINT('Ctrl Pts',(-19.2499997814175,40.78590140049,7.87074511714441));
#59612=CARTESIAN_POINT('Ctrl Pts',(-19.2500292717684,40.7809229133116,7.8204808874935));
#59613=CARTESIAN_POINT('Ctrl Pts',(-19.2470703767674,40.7759444261332,7.77021052155451));
#59614=CARTESIAN_POINT('Ctrl Pts',(-19.2411472950103,40.7709659389547,7.72030864992208));
#59615=CARTESIAN_POINT('Ctrl Pts',(-19.234951069999,40.7657578685552,7.6681055506235));
#59616=CARTESIAN_POINT('Ctrl Pts',(-19.2255106220564,40.7605497981556,7.61630639720772));
#59617=CARTESIAN_POINT('Ctrl Pts',(-19.2129139779418,40.755341727756,7.56533112565334));
#59618=CARTESIAN_POINT('Ctrl Pts',(-19.2008516061128,40.7503545517193,7.51651791207196));
#59619=CARTESIAN_POINT('Ctrl Pts',(-19.185895653102,40.7453673756826,7.46846059818919));
#59620=CARTESIAN_POINT('Ctrl Pts',(-19.1681744271675,40.7403801996459,7.42151195040994));
#59621=CARTESIAN_POINT('Ctrl Pts',(-19.1504375370169,40.7353886153248,7.37452180359616));
#59622=CARTESIAN_POINT('Ctrl Pts',(-19.1299307302168,40.7303970310037,7.32864275755956));
#59623=CARTESIAN_POINT('Ctrl Pts',(-19.1068294753863,40.7254054466826,7.28420538291932));
#59624=CARTESIAN_POINT('Ctrl Pts',(-19.0836825292143,40.7204039896431,7.23968011680862));
#59625=CARTESIAN_POINT('Ctrl Pts',(-19.0579311765533,40.7154025326036,7.19660266311589));
#59626=CARTESIAN_POINT('Ctrl Pts',(-19.0297946982172,40.7104010755641,7.15527551350531));
#59627=CARTESIAN_POINT('Ctrl Pts',(-19.0261718104269,40.7097570817627,7.14995417854845));
#59628=CARTESIAN_POINT('Ctrl Pts',(-19.0225094325684,40.7091130879613,7.14466181686219));
#59629=CARTESIAN_POINT('Ctrl Pts',(-19.0188080796698,40.7084690941599,7.13939903256795));
#59630=CARTESIAN_POINT('Ctrl Pts',(-18.9903689402581,40.7035210035561,7.09896272175442));
#59631=CARTESIAN_POINT('Ctrl Pts',(-18.9595023877379,40.6985729129523,7.06010002379334));
#59632=CARTESIAN_POINT('Ctrl Pts',(-18.9264088784134,40.6936248223485,7.02311734292156));
#59633=CARTESIAN_POINT('Ctrl Pts',(-18.8933762760976,40.6886858384669,6.98620272689119));
#59634=CARTESIAN_POINT('Ctrl Pts',(-18.8581252083308,40.6837468545854,6.95116167046038));
#59635=CARTESIAN_POINT('Ctrl Pts',(-18.8208979175303,40.6788078707038,6.91826963256748));
#59636=CARTESIAN_POINT('Ctrl Pts',(-18.7837084376806,40.6738739032409,6.88541100240317));
#59637=CARTESIAN_POINT('Ctrl Pts',(-18.744547117042,40.6689399357781,6.85469743083038));
#59638=CARTESIAN_POINT('Ctrl Pts',(-18.7036932738055,40.6640059683152,6.82636785913397));
#59639=CARTESIAN_POINT('Ctrl Pts',(-18.6628635413039,40.6590749127345,6.79805500671626));
#59640=CARTESIAN_POINT('Ctrl Pts',(-18.6203437144694,40.6541438571539,6.77212367858167));
#59641=CARTESIAN_POINT('Ctrl Pts',(-18.576444394999,40.6492128015733,6.74877117247448));
#59642=CARTESIAN_POINT('Ctrl Pts',(-18.5325523052841,40.6442825580856,6.72542251227902));
#59643=CARTESIAN_POINT('Ctrl Pts',(-18.4872816579289,40.6393523145978,6.70465208730612));
#59644=CARTESIAN_POINT('Ctrl Pts',(-18.4409678318851,40.6344220711101,6.68661136647036));
#59645=CARTESIAN_POINT('Ctrl Pts',(-18.3946087602894,40.6294870110999,6.66855302104083));
#59646=CARTESIAN_POINT('Ctrl Pts',(-18.3472049871667,40.6245519510896,6.65322990253454));
#59647=CARTESIAN_POINT('Ctrl Pts',(-18.2991103659587,40.6196168910793,6.64074470741929));
#59648=CARTESIAN_POINT('Ctrl Pts',(-18.2509898794041,40.6146791769877,6.6282527977507));
#59649=CARTESIAN_POINT('Ctrl Pts',(-18.2021783430207,40.6097414628961,6.61860195709194));
#59650=CARTESIAN_POINT('Ctrl Pts',(-18.1530397230229,40.6048037488044,6.61184370833502));
#59651=CARTESIAN_POINT('Ctrl Pts',(-18.1038093074305,40.5998568105954,6.60507283452957));
#59652=CARTESIAN_POINT('Ctrl Pts',(-18.0542511352957,40.5949098723863,6.6012053802761));
#59653=CARTESIAN_POINT('Ctrl Pts',(-18.0047325749995,40.5899629341773,6.60024084971445));
#59654=CARTESIAN_POINT('Ctrl Pts',(-17.9796043103234,40.5874526032648,6.59975139729304));
#59655=CARTESIAN_POINT('Ctrl Pts',(-17.9544862158352,40.5849422723523,6.60000863318833));
#59656=CARTESIAN_POINT('Ctrl Pts',(-17.9294257401133,40.5824319414398,6.6010073899991));
#59657=CARTESIAN_POINT('Ctrl Pts',(-17.8800299431995,40.5774839190114,6.60297600341003));
#59658=CARTESIAN_POINT('Ctrl Pts',(-17.8306400654593,40.5725358965829,6.60783739216335));
#59659=CARTESIAN_POINT('Ctrl Pts',(-17.7816222424847,40.5675878741545,6.61558927566638));
#59660=CARTESIAN_POINT('Ctrl Pts',(-17.7326946132916,40.562648956187,6.62332689554764));
#59661=CARTESIAN_POINT('Ctrl Pts',(-17.6841382179459,40.5577100382194,6.63394437677166));
#59662=CARTESIAN_POINT('Ctrl Pts',(-17.6363158496529,40.5527711202519,6.64738754922084));
#59663=CARTESIAN_POINT('Ctrl Pts',(-17.5885420400171,40.5478372172436,6.66081707152211));
#59664=CARTESIAN_POINT('Ctrl Pts',(-17.5415013069363,40.5429033142352,6.67706645745127));
#59665=CARTESIAN_POINT('Ctrl Pts',(-17.4955458646341,40.5379694112268,6.69603058356408));
#59666=CARTESIAN_POINT('Ctrl Pts',(-17.4496175294702,40.5330384185156,6.7149835235548));
#59667=CARTESIAN_POINT('Ctrl Pts',(-17.4047737224866,40.5281074258043,6.73664782283407));
#59668=CARTESIAN_POINT('Ctrl Pts',(-17.3613486310191,40.523176433093,6.76086949205333));
#59669=CARTESIAN_POINT('Ctrl Pts',(-17.3179306762151,40.518246250762,6.78508718058086));
#59670=CARTESIAN_POINT('Ctrl Pts',(-17.2759314518796,40.513316068431,6.81186113701932));
#59671=CARTESIAN_POINT('Ctrl Pts',(-17.2356600737474,40.5083858861,6.84099170353868));
#59672=CARTESIAN_POINT('Ctrl Pts',(-17.1953493273036,40.5034508841436,6.87015074738542));
#59673=CARTESIAN_POINT('Ctrl Pts',(-17.1567702437983,40.4985158821873,6.901670678426));
#59674=CARTESIAN_POINT('Ctrl Pts',(-17.1202009765152,40.4935808802309,6.93530986994908));
#59675=CARTESIAN_POINT('Ctrl Pts',(-17.0836120295355,40.4886432225106,6.9689671643529));
#59676=CARTESIAN_POINT('Ctrl Pts',(-17.0490354337303,40.4837055647903,7.0047455958323));
#59677=CARTESIAN_POINT('Ctrl Pts',(-17.0167118280288,40.47876790707,7.04236729297323));
#59678=CARTESIAN_POINT('Ctrl Pts',(-16.9843278164935,40.4738210219344,7.08005929693602));
#59679=CARTESIAN_POINT('Ctrl Pts',(-16.9542055306432,40.4688741367989,7.11960100553891));
#59680=CARTESIAN_POINT('Ctrl Pts',(-16.9265437463089,40.4639272516634,7.16068348280958));
#59681=CARTESIAN_POINT('Ctrl Pts',(-16.9125038431012,40.4614164306822,7.18153513856123));
#59682=CARTESIAN_POINT('Ctrl Pts',(-16.8990970792571,40.458905609701,7.20278328899552));
#59683=CARTESIAN_POINT('Ctrl Pts',(-16.8863448531053,40.4563947887199,7.2243852389616));
#59684=CARTESIAN_POINT('Ctrl Pts',(-16.8612152184356,40.4514469456354,7.26695420726064));
#59685=CARTESIAN_POINT('Ctrl Pts',(-16.8385191063271,40.4464991025508,7.31108675266179));
#59686=CARTESIAN_POINT('Ctrl Pts',(-16.8184531478053,40.4415512594663,7.35647404139954));
#59687=CARTESIAN_POINT('Ctrl Pts',(-16.7984241350082,40.43661252642,7.40177776242349));
#59688=CARTESIAN_POINT('Ctrl Pts',(-16.7810158909585,40.4316737933737,7.4483311476469));
#59689=CARTESIAN_POINT('Ctrl Pts',(-16.7663796379728,40.4267350603274,7.49580003090198));
#59690=CARTESIAN_POINT('Ctrl Pts',(-16.7517582569089,40.4218013455362,7.54322068094346));
#59691=CARTESIAN_POINT('Ctrl Pts',(-16.7399034516814,40.416867630745,7.59155446629698));
#59692=CARTESIAN_POINT('Ctrl Pts',(-16.73091789783,40.4119339159538,7.64044847628775));
#59693=CARTESIAN_POINT('Ctrl Pts',(-16.7219376497172,40.4070031143944,7.6893136156227));
#59694=CARTESIAN_POINT('Ctrl Pts',(-16.7158233955496,40.4020723128349,7.73873778628424));
#59695=CARTESIAN_POINT('Ctrl Pts',(-16.7126269786028,40.3971415112754,7.78835672327441));
#59696=CARTESIAN_POINT('Ctrl Pts',(-16.7094310886601,40.392211522674,7.83796747942134));
#59697=CARTESIAN_POINT('Ctrl Pts',(-16.7091521151252,40.3872815340726,7.8877723914887));
#59698=CARTESIAN_POINT('Ctrl Pts',(-16.711789934967,40.3823515454712,7.93740349359653));
#59699=CARTESIAN_POINT('Ctrl Pts',(-16.7144303323067,40.3774167396208,7.9870830918365));
#59700=CARTESIAN_POINT('Ctrl Pts',(-16.7199931834056,40.3724819337704,8.03658799276528));
#59701=CARTESIAN_POINT('Ctrl Pts',(-16.7284263127276,40.3675471279199,8.08555348600119));
#59702=CARTESIAN_POINT('Ctrl Pts',(-16.7368639777004,40.3626096679472,8.13454531470192));
#59703=CARTESIAN_POINT('Ctrl Pts',(-16.7481748702453,40.3576722079745,8.18299662378046));
#59704=CARTESIAN_POINT('Ctrl Pts',(-16.7622560188676,40.3527347480018,8.23055456787554));
#59705=CARTESIAN_POINT('Ctrl Pts',(-16.7763634825116,40.3477880608439,8.27820138883457));
#59706=CARTESIAN_POINT('Ctrl Pts',(-16.7932513487559,40.342841373686,8.32495099692852));
#59707=CARTESIAN_POINT('Ctrl Pts',(-16.8127678444057,40.3378946865281,8.37046887510291));
#59708=CARTESIAN_POINT('Ctrl Pts',(-16.8226799875669,40.335382336352,8.39358674077668));
#59709=CARTESIAN_POINT('Ctrl Pts',(-16.8332694302267,40.3328699861759,8.41638725639511));
#59710=CARTESIAN_POINT('Ctrl Pts',(-16.8445118559991,40.3303576359998,8.43882921411729));
#59711=CARTESIAN_POINT('Ctrl Pts',(-16.8666532967774,40.3254096778132,8.48302761826214));
#59712=CARTESIAN_POINT('Ctrl Pts',(-16.8914281664316,40.3204617196265,8.52602906244405));
#59713=CARTESIAN_POINT('Ctrl Pts',(-16.9186835779852,40.3155137614398,8.56750086190748));
#59714=CARTESIAN_POINT('Ctrl Pts',(-16.9458888212654,40.3105749108214,8.60889632539012));
#59715=CARTESIAN_POINT('Ctrl Pts',(-16.9755652522928,40.3056360602029,8.64876727415595));
#59716=CARTESIAN_POINT('Ctrl Pts',(-17.0075140777037,40.3006972095844,8.68680544252321));
#59717=CARTESIAN_POINT('Ctrl Pts',(-17.0394304498725,40.2957633757924,8.72480497216521));
#59718=CARTESIAN_POINT('Ctrl Pts',(-17.0736142961015,40.2908295420005,8.76097498935866));
#59719=CARTESIAN_POINT('Ctrl Pts',(-17.1098247504854,40.2858957082085,8.79503785605357));
#59720=CARTESIAN_POINT('Ctrl Pts',(-17.1460138328477,40.2809647864486,8.82908061826942));
#59721=CARTESIAN_POINT('Ctrl Pts',(-17.1842267553722,40.2760338646886,8.86101831898162));
#59722=CARTESIAN_POINT('Ctrl Pts',(-17.2241855496806,40.2711029429287,8.89060987487303));
#59723=CARTESIAN_POINT('Ctrl Pts',(-17.2641377638907,40.2661728331539,8.92019655786101));
#59724=CARTESIAN_POINT('Ctrl Pts',(-17.3058348384027,40.2612427233792,8.94743753785365));
#59725=CARTESIAN_POINT('Ctrl Pts',(-17.3489675178731,40.2563126136045,8.97213338870606));
#59726=CARTESIAN_POINT('Ctrl Pts',(-17.392142347096,40.2513776860695,8.99685337262922));
#59727=CARTESIAN_POINT('Ctrl Pts',(-17.4367551053224,40.2464427585345,9.01902298964242));
#59728=CARTESIAN_POINT('Ctrl Pts',(-17.4824710481861,40.2415078309995,9.03848831492104));
#59729=CARTESIAN_POINT('Ctrl Pts',(-17.5282115825324,40.2365702488724,9.05796411097146));
#59730=CARTESIAN_POINT('Ctrl Pts',(-17.5750559667399,40.2316326667453,9.07473253367482));
#59731=CARTESIAN_POINT('Ctrl Pts',(-17.6226518823375,40.2266950846181,9.08868877191967));
#59732=CARTESIAN_POINT('Ctrl Pts',(-17.6703367367258,40.2217482760148,9.10267108910292));
#59733=CARTESIAN_POINT('Ctrl Pts',(-17.7187753910701,40.2168014674114,9.11383061058746));
#59734=CARTESIAN_POINT('Ctrl Pts',(-17.767604464576,40.2118546588081,9.12211346791413));
#59735=CARTESIAN_POINT('Ctrl Pts',(-17.7923939696334,40.2093432669653,9.12631850230956));
#59736=CARTESIAN_POINT('Ctrl Pts',(-17.817284006811,40.2068318751226,9.12978294105041));
#59737=CARTESIAN_POINT('Ctrl Pts',(-17.8422268232743,40.2043204832799,9.13250487198066));
#59738=CARTESIAN_POINT('Ctrl Pts',(-17.8913534837793,40.1993741174741,9.1378659095734));
#59739=CARTESIAN_POINT('Ctrl Pts',(-17.9409021352363,40.1944277516684,9.14036708668766));
#59740=CARTESIAN_POINT('Ctrl Pts',(-17.9905106969094,40.1894813858626,9.13995650525933));
#59741=CARTESIAN_POINT('Ctrl Pts',(-18.0400449886139,40.18454242536,9.13954653852064));
#59742=CARTESIAN_POINT('Ctrl Pts',(-18.0896384699735,40.1796034648573,9.13623344728117));
#59743=CARTESIAN_POINT('Ctrl Pts',(-18.1389243096997,40.1746645043546,9.13001708868827));
#59744=CARTESIAN_POINT('Ctrl Pts',(-18.1881573429765,40.1697308356146,9.12380739050388));
#59745=CARTESIAN_POINT('Ctrl Pts',(-18.2370828464377,40.1647971668746,9.11470065464772));
#59746=CARTESIAN_POINT('Ctrl Pts',(-18.2853369673953,40.1598634981346,9.10274869147845));
#59747=CARTESIAN_POINT('Ctrl Pts',(-18.3336099836073,40.1549278974782,9.0907920481828));
#59748=CARTESIAN_POINT('Ctrl Pts',(-18.3812105498021,40.1499922968219,9.07598804149137));
#59749=CARTESIAN_POINT('Ctrl Pts',(-18.42778436983,40.1450566961655,9.05843979996295));
#59750=CARTESIAN_POINT('Ctrl Pts',(-18.4743157618438,40.1401255917633,9.04090754460523));
#59751=CARTESIAN_POINT('Ctrl Pts',(-18.5198217640123,40.1351944873612,9.02063624598971));
#59752=CARTESIAN_POINT('Ctrl Pts',(-18.5639669334419,40.130263382959,8.99777773548093));
#59753=CARTESIAN_POINT('Ctrl Pts',(-18.6081724812026,40.1253255341755,8.97488796087836));
#59754=CARTESIAN_POINT('Ctrl Pts',(-18.651012987107,40.1203876853921,8.94940415445937));
#59755=CARTESIAN_POINT('Ctrl Pts',(-18.6921770859854,40.1154498366086,8.92152451145817));
#59756=CARTESIAN_POINT('Ctrl Pts',(-18.7333411848638,40.1105119878252,8.89364486845697));
#59757=CARTESIAN_POINT('Ctrl Pts',(-18.7728284521389,40.1055741390417,8.86336973860931));
#59758=CARTESIAN_POINT('Ctrl Pts',(-18.810359785549,40.1006362902583,8.83093840933902));
#59759=CARTESIAN_POINT('Ctrl Pts',(-18.810359785549,40.8943234078509,8.83093840933902));
#59760=CARTESIAN_POINT('Ctrl Pts',(-18.8483926190765,40.8893386444367,8.79807372708177));
#59761=CARTESIAN_POINT('Ctrl Pts',(-18.8844667877788,40.8843538810224,8.76295164180727));
#59762=CARTESIAN_POINT('Ctrl Pts',(-18.9183146859056,40.8793691176081,8.72584201241465));
#59763=CARTESIAN_POINT('Ctrl Pts',(-18.9518376889585,40.8744322013326,8.68908858640387));
#59764=CARTESIAN_POINT('Ctrl Pts',(-18.9831766720718,40.8694952850571,8.65038607854338));
#59765=CARTESIAN_POINT('Ctrl Pts',(-19.0121121380009,40.8645583687816,8.61003009032823));
#59766=CARTESIAN_POINT('Ctrl Pts',(-19.0414682549524,40.859549681798,8.56908742458229));
#59767=CARTESIAN_POINT('Ctrl Pts',(-19.0683500745277,40.8545409948143,8.52644329266378));
#59768=CARTESIAN_POINT('Ctrl Pts',(-19.0925755837736,40.8495323078307,8.48243413555332));
#59769=CARTESIAN_POINT('Ctrl Pts',(-19.1168010930194,40.8445236208471,8.43842497844286));
#59770=CARTESIAN_POINT('Ctrl Pts',(-19.1383701029171,40.8395149338635,8.39305134970394));
#59771=CARTESIAN_POINT('Ctrl Pts',(-19.157151668176,40.8345062468798,8.34666964462862));
#59772=CARTESIAN_POINT('Ctrl Pts',(-19.177972122364,40.8289538269166,8.29525283498756));
#59773=CARTESIAN_POINT('Ctrl Pts',(-19.1954458292539,40.8234014069534,8.24240611743118));
#59774=CARTESIAN_POINT('Ctrl Pts',(-19.2093998643273,40.8178489869902,8.18855293687549));
#59775=CARTESIAN_POINT('Ctrl Pts',(-19.2232553640092,40.8123357750318,8.13508003659026));
#59776=CARTESIAN_POINT('Ctrl Pts',(-19.2336405829136,40.8068225630735,8.08061511205944));
#59777=CARTESIAN_POINT('Ctrl Pts',(-19.2404326460799,40.8013093511151,8.02559416665144));
#59778=CARTESIAN_POINT('Ctrl Pts',(-19.2467599784388,40.7961733676046,7.97433789889201));
#59779=CARTESIAN_POINT('Ctrl Pts',(-19.249969358089,40.791037384094,7.92259947572652));
#59780=CARTESIAN_POINT('Ctrl Pts',(-19.2499997814169,40.7859014005834,7.87074511808734));
#59781=CARTESIAN_POINT('',(-19.2499999197349,40.9554735995101,7.87045152332722));
#59782=CARTESIAN_POINT('Ctrl Pts',(-18.810359785549,41.063821643627,8.83093840933902));
#59783=CARTESIAN_POINT('Ctrl Pts',(-18.8479499855859,41.0588777342526,8.79845621262589));
#59784=CARTESIAN_POINT('Ctrl Pts',(-18.8836800735341,41.0539338248782,8.76372296388289));
#59785=CARTESIAN_POINT('Ctrl Pts',(-18.9172735335047,41.0489899155038,8.72698210214193));
#59786=CARTESIAN_POINT('Ctrl Pts',(-18.9508427414233,41.044049575275,8.69026776464973));
#59787=CARTESIAN_POINT('Ctrl Pts',(-18.9822780092121,41.0391092350461,8.65154908674822));
#59788=CARTESIAN_POINT('Ctrl Pts',(-19.0113395539479,41.0341688948173,8.61110641912118));
#59789=CARTESIAN_POINT('Ctrl Pts',(-19.040392367812,41.0292300387998,8.57067590156185));
#59790=CARTESIAN_POINT('Ctrl Pts',(-19.0670725549055,41.0242911827824,8.52852286460955));
#59791=CARTESIAN_POINT('Ctrl Pts',(-19.091182129228,41.0193523267649,8.48495875933612));
#59792=CARTESIAN_POINT('Ctrl Pts',(-19.1153130085742,41.0144091064048,8.44135615756007));
#59793=CARTESIAN_POINT('Ctrl Pts',(-19.1368684688677,41.0094658860446,8.39634047332026));
#59794=CARTESIAN_POINT('Ctrl Pts',(-19.1556961153788,41.0045226656845,8.35024852345759));
#59795=CARTESIAN_POINT('Ctrl Pts',(-19.1745314548344,40.9995774255329,8.30413774050222));
#59796=CARTESIAN_POINT('Ctrl Pts',(-19.1906365789394,40.9946321853813,8.25695033198814));
#59797=CARTESIAN_POINT('Ctrl Pts',(-19.2039082916343,40.9896869452297,8.20904054870888));
#59798=CARTESIAN_POINT('Ctrl Pts',(-19.2172064675032,40.9847318445007,8.16103523556413));
#59799=CARTESIAN_POINT('Ctrl Pts',(-19.2276598262009,40.9797767437717,8.11230520480288));
#59800=CARTESIAN_POINT('Ctrl Pts',(-19.235216157106,40.9748216430426,8.06321593862808));
#59801=CARTESIAN_POINT('Ctrl Pts',(-19.241809197014,40.9704982250684,8.02038463663699));
#59802=CARTESIAN_POINT('Ctrl Pts',(-19.2461975587629,40.9661748070942,7.97728021341245));
#59803=CARTESIAN_POINT('Ctrl Pts',(-19.2483789912293,40.96185138912,7.93414619714567));
#59804=CARTESIAN_POINT('Ctrl Pts',(-19.2494516546792,40.95972545925,7.91293615126488));
#59805=CARTESIAN_POINT('Ctrl Pts',(-19.2499923657969,40.95759952938,7.89169848919924));
#59806=CARTESIAN_POINT('Ctrl Pts',(-19.2499999197349,40.9554735995101,7.87045152332722));
#59807=CARTESIAN_POINT('Ctrl Pts',(-19.2499998766701,40.9543644179868,7.87055969442492));
#59808=CARTESIAN_POINT('Ctrl Pts',(-19.250007281152,40.9527258740035,7.85375822096658));
#59809=CARTESIAN_POINT('Ctrl Pts',(-19.2496812724635,40.9511020712888,7.83695686015624));
#59810=CARTESIAN_POINT('Ctrl Pts',(-19.2462699092907,40.9427582088214,7.75008733675439));
#59811=CARTESIAN_POINT('Ctrl Pts',(-19.237717536916,40.9362295709881,7.68034909395144));
#59812=CARTESIAN_POINT('Ctrl Pts',(-19.2140602666449,40.9253330909973,7.56647835519206));
#59813=CARTESIAN_POINT('Ctrl Pts',(-19.202216554662,40.9209996991522,7.52183874183336));
#59814=CARTESIAN_POINT('Ctrl Pts',(-19.1774953312972,40.9133763697255,7.44566946610432));
#59815=CARTESIAN_POINT('Ctrl Pts',(-19.165731729046,40.9101174368386,7.41382976234178));
#59816=CARTESIAN_POINT('Ctrl Pts',(-19.1452338292564,40.9049227256803,7.36452069340626));
#59817=CARTESIAN_POINT('Ctrl Pts',(-19.137346857584,40.9030155713523,7.34671484396063));
#59818=CARTESIAN_POINT('Ctrl Pts',(-19.1213350143937,40.8993056729837,7.31270037717588));
#59819=CARTESIAN_POINT('Ctrl Pts',(-19.1132662153869,40.8975052764277,7.29647050445557));
#59820=CARTESIAN_POINT('Ctrl Pts',(-19.0929460119853,40.8931265728803,7.25770181112711));
#59821=CARTESIAN_POINT('Ctrl Pts',(-19.0803542564405,40.8905367239873,7.23535193864384));
#59822=CARTESIAN_POINT('Ctrl Pts',(-19.0261873612767,40.8798599412999,7.1456707768098));
#59823=CARTESIAN_POINT('Ctrl Pts',(-18.9790474763241,40.8715799850507,7.08192647799003));
#59824=CARTESIAN_POINT('Ctrl Pts',(-18.8943595007561,40.8581880742321,6.98731096414885));
#59825=CARTESIAN_POINT('Ctrl Pts',(-18.8604273929855,40.8531292207383,6.95346233473273));
#59826=CARTESIAN_POINT('Ctrl Pts',(-18.8033411659183,40.8451515924129,6.90261974323977));
#59827=CARTESIAN_POINT('Ctrl Pts',(-18.7813823505824,40.8421960567695,6.88435201438156));
#59828=CARTESIAN_POINT('Ctrl Pts',(-18.7489435810057,40.8380068978013,6.85916755787131));
#59829=CARTESIAN_POINT('Ctrl Pts',(-18.7389498837332,40.8367393093728,6.85164270652434));
#59830=CARTESIAN_POINT('Ctrl Pts',(-18.7205139141966,40.8344446474489,6.83818336616758));
#59831=CARTESIAN_POINT('Ctrl Pts',(-18.7121084929173,40.8334148378287,6.83220252700361));
#59832=CARTESIAN_POINT('Ctrl Pts',(-18.6910604241126,40.8308746016824,6.81760890219221));
#59833=CARTESIAN_POINT('Ctrl Pts',(-18.6783332987314,40.8293721754493,6.80912082099662));
#59834=CARTESIAN_POINT('Ctrl Pts',(-18.5949136776903,40.8197163394275,6.75563802088071));
#59835=CARTESIAN_POINT('Ctrl Pts',(-18.5200556333534,40.8119210932889,6.71749542843296));
#59836=CARTESIAN_POINT('Ctrl Pts',(-18.3976613609614,40.7996096983438,6.669699279121));
#59837=CARTESIAN_POINT('Ctrl Pts',(-18.352417038883,40.7951457148352,6.65490008525363));
#59838=CARTESIAN_POINT('Ctrl Pts',(-18.2729820548916,40.7873232382475,6.63377145556607));
#59839=CARTESIAN_POINT('Ctrl Pts',(-18.2391654813188,40.7839979816903,6.62624267728335));
#59840=CARTESIAN_POINT('Ctrl Pts',(-18.1857077137223,40.7787145261421,6.61661575641215));
#59841=CARTESIAN_POINT('Ctrl Pts',(-18.1662515355845,40.7767862242785,6.61357730622942));
#59842=CARTESIAN_POINT('Ctrl Pts',(-18.1286401191192,40.7730424553114,6.60859632115452));
#59843=CARTESIAN_POINT('Ctrl Pts',(-18.1104980615269,40.771229477806,6.6065906074063));
#59844=CARTESIAN_POINT('Ctrl Pts',(-18.0666762831058,40.7668287232122,6.60269971202443));
#59845=CARTESIAN_POINT('Ctrl Pts',(-18.0409715279906,40.7642295026928,6.60120331651778));
#59846=CARTESIAN_POINT('Ctrl Pts',(-17.942139920233,40.7541555756746,6.59845977091006));
#59847=CARTESIAN_POINT('Ctrl Pts',(-17.8690144642146,40.7465223802064,6.60274861594604));
#59848=CARTESIAN_POINT('Ctrl Pts',(-17.7460325529543,40.7334339939283,6.62068866460258));
#59849=CARTESIAN_POINT('Ctrl Pts',(-17.6958778722398,40.7280265944951,6.63113172465954));
#59850=CARTESIAN_POINT('Ctrl Pts',(-17.6178891172514,40.719589979437,6.65235710478228));
#59851=CARTESIAN_POINT('Ctrl Pts',(-17.5895674321675,40.7165207402653,6.66114047979514));
#59852=CARTESIAN_POINT('Ctrl Pts',(-17.5495570824783,40.7121975221576,6.67510212248155));
#59853=CARTESIAN_POINT('Ctrl Pts',(-17.5376010403528,40.7109073363997,6.67947690003055));
#59854=CARTESIAN_POINT('Ctrl Pts',(-17.5160476616713,40.7085868903455,6.68773297001442));
#59855=CARTESIAN_POINT('Ctrl Pts',(-17.5064293721965,40.7075536293404,6.69155272397297));
#59856=CARTESIAN_POINT('Ctrl Pts',(-17.4827808638863,40.7050171999904,6.70128069411211));
#59857=CARTESIAN_POINT('Ctrl Pts',(-17.468808174912,40.7035218213224,6.70732434393366));
#59858=CARTESIAN_POINT('Ctrl Pts',(-17.3780745486415,40.6938099009134,6.74852182997586));
#59859=CARTESIAN_POINT('Ctrl Pts',(-17.3048593364787,40.6859576526881,6.79101059244738));
#59860=CARTESIAN_POINT('Ctrl Pts',(-17.1981270169557,40.6736195900199,6.86810039523383));
#59861=CARTESIAN_POINT('Ctrl Pts',(-17.161434467363,40.6691886772591,6.89784873872427));
#59862=CARTESIAN_POINT('Ctrl Pts',(-17.1009752694255,40.661417041168,6.95272017823123));
#59863=CARTESIAN_POINT('Ctrl Pts',(-17.0764210128806,40.6581089290884,6.97689793695855));
#59864=CARTESIAN_POINT('Ctrl Pts',(-17.0394582020459,40.6528476076009,7.01638010686075));
#59865=CARTESIAN_POINT('Ctrl Pts',(-17.0263698521508,40.650923917104,7.03102727588699));
#59866=CARTESIAN_POINT('Ctrl Pts',(-17.001797087242,40.6471865283621,7.05984477166056));
#59867=CARTESIAN_POINT('Ctrl Pts',(-16.9902678896433,40.6453752741507,7.07397067030402));
#59868=CARTESIAN_POINT('Ctrl Pts',(-16.9631973777922,40.6409752495249,7.10863569012619));
#59869=CARTESIAN_POINT('Ctrl Pts',(-16.9479698553032,40.6383749734931,7.12940786002853));
#59870=CARTESIAN_POINT('Ctrl Pts',(-16.8897069021195,40.6278930980094,7.21417447723697));
#59871=CARTESIAN_POINT('Ctrl Pts',(-16.851915671158,40.6198314044893,7.28155527115836));
#59872=CARTESIAN_POINT('Ctrl Pts',(-16.800551421224,40.6065601178852,7.39651735041782));
#59873=CARTESIAN_POINT('Ctrl Pts',(-16.7832179507076,40.6014021537742,7.44221741792405));
#59874=CARTESIAN_POINT('Ctrl Pts',(-16.7598888472047,40.5932916840693,7.5163573503009));
#59875=CARTESIAN_POINT('Ctrl Pts',(-16.7521603467498,40.5903016996136,7.5442017044723));
#59876=CARTESIAN_POINT('Ctrl Pts',(-16.7424328183009,40.5860688653072,7.58454186948642));
#59877=CARTESIAN_POINT('Ctrl Pts',(-16.7396604500834,40.5847915379565,7.59683938523784));
#59878=CARTESIAN_POINT('Ctrl Pts',(-16.734948470425,40.5824851121012,7.61929390362714));
#59879=CARTESIAN_POINT('Ctrl Pts',(-16.7329491645861,40.5814531783995,7.62943589092593));
#59880=CARTESIAN_POINT('Ctrl Pts',(-16.7282966901755,40.5789097129878,7.65465576906936));
#59881=CARTESIAN_POINT('Ctrl Pts',(-16.7257918572627,40.5774061670467,7.6697593257701));
#59882=CARTESIAN_POINT('Ctrl Pts',(-16.7113812272796,40.567771734605,7.76758021481907));
#59883=CARTESIAN_POINT('Ctrl Pts',(-16.7073892850552,40.5599971284281,7.85127138567328));
#59884=CARTESIAN_POINT('Ctrl Pts',(-16.7140799847703,40.5477039213984,7.98230784505999));
#59885=CARTESIAN_POINT('Ctrl Pts',(-16.7191790746373,40.5432366545736,8.02967639823069));
#59886=CARTESIAN_POINT('Ctrl Pts',(-16.732558520168,40.535411754879,8.11080842291858));
#59887=CARTESIAN_POINT('Ctrl Pts',(-16.7395867608868,40.5320874869395,8.14472434230894));
#59888=CARTESIAN_POINT('Ctrl Pts',(-16.7527623240707,40.5268085748212,8.19737439431743));
#59889=CARTESIAN_POINT('Ctrl Pts',(-16.7579753712203,40.5248838983516,8.21632644815318));
#59890=CARTESIAN_POINT('Ctrl Pts',(-16.7688567994311,40.521149563144,8.25257439568354));
#59891=CARTESIAN_POINT('Ctrl Pts',(-16.7744613965734,40.5193424201344,8.26988449347853));
#59892=CARTESIAN_POINT('Ctrl Pts',(-16.7888438506188,40.5149617668288,8.31125117182886));
#59893=CARTESIAN_POINT('Ctrl Pts',(-16.7979808072105,40.5123769574935,8.33517303564982));
#59894=CARTESIAN_POINT('Ctrl Pts',(-16.8387002840066,40.5015980456084,8.43282028008869));
#59895=CARTESIAN_POINT('Ctrl Pts',(-16.8765024211767,40.4932057546648,8.50373462868146));
#59896=CARTESIAN_POINT('Ctrl Pts',(-16.9466106994287,40.4798075664947,8.60973526833562));
#59897=CARTESIAN_POINT('Ctrl Pts',(-16.9746459313085,40.4748543221235,8.64740939108677));
#59898=CARTESIAN_POINT('Ctrl Pts',(-17.0227857036458,40.4670154608755,8.70512741450899));
#59899=CARTESIAN_POINT('Ctrl Pts',(-17.0415882024122,40.4640946704907,8.72620130750585));
#59900=CARTESIAN_POINT('Ctrl Pts',(-17.0697104785887,40.4599400032964,8.75568014811557));
#59901=CARTESIAN_POINT('Ctrl Pts',(-17.0784749538847,40.4586732394454,8.76459989653525));
#59902=CARTESIAN_POINT('Ctrl Pts',(-17.0947382606243,40.4563753990957,8.78066950019678));
#59903=CARTESIAN_POINT('Ctrl Pts',(-17.1021945954706,40.455341667552,8.78785890823777));
#59904=CARTESIAN_POINT('Ctrl Pts',(-17.1210118338545,40.452779834005,8.80556341268336));
#59905=CARTESIAN_POINT('Ctrl Pts',(-17.1324785773211,40.4512600069224,8.81596357669802));
#59906=CARTESIAN_POINT('Ctrl Pts',(-17.2058990046647,40.441761216154,8.88014756294862));
#59907=CARTESIAN_POINT('Ctrl Pts',(-17.2727632147549,40.4341229455702,8.9280414485952));
#59908=CARTESIAN_POINT('Ctrl Pts',(-17.385585506634,40.4219097727431,8.99334462576646));
#59909=CARTESIAN_POINT('Ctrl Pts',(-17.4287201947854,40.4173803092128,9.0151295684408));
#59910=CARTESIAN_POINT('Ctrl Pts',(-17.5050174941755,40.409463131924,9.04835140369458));
#59911=CARTESIAN_POINT('Ctrl Pts',(-17.5376055627803,40.4061099569932,9.06096897044695));
#59912=CARTESIAN_POINT('Ctrl Pts',(-17.589335121813,40.4007954550415,9.07858171576351));
#59913=CARTESIAN_POINT('Ctrl Pts',(-17.6081452829912,40.3988647531316,9.08450103913765));
#59914=CARTESIAN_POINT('Ctrl Pts',(-17.6445649901821,40.3951241364239,9.09503652920914));
#59915=CARTESIAN_POINT('Ctrl Pts',(-17.6621510767718,40.3933168252073,9.09971668189172));
#59916=CARTESIAN_POINT('Ctrl Pts',(-17.7046263449102,40.3889447820579,9.11004861315677));
#59917=CARTESIAN_POINT('Ctrl Pts',(-17.7295959201395,40.3863689241327,9.11533078685432));
#59918=CARTESIAN_POINT('Ctrl Pts',(-17.8349655810278,40.3754623995383,9.13432433334843));
#59919=CARTESIAN_POINT('Ctrl Pts',(-17.9164158388159,40.3669255575321,9.14102423373969));
#59920=CARTESIAN_POINT('Ctrl Pts',(-18.0439958587764,40.3534744668979,9.13922307157601));
#59921=CARTESIAN_POINT('Ctrl Pts',(-18.0899966570576,40.3486127246355,9.13606629434577));
#59922=CARTESIAN_POINT('Ctrl Pts',(-18.1634527700716,40.3408955258291,9.12699068055585));
#59923=CARTESIAN_POINT('Ctrl Pts',(-18.1910619369153,40.3380060162458,9.12265067427382));
#59924=CARTESIAN_POINT('Ctrl Pts',(-18.2307555026782,40.3338855507928,9.11506110330259));
#59925=CARTESIAN_POINT('Ctrl Pts',(-18.2429682886803,40.3326224834983,9.11253901264723));
#59926=CARTESIAN_POINT('Ctrl Pts',(-18.2652712994163,40.3303267108203,9.10758956195903));
#59927=CARTESIAN_POINT('Ctrl Pts',(-18.2753714130709,40.3292914290233,9.10521795010416));
#59928=CARTESIAN_POINT('Ctrl Pts',(-18.3005659040645,40.3267180974789,9.09897528751248));
#59929=CARTESIAN_POINT('Ctrl Pts',(-18.3156202671508,40.3251884905972,9.0949497440672));
#59930=CARTESIAN_POINT('Ctrl Pts',(-18.4085159051642,40.3157763919866,9.06826798957341));
#59931=CARTESIAN_POINT('Ctrl Pts',(-18.4841271356515,40.3082250949298,9.03847458477402));
#59932=CARTESIAN_POINT('Ctrl Pts',(-18.599797485842,40.2960638521589,8.9795601897357));
#59933=CARTESIAN_POINT('Ctrl Pts',(-18.6418915187764,40.2914958553629,8.95497546777293));
#59934=CARTESIAN_POINT('Ctrl Pts',(-18.7117228903261,40.2835224210026,8.90861194925388));
#59935=CARTESIAN_POINT('Ctrl Pts',(-18.7401570325403,40.2801522842537,8.8879852474216));
#59936=CARTESIAN_POINT('Ctrl Pts',(-18.7821738962323,40.2749433911493,8.85476272556558));
#59937=CARTESIAN_POINT('Ctrl Pts',(-18.7963979653531,40.2731373371248,8.84300300568812));
#59938=CARTESIAN_POINT('Ctrl Pts',(-18.8103597856021,40.2713186493562,8.83093840929314));
#59939=CARTESIAN_POINT('Origin',(-17.98,42.93984859951,7.87));
#59940=CARTESIAN_POINT('',(-18.8112652832218,39.306728237878,8.83197225855912));
#59941=CARTESIAN_POINT('',(-18.8103598916419,39.4763547317748,8.83093831766272));
#59942=CARTESIAN_POINT('',(-18.810359785549,42.93984859951,8.83093840933902));
#59943=CARTESIAN_POINT('',(-19.2490488064308,39.9921506520735,7.86895363828034));
#59944=CARTESIAN_POINT('Ctrl Pts',(-19.2490122151085,39.9921506232699,7.86895337816756));
#59945=CARTESIAN_POINT('Ctrl Pts',(-19.2500434345316,39.9788491414599,7.73500034620256));
#59946=CARTESIAN_POINT('Ctrl Pts',(-19.1688377106395,39.9235352754098,7.17917982593972));
#59947=CARTESIAN_POINT('Ctrl Pts',(-18.3618920861238,39.8262090251199,6.41823176153347));
#59948=CARTESIAN_POINT('Ctrl Pts',(-16.967275569684,39.7001718723999,6.76191054540271));
#59949=CARTESIAN_POINT('Ctrl Pts',(-16.4998154505205,39.5741347196799,8.12005338135742));
#59950=CARTESIAN_POINT('Ctrl Pts',(-17.3874749649531,39.4480975669599,9.24927045136922));
#59951=CARTESIAN_POINT('Ctrl Pts',(-18.398879038736,39.3589620730259,9.1548465851481));
#59952=CARTESIAN_POINT('Ctrl Pts',(-18.7727866904524,39.311838963332,8.8657852835991));
#59953=CARTESIAN_POINT('Ctrl Pts',(-18.8112652832218,39.306728237878,8.83197225855911));
#59954=CARTESIAN_POINT('Ctrl Pts',(-18.810359785549,40.1006362902583,8.83093840933902));
#59955=CARTESIAN_POINT('Ctrl Pts',(-18.847959120699,40.0956894947554,8.79844831885196));
#59956=CARTESIAN_POINT('Ctrl Pts',(-18.8835950569689,40.0907426992525,8.76379461517207));
#59957=CARTESIAN_POINT('Ctrl Pts',(-18.9170253535683,40.0857959037497,8.72725345538537));
#59958=CARTESIAN_POINT('Ctrl Pts',(-18.9339486021519,40.0832917126864,8.70875541039301));
#59959=CARTESIAN_POINT('Ctrl Pts',(-18.9503072702293,40.0807875216231,8.68977420582005));
#59960=CARTESIAN_POINT('Ctrl Pts',(-18.9660740975914,40.0782833305598,8.67034859533788));
#59961=CARTESIAN_POINT('Ctrl Pts',(-18.9971163167093,40.0733530014636,8.63210285044349));
#59962=CARTESIAN_POINT('Ctrl Pts',(-19.0260027419378,40.0684226723673,8.59195889304783));
#59963=CARTESIAN_POINT('Ctrl Pts',(-19.0524931374539,40.063492343271,8.55019002500348));
#59964=CARTESIAN_POINT('Ctrl Pts',(-19.0789414125603,40.0585698535248,8.50848757053285));
#59965=CARTESIAN_POINT('Ctrl Pts',(-19.1030009068902,40.0536473637785,8.46516578154316));
#59966=CARTESIAN_POINT('Ctrl Pts',(-19.1244721268655,40.0487248740322,8.42053024515274));
#59967=CARTESIAN_POINT('Ctrl Pts',(-19.1459198459749,40.0438077720921,8.3759435636367));
#59968=CARTESIAN_POINT('Ctrl Pts',(-19.1647846613904,40.0388906701519,8.33004647638606));
#59969=CARTESIAN_POINT('Ctrl Pts',(-19.1809122084234,40.0339735682118,8.28317050676398));
#59970=CARTESIAN_POINT('Ctrl Pts',(-19.1970288332318,40.0290597963312,8.23632628343698));
#59971=CARTESIAN_POINT('Ctrl Pts',(-19.2104116848931,40.0241460244506,8.18850501252312));
#59972=CARTESIAN_POINT('Ctrl Pts',(-19.2209549331405,40.01923225257,8.14005713083393));
#59973=CARTESIAN_POINT('Ctrl Pts',(-19.2315006822663,40.0143173151335,8.091597757216));
#59974=CARTESIAN_POINT('Ctrl Pts',(-19.2392053521092,40.009402377697,8.04251201270796));
#59975=CARTESIAN_POINT('Ctrl Pts',(-19.2440138612301,40.0044874402604,7.99316232629432));
#59976=CARTESIAN_POINT('Ctrl Pts',(-19.2480368327339,40.0003754270036,7.95187460546928));
#59977=CARTESIAN_POINT('Ctrl Pts',(-19.2500334984016,39.9962634137468,7.91040250412155));
#59978=CARTESIAN_POINT('Ctrl Pts',(-19.2499995744981,39.99215140049,7.86896039690264));
#59979=CARTESIAN_POINT('Ctrl Pts',(-18.8103597856021,40.2713186493562,8.83093840929314));
#59980=CARTESIAN_POINT('Ctrl Pts',(-18.8113353487289,40.2711915710316,8.83009541209269));
#59981=CARTESIAN_POINT('Ctrl Pts',(-18.8123096314845,40.2710644312613,8.82925092636535));
#59982=CARTESIAN_POINT('Ctrl Pts',(-18.8270029153982,40.2691435575313,8.81647588987751));
#59983=CARTESIAN_POINT('Ctrl Pts',(-18.8404645086,40.2673380063092,8.80425440351711));
#59984=CARTESIAN_POINT('Ctrl Pts',(-18.8721112373488,40.2629773532221,8.77425878974085));
#59985=CARTESIAN_POINT('Ctrl Pts',(-18.8900330129945,40.2604112711266,8.75622011676833));
#59986=CARTESIAN_POINT('Ctrl Pts',(-18.9512887341706,40.2512791113806,8.69074664278821));
#59987=CARTESIAN_POINT('Ctrl Pts',(-18.9915466578312,40.2445956812025,8.64058242508443));
#59988=CARTESIAN_POINT('Ctrl Pts',(-19.0674435395144,40.2304722228324,8.52975837315787));
#59989=CARTESIAN_POINT('Ctrl Pts',(-19.1021991430942,40.2230412192,8.46873574689834));
#59990=CARTESIAN_POINT('Ctrl Pts',(-19.1416774742103,40.2133112943378,8.38377170479687));
#59991=CARTESIAN_POINT('Ctrl Pts',(-19.1510164752077,40.2108821353506,8.36211438849281));
#59992=CARTESIAN_POINT('Ctrl Pts',(-19.1641058645599,40.2072853700062,8.32927317505436));
#59993=CARTESIAN_POINT('Ctrl Pts',(-19.1683119399862,40.2060954771038,8.31827817315408));
#59994=CARTESIAN_POINT('Ctrl Pts',(-19.1759741115113,40.2038629018916,8.29738254012028));
#59995=CARTESIAN_POINT('Ctrl Pts',(-19.1794612974114,40.2028187556447,8.28749553797094));
#59996=CARTESIAN_POINT('Ctrl Pts',(-19.1882986429718,40.2000936577208,8.26141435404993));
#59997=CARTESIAN_POINT('Ctrl Pts',(-19.1934459110803,40.1984238713517,8.24515321351769));
#59998=CARTESIAN_POINT('Ctrl Pts',(-19.216160788911,40.1906177315345,8.16802568509439));
#59999=CARTESIAN_POINT('Ctrl Pts',(-19.2294885616162,40.1846679792351,8.10599530685499));
#60000=CARTESIAN_POINT('Ctrl Pts',(-19.2459963888156,40.1733244437961,7.98609559644813));
#60001=CARTESIAN_POINT('Ctrl Pts',(-19.2499612607445,40.1679420593289,7.92850519690748));
#60002=CARTESIAN_POINT('Ctrl Pts',(-19.2500255463564,40.1588006770076,7.83212210856226));
#60003=CARTESIAN_POINT('Ctrl Pts',(-19.2482801773884,40.155094883314,7.79342073388342));
#60004=CARTESIAN_POINT('Ctrl Pts',(-19.2429290652543,40.1493639202297,7.7346390450327));
#60005=CARTESIAN_POINT('Ctrl Pts',(-19.2406032799203,40.1473784948397,7.71446329122071));
#60006=CARTESIAN_POINT('Ctrl Pts',(-19.2353027391457,40.1436021061938,7.67650644555688));
#60007=CARTESIAN_POINT('Ctrl Pts',(-19.2324310942089,40.1418148587708,7.65871585119259));
#60008=CARTESIAN_POINT('Ctrl Pts',(-19.2248327890104,40.1376064267281,7.61726869868185));
#60009=CARTESIAN_POINT('Ctrl Pts',(-19.219808844847,40.1351763608475,7.59367481668449));
#60010=CARTESIAN_POINT('Ctrl Pts',(-19.1961481691293,40.1249880999119,7.49626335113258));
#60011=CARTESIAN_POINT('Ctrl Pts',(-19.1715684217584,40.1170489948712,7.42406796970317));
#60012=CARTESIAN_POINT('Ctrl Pts',(-19.1106970351154,40.1012526137591,7.28700633499525));
#60013=CARTESIAN_POINT('Ctrl Pts',(-19.0748758555869,40.093430456798,7.22222963867681));
#60014=CARTESIAN_POINT('Ctrl Pts',(-19.0245037562927,40.0841515313849,7.14738072513215));
#60015=CARTESIAN_POINT('Ctrl Pts',(-19.0151242798023,40.082484018365,7.13400779143111));
#60016=CARTESIAN_POINT('Ctrl Pts',(-18.9993705176888,40.0797833684871,7.11244385553752));
#60017=CARTESIAN_POINT('Ctrl Pts',(-18.9931495827782,40.0787410190934,7.104143924455));
#60018=CARTESIAN_POINT('Ctrl Pts',(-18.9794826818378,40.076503372708,7.08636771589139));
#60019=CARTESIAN_POINT('Ctrl Pts',(-18.9720023261264,40.0753104388076,7.07691954059687));
#60020=CARTESIAN_POINT('Ctrl Pts',(-18.9484368262584,40.0716436021589,7.04801004635702));
#60021=CARTESIAN_POINT('Ctrl Pts',(-18.9319037472022,40.0691981711877,7.02891919351889));
#60022=CARTESIAN_POINT('Ctrl Pts',(-18.8884721280407,40.0630454553267,6.98169127715097));
#60023=CARTESIAN_POINT('Ctrl Pts',(-18.8608288661704,40.059374288492,6.95427347200496));
#60024=CARTESIAN_POINT('Ctrl Pts',(-18.7603437351167,40.0466484657817,6.86337625602024));
#60025=CARTESIAN_POINT('Ctrl Pts',(-18.681572567109,40.0376956862913,6.80697566212655));
#60026=CARTESIAN_POINT('Ctrl Pts',(-18.5765124034718,40.0261081354837,6.74855807180531));
#60027=CARTESIAN_POINT('Ctrl Pts',(-18.5555327850923,40.0238117659273,6.7376480729766));
#60028=CARTESIAN_POINT('Ctrl Pts',(-18.5180520475528,40.0197291773038,6.71946768852931));
#60029=CARTESIAN_POINT('Ctrl Pts',(-18.5016772113961,40.0179520638477,6.71195103346215));
#60030=CARTESIAN_POINT('Ctrl Pts',(-18.4664887054554,40.0141425658507,6.69669595059737));
#60031=CARTESIAN_POINT('Ctrl Pts',(-18.4476381662762,40.0121073750776,6.68905627792513));
#60032=CARTESIAN_POINT('Ctrl Pts',(-18.3922052104593,40.0061325635714,6.66812586881319));
#60033=CARTESIAN_POINT('Ctrl Pts',(-18.3551892933437,40.0021545126848,6.65606147057318));
#60034=CARTESIAN_POINT('Ctrl Pts',(-18.2615925230894,39.9921112811397,6.63024554235934));
#60035=CARTESIAN_POINT('Ctrl Pts',(-18.2045118173154,39.9859973451132,6.61864937705951));
#60036=CARTESIAN_POINT('Ctrl Pts',(-18.08478444842,39.9732638633122,6.60278285492688));
#60037=CARTESIAN_POINT('Ctrl Pts',(-18.0221945479173,39.9666573375357,6.59915759520186));
#60038=CARTESIAN_POINT('Ctrl Pts',(-17.9425738396787,39.9584579560645,6.60043756226792));
#60039=CARTESIAN_POINT('Ctrl Pts',(-17.9255669914728,39.9567188288707,6.60105293603353));
#60040=CARTESIAN_POINT('Ctrl Pts',(-17.8981150054009,39.9539361421134,6.60259926183075));
#60041=CARTESIAN_POINT('Ctrl Pts',(-17.8876606452886,39.9528822443823,6.60331800807715));
#60042=CARTESIAN_POINT('Ctrl Pts',(-17.8654678125533,39.9506586344449,6.60512004883764));
#60043=CARTESIAN_POINT('Ctrl Pts',(-17.8537333560946,39.9494907598806,6.60623748780333));
#60044=CARTESIAN_POINT('Ctrl Pts',(-17.8184884581944,39.9460017648623,6.61008962726633));
#60045=CARTESIAN_POINT('Ctrl Pts',(-17.795035416464,39.9437052458999,6.61331846560482));
#60046=CARTESIAN_POINT('Ctrl Pts',(-17.7024090264132,39.9346832097889,6.62872044589387));
#60047=CARTESIAN_POINT('Ctrl Pts',(-17.6342004609265,39.9281416450755,6.64596700181565));
#60048=CARTESIAN_POINT('Ctrl Pts',(-17.5072479134832,39.9155638767811,6.68953460985917));
#60049=CARTESIAN_POINT('Ctrl Pts',(-17.4483984713352,39.9095528034171,6.71484149247598));
#60050=CARTESIAN_POINT('Ctrl Pts',(-17.3691894741759,39.900957648147,6.75624226643411));
#60051=CARTESIAN_POINT('Ctrl Pts',(-17.3470282816727,39.8984945196304,6.76868606601498));
#60052=CARTESIAN_POINT('Ctrl Pts',(-17.3096802008461,39.8942286220278,6.79115717710812));
#60053=CARTESIAN_POINT('Ctrl Pts',(-17.2943075317554,39.8924379255155,6.80086192520758));
#60054=CARTESIAN_POINT('Ctrl Pts',(-17.2626806614534,39.8886757765791,6.82179059744195));
#60055=CARTESIAN_POINT('Ctrl Pts',(-17.2464696052222,39.8867025996206,6.83307038240985));
#60056=CARTESIAN_POINT('Ctrl Pts',(-17.202159545702,39.8811772887929,6.86546073591962));
#60057=CARTESIAN_POINT('Ctrl Pts',(-17.1746665462111,39.87759559835,6.88736459951935));
#60058=CARTESIAN_POINT('Ctrl Pts',(-17.1112712459221,39.8689473234779,6.94232086586985));
#60059=CARTESIAN_POINT('Ctrl Pts',(-17.076297438735,39.8638497311538,6.97635644323875));
#60060=CARTESIAN_POINT('Ctrl Pts',(-16.9886890915822,39.8501998686765,7.07202846990108));
#60061=CARTESIAN_POINT('Ctrl Pts',(-16.9398389321582,39.8416100730414,7.13684021724949));
#60062=CARTESIAN_POINT('Ctrl Pts',(-16.889335823128,39.8316910108919,7.21915841412927));
#60063=CARTESIAN_POINT('Ctrl Pts',(-16.8814268110546,39.8301009339494,7.23259891196903));
#60064=CARTESIAN_POINT('Ctrl Pts',(-16.8686713706722,39.8274772654278,7.25521850665502));
#60065=CARTESIAN_POINT('Ctrl Pts',(-16.8636866044053,39.8264358104254,7.26431687336797));
#60066=CARTESIAN_POINT('Ctrl Pts',(-16.8529636307684,39.8241599085938,7.28447107443897));
#60067=CARTESIAN_POINT('Ctrl Pts',(-16.8472755852718,39.8229284351527,7.29555196365927));
#60068=CARTESIAN_POINT('Ctrl Pts',(-16.8293962487398,39.81897066317,7.33168137585604));
#60069=CARTESIAN_POINT('Ctrl Pts',(-16.8178646186946,39.8162797835117,7.3570500298097));
#60070=CARTESIAN_POINT('Ctrl Pts',(-16.7895901132734,39.8092332896906,7.42511182821588));
#60071=CARTESIAN_POINT('Ctrl Pts',(-16.7743077644469,39.804928644466,7.46836809948586));
#60072=CARTESIAN_POINT('Ctrl Pts',(-16.7382994996124,39.7929442245416,7.59106059757405));
#60073=CARTESIAN_POINT('Ctrl Pts',(-16.7228829887931,39.7852993494336,7.67180385370116));
#60074=CARTESIAN_POINT('Ctrl Pts',(-16.7130191891761,39.7749629706454,7.77884460871983));
#60075=CARTESIAN_POINT('Ctrl Pts',(-16.7114451337938,39.7724926784476,7.80428835767221));
#60076=CARTESIAN_POINT('Ctrl Pts',(-16.7100613401128,39.768218615089,7.84794009257589));
#60077=CARTESIAN_POINT('Ctrl Pts',(-16.7098756875831,39.7664270447809,7.8661290034549));
#60078=CARTESIAN_POINT('Ctrl Pts',(-16.7103029376445,39.7626669647809,7.90403279587781));
#60079=CARTESIAN_POINT('Ctrl Pts',(-16.7109844084988,39.7606967853505,7.92374176402436));
#60080=CARTESIAN_POINT('Ctrl Pts',(-16.7141459314526,39.7551924137859,7.97833340212956));
#60081=CARTESIAN_POINT('Ctrl Pts',(-16.7176080388215,39.7516290519761,8.01313836073583));
#60082=CARTESIAN_POINT('Ctrl Pts',(-16.7292705430451,39.7430414086906,8.09564419373493));
#60083=CARTESIAN_POINT('Ctrl Pts',(-16.7387698433991,39.7379867845643,8.14310454984465));
#60084=CARTESIAN_POINT('Ctrl Pts',(-16.7715699063949,39.724287317659,8.26912084416163));
#60085=CARTESIAN_POINT('Ctrl Pts',(-16.7998015355897,39.7156010564592,8.34616676039986));
#60086=CARTESIAN_POINT('Ctrl Pts',(-16.8419669818062,39.7056022260889,8.43393351215351));
#60087=CARTESIAN_POINT('Ctrl Pts',(-16.8489335326136,39.7040221209275,8.44777926889655));
#60088=CARTESIAN_POINT('Ctrl Pts',(-16.8609783268866,39.7014095719741,8.47066451711307));
#60089=CARTESIAN_POINT('Ctrl Pts',(-16.8659165936715,39.7003694209181,8.47977501629416));
#60090=CARTESIAN_POINT('Ctrl Pts',(-16.8770598819799,39.6980898219277,8.4997455681153));
#60091=CARTESIAN_POINT('Ctrl Pts',(-16.8833147170632,39.6968534438551,8.51057616340708));
#60092=CARTESIAN_POINT('Ctrl Pts',(-16.9041937609624,39.6928569785644,8.54552679796158));
#60093=CARTESIAN_POINT('Ctrl Pts',(-16.9194629556755,39.6901332917146,8.5692546687293));
#60094=CARTESIAN_POINT('Ctrl Pts',(-16.9621572175028,39.6829603224973,8.63097965992323));
#60095=CARTESIAN_POINT('Ctrl Pts',(-16.9909159684543,39.6785643222908,8.66800222151471));
#60096=CARTESIAN_POINT('Ctrl Pts',(-17.0743240718698,39.6666528054053,8.76392011661483));
#60097=CARTESIAN_POINT('Ctrl Pts',(-17.1326070034488,39.6591665509276,8.8193496747899));
#60098=CARTESIAN_POINT('Ctrl Pts',(-17.2158627338382,39.6489899015847,8.8847165841836));
#60099=CARTESIAN_POINT('Ctrl Pts',(-17.2364721786914,39.6465089196388,8.89991342952036));
#60100=CARTESIAN_POINT('Ctrl Pts',(-17.2724971538794,39.6422226017263,8.92483227959429));
#60101=CARTESIAN_POINT('Ctrl Pts',(-17.2876891291906,39.6404296574473,8.93486477429318));
#60102=CARTESIAN_POINT('Ctrl Pts',(-17.3197412875435,39.6366723881534,8.95505562024733));
#60103=CARTESIAN_POINT('Ctrl Pts',(-17.3366323507818,39.6347064731809,8.96515534165965));
#60104=CARTESIAN_POINT('Ctrl Pts',(-17.3839517596869,39.6292320654451,8.99197669001587));
#60105=CARTESIAN_POINT('Ctrl Pts',(-17.41483877871,39.6256949550742,9.00784770893681));
#60106=CARTESIAN_POINT('Ctrl Pts',(-17.4897091674399,39.6171937158938,9.04251858178448));
#60107=CARTESIAN_POINT('Ctrl Pts',(-17.5341791180803,39.6122001798439,9.06013764441958));
#60108=CARTESIAN_POINT('Ctrl Pts',(-17.6584274885196,39.5984287485641,9.10142319171068));
#60109=CARTESIAN_POINT('Ctrl Pts',(-17.7397138757666,39.5896036044402,9.1198308004542));
#60110=CARTESIAN_POINT('Ctrl Pts',(-17.8374630292318,39.5794901834321,9.13206937826961));
#60111=CARTESIAN_POINT('Ctrl Pts',(-17.8527378479838,39.5779245133499,9.13370104336077));
#60112=CARTESIAN_POINT('Ctrl Pts',(-17.8783452606535,39.5753279909192,9.13596735711944));
#60113=CARTESIAN_POINT('Ctrl Pts',(-17.888662094416,39.5742896574515,9.13675351249818));
#60114=CARTESIAN_POINT('Ctrl Pts',(-17.9115455582949,39.5720043823179,9.13821619148546));
#60115=CARTESIAN_POINT('Ctrl Pts',(-17.9241145881642,39.5707606541838,9.13883221383704));
#60116=CARTESIAN_POINT('Ctrl Pts',(-17.9654131052831,39.5667052660875,9.14024135741522));
#60117=CARTESIAN_POINT('Ctrl Pts',(-17.9941632243274,39.5639315296725,9.14024631534447));
#60118=CARTESIAN_POINT('Ctrl Pts',(-18.0712707888497,39.5565619798298,9.13764064319379));
#60119=CARTESIAN_POINT('Ctrl Pts',(-18.1195207317315,39.5520231504256,9.13324105365444));
#60120=CARTESIAN_POINT('Ctrl Pts',(-18.2442319599846,39.5402095655214,9.11463454675975));
#60121=CARTESIAN_POINT('Ctrl Pts',(-18.3198350534797,39.5329568290069,9.09614988885193));
#60122=CARTESIAN_POINT('Ctrl Pts',(-18.4175908919481,39.5230191414013,9.0625081774107));
#60123=CARTESIAN_POINT('Ctrl Pts',(-18.4416494713176,39.5205271433573,9.05340233669953));
#60124=CARTESIAN_POINT('Ctrl Pts',(-18.4822507024794,39.5162282075644,9.03660886190208));
#60125=CARTESIAN_POINT('Ctrl Pts',(-18.4989352741138,39.5144338594558,9.0292834424446));
#60126=CARTESIAN_POINT('Ctrl Pts',(-18.5332624258663,39.5106794599438,9.01332249562221));
#60127=CARTESIAN_POINT('Ctrl Pts',(-18.5508736271378,39.5087178999333,9.0046315840121));
#60128=CARTESIAN_POINT('Ctrl Pts',(-18.5988177209228,39.5032738196776,8.9795730332508));
#60129=CARTESIAN_POINT('Ctrl Pts',(-18.6286940166845,39.4997632343544,8.96237502239997));
#60130=CARTESIAN_POINT('Ctrl Pts',(-18.6977740857092,39.4913486937,8.91877612204459));
#60131=CARTESIAN_POINT('Ctrl Pts',(-18.7362750311286,39.486416251705,8.89136087741531));
#60132=CARTESIAN_POINT('Ctrl Pts',(-18.7857570470864,39.4797536655886,8.85179219470766));
#60133=CARTESIAN_POINT('Ctrl Pts',(-18.7981605331482,39.4780544335529,8.84147994953515));
#60134=CARTESIAN_POINT('Ctrl Pts',(-18.8103598916419,39.4763547317748,8.83093831766273));
#60135=CARTESIAN_POINT('Origin',(-17.98,42.93984859951,7.87));
#60136=CARTESIAN_POINT('',(-18.810359785549,38.5130319987649,8.83093840933902));
#60137=CARTESIAN_POINT('',(-18.8114966369182,38.6825722678645,8.83223897649705));
#60138=CARTESIAN_POINT('',(-18.810359785549,42.93984859951,8.83093840933902));
#60139=CARTESIAN_POINT('',(-19.2502055238694,39.1984014318383,7.8698527011545));
#60140=CARTESIAN_POINT('Ctrl Pts',(-19.2499999914242,39.19840140049,7.86985241131098));
#60141=CARTESIAN_POINT('Ctrl Pts',(-19.2499990709881,39.1976086874999,7.86193206242186));
#60142=CARTESIAN_POINT('Ctrl Pts',(-19.2499240586173,39.1968159745099,7.85401220706734));
#60143=CARTESIAN_POINT('Ctrl Pts',(-19.2497749766161,39.1960232615198,7.84609375061715));
#60144=CARTESIAN_POINT('Ctrl Pts',(-19.2488444410097,39.1910753291281,7.79666856438271));
#60145=CARTESIAN_POINT('Ctrl Pts',(-19.2450217674801,39.1861273967363,7.74718848012828));
#60146=CARTESIAN_POINT('Ctrl Pts',(-19.238301528929,39.1811794643445,7.69801958746717));
#60147=CARTESIAN_POINT('Ctrl Pts',(-19.2315936606194,39.1762406398317,7.64894120217045));
#60148=CARTESIAN_POINT('Ctrl Pts',(-19.2219988793534,39.1713018153188,7.60017341090091));
#60149=CARTESIAN_POINT('Ctrl Pts',(-19.20956370635,39.1663629908059,7.55208005405956));
#60150=CARTESIAN_POINT('Ctrl Pts',(-19.1971411653439,39.1614291832894,7.50403555179797));
#60151=CARTESIAN_POINT('Ctrl Pts',(-19.1818840811064,39.1564953757729,7.45666465568764));
#60152=CARTESIAN_POINT('Ctrl Pts',(-19.163890139538,39.1515615682564,7.41032170216033));
#60153=CARTESIAN_POINT('Ctrl Pts',(-19.1459068187889,39.146630672891,7.36400610229174));
#60154=CARTESIAN_POINT('Ctrl Pts',(-19.1251900388791,39.1416997775257,7.31871775292844));
#60155=CARTESIAN_POINT('Ctrl Pts',(-19.101886720145,39.1367688821604,7.27479399602969));
#60156=CARTESIAN_POINT('Ctrl Pts',(-19.0785872391627,39.131838798849,7.23087747279921));
#60157=CARTESIAN_POINT('Ctrl Pts',(-19.0527023225667,39.1269087155376,7.18832557925812));
#60158=CARTESIAN_POINT('Ctrl Pts',(-19.0244250765477,39.1219786322263,7.14745155215842));
#60159=CARTESIAN_POINT('Ctrl Pts',(-18.9961201969123,39.1170437310472,7.10653758138144));
#60160=CARTESIAN_POINT('Ctrl Pts',(-18.9654186332303,39.1121088298681,7.06730520180628));
#60161=CARTESIAN_POINT('Ctrl Pts',(-18.9325561024963,39.107173928689,7.03003757727084));
#60162=CARTESIAN_POINT('Ctrl Pts',(-18.8996758941321,39.1022363728951,6.99274990548792));
#60163=CARTESIAN_POINT('Ctrl Pts',(-18.8646327902994,39.0972988171013,6.95742948276588));
#60164=CARTESIAN_POINT('Ctrl Pts',(-18.8276995335412,39.0923612613074,6.92432272902744));
#60165=CARTESIAN_POINT('Ctrl Pts',(-18.7906972595141,39.0874144786908,6.89115410861595));
#60166=CARTESIAN_POINT('Ctrl Pts',(-18.7517982119447,39.0824676960742,6.86020775485804));
#60167=CARTESIAN_POINT('Ctrl Pts',(-18.7113070711933,39.0775209134575,6.8316888868828));
#60168=CARTESIAN_POINT('Ctrl Pts',(-18.6907487366439,39.075009311905,6.81720916569135));
#60169=CARTESIAN_POINT('Ctrl Pts',(-18.6697804286997,39.0724977103524,6.80335450224794));
#60170=CARTESIAN_POINT('Ctrl Pts',(-18.6484444243639,39.0699861087999,6.79014720839513));
#60171=CARTESIAN_POINT('Ctrl Pts',(-18.6064118395895,39.0650381764919,6.76412843328754));
#60172=CARTESIAN_POINT('Ctrl Pts',(-18.5627648770544,39.0600902441839,6.74050992054005));
#60173=CARTESIAN_POINT('Ctrl Pts',(-18.5178081895561,39.0551423118759,6.71949474088712));
#60174=CARTESIAN_POINT('Ctrl Pts',(-18.4729342558417,39.050203487448,6.6985182448146));
#60175=CARTESIAN_POINT('Ctrl Pts',(-18.426755871122,39.0452646630201,6.68013580773455));
#60176=CARTESIAN_POINT('Ctrl Pts',(-18.3796039671525,39.0403258385923,6.66450563276471));
#60177=CARTESIAN_POINT('Ctrl Pts',(-18.3324999614159,39.0353920311615,6.64889133536713));
#60178=CARTESIAN_POINT('Ctrl Pts',(-18.2844249118265,39.0304582237306,6.6360239369202));
#60179=CARTESIAN_POINT('Ctrl Pts',(-18.2357295085853,39.0255244162998,6.62601349748531));
#60180=CARTESIAN_POINT('Ctrl Pts',(-18.1870628475282,39.0205935210207,6.61600896665523));
#60181=CARTESIAN_POINT('Ctrl Pts',(-18.1377770939678,39.0156626257416,6.60885816435106));
#60182=CARTESIAN_POINT('Ctrl Pts',(-18.0882353562146,39.0107317304625,6.604620567709));
#60183=CARTESIAN_POINT('Ctrl Pts',(-18.0387017773414,39.0058016472377,6.600383668944));
#60184=CARTESIAN_POINT('Ctrl Pts',(-17.9889128437644,39.0008715640129,6.59905906908673));
#60185=CARTESIAN_POINT('Ctrl Pts',(-17.9392364542431,38.9959414807881,6.60065436805521));
#60186=CARTESIAN_POINT('Ctrl Pts',(-17.8895115190339,38.9910065796955,6.6022512260115));
#60187=CARTESIAN_POINT('Ctrl Pts',(-17.8398998962177,38.9860716786028,6.60677366137129));
#60188=CARTESIAN_POINT('Ctrl Pts',(-17.7907673222606,38.9811367775101,6.61417716469417));
#60189=CARTESIAN_POINT('Ctrl Pts',(-17.7416083185838,38.9761992218028,6.6215846505586));
#60190=CARTESIAN_POINT('Ctrl Pts',(-17.6929294136144,38.9712616660954,6.63187617705311));
#60191=CARTESIAN_POINT('Ctrl Pts',(-17.6450855478346,38.9663241103881,6.6449562008929));
#60192=CARTESIAN_POINT('Ctrl Pts',(-17.597152276093,38.961377327857,6.65806066740873));
#60193=CARTESIAN_POINT('Ctrl Pts',(-17.5500576774657,38.9564305453259,6.67396385609788));
#60194=CARTESIAN_POINT('Ctrl Pts',(-17.5041393928909,38.9514837627948,6.6925210479156));
#60195=CARTESIAN_POINT('Ctrl Pts',(-17.4808255589814,38.9489721605565,6.70194298716862));
#60196=CARTESIAN_POINT('Ctrl Pts',(-17.4578146043481,38.9464605583182,6.71204832976388));
#60197=CARTESIAN_POINT('Ctrl Pts',(-17.4351482004246,38.9439489560799,6.72281365223456));
#60198=CARTESIAN_POINT('Ctrl Pts',(-17.3904946998796,38.9390010237879,6.74402166275233));
#60199=CARTESIAN_POINT('Ctrl Pts',(-17.3469825560467,38.934053091496,6.76788763859601));
#60200=CARTESIAN_POINT('Ctrl Pts',(-17.3049475898042,38.929105159204,6.79426571892089));
#60201=CARTESIAN_POINT('Ctrl Pts',(-17.2629899992104,38.924166334793,6.82059524392954));
#60202=CARTESIAN_POINT('Ctrl Pts',(-17.2225046537098,38.9192275103821,6.84942741328755));
#60203=CARTESIAN_POINT('Ctrl Pts',(-17.1838039252047,38.9142886859711,6.88056995675263));
#60204=CARTESIAN_POINT('Ctrl Pts',(-17.1451425099946,38.9093548785577,6.91168086474088));
#60205=CARTESIAN_POINT('Ctrl Pts',(-17.1082625478236,38.9044210711444,6.94509715880468));
#60206=CARTESIAN_POINT('Ctrl Pts',(-17.0734466738052,38.899487263731,6.98058386187057));
#60207=CARTESIAN_POINT('Ctrl Pts',(-17.0386513496615,38.8945563684698,7.0160496191086));
#60208=CARTESIAN_POINT('Ctrl Pts',(-17.0059180832057,38.8896254732087,7.05358297398715));
#60209=CARTESIAN_POINT('Ctrl Pts',(-16.9754937424663,38.8846945779475,7.09291108708482));
#60210=CARTESIAN_POINT('Ctrl Pts',(-16.9450744122231,38.8797644947411,7.13223272334995));
#60211=CARTESIAN_POINT('Ctrl Pts',(-16.9169635871612,38.8748344115348,7.17334809724056));
#60212=CARTESIAN_POINT('Ctrl Pts',(-16.891367144662,38.8699043283284,7.21595221407101));
#60213=CARTESIAN_POINT('Ctrl Pts',(-16.8657456883327,38.8649694272547,7.25859796528643));
#60214=CARTESIAN_POINT('Ctrl Pts',(-16.8426438024454,38.860034526181,7.30273489305767));
#60215=CARTESIAN_POINT('Ctrl Pts',(-16.822222408586,38.8550996251074,7.34803156338751));
#60216=CARTESIAN_POINT('Ctrl Pts',(-16.8017900295166,38.8501620694193,7.39335259999923));
#60217=CARTESIAN_POINT('Ctrl Pts',(-16.784041209444,38.8452245137313,7.4398341089843));
#60218=CARTESIAN_POINT('Ctrl Pts',(-16.7690881362387,38.8402869580433,7.48712605442254));
#60219=CARTESIAN_POINT('Ctrl Pts',(-16.7541071201858,38.8353401755318,7.53450637444479));
#60220=CARTESIAN_POINT('Ctrl Pts',(-16.7419324125825,38.8303933930204,7.58269962200204));
#60221=CARTESIAN_POINT('Ctrl Pts',(-16.7326255022506,38.8254466105089,7.631343631209));
#60222=CARTESIAN_POINT('Ctrl Pts',(-16.7279001564094,38.8229350081259,7.65604138356838));
#60223=CARTESIAN_POINT('Ctrl Pts',(-16.7239132546785,38.8204234057429,7.68085522387331));
#60224=CARTESIAN_POINT('Ctrl Pts',(-16.7206677123897,38.8179118033599,7.70573743767299));
#60225=CARTESIAN_POINT('Ctrl Pts',(-16.7142738963535,38.812963871038,7.75475614809193));
#60226=CARTESIAN_POINT('Ctrl Pts',(-16.710732251272,38.8080159387161,7.80425714047221));
#60227=CARTESIAN_POINT('Ctrl Pts',(-16.7101023196782,38.8030680063941,7.85387915903438));
#60228=CARTESIAN_POINT('Ctrl Pts',(-16.7094735476278,38.7981291819524,7.90340983612862));
#60229=CARTESIAN_POINT('Ctrl Pts',(-16.7117458658497,38.7931903575107,7.95306055406278));
#60230=CARTESIAN_POINT('Ctrl Pts',(-16.7169271076727,38.788251533069,8.00246459401625));
#60231=CARTESIAN_POINT('Ctrl Pts',(-16.7221030862441,38.7833177256245,8.051818447953));
#60232=CARTESIAN_POINT('Ctrl Pts',(-16.7301820817317,38.7783839181799,8.10092557758484));
#60233=CARTESIAN_POINT('Ctrl Pts',(-16.7411199196841,38.7734501107353,8.14942109189623));
#60234=CARTESIAN_POINT('Ctrl Pts',(-16.7520513016398,38.7685192154425,8.19788798200591));
#60235=CARTESIAN_POINT('Ctrl Pts',(-16.7658380628878,38.7635883201497,8.24574343838036));
#60236=CARTESIAN_POINT('Ctrl Pts',(-16.7823848217199,38.7586574248569,8.2926320914853));
#60237=CARTESIAN_POINT('Ctrl Pts',(-16.7989288555157,38.7537273416186,8.33951302263769));
#60238=CARTESIAN_POINT('Ctrl Pts',(-16.8182318013396,38.7487972583803,8.3854269504489));
#60239=CARTESIAN_POINT('Ctrl Pts',(-16.8401490329719,38.743867175142,8.43003551045009));
#60240=CARTESIAN_POINT('Ctrl Pts',(-16.8620876829688,38.738932274036,8.47468766365754));
#60241=CARTESIAN_POINT('Ctrl Pts',(-16.886645476655,38.7339973729301,8.51803140971679));
#60242=CARTESIAN_POINT('Ctrl Pts',(-16.9136311958668,38.7290624718242,8.55975182027424));
#60243=CARTESIAN_POINT('Ctrl Pts',(-16.9406314314147,38.7241249161037,8.60149467335002));
#60244=CARTESIAN_POINT('Ctrl Pts',(-16.9700618687458,38.7191873603833,8.64161200973613));
#60245=CARTESIAN_POINT('Ctrl Pts',(-17.0016892343157,38.7142498046628,8.67981976127177));
#60246=CARTESIAN_POINT('Ctrl Pts',(-17.0333757020269,38.709303022119,8.71809891173316));
#60247=CARTESIAN_POINT('Ctrl Pts',(-17.0672669180125,38.7043562395752,8.75446095407676));
#60248=CARTESIAN_POINT('Ctrl Pts',(-17.1030919255177,38.6994094570314,8.7886578410419));
#60249=CARTESIAN_POINT('Ctrl Pts',(-17.1212811554622,38.6968978549009,8.80602043448458));
#60250=CARTESIAN_POINT('Ctrl Pts',(-17.1399683433277,38.6943862527704,8.82282552115789));
#60251=CARTESIAN_POINT('Ctrl Pts',(-17.1591149793417,38.6918746506399,8.83904477856231));
#60252=CARTESIAN_POINT('Ctrl Pts',(-17.1968344325165,38.6869267183303,8.87099720716376));
#60253=CARTESIAN_POINT('Ctrl Pts',(-17.2365056878571,38.6819787860206,8.90081470174741));
#60254=CARTESIAN_POINT('Ctrl Pts',(-17.277857497935,38.677030853711,8.92825134386583));
#60255=CARTESIAN_POINT('Ctrl Pts',(-17.3191331898854,38.6720920292818,8.95563748212925));
#60256=CARTESIAN_POINT('Ctrl Pts',(-17.362082848269,38.6671532048526,8.98065115946237));
#60257=CARTESIAN_POINT('Ctrl Pts',(-17.4064025963729,38.6622143804234,9.00308694218593));
#60258=CARTESIAN_POINT('Ctrl Pts',(-17.4506773232259,38.6572805729914,9.02549993400824));
#60259=CARTESIAN_POINT('Ctrl Pts',(-17.4963188979979,38.6523467655594,9.04533996901389));
#60260=CARTESIAN_POINT('Ctrl Pts',(-17.5429967787013,38.6474129581275,9.06244630259586));
#60261=CARTESIAN_POINT('Ctrl Pts',(-17.5896471080499,38.6424820628474,9.0795425392613));
#60262=CARTESIAN_POINT('Ctrl Pts',(-17.6373320180086,38.6375511675673,9.09390808279222));
#60263=CARTESIAN_POINT('Ctrl Pts',(-17.6857011997727,38.6326202722872,9.10543037690709));
#60264=CARTESIAN_POINT('Ctrl Pts',(-17.7340624157598,38.6276901890617,9.11695077344951));
#60265=CARTESIAN_POINT('Ctrl Pts',(-17.7831071468094,38.6227601058361,9.12562872419306));
#60266=CARTESIAN_POINT('Ctrl Pts',(-17.8324726694454,38.6178300226106,9.13140226999139));
#60267=CARTESIAN_POINT('Ctrl Pts',(-17.8818864339751,38.6128951215175,9.13718145792148));
#60268=CARTESIAN_POINT('Ctrl Pts',(-17.9316210705484,38.6079602204243,9.14005051114982));
#60269=CARTESIAN_POINT('Ctrl Pts',(-17.9813082828559,38.6030253193312,9.13999932613997));
#60270=CARTESIAN_POINT('Ctrl Pts',(-18.0310222232361,38.5980877636235,9.13994811359634));
#60271=CARTESIAN_POINT('Ctrl Pts',(-18.0806881409664,38.5931502079159,9.13697356751715));
#60272=CARTESIAN_POINT('Ctrl Pts',(-18.1299408646946,38.5882126522082,9.13111765394615));
#60273=CARTESIAN_POINT('Ctrl Pts',(-18.1792856271185,38.5832658696771,9.1252507974139));
#60274=CARTESIAN_POINT('Ctrl Pts',(-18.2282151147304,38.578319087146,9.11649192337859));
#60275=CARTESIAN_POINT('Ctrl Pts',(-18.2763739880558,38.5733723046148,9.10493419225637));
#60276=CARTESIAN_POINT('Ctrl Pts',(-18.3008254235003,38.5708607023832,9.09906605006564));
#60277=CARTESIAN_POINT('Ctrl Pts',(-18.3250784467569,38.5683491001516,9.09247720781038));
#60278=CARTESIAN_POINT('Ctrl Pts',(-18.3490883789177,38.5658374979199,9.08518466438147));
#60279=CARTESIAN_POINT('Ctrl Pts',(-18.3963731598043,38.5608911881843,9.07082284462152));
#60280=CARTESIAN_POINT('Ctrl Pts',(-18.4429229680734,38.5559448784487,9.0536652596052));
#60281=CARTESIAN_POINT('Ctrl Pts',(-18.4883844413207,38.5509985687131,9.03380636697995));
#60282=CARTESIAN_POINT('Ctrl Pts',(-18.5337803369426,38.5460593939695,9.01397612056713));
#60283=CARTESIAN_POINT('Ctrl Pts',(-18.5780905064593,38.5411202192259,8.99145249459473));
#60284=CARTESIAN_POINT('Ctrl Pts',(-18.6209774872879,38.5361810444823,8.9663794328562));
#60285=CARTESIAN_POINT('Ctrl Pts',(-18.6638174517488,38.5312472844835,8.94133385834727));
#60286=CARTESIAN_POINT('Ctrl Pts',(-18.7052368477543,38.5263135244846,8.9137446606519));
#60287=CARTESIAN_POINT('Ctrl Pts',(-18.7449213816353,38.5213797644858,8.88380238701495));
#60288=CARTESIAN_POINT('Ctrl Pts',(-18.7673030399554,38.5185971759122,8.86691526066286));
#60289=CARTESIAN_POINT('Ctrl Pts',(-18.7891333083039,38.5158145873385,8.84928049341218));
#60290=CARTESIAN_POINT('Ctrl Pts',(-18.810359785549,38.5130319987649,8.83093840933902));
#60291=CARTESIAN_POINT('Ctrl Pts',(-18.8112652832218,39.306728237878,8.83197225855911));
#60292=CARTESIAN_POINT('Ctrl Pts',(-19.0831283208982,39.2706193979584,8.59307288519897));
#60293=CARTESIAN_POINT('Ctrl Pts',(-19.2514866871259,39.2345105580389,8.23122653928661));
#60294=CARTESIAN_POINT('Ctrl Pts',(-19.2520824989184,39.1984017181193,7.86985534807999));
#60295=CARTESIAN_POINT('',(-19.2486386161102,39.3679726942069,7.86909595157452));
#60296=CARTESIAN_POINT('Ctrl Pts',(-18.8103598916419,39.4763547317748,8.83093831766273));
#60297=CARTESIAN_POINT('Ctrl Pts',(-18.8620061132681,39.4691590112148,8.78631011395291));
#60298=CARTESIAN_POINT('Ctrl Pts',(-18.9099933252366,39.4619476178614,8.73757128028793));
#60299=CARTESIAN_POINT('Ctrl Pts',(-18.9636126774288,39.4533741735106,8.67351579312111));
#60300=CARTESIAN_POINT('Ctrl Pts',(-18.9731698682519,39.4518234846111,8.66167241875458));
#60301=CARTESIAN_POINT('Ctrl Pts',(-18.9888542235223,39.4492435241503,8.64150493370748));
#60302=CARTESIAN_POINT('Ctrl Pts',(-18.9950964108587,39.4482070059909,8.63327322898891));
#60303=CARTESIAN_POINT('Ctrl Pts',(-19.0087675185221,39.4459154563924,8.61478037931914));
#60304=CARTESIAN_POINT('Ctrl Pts',(-19.0161445770296,39.4446637927418,8.60448273233148));
#60305=CARTESIAN_POINT('Ctrl Pts',(-19.0400868044573,39.4405436115412,8.56998284764106));
#60306=CARTESIAN_POINT('Ctrl Pts',(-19.0559693654605,39.4377147303983,8.54531502409662));
#60307=CARTESIAN_POINT('Ctrl Pts',(-19.1079695130391,39.4280173732117,8.45805155733503));
#60308=CARTESIAN_POINT('Ctrl Pts',(-19.1395933465726,39.4213072403054,8.39293879686302));
#60309=CARTESIAN_POINT('Ctrl Pts',(-19.1870409289255,39.4088898079164,8.26944492086036));
#60310=CARTESIAN_POINT('Ctrl Pts',(-19.2045684028458,39.4032218674176,8.21195696228121));
#60311=CARTESIAN_POINT('Ctrl Pts',(-19.2230682907053,39.3952176097225,8.13115936753069));
#60312=CARTESIAN_POINT('Ctrl Pts',(-19.2275689638199,39.3929928096936,8.10873523588568));
#60313=CARTESIAN_POINT('Ctrl Pts',(-19.2345113261439,39.388990571676,8.06855040817372));
#60314=CARTESIAN_POINT('Ctrl Pts',(-19.2371870191359,39.3872210676874,8.05083597018949));
#60315=CARTESIAN_POINT('Ctrl Pts',(-19.24165923346,39.3837568503842,8.01629480779699));
#60316=CARTESIAN_POINT('Ctrl Pts',(-19.2434958765408,39.3820638031193,7.99947698992941));
#60317=CARTESIAN_POINT('Ctrl Pts',(-19.246521307358,39.3786278320891,7.96549663107796));
#60318=CARTESIAN_POINT('Ctrl Pts',(-19.2476983593243,39.3768849072122,7.94833661507711));
#60319=CARTESIAN_POINT('Ctrl Pts',(-19.2495244548045,39.3730190528955,7.91046075630686));
#60320=CARTESIAN_POINT('Ctrl Pts',(-19.2500155520902,39.3708920262909,7.88974282348426));
#60321=CARTESIAN_POINT('Ctrl Pts',(-19.2499996247524,39.3687519858842,7.86902371692696));
#60322=CARTESIAN_POINT('Ctrl Pts',(-19.2486386161102,39.3679726942069,7.86909595157452));
#60323=CARTESIAN_POINT('Ctrl Pts',(-19.2496120538636,39.3531045973913,7.71925523329057));
#60324=CARTESIAN_POINT('Ctrl Pts',(-19.1557551286073,39.2962241163357,7.14719552633411));
#60325=CARTESIAN_POINT('Ctrl Pts',(-18.3076284955857,39.19733125104,6.40503162152318));
#60326=CARTESIAN_POINT('Ctrl Pts',(-16.9267603470372,39.0712940983201,6.80034628368819));
#60327=CARTESIAN_POINT('Ctrl Pts',(-16.5101406589765,38.9452569456,8.17493663311751));
#60328=CARTESIAN_POINT('Ctrl Pts',(-17.4391877588077,38.8192197928801,9.27035529110332));
#60329=CARTESIAN_POINT('Ctrl Pts',(-18.4285950040459,38.7316582336349,9.14070744036985));
#60330=CARTESIAN_POINT('Ctrl Pts',(-18.7848458224106,38.6861090586297,8.8555733520524));
#60331=CARTESIAN_POINT('Ctrl Pts',(-18.8114966369182,38.6825722678645,8.83223897649705));
#60332=CARTESIAN_POINT('Origin',(-17.98,42.93984859951,7.87));
#60333=CARTESIAN_POINT('',(-18.8099615219029,37.7194233520466,8.8304622415411));
#60334=CARTESIAN_POINT('',(-18.8103597914526,37.8897334522804,8.83093840423764));
#60335=CARTESIAN_POINT('',(-18.810359785549,42.93984859951,8.83093840933902));
#60336=CARTESIAN_POINT('',(-19.2494450023513,38.40465140049,7.87113066820918));
#60337=CARTESIAN_POINT('Ctrl Pts',(-19.2494450023513,38.40465140049,7.87113066820918));
#60338=CARTESIAN_POINT('Ctrl Pts',(-19.2468218434614,38.3743553311533,7.5662963047995));
#60339=CARTESIAN_POINT('Ctrl Pts',(-18.9838065853326,38.3020468775766,6.83467797247145));
#60340=CARTESIAN_POINT('Ctrl Pts',(-17.7610940240468,38.1877260397599,6.38488952760496));
#60341=CARTESIAN_POINT('Ctrl Pts',(-16.6134802208024,38.0616888870399,7.2486332527821));
#60342=CARTESIAN_POINT('Ctrl Pts',(-16.7169250908296,37.9356517343199,8.68124269815259));
#60343=CARTESIAN_POINT('Ctrl Pts',(-17.857291976994,37.8215632226555,9.30574832435665));
#60344=CARTESIAN_POINT('Ctrl Pts',(-18.5791970423144,37.749487095231,9.02612225094904));
#60345=CARTESIAN_POINT('Ctrl Pts',(-18.8099615219027,37.7194233520466,8.8304622415412));
#60346=CARTESIAN_POINT('Ctrl Pts',(-18.810359785549,38.5130319987649,8.83093840933902));
#60347=CARTESIAN_POINT('Ctrl Pts',(-18.8479687726811,38.5081018195057,8.79843997844458));
#60348=CARTESIAN_POINT('Ctrl Pts',(-18.8836801829122,38.5031716402464,8.76371901167769));
#60349=CARTESIAN_POINT('Ctrl Pts',(-18.9172289811395,38.4982414609872,8.72703082611549));
#60350=CARTESIAN_POINT('Ctrl Pts',(-18.9508060520644,38.4933071269006,8.69031172218875));
#60351=CARTESIAN_POINT('Ctrl Pts',(-18.9822164951175,38.4883727928139,8.6516224889439));
#60352=CARTESIAN_POINT('Ctrl Pts',(-19.0112335911466,38.4834384587273,8.61125385698215));
#60353=CARTESIAN_POINT('Ctrl Pts',(-19.0402614685323,38.4785022912796,8.57087022597931));
#60354=CARTESIAN_POINT('Ctrl Pts',(-19.066893928649,38.4735661238318,8.52880641405647));
#60355=CARTESIAN_POINT('Ctrl Pts',(-19.0909479632238,38.4686299563841,8.48538168888006));
#60356=CARTESIAN_POINT('Ctrl Pts',(-19.1150504368909,38.4636838486716,8.44186951665765));
#60357=CARTESIAN_POINT('Ctrl Pts',(-19.1365638683119,38.4587377409592,8.39699144942104));
#60358=CARTESIAN_POINT('Ctrl Pts',(-19.1553521553955,38.4537916332468,8.3510897118076));
#60359=CARTESIAN_POINT('Ctrl Pts',(-19.1730679265148,38.4491278705645,8.30780824213878));
#60360=CARTESIAN_POINT('Ctrl Pts',(-19.1883611183866,38.4444641078822,8.26361718459007));
#60361=CARTESIAN_POINT('Ctrl Pts',(-19.2011587165291,38.4398003451999,8.21881426152752));
#60362=CARTESIAN_POINT('Ctrl Pts',(-19.2180120774238,38.4336585618171,8.1598125783129));
#60363=CARTESIAN_POINT('Ctrl Pts',(-19.2305987195022,38.4275167784342,8.09954154746724));
#60364=CARTESIAN_POINT('Ctrl Pts',(-19.2387654218309,38.4213749950514,8.03855151379594));
#60365=CARTESIAN_POINT('Ctrl Pts',(-19.2461778518552,38.4158004635309,7.98319448735252));
#60366=CARTESIAN_POINT('Ctrl Pts',(-19.2499495165899,38.4102259320105,7.92724526151886));
#60367=CARTESIAN_POINT('Ctrl Pts',(-19.2499994962489,38.40465140049,7.87113116208534));
#60368=CARTESIAN_POINT('',(-19.2518542553689,38.5741828836634,7.86958341168147));
#60369=CARTESIAN_POINT('Ctrl Pts',(-18.8114966369182,38.6825722678645,8.83223897649705));
#60370=CARTESIAN_POINT('Ctrl Pts',(-19.0836414450039,38.6464563268767,8.59395998673138));
#60371=CARTESIAN_POINT('Ctrl Pts',(-19.2503375314429,38.610340385889,8.23113979624163));
#60372=CARTESIAN_POINT('Ctrl Pts',(-19.251927057606,38.5742244449012,7.86957941617817));
#60373=CARTESIAN_POINT('Ctrl Pts',(-19.2499999609793,38.5731243067121,7.86968517832548));
#60374=CARTESIAN_POINT('Ctrl Pts',(-19.2499976467982,38.5721649088099,7.86034970331008));
#60375=CARTESIAN_POINT('Ctrl Pts',(-19.2498923981337,38.5712095171252,7.85101405572014));
#60376=CARTESIAN_POINT('Ctrl Pts',(-19.2494850282136,38.5693492592664,7.83275027757938));
#60377=CARTESIAN_POINT('Ctrl Pts',(-19.249191645318,38.5684440456419,7.82382248568587));
#60378=CARTESIAN_POINT('Ctrl Pts',(-19.248400106877,38.5666053569461,7.80559613257907));
#60379=CARTESIAN_POINT('Ctrl Pts',(-19.2478938593267,38.5656725322555,7.79629874300408));
#60380=CARTESIAN_POINT('Ctrl Pts',(-19.2464351530712,38.5634499807966,7.77402471215421));
#60381=CARTESIAN_POINT('Ctrl Pts',(-19.2453854873138,38.5621655154125,7.76105564341872));
#60382=CARTESIAN_POINT('Ctrl Pts',(-19.2412723286484,38.5579653159507,7.71839964852164));
#60383=CARTESIAN_POINT('Ctrl Pts',(-19.2373615874497,38.555089990553,7.6888016453913));
#60384=CARTESIAN_POINT('Ctrl Pts',(-19.2262667308048,38.5487105183809,7.62283282772677));
#60385=CARTESIAN_POINT('Ctrl Pts',(-19.2185265717978,38.5452249650623,7.58658384614804));
#60386=CARTESIAN_POINT('Ctrl Pts',(-19.1916012843344,38.5351784646923,7.48292197233717));
#60387=CARTESIAN_POINT('Ctrl Pts',(-19.1684126116585,38.5286556766224,7.41669925232812));
#60388=CARTESIAN_POINT('Ctrl Pts',(-19.1258751099155,38.5187147638503,7.32131685817229));
#60389=CARTESIAN_POINT('Ctrl Pts',(-19.1105976205512,38.5154119558307,7.2904902828806));
#60390=CARTESIAN_POINT('Ctrl Pts',(-19.0846677173216,38.5101575485012,7.24310731694291));
#60391=CARTESIAN_POINT('Ctrl Pts',(-19.074848631642,38.5082353703526,7.22611214426612));
#60392=CARTESIAN_POINT('Ctrl Pts',(-19.0551595489161,38.5045002516073,7.19378693092562));
#60393=CARTESIAN_POINT('Ctrl Pts',(-19.0453454060493,38.5026897429341,7.17842842180635));
#60394=CARTESIAN_POINT('Ctrl Pts',(-19.0208741330301,38.498290447733,7.14188994021249));
#60395=CARTESIAN_POINT('Ctrl Pts',(-19.0058973076877,38.4956901403741,7.12093545907858));
#60396=CARTESIAN_POINT('Ctrl Pts',(-18.9440180261012,38.4852836404473,7.03969765236556));
#60397=CARTESIAN_POINT('Ctrl Pts',(-18.8923643010938,38.477301370748,6.98325339636389));
#60398=CARTESIAN_POINT('Ctrl Pts',(-18.799581647996,38.4640653519918,6.89860316337923));
#60399=CARTESIAN_POINT('Ctrl Pts',(-18.7612943287668,38.4588627231777,6.86755025023491));
#60400=CARTESIAN_POINT('Ctrl Pts',(-18.6977355144261,38.4506939261036,6.8218598064911));
#60401=CARTESIAN_POINT('Ctrl Pts',(-18.6735959915075,38.4476897889213,6.80573164408738));
#60402=CARTESIAN_POINT('Ctrl Pts',(-18.6381925271546,38.4434412698912,6.78379471308814));
#60403=CARTESIAN_POINT('Ctrl Pts',(-18.627363489712,38.4421620802644,6.77730613275331));
#60404=CARTESIAN_POINT('Ctrl Pts',(-18.6074920237669,38.4398536564728,6.76579863880266));
#60405=CARTESIAN_POINT('Ctrl Pts',(-18.5984827821527,38.4388215622287,6.76072728656436));
#60406=CARTESIAN_POINT('Ctrl Pts',(-18.5759972610137,38.4362796645418,6.74842921218987));
#60407=CARTESIAN_POINT('Ctrl Pts',(-18.5624505393226,38.4347778069882,6.74133476378052));
#60408=CARTESIAN_POINT('Ctrl Pts',(-18.4738786457491,38.4251247828164,6.69696918396517));
#60409=CARTESIAN_POINT('Ctrl Pts',(-18.395436327126,38.4173316741842,6.66694742866786));
#60410=CARTESIAN_POINT('Ctrl Pts',(-18.2687553604257,38.4050271455999,6.63234967898701));
#60411=CARTESIAN_POINT('Ctrl Pts',(-18.2222529478992,38.4005678844358,6.62241396824339));
#60412=CARTESIAN_POINT('Ctrl Pts',(-18.1411270533502,38.3927543340857,6.60978788549234));
#60413=CARTESIAN_POINT('Ctrl Pts',(-18.1067486828358,38.3894332290498,6.60586757038739));
#60414=CARTESIAN_POINT('Ctrl Pts',(-18.0526497345825,38.3841571185286,6.6019272587129));
#60415=CARTESIAN_POINT('Ctrl Pts',(-18.0330139422562,38.3822319727734,6.60095473768511));
#60416=CARTESIAN_POINT('Ctrl Pts',(-17.9951584018545,38.3784952508256,6.59995987294544));
#60417=CARTESIAN_POINT('Ctrl Pts',(-17.9769450927404,38.3766861705908,6.59987312414843));
#60418=CARTESIAN_POINT('Ctrl Pts',(-17.9330804791314,38.3722978015241,6.60060761761898));
#60419=CARTESIAN_POINT('Ctrl Pts',(-17.9074450061548,38.3697071444885,6.60181468635598));
#60420=CARTESIAN_POINT('Ctrl Pts',(-17.8029447999354,38.3590277439848,6.60991372483158));
#60421=CARTESIAN_POINT('Ctrl Pts',(-17.7247847130406,38.3507471318824,6.62339417503107));
#60422=CARTESIAN_POINT('Ctrl Pts',(-17.6025485286636,38.3373989980658,6.65645688488191));
#60423=CARTESIAN_POINT('Ctrl Pts',(-17.5574233956132,38.3323838659728,6.67142335791343));
#60424=CARTESIAN_POINT('Ctrl Pts',(-17.4867987210199,38.324462625584,6.69933314732718));
#60425=CARTESIAN_POINT('Ctrl Pts',(-17.4607117141526,38.3215206842797,6.71066897000109));
#60426=CARTESIAN_POINT('Ctrl Pts',(-17.4236991583217,38.3173417127826,6.72825283703624));
#60427=CARTESIAN_POINT('Ctrl Pts',(-17.41245333362,38.3160713382579,6.73380105682558));
#60428=CARTESIAN_POINT('Ctrl Pts',(-17.3920728509226,38.3137701171472,6.74423408161451));
#60429=CARTESIAN_POINT('Ctrl Pts',(-17.3829134300982,38.3127365617054,6.74906517504684));
#60430=CARTESIAN_POINT('Ctrl Pts',(-17.3602477065413,38.3101788602424,6.76137679775517));
#60431=CARTESIAN_POINT('Ctrl Pts',(-17.3468167662757,38.3086629145994,6.76899255979818));
#60432=CARTESIAN_POINT('Ctrl Pts',(-17.2625958038725,38.2991314819451,6.81879970857973));
#60433=CARTESIAN_POINT('Ctrl Pts',(-17.1959019073837,38.2914603565271,6.86755987551028));
#60434=CARTESIAN_POINT('Ctrl Pts',(-17.0984938198642,38.2792284803047,6.95448801984256));
#60435=CARTESIAN_POINT('Ctrl Pts',(-17.0644453845139,38.2747145515071,6.98853843346888));
#60436=CARTESIAN_POINT('Ctrl Pts',(-17.0092051794265,38.2668204807477,7.05044378092391));
#60437=CARTESIAN_POINT('Ctrl Pts',(-16.9870807916653,38.2634745808771,7.07739294505653));
#60438=CARTESIAN_POINT('Ctrl Pts',(-16.9542302326868,38.2581690661467,7.12094422761147));
#60439=CARTESIAN_POINT('Ctrl Pts',(-16.9427343459682,38.25623990979,7.1369460983174));
#60440=CARTESIAN_POINT('Ctrl Pts',(-16.9213462026713,38.2525009565014,7.1682285069406));
#60441=CARTESIAN_POINT('Ctrl Pts',(-16.9114010824907,38.250693741297,7.18346714822124));
#60442=CARTESIAN_POINT('Ctrl Pts',(-16.8882924262967,38.246319754514,7.22059504863165));
#60443=CARTESIAN_POINT('Ctrl Pts',(-16.8754558736915,38.2437418152971,7.2426769183748));
#60444=CARTESIAN_POINT('Ctrl Pts',(-16.824569092692,38.2328577040173,7.3366234092631));
#60445=CARTESIAN_POINT('Ctrl Pts',(-16.7928069620044,38.224346786645,7.41165684700205));
#60446=CARTESIAN_POINT('Ctrl Pts',(-16.7545701246106,38.2109028708543,7.53330991949744));
#60447=CARTESIAN_POINT('Ctrl Pts',(-16.7431229774018,38.2060224670745,7.57815368389028));
#60448=CARTESIAN_POINT('Ctrl Pts',(-16.7287133597135,38.1982803814804,7.65098946282639));
#60449=CARTESIAN_POINT('Ctrl Pts',(-16.7241887573008,38.195384404995,7.67863030656963));
#60450=CARTESIAN_POINT('Ctrl Pts',(-16.7189743124548,38.1912569763955,7.71877222552474));
#60451=CARTESIAN_POINT('Ctrl Pts',(-16.7175495595056,38.1899932446534,7.73116716701736));
#60452=CARTESIAN_POINT('Ctrl Pts',(-16.7152754110474,38.1876973347979,7.75389987776677));
#60453=CARTESIAN_POINT('Ctrl Pts',(-16.7143696595033,38.1866625624029,7.7642295727156));
#60454=CARTESIAN_POINT('Ctrl Pts',(-16.7124217274978,38.184092387392,7.79007985859153));
#60455=CARTESIAN_POINT('Ctrl Pts',(-16.7115379364456,38.1825653852408,7.80561070027402));
#60456=CARTESIAN_POINT('Ctrl Pts',(-16.7078119969442,38.1731307884693,7.9024160823585));
#60457=CARTESIAN_POINT('Ctrl Pts',(-16.7124959753099,38.1655568916047,7.98380542716558));
#60458=CARTESIAN_POINT('Ctrl Pts',(-16.7323676674995,38.1533821422053,8.1122306411467));
#60459=CARTESIAN_POINT('Ctrl Pts',(-16.7425499134142,38.1488241262221,8.15979098488128));
#60460=CARTESIAN_POINT('Ctrl Pts',(-16.7647275357339,38.1408652981565,8.24046279470303));
#60461=CARTESIAN_POINT('Ctrl Pts',(-16.7754191607689,38.1374995930019,8.27387418437521));
#60462=CARTESIAN_POINT('Ctrl Pts',(-16.7942662964075,38.1321705970052,8.32532967119125));
#60463=CARTESIAN_POINT('Ctrl Pts',(-16.8014849235645,38.1302382466433,8.34369994040799));
#60464=CARTESIAN_POINT('Ctrl Pts',(-16.8161707491735,38.1264974651681,8.3786571520249));
#60465=CARTESIAN_POINT('Ctrl Pts',(-16.8235720838452,38.1246916834838,8.39526660880723));
#60466=CARTESIAN_POINT('Ctrl Pts',(-16.8421798361182,38.1203288476713,8.43472352953543));
#60467=CARTESIAN_POINT('Ctrl Pts',(-16.8537208225479,38.1177607811575,8.45740306906119));
#60468=CARTESIAN_POINT('Ctrl Pts',(-16.9125639166615,38.1052768086952,8.5649200037193));
#60469=CARTESIAN_POINT('Ctrl Pts',(-16.9688043742522,38.0950518824559,8.64447311777763));
#60470=CARTESIAN_POINT('Ctrl Pts',(-17.0577420795365,38.0809973294834,8.74387521550877));
#60471=CARTESIAN_POINT('Ctrl Pts',(-17.0830958193713,38.0771823958861,8.76987823280343));
#60472=CARTESIAN_POINT('Ctrl Pts',(-17.1271289231425,38.0708983650362,8.8113262122702));
#60473=CARTESIAN_POINT('Ctrl Pts',(-17.1451985787768,38.0684069477507,8.82738756619677));
#60474=CARTESIAN_POINT('Ctrl Pts',(-17.1728118306571,38.0647386307379,8.85055503791356));
#60475=CARTESIAN_POINT('Ctrl Pts',(-17.182013269141,38.0635381997632,8.85805776186167));
#60476=CARTESIAN_POINT('Ctrl Pts',(-17.1995026857574,38.061299246945,8.87191464252989));
#60477=CARTESIAN_POINT('Ctrl Pts',(-17.2077655167593,38.060259073004,8.87829704352528));
#60478=CARTESIAN_POINT('Ctrl Pts',(-17.2295119773185,38.05756444592,8.89467033013827));
#60479=CARTESIAN_POINT('Ctrl Pts',(-17.2431168415203,38.0559206693928,8.90449739947941));
#60480=CARTESIAN_POINT('Ctrl Pts',(-17.3116957394469,38.0478172357043,8.95199352425984));
#60481=CARTESIAN_POINT('Ctrl Pts',(-17.3693886087074,38.0415677440801,8.98557039862542));
#60482=CARTESIAN_POINT('Ctrl Pts',(-17.4798590050485,38.0300815396568,9.03871161820281));
#60483=CARTESIAN_POINT('Ctrl Pts',(-17.5318015383826,38.0248568531135,9.05959884036158));
#60484=CARTESIAN_POINT('Ctrl Pts',(-17.6211317674732,38.015937632364,9.08883674993836));
#60485=CARTESIAN_POINT('Ctrl Pts',(-17.6578244661591,38.012292553772,9.09904505763649));
#60486=CARTESIAN_POINT('Ctrl Pts',(-17.7146105692434,38.0066330747568,9.11212595369512));
#60487=CARTESIAN_POINT('Ctrl Pts',(-17.7344086287793,38.0046567699047,9.1161914779871));
#60488=CARTESIAN_POINT('Ctrl Pts',(-17.7720504322914,38.0008869459159,9.12298944707232));
#60489=CARTESIAN_POINT('Ctrl Pts',(-17.7898720548233,37.9990969635814,9.12581720645946));
#60490=CARTESIAN_POINT('Ctrl Pts',(-17.831845995079,37.9948648690826,9.13156333570185));
#60491=CARTESIAN_POINT('Ctrl Pts',(-17.856032817531,37.9924135537111,9.13416912918405));
#60492=CARTESIAN_POINT('Ctrl Pts',(-17.973286790395,37.9804554308039,9.14340462387749));
#60493=CARTESIAN_POINT('Ctrl Pts',(-18.0667994732495,37.9706614131296,9.14045752181102));
#60494=CARTESIAN_POINT('Ctrl Pts',(-18.1990356764231,37.9565788141841,9.12161847205612));
#60495=CARTESIAN_POINT('Ctrl Pts',(-18.2386584939408,37.9523334922567,9.11403441921126));
#60496=CARTESIAN_POINT('Ctrl Pts',(-18.3029399376025,37.9454511942824,9.09852579939953));
#60497=CARTESIAN_POINT('Ctrl Pts',(-18.3278367798188,37.9427871377813,9.09171016040832));
#60498=CARTESIAN_POINT('Ctrl Pts',(-18.36411628046,37.938921689114,9.08057921542769));
#60499=CARTESIAN_POINT('Ctrl Pts',(-18.3756704962152,37.9376931698901,9.07685220919659));
#60500=CARTESIAN_POINT('Ctrl Pts',(-18.3969677371777,37.935435492855,9.06964365237925));
#60501=CARTESIAN_POINT('Ctrl Pts',(-18.4067238758456,37.934404186528,9.06620806574128));
#60502=CARTESIAN_POINT('Ctrl Pts',(-18.4315836755829,37.9317816272642,9.05711090055117));
#60503=CARTESIAN_POINT('Ctrl Pts',(-18.4466236339688,37.930199904274,9.05128006057468));
#60504=CARTESIAN_POINT('Ctrl Pts',(-18.5317870734777,37.9212477217241,9.0163824299917));
#60505=CARTESIAN_POINT('Ctrl Pts',(-18.5993158529918,37.914160632271,8.98135669529544));
#60506=CARTESIAN_POINT('Ctrl Pts',(-18.7063745890262,37.9022635166177,8.91301909582715));
#60507=CARTESIAN_POINT('Ctrl Pts',(-18.7477281708972,37.8974800210177,8.88296679479367));
#60508=CARTESIAN_POINT('Ctrl Pts',(-18.7949705016936,37.8916644219046,8.84407673226505));
#60509=CARTESIAN_POINT('Ctrl Pts',(-18.8027049932364,37.8907003227464,8.83755301826742));
#60510=CARTESIAN_POINT('Ctrl Pts',(-18.8103597914526,37.8897334522804,8.83093840423764));
#60511=CARTESIAN_POINT('Origin',(-17.98,42.93984859951,7.87));
#60512=CARTESIAN_POINT('',(-18.8103597855476,36.9267571849074,8.8309384093402));
#60513=CARTESIAN_POINT('',(-18.8103598139481,37.0958383925403,8.83093838479897));
#60514=CARTESIAN_POINT('',(-18.810359785549,42.93984859951,8.83093840933902));
#60515=CARTESIAN_POINT('',(-19.2481622217284,37.6108862619992,7.86948592254581));
#60516=CARTESIAN_POINT('Ctrl Pts',(-18.8103597855476,36.9267571849074,8.8309384093402));
#60517=CARTESIAN_POINT('Ctrl Pts',(-18.8032147727197,36.92770968048,8.83711251088705));
#60518=CARTESIAN_POINT('Ctrl Pts',(-18.796000732487,36.9286565669442,8.84320707286185));
#60519=CARTESIAN_POINT('Ctrl Pts',(-18.7789281998143,36.9308627477655,8.85730692212138));
#60520=CARTESIAN_POINT('Ctrl Pts',(-18.7690164583287,36.9321174496358,8.86524585090824));
#60521=CARTESIAN_POINT('Ctrl Pts',(-18.7356538134999,36.9362616373254,8.89115625551136));
#60522=CARTESIAN_POINT('Ctrl Pts',(-18.7116928525083,36.9391108481981,8.90845982068869));
#60523=CARTESIAN_POINT('Ctrl Pts',(-18.6449018654357,36.9467852874517,8.95323224648113));
#60524=CARTESIAN_POINT('Ctrl Pts',(-18.6009900105569,36.9515475452395,8.97899003559175));
#60525=CARTESIAN_POINT('Ctrl Pts',(-18.4896955937105,36.9632433025765,9.03558348480202));
#60526=CARTESIAN_POINT('Ctrl Pts',(-18.4209470858209,36.9701627390575,9.06328873037541));
#60527=CARTESIAN_POINT('Ctrl Pts',(-18.3255305213228,36.9797503580514,9.0923636527249));
#60528=CARTESIAN_POINT('Ctrl Pts',(-18.3006560116582,36.982247274934,9.09912316088744));
#60529=CARTESIAN_POINT('Ctrl Pts',(-18.2578643879094,36.9865521630873,9.10936425879658));
#60530=CARTESIAN_POINT('Ctrl Pts',(-18.2400455744002,36.9883474600287,9.11322507897373));
#60531=CARTESIAN_POINT('Ctrl Pts',(-18.2028847358233,36.992101612378,9.12044295582655));
#60532=CARTESIAN_POINT('Ctrl Pts',(-18.1835358043025,36.9940619456363,9.12373771440852));
#60533=CARTESIAN_POINT('Ctrl Pts',(-18.1301068798706,36.9994958824706,9.13156634041531));
#60534=CARTESIAN_POINT('Ctrl Pts',(-18.095910162572,37.0029973583274,9.13516638191484));
#60535=CARTESIAN_POINT('Ctrl Pts',(-18.0146737588531,37.0113819650799,9.14039765636493));
#60536=CARTESIAN_POINT('Ctrl Pts',(-17.9676080787579,37.0162932639401,9.14080993719881));
#60537=CARTESIAN_POINT('Ctrl Pts',(-17.835829115862,37.0301650074422,9.13464313778041));
#60538=CARTESIAN_POINT('Ctrl Pts',(-17.7516301602392,37.0391811380149,9.12218100248414));
#60539=CARTESIAN_POINT('Ctrl Pts',(-17.6545926545394,37.0494514364498,9.09769706672792));
#60540=CARTESIAN_POINT('Ctrl Pts',(-17.6399532677227,37.0509969477241,9.09372314033049));
#60541=CARTESIAN_POINT('Ctrl Pts',(-17.6154715581996,37.0535713957757,9.08660414816243));
#60542=CARTESIAN_POINT('Ctrl Pts',(-17.6055907512118,37.0546074955674,9.08359976546825));
#60543=CARTESIAN_POINT('Ctrl Pts',(-17.58364067524,37.0569020631242,9.07663192496756));
#60544=CARTESIAN_POINT('Ctrl Pts',(-17.5715923482799,37.058157101892,9.07260739855669));
#60545=CARTESIAN_POINT('Ctrl Pts',(-17.5317041161362,37.0623040875157,9.05861477728356));
#60546=CARTESIAN_POINT('Ctrl Pts',(-17.5041494145224,37.065155683937,9.04785438621417));
#60547=CARTESIAN_POINT('Ctrl Pts',(-17.4302198010537,37.0728399499147,9.01596527888472));
#60548=CARTESIAN_POINT('Ctrl Pts',(-17.3846994047278,37.0776094507408,8.99299278388375));
#60549=CARTESIAN_POINT('Ctrl Pts',(-17.2768454439438,37.0893020305867,8.93015631443276));
#60550=CARTESIAN_POINT('Ctrl Pts',(-17.2163870695905,37.0962112421349,8.88747280345882));
#60551=CARTESIAN_POINT('Ctrl Pts',(-17.1403056282913,37.1057879323274,8.82314089395605));
#60552=CARTESIAN_POINT('Ctrl Pts',(-17.1211386618713,37.1082847782095,8.8059066114038));
#60553=CARTESIAN_POINT('Ctrl Pts',(-17.0893309797913,37.1125895848295,8.77550597823357));
#60554=CARTESIAN_POINT('Ctrl Pts',(-17.0764249581612,37.1143848725165,8.76262782706307));
#60555=CARTESIAN_POINT('Ctrl Pts',(-17.0502099748453,37.1181390423304,8.7353182712188));
#60556=CARTESIAN_POINT('Ctrl Pts',(-17.0369496243363,37.1200994028227,8.72084727140804));
#60557=CARTESIAN_POINT('Ctrl Pts',(-17.0013991121509,37.12553352916,8.68019881367165));
#60558=CARTESIAN_POINT('Ctrl Pts',(-16.9798303666594,37.129035170718,8.65341684492043));
#60559=CARTESIAN_POINT('Ctrl Pts',(-16.9313821811308,37.1374203159222,8.58799267093613));
#60560=CARTESIAN_POINT('Ctrl Pts',(-16.9055130546705,37.1423319931642,8.54866751142825));
#60561=CARTESIAN_POINT('Ctrl Pts',(-16.839241869639,37.1562032654584,8.43460340653079));
#60562=CARTESIAN_POINT('Ctrl Pts',(-16.8040600152699,37.1652185060364,8.35710759355697));
#60563=CARTESIAN_POINT('Ctrl Pts',(-16.7720155421243,37.1754880770742,8.26230550034684));
#60564=CARTESIAN_POINT('Ctrl Pts',(-16.7674160264586,37.1770336847903,8.24784949301934));
#60565=CARTESIAN_POINT('Ctrl Pts',(-16.7601220713794,37.1796082388778,8.22341827832901));
#60566=CARTESIAN_POINT('Ctrl Pts',(-16.7572885300784,37.1806443497761,8.21348702979182));
#60567=CARTESIAN_POINT('Ctrl Pts',(-16.7512407667314,37.1829388741249,8.191266321197));
#60568=CARTESIAN_POINT('Ctrl Pts',(-16.7480891929481,37.184193859606,8.17896134760367));
#60569=CARTESIAN_POINT('Ctrl Pts',(-16.7382177390019,37.1883404025483,8.13786352204775));
#60570=CARTESIAN_POINT('Ctrl Pts',(-16.7323179536728,37.1911916215231,8.10888073979877));
#60571=CARTESIAN_POINT('Ctrl Pts',(-16.7190254406704,37.1988743319381,8.02948844936912));
#60572=CARTESIAN_POINT('Ctrl Pts',(-16.7136440230555,37.2036426860336,7.97879727898873));
#60573=CARTESIAN_POINT('Ctrl Pts',(-16.7079514469827,37.2153357665958,7.85409839389578));
#60574=CARTESIAN_POINT('Ctrl Pts',(-16.7110307687797,37.2222465948687,7.78013708005916));
#60575=CARTESIAN_POINT('Ctrl Pts',(-16.7238310514371,37.2318250137831,7.68131035823987));
#60576=CARTESIAN_POINT('Ctrl Pts',(-16.7279184201746,37.2343218717183,7.65586054195609));
#60577=CARTESIAN_POINT('Ctrl Pts',(-16.736214035353,37.2386266921784,7.6126503254698));
#60578=CARTESIAN_POINT('Ctrl Pts',(-16.7400362628188,37.2404219814352,7.59482328402615));
#60579=CARTESIAN_POINT('Ctrl Pts',(-16.7487672856928,37.2441761482803,7.55798845713815));
#60580=CARTESIAN_POINT('Ctrl Pts',(-16.7537357062197,37.2461365041465,7.53900004474447));
#60581=CARTESIAN_POINT('Ctrl Pts',(-16.7686120872288,37.2515705983024,7.48708862421732));
#60582=CARTESIAN_POINT('Ctrl Pts',(-16.7794191360676,37.2550722117221,7.45444396398152));
#60583=CARTESIAN_POINT('Ctrl Pts',(-16.8081185623732,37.2634572654977,7.37826160861739));
#60584=CARTESIAN_POINT('Ctrl Pts',(-16.8271325697097,37.2683688784931,7.33520245064047));
#60585=CARTESIAN_POINT('Ctrl Pts',(-16.8870362131116,37.2822402306931,7.2176684008618));
#60586=CARTESIAN_POINT('Ctrl Pts',(-16.9330731704459,37.2912556222798,7.14608487720421));
#60587=CARTESIAN_POINT('Ctrl Pts',(-16.9953525687587,37.3015253167339,7.067753474623));
#60588=CARTESIAN_POINT('Ctrl Pts',(-17.0050046249948,37.3030709080812,7.05605028027594));
#60589=CARTESIAN_POINT('Ctrl Pts',(-17.021576983394,37.3056454441737,7.03667415670937));
#60590=CARTESIAN_POINT('Ctrl Pts',(-17.0283849269966,37.3066815531887,7.02890819121319));
#60591=CARTESIAN_POINT('Ctrl Pts',(-17.0437758811704,37.3089760848798,7.01177759047472));
#60592=CARTESIAN_POINT('Ctrl Pts',(-17.0524058997014,37.3102310794118,7.00245718356506));
#60593=CARTESIAN_POINT('Ctrl Pts',(-17.081584890469,37.3143776975236,6.97187730149772));
#60594=CARTESIAN_POINT('Ctrl Pts',(-17.1027381710886,37.3172289805884,6.95120392874093));
#60595=CARTESIAN_POINT('Ctrl Pts',(-17.1622395118933,37.3249119551117,6.89698334720371));
#60596=CARTESIAN_POINT('Ctrl Pts',(-17.2019149886439,37.3296805038975,6.8649735121972));
#60597=CARTESIAN_POINT('Ctrl Pts',(-17.3036024417685,37.3413734993826,6.7925742360146));
#60598=CARTESIAN_POINT('Ctrl Pts',(-17.3674134391802,37.3482840531108,6.75505806825942));
#60599=CARTESIAN_POINT('Ctrl Pts',(-17.4573877313516,37.3578621784835,6.71222600487515));
#60600=CARTESIAN_POINT('Ctrl Pts',(-17.480987505808,37.3603590343976,6.70186023115464));
#60601=CARTESIAN_POINT('Ctrl Pts',(-17.5217918187434,37.364663852542,6.68539979598401));
#60602=CARTESIAN_POINT('Ctrl Pts',(-17.5388430335696,37.3664591415407,6.67894465896834));
#60603=CARTESIAN_POINT('Ctrl Pts',(-17.5745267446772,37.3702133088996,6.66630708269495));
#60604=CARTESIAN_POINT('Ctrl Pts',(-17.5931752950012,37.3721736655526,6.6601852470418));
#60605=CARTESIAN_POINT('Ctrl Pts',(-17.644858999498,37.3776077651561,6.64453587983283));
#60606=CARTESIAN_POINT('Ctrl Pts',(-17.6781478086027,37.381109383335,6.6359147162447));
#60607=CARTESIAN_POINT('Ctrl Pts',(-17.757720017215,37.389494452571,6.61871890921272));
#60608=CARTESIAN_POINT('Ctrl Pts',(-17.8042095413234,37.394406076429,6.61134617358325));
#60609=CARTESIAN_POINT('Ctrl Pts',(-17.9354463509943,37.4082774150947,6.59794603608985));
#60610=CARTESIAN_POINT('Ctrl Pts',(-18.0205553622639,37.4172927811241,6.5978112899045));
#60611=CARTESIAN_POINT('Ctrl Pts',(-18.1201415089112,37.4275624546922,6.6076647000054));
#60612=CARTESIAN_POINT('Ctrl Pts',(-18.1352085804882,37.4291080488103,6.60942853242417));
#60613=CARTESIAN_POINT('Ctrl Pts',(-18.1604751086731,37.4316825879504,6.6128463200297));
#60614=CARTESIAN_POINT('Ctrl Pts',(-18.1706918102567,37.4327186972858,6.61435541990018));
#60615=CARTESIAN_POINT('Ctrl Pts',(-18.1934309520643,37.4350132277385,6.61799818962467));
#60616=CARTESIAN_POINT('Ctrl Pts',(-18.2059417207708,37.4362682207414,6.6201953385972));
#60617=CARTESIAN_POINT('Ctrl Pts',(-18.2474576090307,37.440414826157,6.62813023583685));
#60618=CARTESIAN_POINT('Ctrl Pts',(-18.2762979595537,37.4432660983974,6.63469354030739));
#60619=CARTESIAN_POINT('Ctrl Pts',(-18.3541190855989,37.4509490283154,6.65528666116701));
#60620=CARTESIAN_POINT('Ctrl Pts',(-18.4025279273838,37.45571754422,6.67126540056843));
#60621=CARTESIAN_POINT('Ctrl Pts',(-18.5184990658107,37.4674105540678,6.71744684913855));
#60622=CARTESIAN_POINT('Ctrl Pts',(-18.5846226474918,37.4743211541578,6.750719277603));
#60623=CARTESIAN_POINT('Ctrl Pts',(-18.6693996600084,37.4838993290987,6.80309217075874));
#60624=CARTESIAN_POINT('Ctrl Pts',(-18.6909060815612,37.4863961853522,6.81730035988232));
#60625=CARTESIAN_POINT('Ctrl Pts',(-18.7268624561893,37.4907010038829,6.84265932997988));
#60626=CARTESIAN_POINT('Ctrl Pts',(-18.7415321487791,37.4924962929224,6.85348581868069));
#60627=CARTESIAN_POINT('Ctrl Pts',(-18.7714998507502,37.4962504601872,6.87661528793545));
#60628=CARTESIAN_POINT('Ctrl Pts',(-18.7867556450977,37.4982108167026,6.88896461943294));
#60629=CARTESIAN_POINT('Ctrl Pts',(-18.82792984546,37.503644915365,6.92390445689966));
#60630=CARTESIAN_POINT('Ctrl Pts',(-18.8532242472879,37.5071465327236,6.94719956304562));
#60631=CARTESIAN_POINT('Ctrl Pts',(-18.9108202282476,37.5155315992946,7.00473330125536));
#60632=CARTESIAN_POINT('Ctrl Pts',(-18.9422237122834,37.5204432212802,7.03979685257261));
#60633=CARTESIAN_POINT('Ctrl Pts',(-19.0246454802072,37.5343145623159,7.1427984169679));
#60634=CARTESIAN_POINT('Ctrl Pts',(-19.07090877644,37.5433299327892,7.2142356368844));
#60635=CARTESIAN_POINT('Ctrl Pts',(-19.1166299938529,37.5535996099898,7.30325287026133));
#60636=CARTESIAN_POINT('Ctrl Pts',(-19.1233180506155,37.5551452036275,7.31686894561871));
#60637=CARTESIAN_POINT('Ctrl Pts',(-19.1341470404879,37.5577197422377,7.33995165424622));
#60638=CARTESIAN_POINT('Ctrl Pts',(-19.1384190347504,37.5587558515162,7.34935422987331));
#60639=CARTESIAN_POINT('Ctrl Pts',(-19.1476885271846,37.5610503821786,7.37043538152376));
#60640=CARTESIAN_POINT('Ctrl Pts',(-19.1526263600369,37.5623053754431,7.38213857227139));
#60641=CARTESIAN_POINT('Ctrl Pts',(-19.168471153579,37.5664519830324,7.4213237224336));
#60642=CARTESIAN_POINT('Ctrl Pts',(-19.1785951192066,37.5693032571264,7.44911489503905));
#60643=CARTESIAN_POINT('Ctrl Pts',(-19.2034906236037,37.5769861946825,7.52566834882584));
#60644=CARTESIAN_POINT('Ctrl Pts',(-19.2163145043556,37.5817547162179,7.57500687819286));
#60645=CARTESIAN_POINT('Ctrl Pts',(-19.2371219520155,37.5918576196773,7.68083363887858));
#60646=CARTESIAN_POINT('Ctrl Pts',(-19.2443350737353,37.59718194391,7.73735183038249));
#60647=CARTESIAN_POINT('Ctrl Pts',(-19.2492360708524,37.6049924265085,7.81927636743861));
#60648=CARTESIAN_POINT('Ctrl Pts',(-19.2499917500813,37.6074024411012,7.8444297094667));
#60649=CARTESIAN_POINT('Ctrl Pts',(-19.249999932819,37.6098335524356,7.8695869145078));
#60650=CARTESIAN_POINT('Ctrl Pts',(-18.8099615219027,37.7194233520466,8.8304622415412));
#60651=CARTESIAN_POINT('Ctrl Pts',(-18.9016773777114,37.7074747109911,8.75269843125987));
#60652=CARTESIAN_POINT('Ctrl Pts',(-19.1457002117025,37.6713007271388,8.4794805454805));
#60653=CARTESIAN_POINT('Ctrl Pts',(-19.2472428947117,37.6351267432866,8.11387022531887));
#60654=CARTESIAN_POINT('Ctrl Pts',(-19.2481357945224,37.61090140049,7.86948447023081));
#60655=CARTESIAN_POINT('Ctrl Pts',(-18.8103597914526,37.8897334522804,8.83093840423764));
#60656=CARTESIAN_POINT('Ctrl Pts',(-18.8300348678934,37.8872483116158,8.81393690622473));
#60657=CARTESIAN_POINT('Ctrl Pts',(-18.8491834500945,37.884744708031,8.79633489929289));
#60658=CARTESIAN_POINT('Ctrl Pts',(-18.8820134020668,37.8802822135894,8.76424162825049));
#60659=CARTESIAN_POINT('Ctrl Pts',(-18.8959180353935,37.8783340914939,8.74999449475032));
#60660=CARTESIAN_POINT('Ctrl Pts',(-18.9218326402294,37.8745836694053,8.72216184613498));
#60661=CARTESIAN_POINT('Ctrl Pts',(-18.9338978123935,37.8727843460154,8.70863425330909));
#60662=CARTESIAN_POINT('Ctrl Pts',(-18.9619094478656,37.868472964352,8.67584062268679));
#60663=CARTESIAN_POINT('Ctrl Pts',(-18.9775836357603,37.8659506076449,8.65635356894627));
#60664=CARTESIAN_POINT('Ctrl Pts',(-19.04543573706,37.8545064982477,8.56670035962305));
#60665=CARTESIAN_POINT('Ctrl Pts',(-19.0908482208755,37.8453401152098,8.49173493060826));
#60666=CARTESIAN_POINT('Ctrl Pts',(-19.1465824485972,37.8315882950702,8.37382196217949));
#60667=CARTESIAN_POINT('Ctrl Pts',(-19.1629813568602,37.8270527903362,8.33401156590888));
#60668=CARTESIAN_POINT('Ctrl Pts',(-19.1862766564356,37.8197744014533,8.26814176587284));
#60669=CARTESIAN_POINT('Ctrl Pts',(-19.1944215314265,37.8170011561596,8.24255994228225));
#60670=CARTESIAN_POINT('Ctrl Pts',(-19.2051086219464,37.8130119647009,8.20490321993921));
#60671=CARTESIAN_POINT('Ctrl Pts',(-19.2082950704449,37.8117665114033,8.19302099989463));
#60672=CARTESIAN_POINT('Ctrl Pts',(-19.2138594272067,37.8094846536562,8.17099726688584));
#60673=CARTESIAN_POINT('Ctrl Pts',(-19.216285896331,37.808445973111,8.16087048729322));
#60674=CARTESIAN_POINT('Ctrl Pts',(-19.2221012019579,37.8058387315869,8.13521172880683));
#60675=CARTESIAN_POINT('Ctrl Pts',(-19.2253235487809,37.8042791626728,8.11964375305414));
#60676=CARTESIAN_POINT('Ctrl Pts',(-19.2426459370111,37.795130771309,8.02724607696535));
#60677=CARTESIAN_POINT('Ctrl Pts',(-19.2499282836218,37.7878452278459,7.94929534338273));
#60678=CARTESIAN_POINT('Ctrl Pts',(-19.2500624775109,37.7740476776123,7.80200242607106));
#60679=CARTESIAN_POINT('Ctrl Pts',(-19.2444771305498,37.767565959847,7.73296711427041));
#60680=CARTESIAN_POINT('Ctrl Pts',(-19.2291580819846,37.7584540476398,7.63943217797024));
#60681=CARTESIAN_POINT('Ctrl Pts',(-19.2242489537417,37.7559695433459,7.61426232146536));
#60682=CARTESIAN_POINT('Ctrl Pts',(-19.2145565353906,37.7516791989012,7.57150081758896));
#60683=CARTESIAN_POINT('Ctrl Pts',(-19.2101499181603,37.7498858137683,7.55383122577677));
#60684=CARTESIAN_POINT('Ctrl Pts',(-19.200197431579,37.7461294947516,7.51728912017404));
#60685=CARTESIAN_POINT('Ctrl Pts',(-19.1945899766567,37.7441649971644,7.49843868119012));
#60686=CARTESIAN_POINT('Ctrl Pts',(-19.1779045879273,37.7387004445672,7.44676945610031));
#60687=CARTESIAN_POINT('Ctrl Pts',(-19.1659192761353,37.7351719517395,7.41426500407277));
#60688=CARTESIAN_POINT('Ctrl Pts',(-19.1343369829196,37.726698944372,7.33832961017935));
#60689=CARTESIAN_POINT('Ctrl Pts',(-19.1135956950872,37.7217253240388,7.29543318194078));
#60690=CARTESIAN_POINT('Ctrl Pts',(-19.0499550046961,37.7079298625437,7.18074041689903));
#60691=CARTESIAN_POINT('Ctrl Pts',(-19.0022965308763,37.6990587882167,7.1118477773202));
#60692=CARTESIAN_POINT('Ctrl Pts',(-18.938301227963,37.6889075712726,7.03645741087996));
#60693=CARTESIAN_POINT('Ctrl Pts',(-18.9281803210313,37.687346721933,7.02496233911568));
#60694=CARTESIAN_POINT('Ctrl Pts',(-18.9108806070277,37.6847555416129,7.00601607517522));
#60695=CARTESIAN_POINT('Ctrl Pts',(-18.9038147120301,37.6837178049028,6.99846494986995));
#60696=CARTESIAN_POINT('Ctrl Pts',(-18.8879295768371,37.6814305695523,6.98189929332437));
#60697=CARTESIAN_POINT('Ctrl Pts',(-18.8790670054897,37.6801843333883,6.97292834802095));
#60698=CARTESIAN_POINT('Ctrl Pts',(-18.8494406842844,37.6761085995669,6.94381998775933));
#60699=CARTESIAN_POINT('Ctrl Pts',(-18.8281206851935,37.6733175590677,6.92425783440027));
#60700=CARTESIAN_POINT('Ctrl Pts',(-18.7689642970215,37.6658789910054,6.87359028598551));
#60701=CARTESIAN_POINT('Ctrl Pts',(-18.7299661820066,37.6612897773079,6.84391591089947));
#60702=CARTESIAN_POINT('Ctrl Pts',(-18.6256367778902,37.6495062819862,6.77366387540398));
#60703=CARTESIAN_POINT('Ctrl Pts',(-18.5581725166867,37.6423318853709,6.73663595867115));
#60704=CARTESIAN_POINT('Ctrl Pts',(-18.4641850231329,37.6324755064397,6.69563733148107));
#60705=CARTESIAN_POINT('Ctrl Pts',(-18.4402817772613,37.6299811927968,6.68606449425396));
#60706=CARTESIAN_POINT('Ctrl Pts',(-18.3989897993358,37.6256795994836,6.67096719033118));
#60707=CARTESIAN_POINT('Ctrl Pts',(-18.3817419663761,37.6238849511069,6.66507865947308));
#60708=CARTESIAN_POINT('Ctrl Pts',(-18.3456658829058,37.6201311300037,6.65362268630146));
#60709=CARTESIAN_POINT('Ctrl Pts',(-18.3268234522634,37.6181704655535,6.64811674492403));
#60710=CARTESIAN_POINT('Ctrl Pts',(-18.2746179459316,37.612732619033,6.63416652777873));
#60711=CARTESIAN_POINT('Ctrl Pts',(-18.2410305442971,37.6092274850052,6.62663899389277));
#60712=CARTESIAN_POINT('Ctrl Pts',(-18.1608253925956,37.6008306843994,6.61205634645845));
#60713=CARTESIAN_POINT('Ctrl Pts',(-18.1140404250063,37.5959107175078,6.60621512898476));
#60714=CARTESIAN_POINT('Ctrl Pts',(-17.9825334047712,37.5820496667026,6.59718052106978));
#60715=CARTESIAN_POINT('Ctrl Pts',(-17.8976470506054,37.5730538159799,6.59984395902575));
#60716=CARTESIAN_POINT('Ctrl Pts',(-17.7985964209878,37.5628002568999,6.61293064661125));
#60717=CARTESIAN_POINT('Ctrl Pts',(-17.7835767736196,37.5612527067091,6.6151898110559));
#60718=CARTESIAN_POINT('Ctrl Pts',(-17.7584173899679,37.5586762016982,6.61943701142443));
#60719=CARTESIAN_POINT('Ctrl Pts',(-17.7482555591945,37.5576400494988,6.62128017800801));
#60720=CARTESIAN_POINT('Ctrl Pts',(-17.7256644858379,37.5553471162272,6.6256630989959));
#60721=CARTESIAN_POINT('Ctrl Pts',(-17.7132488896122,37.5540937360872,6.62826541875204));
#60722=CARTESIAN_POINT('Ctrl Pts',(-17.6721387845193,37.5499593837391,6.63752725712236));
#60723=CARTESIAN_POINT('Ctrl Pts',(-17.643634326914,37.5471184277162,6.64499952405626));
#60724=CARTESIAN_POINT('Ctrl Pts',(-17.5669539627857,37.5394775957703,6.66798000669751));
#60725=CARTESIAN_POINT('Ctrl Pts',(-17.5194025060431,37.5347400201923,6.68538616565481));
#60726=CARTESIAN_POINT('Ctrl Pts',(-17.4048165879097,37.5230329594593,6.73527695349495));
#60727=CARTESIAN_POINT('Ctrl Pts',(-17.3393695002255,37.5160782339928,6.77089911019834));
#60728=CARTESIAN_POINT('Ctrl Pts',(-17.2559512047949,37.5064532264038,6.826296244133));
#60729=CARTESIAN_POINT('Ctrl Pts',(-17.2349230539527,37.5039564137256,6.84120249119583));
#60730=CARTESIAN_POINT('Ctrl Pts',(-17.1998212331697,37.4996519518082,6.86772590658961));
#60731=CARTESIAN_POINT('Ctrl Pts',(-17.1855172287835,37.4978569788531,6.87902608181375));
#60732=CARTESIAN_POINT('Ctrl Pts',(-17.1563320419713,37.4941037771619,6.90312046056595));
#60733=CARTESIAN_POINT('Ctrl Pts',(-17.1414944667088,37.4921440748641,6.91595948276378));
#60734=CARTESIAN_POINT('Ctrl Pts',(-17.1015097625954,37.4867129194701,6.95221180615699));
#60735=CARTESIAN_POINT('Ctrl Pts',(-17.0770083707477,37.4832136355872,6.97630776129775));
#60736=CARTESIAN_POINT('Ctrl Pts',(-17.0213745734389,37.4748358492621,7.0356465583227));
#60737=CARTESIAN_POINT('Ctrl Pts',(-16.9911642464969,37.4699292454559,7.07168226249463));
#60738=CARTESIAN_POINT('Ctrl Pts',(-16.9121105187079,37.4560515609369,7.17736951288542));
#60739=CARTESIAN_POINT('Ctrl Pts',(-16.8681559722528,37.4470242886199,7.25037887929964));
#60740=CARTESIAN_POINT('Ctrl Pts',(-16.8253469751711,37.4367450435555,7.34093854392923));
#60741=CARTESIAN_POINT('Ctrl Pts',(-16.8191159331536,37.4352008949839,7.35475453287355));
#60742=CARTESIAN_POINT('Ctrl Pts',(-16.8090581676939,37.4326281315143,7.37816486859752));
#60743=CARTESIAN_POINT('Ctrl Pts',(-16.8050987290957,37.4315923725561,7.38769966535942));
#60744=CARTESIAN_POINT('Ctrl Pts',(-16.7965270808923,37.4292979219784,7.40907351367023));
#60745=CARTESIAN_POINT('Ctrl Pts',(-16.7919754670223,37.4280426674629,7.42093526803272));
#60746=CARTESIAN_POINT('Ctrl Pts',(-16.7774151962916,37.4238927630328,7.46065206558879));
#60747=CARTESIAN_POINT('Ctrl Pts',(-16.7682012606276,37.4210385484136,7.48879112757948));
#60748=CARTESIAN_POINT('Ctrl Pts',(-16.7458037897351,37.4133431719075,7.56625067365603));
#60749=CARTESIAN_POINT('Ctrl Pts',(-16.7345955526899,37.4085654082228,7.61608543269077));
#60750=CARTESIAN_POINT('Ctrl Pts',(-16.7145964222888,37.3968762057408,7.73926028246334));
#60751=CARTESIAN_POINT('Ctrl Pts',(-16.7091416258319,37.3899784178123,7.81293899509459));
#60752=CARTESIAN_POINT('Ctrl Pts',(-16.7104475938165,37.3804141991619,7.91243468420286));
#60753=CARTESIAN_POINT('Ctrl Pts',(-16.7115698864676,37.3779177016801,7.93818242760502));
#60754=CARTESIAN_POINT('Ctrl Pts',(-16.7148216951835,37.3736136016348,7.98205403335076));
#60755=CARTESIAN_POINT('Ctrl Pts',(-16.7165601537087,37.3718186696788,8.00019953121382));
#60756=CARTESIAN_POINT('Ctrl Pts',(-16.7209795700339,37.3680653902383,8.03778721898458));
#60757=CARTESIAN_POINT('Ctrl Pts',(-16.7237219040064,37.3661055669052,8.05721706242381));
#60758=CARTESIAN_POINT('Ctrl Pts',(-16.7325021958648,37.360673570058,8.11047864163257));
#60759=CARTESIAN_POINT('Ctrl Pts',(-16.7394643874593,37.3571735505313,8.14413787797057));
#60760=CARTESIAN_POINT('Ctrl Pts',(-16.7591624715368,37.34879337476,8.2230801174656));
#60761=CARTESIAN_POINT('Ctrl Pts',(-16.7730656431776,37.3438850921945,8.26801794079559));
#60762=CARTESIAN_POINT('Ctrl Pts',(-16.8190003224163,37.3300095043497,8.39172645694));
#60763=CARTESIAN_POINT('Ctrl Pts',(-16.8564955624613,37.3209861875035,8.46821322664545));
#60764=CARTESIAN_POINT('Ctrl Pts',(-16.9093537069664,37.3107101738324,8.55326149576562));
#60765=CARTESIAN_POINT('Ctrl Pts',(-16.9175854348212,37.3091655957653,8.56599218683689));
#60766=CARTESIAN_POINT('Ctrl Pts',(-16.9318037602163,37.3065923601604,8.58714100625244));
#60767=CARTESIAN_POINT('Ctrl Pts',(-16.9376682440562,37.3055565518295,8.59563842825465));
#60768=CARTESIAN_POINT('Ctrl Pts',(-16.9509776385803,37.3032622942126,8.61442883636469));
#60769=CARTESIAN_POINT('Ctrl Pts',(-16.9584744134487,37.302007277446,8.62468326939275));
#60770=CARTESIAN_POINT('Ctrl Pts',(-16.9839371151218,37.297859349712,8.65843744638727));
#60771=CARTESIAN_POINT('Ctrl Pts',(-17.0025716876115,37.2950068206424,8.68142419151736));
#60772=CARTESIAN_POINT('Ctrl Pts',(-17.0554574247065,37.2873183978818,8.74219219273994));
#60773=CARTESIAN_POINT('Ctrl Pts',(-17.091207815977,37.2825457618921,8.77859647422016));
#60774=CARTESIAN_POINT('Ctrl Pts',(-17.1838586369744,37.2708543423037,8.86222466339401));
#60775=CARTESIAN_POINT('Ctrl Pts',(-17.242866698744,37.2639493447231,8.90681397703108));
#60776=CARTESIAN_POINT('Ctrl Pts',(-17.3272409798854,37.2543774105935,8.95971083770372));
#60777=CARTESIAN_POINT('Ctrl Pts',(-17.3494838245695,37.251880851879,8.97272987741142));
#60778=CARTESIAN_POINT('Ctrl Pts',(-17.3881094986076,37.2475766815356,8.9937872961838));
#60779=CARTESIAN_POINT('Ctrl Pts',(-17.4042984388306,37.2457817416169,9.00216601208701));
#60780=CARTESIAN_POINT('Ctrl Pts',(-17.4382766132721,37.2420284772915,9.01883452134757));
#60781=CARTESIAN_POINT('Ctrl Pts',(-17.4560887486572,37.2400686774807,9.02706606332457));
#60782=CARTESIAN_POINT('Ctrl Pts',(-17.5055997441572,37.234636844165,9.04856906963251));
#60783=CARTESIAN_POINT('Ctrl Pts',(-17.5376547931556,37.231136967607,9.06097053128938));
#60784=CARTESIAN_POINT('Ctrl Pts',(-17.6146605148829,37.2227572562461,9.08722496518036));
#60785=CARTESIAN_POINT('Ctrl Pts',(-17.6599540555282,37.217849299974,9.09991021275116));
#60786=CARTESIAN_POINT('Ctrl Pts',(-17.7888078696275,37.2039733047731,9.12839799701166));
#60787=CARTESIAN_POINT('Ctrl Pts',(-17.8734122417257,37.1949492193082,9.13836963777536));
#60788=CARTESIAN_POINT('Ctrl Pts',(-17.9735398806138,37.1846725776728,9.14007401323111));
#60789=CARTESIAN_POINT('Ctrl Pts',(-17.9886992834016,37.1831280830351,9.14006067994603));
#60790=CARTESIAN_POINT('Ctrl Pts',(-18.0141778891335,37.1805549391477,9.13958199818897));
#60791=CARTESIAN_POINT('Ctrl Pts',(-18.0244975003084,37.1795191404128,9.13926222222058));
#60792=CARTESIAN_POINT('Ctrl Pts',(-18.0475029378813,37.1772248453393,9.1382683779033));
#60793=CARTESIAN_POINT('Ctrl Pts',(-18.0601844934833,37.1759697824103,9.13752981045374));
#60794=CARTESIAN_POINT('Ctrl Pts',(-18.1023564244237,37.1718214709779,9.13443821097716));
#60795=CARTESIAN_POINT('Ctrl Pts',(-18.1317783168588,37.1689686147343,9.1312449696965));
#60796=CARTESIAN_POINT('Ctrl Pts',(-18.2115280182011,37.1612788426634,9.11975761064508));
#60797=CARTESIAN_POINT('Ctrl Pts',(-18.261511607922,37.1565052117878,9.10945610176486));
#60798=CARTESIAN_POINT('Ctrl Pts',(-18.3820116156005,37.1448142237615,9.07695286895875));
#60799=CARTESIAN_POINT('Ctrl Pts',(-18.4514582369022,37.1379106262632,9.05155557322976));
#60800=CARTESIAN_POINT('Ctrl Pts',(-18.54164070453,37.1283401900378,9.00935234273155));
#60801=CARTESIAN_POINT('Ctrl Pts',(-18.5646405437834,37.1258436427352,8.99772304148919));
#60802=CARTESIAN_POINT('Ctrl Pts',(-18.6032779015198,37.12153948549,8.97668735854328));
#60803=CARTESIAN_POINT('Ctrl Pts',(-18.6190962389709,37.1197445470522,8.9676284267324));
#60804=CARTESIAN_POINT('Ctrl Pts',(-18.6515260036642,37.1159912799001,8.9481177176939));
#60805=CARTESIAN_POINT('Ctrl Pts',(-18.6681009036295,37.1140314756987,8.93761510959687));
#60806=CARTESIAN_POINT('Ctrl Pts',(-18.7130155425385,37.1085996118756,8.90767474987375));
#60807=CARTESIAN_POINT('Ctrl Pts',(-18.7408174193683,37.1050997086488,8.8874659504289));
#60808=CARTESIAN_POINT('Ctrl Pts',(-18.7822189556672,37.0996632089337,8.85472555352821));
#60809=CARTESIAN_POINT('Ctrl Pts',(-18.7964211951468,37.09775501192,8.8429829332296));
#60810=CARTESIAN_POINT('Ctrl Pts',(-18.8103598139481,37.0958383925403,8.83093838479897));
#60811=CARTESIAN_POINT('Origin',(-17.98,42.93984859951,7.87));
#60812=CARTESIAN_POINT('',(-18.8103594475449,36.1311618021068,8.83093870141285));
#60813=CARTESIAN_POINT('',(-18.8103597855904,36.3002088453023,8.83093840930324));
#60814=CARTESIAN_POINT('',(-18.810359785549,42.93984859951,8.83093840933902));
#60815=CARTESIAN_POINT('Ctrl Pts',(-18.8103594475449,36.1311618021068,8.83093870141285));
#60816=CARTESIAN_POINT('Ctrl Pts',(-18.7760032109335,36.1358942904264,8.86062636578764));
#60817=CARTESIAN_POINT('Ctrl Pts',(-18.7400620458144,36.1406769039139,8.88846536013866));
#60818=CARTESIAN_POINT('Ctrl Pts',(-18.6665241498893,36.1501062373779,8.93935421122266));
#60819=CARTESIAN_POINT('Ctrl Pts',(-18.6290854197678,36.1547435258644,8.96248450985219));
#60820=CARTESIAN_POINT('Ctrl Pts',(-18.5666796502928,36.1621596382488,8.9966970231326));
#60821=CARTESIAN_POINT('Ctrl Pts',(-18.5424227771892,36.1649699795933,9.00899962838746));
#60822=CARTESIAN_POINT('Ctrl Pts',(-18.5065938376522,36.1690012000212,9.02574719947508));
#60823=CARTESIAN_POINT('Ctrl Pts',(-18.4953241691024,36.1702524118464,9.03081596489765));
#60824=CARTESIAN_POINT('Ctrl Pts',(-18.4744338531305,36.1725389076545,9.03984758028955));
#60825=CARTESIAN_POINT('Ctrl Pts',(-18.4648362781758,36.1735765644151,9.04385774131803));
#60826=CARTESIAN_POINT('Ctrl Pts',(-18.4405426876497,36.176172958714,9.05365952841414));
#60827=CARTESIAN_POINT('Ctrl Pts',(-18.4257858197682,36.177722882049,9.05929581490953));
#60828=CARTESIAN_POINT('Ctrl Pts',(-18.3365431046723,36.1869573385961,9.09148671033355));
#60829=CARTESIAN_POINT('Ctrl Pts',(-18.2598022207941,36.1943296290845,9.11131709898632));
#60830=CARTESIAN_POINT('Ctrl Pts',(-18.1327162635908,36.2063876872943,9.13176046738748));
#60831=CARTESIAN_POINT('Ctrl Pts',(-18.0833139910934,36.2110381057285,9.13676254922227));
#60832=CARTESIAN_POINT('Ctrl Pts',(-17.9982701370895,36.2191322722624,9.1403649796513));
#60833=CARTESIAN_POINT('Ctrl Pts',(-17.9627481523514,36.2225390696275,9.14037901732945));
#60834=CARTESIAN_POINT('Ctrl Pts',(-17.9074823685278,36.2279170356055,9.13808266363422));
#60835=CARTESIAN_POINT('Ctrl Pts',(-17.887712503366,36.2298562566793,9.13679728417607));
#60836=CARTESIAN_POINT('Ctrl Pts',(-17.8498905258271,36.2336016819869,9.1334482166024));
#60837=CARTESIAN_POINT('Ctrl Pts',(-17.8318366519856,36.2354051003027,9.13145844408052));
#60838=CARTESIAN_POINT('Ctrl Pts',(-17.7887846573185,36.2397472464753,9.12577666432706));
#60839=CARTESIAN_POINT('Ctrl Pts',(-17.7638431566658,36.2422966907281,9.12172453951716));
#60840=CARTESIAN_POINT('Ctrl Pts',(-17.679209070971,36.2510740921771,9.10536973848571));
#60841=CARTESIAN_POINT('Ctrl Pts',(-17.6202977585061,36.2574055641937,9.08951847377857));
#60842=CARTESIAN_POINT('Ctrl Pts',(-17.4934166814106,36.2715171064884,9.04538383016372));
#60843=CARTESIAN_POINT('Ctrl Pts',(-17.4262930972196,36.2793054042464,9.01529466089719));
#60844=CARTESIAN_POINT('Ctrl Pts',(-17.341351115357,36.2894047168989,8.96799543251322));
#60845=CARTESIAN_POINT('Ctrl Pts',(-17.3208861168189,36.2918571169645,8.95583401132522));
#60846=CARTESIAN_POINT('Ctrl Pts',(-17.2907939889241,36.2954807764256,8.93678702139078));
#60847=CARTESIAN_POINT('Ctrl Pts',(-17.28090289296,36.296674781475,8.93033143375505));
#60848=CARTESIAN_POINT('Ctrl Pts',(-17.2624148785197,36.2989102097108,8.91789371109461));
#60849=CARTESIAN_POINT('Ctrl Pts',(-17.2538000170136,36.2999531653736,8.91194205118032));
#60850=CARTESIAN_POINT('Ctrl Pts',(-17.2314264828812,36.3026679140627,8.89607274675867));
#60851=CARTESIAN_POINT('Ctrl Pts',(-17.2177907841818,36.3043287141557,8.88598464924799));
#60852=CARTESIAN_POINT('Ctrl Pts',(-17.1600139109664,36.3114141695364,8.84142129025013));
#60853=CARTESIAN_POINT('Ctrl Pts',(-17.1179716125759,36.3166957952928,8.8043155506681));
#60854=CARTESIAN_POINT('Ctrl Pts',(-17.0344597503872,36.3278223543935,8.72015583011394));
#60855=CARTESIAN_POINT('Ctrl Pts',(-16.9937494427379,36.3336474510445,8.67257128352692));
#60856=CARTESIAN_POINT('Ctrl Pts',(-16.932750873755,36.3434033739125,8.58958726783062));
#60857=CARTESIAN_POINT('Ctrl Pts',(-16.9103648384086,36.3472697650717,8.55586914786252));
#60858=CARTESIAN_POINT('Ctrl Pts',(-16.8790825672184,36.3531900323301,8.50348546073653));
#60859=CARTESIAN_POINT('Ctrl Pts',(-16.868968657173,36.3551996631879,8.4855747388844));
#60860=CARTESIAN_POINT('Ctrl Pts',(-16.8508370113967,36.3589957492767,8.45156186212521));
#60861=CARTESIAN_POINT('Ctrl Pts',(-16.842717727256,36.360778041389,8.43551940891076));
#60862=CARTESIAN_POINT('Ctrl Pts',(-16.8248844867213,36.3648936738787,8.39834540484185));
#60863=CARTESIAN_POINT('Ctrl Pts',(-16.815405380893,36.3672344693827,8.3771093623447));
#60864=CARTESIAN_POINT('Ctrl Pts',(-16.7684350720293,36.3797052177042,8.26360876050272));
#60865=CARTESIAN_POINT('Ctrl Pts',(-16.7413191913173,36.3901731741449,8.16745199653552));
#60866=CARTESIAN_POINT('Ctrl Pts',(-16.7198013335341,36.4046364467897,8.03192471143991));
#60867=CARTESIAN_POINT('Ctrl Pts',(-16.715551042996,36.4086000772414,7.99445691334066));
#60868=CARTESIAN_POINT('Ctrl Pts',(-16.7112808195574,36.4150924192366,7.93216225369074));
#60869=CARTESIAN_POINT('Ctrl Pts',(-16.7103101997785,36.417645075277,7.90742438437514));
#60870=CARTESIAN_POINT('Ctrl Pts',(-16.7099437921364,36.4213836764688,7.87070262534822));
#60871=CARTESIAN_POINT('Ctrl Pts',(-16.7099935682663,36.4225944033524,7.85873193304394));
#60872=CARTESIAN_POINT('Ctrl Pts',(-16.7104029847268,36.4248402340662,7.83635944989056));
#60873=CARTESIAN_POINT('Ctrl Pts',(-16.7107211944244,36.4258771691182,7.82595913439992));
#60874=CARTESIAN_POINT('Ctrl Pts',(-16.7118761546103,36.4285452090779,7.79903913287394));
#60875=CARTESIAN_POINT('Ctrl Pts',(-16.7129078414682,36.4301660652106,7.78252948486991));
#60876=CARTESIAN_POINT('Ctrl Pts',(-16.7213640660259,36.4402060775442,7.6795696849324));
#60877=CARTESIAN_POINT('Ctrl Pts',(-16.7373104893162,36.4482561535016,7.59403559192311));
#60878=CARTESIAN_POINT('Ctrl Pts',(-16.7804213603706,36.4625466864285,7.4478421696924));
#60879=CARTESIAN_POINT('Ctrl Pts',(-16.8038296414844,36.4687257681357,7.38644299176103));
#60880=CARTESIAN_POINT('Ctrl Pts',(-16.8417186577963,36.4772828230211,7.30631026836668));
#60881=CARTESIAN_POINT('Ctrl Pts',(-16.8521281491136,36.4795230145532,7.28576079027428));
#60882=CARTESIAN_POINT('Ctrl Pts',(-16.8716234185066,36.483541935989,7.24973974122657));
#60883=CARTESIAN_POINT('Ctrl Pts',(-16.8804894038865,36.4853124733835,7.23415583583721));
#60884=CARTESIAN_POINT('Ctrl Pts',(-16.9004330995888,36.4891801170895,7.20076542760622));
#60885=CARTESIAN_POINT('Ctrl Pts',(-16.9116277377321,36.4912810919067,7.18303553278944));
#60886=CARTESIAN_POINT('Ctrl Pts',(-16.947280946252,36.4977730892262,7.12954898813671));
#60887=CARTESIAN_POINT('Ctrl Pts',(-16.9731311844644,36.5022141382845,7.09476426104615));
#60888=CARTESIAN_POINT('Ctrl Pts',(-17.0542058498415,36.515432345718,6.99657800580579));
#60889=CARTESIAN_POINT('Ctrl Pts',(-17.1140036382137,36.5243437943068,6.93725753258706));
#60890=CARTESIAN_POINT('Ctrl Pts',(-17.1937105809719,36.5351154723595,6.87250416097278));
#60891=CARTESIAN_POINT('Ctrl Pts',(-17.2084692493629,36.5370679645552,6.86104540608976));
#60892=CARTESIAN_POINT('Ctrl Pts',(-17.2425883293291,36.5414804686067,6.8357417089507));
#60893=CARTESIAN_POINT('Ctrl Pts',(-17.2620972415296,36.5439324632495,6.82210589399287));
#60894=CARTESIAN_POINT('Ctrl Pts',(-17.2918454986805,36.5475556558794,6.80253438398421));
#60895=CARTESIAN_POINT('Ctrl Pts',(-17.3018018906835,36.5487495914627,6.79618119622263));
#60896=CARTESIAN_POINT('Ctrl Pts',(-17.3207509222787,36.5509849778386,6.78445852412909));
#60897=CARTESIAN_POINT('Ctrl Pts',(-17.3297231980031,36.5520279598731,6.77906015743901));
#60898=CARTESIAN_POINT('Ctrl Pts',(-17.3534018553655,36.5547429091335,6.76520933282668));
#60899=CARTESIAN_POINT('Ctrl Pts',(-17.3682129302077,36.5564038802154,6.75693920273413));
#60900=CARTESIAN_POINT('Ctrl Pts',(-17.4329706837229,36.5635278503611,6.72246357545849));
#60901=CARTESIAN_POINT('Ctrl Pts',(-17.4844731961363,36.5688455902111,6.69930101277673));
#60902=CARTESIAN_POINT('Ctrl Pts',(-17.5957245972839,36.5799835431229,6.65793118292992));
#60903=CARTESIAN_POINT('Ctrl Pts',(-17.655611150837,36.5857847355562,6.64054898574749));
#60904=CARTESIAN_POINT('Ctrl Pts',(-17.756016332831,36.5955078325704,6.61925595475851));
#60905=CARTESIAN_POINT('Ctrl Pts',(-17.7958754378734,36.5993659364716,6.61277018895961));
#60906=CARTESIAN_POINT('Ctrl Pts',(-17.8563936059569,36.6052764719903,6.60586236908693));
#60907=CARTESIAN_POINT('Ctrl Pts',(-17.8768676471414,36.6072848966965,6.60402761101839));
#60908=CARTESIAN_POINT('Ctrl Pts',(-17.9153190570589,36.6110800058669,6.60152071172324));
#60909=CARTESIAN_POINT('Ctrl Pts',(-17.9332839154561,36.6128625496769,6.60073215906969));
#60910=CARTESIAN_POINT('Ctrl Pts',(-17.9745272144698,36.616980649529,6.59979853260095));
#60911=CARTESIAN_POINT('Ctrl Pts',(-17.9978041125463,36.619323694003,6.59991159810141));
#60912=CARTESIAN_POINT('Ctrl Pts',(-18.1204344292266,36.6317806000519,6.60387867263611));
#60913=CARTESIAN_POINT('Ctrl Pts',(-18.2190620238107,36.6422311019821,6.61875068662976));
#60914=CARTESIAN_POINT('Ctrl Pts',(-18.3513352873485,36.6566842686294,6.65491345216613));
#60915=CARTESIAN_POINT('Ctrl Pts',(-18.3872914584938,36.660654888521,6.66648877030307));
#60916=CARTESIAN_POINT('Ctrl Pts',(-18.4459025896686,36.6671569775445,6.68828573177479));
#60917=CARTESIAN_POINT('Ctrl Pts',(-18.4688693719524,36.6697124681243,6.69760039175516));
#60918=CARTESIAN_POINT('Ctrl Pts',(-18.5025107421543,36.6734543103898,6.71240512469698));
#60919=CARTESIAN_POINT('Ctrl Pts',(-18.5134022439764,36.6746655023689,6.71738321272107));
#60920=CARTESIAN_POINT('Ctrl Pts',(-18.5336223757166,36.6769116378522,6.72697309818867));
#60921=CARTESIAN_POINT('Ctrl Pts',(-18.5429667962665,36.6779484208179,6.73154638400424));
#60922=CARTESIAN_POINT('Ctrl Pts',(-18.5670098423513,36.6806152407229,6.7436818333025));
#60923=CARTESIAN_POINT('Ctrl Pts',(-18.5816191997031,36.682235048308,6.75141714506561));
#60924=CARTESIAN_POINT('Ctrl Pts',(-18.6584308453281,36.6907720149526,6.7940276699261));
#60925=CARTESIAN_POINT('Ctrl Pts',(-18.7177741761424,36.697444189274,6.83381580102478));
#60926=CARTESIAN_POINT('Ctrl Pts',(-18.815132955538,36.7091245454212,6.91172029292294));
#60927=CARTESIAN_POINT('Ctrl Pts',(-18.8546496865709,36.7141155853043,6.94764737446438));
#60928=CARTESIAN_POINT('Ctrl Pts',(-18.9040380298795,36.7208535324526,6.99858540022494));
#60929=CARTESIAN_POINT('Ctrl Pts',(-18.9160234459164,36.7225319489762,7.01147234238413));
#60930=CARTESIAN_POINT('Ctrl Pts',(-18.9459342833522,36.7268417131067,7.0450040658457));
#60931=CARTESIAN_POINT('Ctrl Pts',(-18.9634667487566,36.7294851769108,7.06598493182892));
#60932=CARTESIAN_POINT('Ctrl Pts',(-18.9916837909836,36.7339599183775,7.10205674509178));
#60933=CARTESIAN_POINT('Ctrl Pts',(-19.0027410145245,36.7357758196871,7.11684552463702));
#60934=CARTESIAN_POINT('Ctrl Pts',(-19.0246154234862,36.7395037696631,7.147472305832));
#60935=CARTESIAN_POINT('Ctrl Pts',(-19.0354039914933,36.7414163357991,7.16332471172732));
#60936=CARTESIAN_POINT('Ctrl Pts',(-19.0630397868396,36.7465229047993,7.20597694503014));
#60937=CARTESIAN_POINT('Ctrl Pts',(-19.0792496286243,36.7497391133778,7.2331706641325));
#60938=CARTESIAN_POINT('Ctrl Pts',(-19.1423151442754,36.7632439823326,7.34856425988581));
#60939=CARTESIAN_POINT('Ctrl Pts',(-19.1796962098748,36.7738260823295,7.44152145546702));
#60940=CARTESIAN_POINT('Ctrl Pts',(-19.2162205907252,36.7884906932312,7.57632370855713));
#60941=CARTESIAN_POINT('Ctrl Pts',(-19.2248254610046,36.7926447903531,7.61525007202022));
#60942=CARTESIAN_POINT('Ctrl Pts',(-19.2339396686859,36.7981420328911,7.6681890779298));
#60943=CARTESIAN_POINT('Ctrl Pts',(-19.2360688944358,36.7995516734352,7.68189541813096));
#60944=CARTESIAN_POINT('Ctrl Pts',(-19.2393799416035,36.801981944899,7.70578328299771));
#60945=CARTESIAN_POINT('Ctrl Pts',(-19.2406637402371,36.8030075876296,7.71594828667188));
#60946=CARTESIAN_POINT('Ctrl Pts',(-19.2433485954974,36.8053642413517,7.73949589881412));
#60947=CARTESIAN_POINT('Ctrl Pts',(-19.2446602789099,36.8066904720259,7.75288710938346));
#60948=CARTESIAN_POINT('Ctrl Pts',(-19.2485592397566,36.8113627458836,7.80047663378449));
#60949=CARTESIAN_POINT('Ctrl Pts',(-19.2499743351078,36.8146540256962,7.83475976305547));
#60950=CARTESIAN_POINT('Ctrl Pts',(-19.2500519035659,36.824636717189,7.93985156011914));
#60951=CARTESIAN_POINT('Ctrl Pts',(-19.2441855365075,36.831207695006,8.01052479332583));
#60952=CARTESIAN_POINT('Ctrl Pts',(-19.22340539874,36.8430010474847,8.13425649880132));
#60953=CARTESIAN_POINT('Ctrl Pts',(-19.2108809647212,36.8481755539421,8.18752030191754));
#60954=CARTESIAN_POINT('Ctrl Pts',(-19.1883646708274,36.855645412525,8.26149563942603));
#60955=CARTESIAN_POINT('Ctrl Pts',(-19.1811838583637,36.8578517613901,8.28300266001613));
#60956=CARTESIAN_POINT('Ctrl Pts',(-19.1673080719994,36.8618349743332,8.32113214818977));
#60957=CARTESIAN_POINT('Ctrl Pts',(-19.1608294475418,36.8636042242597,8.33782732498489));
#60958=CARTESIAN_POINT('Ctrl Pts',(-19.1459026756098,36.8674978471416,8.37400568988059));
#60959=CARTESIAN_POINT('Ctrl Pts',(-19.1373146579057,36.8696265229225,8.39342470950591));
#60960=CARTESIAN_POINT('Ctrl Pts',(-19.1088685512598,36.8763547816825,8.45362008689353));
#60961=CARTESIAN_POINT('Ctrl Pts',(-19.0873133438803,36.8810102182459,8.49354834798456));
#60962=CARTESIAN_POINT('Ctrl Pts',(-19.0221745438445,36.8939970525749,8.60014094800772));
#60963=CARTESIAN_POINT('Ctrl Pts',(-18.9743868951971,36.9024325342042,8.66399384338684));
#60964=CARTESIAN_POINT('Ctrl Pts',(-18.8954487372901,36.9147678068031,8.75107599236373));
#60965=CARTESIAN_POINT('Ctrl Pts',(-18.8686995537025,36.9187243933491,8.77805018368966));
#60966=CARTESIAN_POINT('Ctrl Pts',(-18.8314356661918,36.9239132717192,8.81240053399039));
#60967=CARTESIAN_POINT('Ctrl Pts',(-18.8219634640118,36.9252062244695,8.82087277333503));
#60968=CARTESIAN_POINT('Ctrl Pts',(-18.8116972203454,36.9265787637597,8.82978149360303));
#60969=CARTESIAN_POINT('Ctrl Pts',(-18.8110288055181,36.9266679984251,8.83036030019834));
#60970=CARTESIAN_POINT('Ctrl Pts',(-18.8103597855476,36.9267571849074,8.8309384093402));
#60971=CARTESIAN_POINT('',(-19.2499996068732,36.9878745608382,7.86961352183627));
#60972=CARTESIAN_POINT('Ctrl Pts',(-18.8103598139481,37.0958383925403,8.83093838479897));
#60973=CARTESIAN_POINT('Ctrl Pts',(-18.8319720210683,37.0928666221235,8.81226298524454));
#60974=CARTESIAN_POINT('Ctrl Pts',(-18.8529504390839,37.0898744369893,8.79286172526314));
#60975=CARTESIAN_POINT('Ctrl Pts',(-18.9336583541334,37.0779359743146,8.7130038368293));
#60976=CARTESIAN_POINT('Ctrl Pts',(-18.9879122389735,37.0689120322178,8.64732566049202));
#60977=CARTESIAN_POINT('Ctrl Pts',(-19.0436375522878,37.0586355077117,8.56412167096038));
#60978=CARTESIAN_POINT('Ctrl Pts',(-19.051846569037,37.0570909975101,8.55137709473417));
#60979=CARTESIAN_POINT('Ctrl Pts',(-19.0652601489183,37.0545178365129,8.52970977537145));
#60980=CARTESIAN_POINT('Ctrl Pts',(-19.0705872504396,37.0534820359881,8.52086562805951));
#60981=CARTESIAN_POINT('Ctrl Pts',(-19.0822267884411,37.0511877479046,8.50099717080175));
#60982=CARTESIAN_POINT('Ctrl Pts',(-19.0884827183789,37.0499326935896,8.48994147638588));
#60983=CARTESIAN_POINT('Ctrl Pts',(-19.1087523403626,37.0457844537475,8.45283205091759));
#60984=CARTESIAN_POINT('Ctrl Pts',(-19.1220229756091,37.0429316585472,8.42638027973928));
#60985=CARTESIAN_POINT('Ctrl Pts',(-19.1678390072408,37.0324436691517,8.32649440535921));
#60986=CARTESIAN_POINT('Ctrl Pts',(-19.19432319928,37.0250086207334,8.25048651960703));
#60987=CARTESIAN_POINT('Ctrl Pts',(-19.226133415198,37.0124454450672,8.12077120684708));
#60988=CARTESIAN_POINT('Ctrl Pts',(-19.2355483171846,37.0073998726599,8.06832241853931));
#60989=CARTESIAN_POINT('Ctrl Pts',(-19.2441503099887,37.0001387262449,7.99370466318839));
#60990=CARTESIAN_POINT('Ctrl Pts',(-19.2460939025166,36.9980080974401,7.97190652745627));
#60991=CARTESIAN_POINT('Ctrl Pts',(-19.248375596739,36.9944547171614,7.93578857165217));
#60992=CARTESIAN_POINT('Ctrl Pts',(-19.2490363322088,36.9930423515387,7.92149306712338));
#60993=CARTESIAN_POINT('Ctrl Pts',(-19.2498222302058,36.9903789954949,7.89466709662065));
#60994=CARTESIAN_POINT('Ctrl Pts',(-19.2500037603679,36.9891299547276,7.88213994300183));
#60995=CARTESIAN_POINT('Ctrl Pts',(-19.249999940972,36.9878750685577,7.8696127904914));
#60996=CARTESIAN_POINT('Ctrl Pts',(-19.2499999411772,36.9878751360372,7.86961346411839));
#60997=CARTESIAN_POINT('Ctrl Pts',(-19.2499965846628,36.9867704107569,7.85858532092341));
#60998=CARTESIAN_POINT('Ctrl Pts',(-19.2498495830066,36.9856612471189,7.84755807683458));
#60999=CARTESIAN_POINT('Ctrl Pts',(-19.2491498541977,36.9829796419562,7.82101290712289));
#61000=CARTESIAN_POINT('Ctrl Pts',(-19.2484561139684,36.9814030655816,7.8055009975196));
#61001=CARTESIAN_POINT('Ctrl Pts',(-19.2438792737663,36.9739852733063,7.73298200009193));
#61002=CARTESIAN_POINT('Ctrl Pts',(-19.2364367565112,36.9680436948589,7.67627503906745));
#61003=CARTESIAN_POINT('Ctrl Pts',(-19.2124017841134,36.9552042403979,7.55643159503664));
#61004=CARTESIAN_POINT('Ctrl Pts',(-19.194708435252,36.9483056553954,7.49367172570919));
#61005=CARTESIAN_POINT('Ctrl Pts',(-19.1621005153993,36.9384226686289,7.40479917747777));
#61006=CARTESIAN_POINT('Ctrl Pts',(-19.1509539363258,36.9353619356922,7.37741424108688));
#61007=CARTESIAN_POINT('Ctrl Pts',(-19.1336659123885,36.9310503252874,7.33885389153321));
#61008=CARTESIAN_POINT('Ctrl Pts',(-19.1282974868712,36.9297632856597,7.32734527042008));
#61009=CARTESIAN_POINT('Ctrl Pts',(-19.1182523236134,36.9274483076655,7.3066277850696));
#61010=CARTESIAN_POINT('Ctrl Pts',(-19.1136347658349,36.9264173753027,7.29739294312918));
#61011=CARTESIAN_POINT('Ctrl Pts',(-19.1019581781109,36.9238888750732,7.2747355433121));
#61012=CARTESIAN_POINT('Ctrl Pts',(-19.0947704441636,36.9223990363303,7.26138118585587));
#61013=CARTESIAN_POINT('Ctrl Pts',(-19.045771323413,36.9126448405902,7.17412608831189));
#61014=CARTESIAN_POINT('Ctrl Pts',(-18.9968703820359,36.904750227946,7.10443533384081));
#61015=CARTESIAN_POINT('Ctrl Pts',(-18.9106393858459,36.8923842792171,7.00453951579789));
#61016=CARTESIAN_POINT('Ctrl Pts',(-18.8779592717906,36.8879698200049,6.97067798306193));
#61017=CARTESIAN_POINT('Ctrl Pts',(-18.8182752023877,36.880222443173,6.91533984828336));
#61018=CARTESIAN_POINT('Ctrl Pts',(-18.7921358784013,36.8769218546092,6.89300656591906));
#61019=CARTESIAN_POINT('Ctrl Pts',(-18.7497019600452,36.8716700801893,6.85963177919455));
#61020=CARTESIAN_POINT('Ctrl Pts',(-18.7340003008718,36.8697482624859,6.84786082627717));
#61021=CARTESIAN_POINT('Ctrl Pts',(-18.7031998642669,36.8660133356724,6.82586677827817));
#61022=CARTESIAN_POINT('Ctrl Pts',(-18.6881411277803,36.8642026506752,6.8155957686715));
#61023=CARTESIAN_POINT('Ctrl Pts',(-18.6512752160318,36.8598020116876,6.79159683310471));
#61024=CARTESIAN_POINT('Ctrl Pts',(-18.6292622601431,36.857200518078,6.77820236505293));
#61025=CARTESIAN_POINT('Ctrl Pts',(-18.5411130850893,36.846871712437,6.72817383691675));
#61026=CARTESIAN_POINT('Ctrl Pts',(-18.4721800310458,36.8389725444363,6.69681236288029));
#61027=CARTESIAN_POINT('Ctrl Pts',(-18.3539279884323,36.825765135631,6.6552758874112));
#61028=CARTESIAN_POINT('Ctrl Pts',(-18.306042034625,36.8205074399493,6.64155633658014));
#61029=CARTESIAN_POINT('Ctrl Pts',(-18.2289893129242,36.8122663172098,6.62430489833243));
#61030=CARTESIAN_POINT('Ctrl Pts',(-18.2002911785705,36.8092442958246,6.61891080832345));
#61031=CARTESIAN_POINT('Ctrl Pts',(-18.1589274997324,36.8049758201063,6.61260392848126));
#61032=CARTESIAN_POINT('Ctrl Pts',(-18.1463968982248,36.8036941323454,6.61088441732415));
#61033=CARTESIAN_POINT('Ctrl Pts',(-18.1235837949876,36.8013836367081,6.60810044484617));
#61034=CARTESIAN_POINT('Ctrl Pts',(-18.1133113281566,36.8003519260606,6.60697391078077));
#61035=CARTESIAN_POINT('Ctrl Pts',(-18.0878478801805,36.7978143589703,6.6044956105997));
#61036=CARTESIAN_POINT('Ctrl Pts',(-18.0726441743024,36.7963163784605,6.60329180145362));
#61037=CARTESIAN_POINT('Ctrl Pts',(-17.9734381348069,36.7866304226467,6.59723277575915));
#61038=CARTESIAN_POINT('Ctrl Pts',(-17.889136446353,36.7788042788842,6.6004612007624));
#61039=CARTESIAN_POINT('Ctrl Pts',(-17.75885068255,36.7664798629953,6.61850661117242));
#61040=CARTESIAN_POINT('Ctrl Pts',(-17.7123447526007,36.7620352579744,6.62762211250088));
#61041=CARTESIAN_POINT('Ctrl Pts',(-17.6330090251657,36.7542433367545,6.64783438041513));
#61042=CARTESIAN_POINT('Ctrl Pts',(-17.599923818932,36.7509289237941,6.65771572445393));
#61043=CARTESIAN_POINT('Ctrl Pts',(-17.548704610305,36.7456607506856,6.67531582102457));
#61044=CARTESIAN_POINT('Ctrl Pts',(-17.5302760585709,36.7437366895387,6.68213036401836));
#61045=CARTESIAN_POINT('Ctrl Pts',(-17.4950787970975,36.7400005583082,6.69608207351858));
#61046=CARTESIAN_POINT('Ctrl Pts',(-17.4782909843485,36.7381909608358,6.7031581742054));
#61047=CARTESIAN_POINT('Ctrl Pts',(-17.4382055969771,36.733798626898,6.72107919684498));
#61048=CARTESIAN_POINT('Ctrl Pts',(-17.4150749112923,36.7312044668707,6.73227438049718));
#61049=CARTESIAN_POINT('Ctrl Pts',(-17.32281674823,36.7206001061223,6.78043404352908));
#61050=CARTESIAN_POINT('Ctrl Pts',(-17.2568533111328,36.7124025328118,6.82305312611031));
#61051=CARTESIAN_POINT('Ctrl Pts',(-17.1575295160172,36.6990870299596,6.90111200220858));
#61052=CARTESIAN_POINT('Ctrl Pts',(-17.1215172754823,36.6940212556487,6.93287167003138));
#61053=CARTESIAN_POINT('Ctrl Pts',(-17.0670477381074,36.6860329509701,6.98669048042444));
#61054=CARTESIAN_POINT('Ctrl Pts',(-17.0473905541815,36.6830740099175,7.00747026362907));
#61055=CARTESIAN_POINT('Ctrl Pts',(-17.0201302959756,36.6788760069471,7.03831018765475));
#61056=CARTESIAN_POINT('Ctrl Pts',(-17.0119504435492,36.6776032032986,7.04784557682713));
#61057=CARTESIAN_POINT('Ctrl Pts',(-16.99729089639,36.6753000145867,7.06545668032291));
#61058=CARTESIAN_POINT('Ctrl Pts',(-16.9907667213301,36.6742668789043,7.07349220079844));
#61059=CARTESIAN_POINT('Ctrl Pts',(-16.9747832282539,36.6717136155761,7.09367772513725));
#61060=CARTESIAN_POINT('Ctrl Pts',(-16.9654452237085,36.6702016169602,7.10592165387163));
#61061=CARTESIAN_POINT('Ctrl Pts',(-16.9073302830408,36.6606358596699,7.18506636991105));
#61062=CARTESIAN_POINT('Ctrl Pts',(-16.8649623719828,36.6529302928472,7.2564441831153));
#61063=CARTESIAN_POINT('Ctrl Pts',(-16.8095085789184,36.6406780216269,7.37487495377104));
#61064=CARTESIAN_POINT('Ctrl Pts',(-16.7916530830842,36.6361796085125,7.41941149503553));
#61065=CARTESIAN_POINT('Ctrl Pts',(-16.7652630475786,36.6283083658968,7.49781204108717));
#61066=CARTESIAN_POINT('Ctrl Pts',(-16.7555272425671,36.6249694765985,7.53121433434715));
#61067=CARTESIAN_POINT('Ctrl Pts',(-16.7424460264537,36.6196722749313,7.58408419675772));
#61068=CARTESIAN_POINT('Ctrl Pts',(-16.7381624142675,36.6177442512461,7.60330356405425));
#61069=CARTESIAN_POINT('Ctrl Pts',(-16.7307821959593,36.6140059355288,7.64046538635637));
#61070=CARTESIAN_POINT('Ctrl Pts',(-16.7276212725735,36.6121982010891,7.65839022750838));
#61071=CARTESIAN_POINT('Ctrl Pts',(-16.7209479723695,36.6078201962696,7.70164931981465));
#61072=CARTESIAN_POINT('Ctrl Pts',(-16.717813795412,36.6052387022558,7.72703251360151));
#61073=CARTESIAN_POINT('Ctrl Pts',(-16.7079743168088,36.594405074193,7.83291804248522));
#61074=CARTESIAN_POINT('Ctrl Pts',(-16.7081920118968,36.5859514542183,7.91385810299549));
#61075=CARTESIAN_POINT('Ctrl Pts',(-16.7206417298067,36.5725320596853,8.04053950811451));
#61076=CARTESIAN_POINT('Ctrl Pts',(-16.72773854774,36.5676188879509,8.08658412378216));
#61077=CARTESIAN_POINT('Ctrl Pts',(-16.7431489026897,36.5598331295398,8.15963634933817));
#61078=CARTESIAN_POINT('Ctrl Pts',(-16.74986174569,36.5569258739288,8.18693863095968));
#61079=CARTESIAN_POINT('Ctrl Pts',(-16.760859265411,36.5527857859602,8.22602230908645));
#61080=CARTESIAN_POINT('Ctrl Pts',(-16.7644199847385,36.5515204140374,8.23799631485117));
#61081=CARTESIAN_POINT('Ctrl Pts',(-16.7712579769957,36.549223202445,8.25980786643985));
#61082=CARTESIAN_POINT('Ctrl Pts',(-16.7744797254456,36.5481887401527,8.26966027626384));
#61083=CARTESIAN_POINT('Ctrl Pts',(-16.7828275022103,36.5456216919705,8.29416861512221));
#61084=CARTESIAN_POINT('Ctrl Pts',(-16.7881022984624,36.5440974564466,8.30877209899046));
#61085=CARTESIAN_POINT('Ctrl Pts',(-16.8227655921861,36.5346385604852,8.39949600316182));
#61086=CARTESIAN_POINT('Ctrl Pts',(-16.8591704031109,36.5270402547169,8.47274668098409));
#61087=CARTESIAN_POINT('Ctrl Pts',(-16.9280137570396,36.5148512223854,8.58314461087094));
#61088=CARTESIAN_POINT('Ctrl Pts',(-16.9559988727532,36.5103043101985,8.62277579333392));
#61089=CARTESIAN_POINT('Ctrl Pts',(-17.0079798538298,36.5023617768724,8.68810936894841));
#61090=CARTESIAN_POINT('Ctrl Pts',(-17.0309023673747,36.4990010438652,8.71459416298967));
#61091=CARTESIAN_POINT('Ctrl Pts',(-17.0684031917117,36.4936779423883,8.75446619112779));
#61092=CARTESIAN_POINT('Ctrl Pts',(-17.0822509992118,36.4917463930899,8.7685186750782));
#61093=CARTESIAN_POINT('Ctrl Pts',(-17.1094827118223,36.488006074352,8.79489479950156));
#61094=CARTESIAN_POINT('Ctrl Pts',(-17.1228152650211,36.4861999374116,8.80726462721867));
#61095=CARTESIAN_POINT('Ctrl Pts',(-17.1554451824731,36.4818343297839,8.83625976931501));
#61096=CARTESIAN_POINT('Ctrl Pts',(-17.1749851060158,36.479263808138,8.85259827481995));
#61097=CARTESIAN_POINT('Ctrl Pts',(-17.2597175161819,36.4682844937013,8.91922391837642));
#61098=CARTESIAN_POINT('Ctrl Pts',(-17.3292149065797,36.4596646582141,8.96368681569382));
#61099=CARTESIAN_POINT('Ctrl Pts',(-17.4431878199489,36.4461729472117,9.0218762634079));
#61100=CARTESIAN_POINT('Ctrl Pts',(-17.4849609601666,36.441353546678,9.04043711651855));
#61101=CARTESIAN_POINT('Ctrl Pts',(-17.5536199042152,36.4336929386438,9.066608841916));
#61102=CARTESIAN_POINT('Ctrl Pts',(-17.5799155932922,36.4308181332423,9.07565564446893));
#61103=CARTESIAN_POINT('Ctrl Pts',(-17.6183849679454,36.426714486714,9.08749310323339));
#61104=CARTESIAN_POINT('Ctrl Pts',(-17.6303339956639,36.4254538515313,9.09097854967112));
#61105=CARTESIAN_POINT('Ctrl Pts',(-17.6523359699693,36.4231603816222,9.097046841018));
#61106=CARTESIAN_POINT('Ctrl Pts',(-17.6623717367259,36.4221250062126,9.09968287401341));
#61107=CARTESIAN_POINT('Ctrl Pts',(-17.6875841674417,36.4195488420825,9.10597597755617));
#61108=CARTESIAN_POINT('Ctrl Pts',(-17.7027980894775,36.4180165496863,9.10947683338117));
#61109=CARTESIAN_POINT('Ctrl Pts',(-17.7971363448254,36.4086284813153,9.12936072449991));
#61110=CARTESIAN_POINT('Ctrl Pts',(-17.8776239742299,36.4011013495125,9.13844496382321));
#61111=CARTESIAN_POINT('Ctrl Pts',(-18.0072709902384,36.3889538622936,9.14064598757898));
#61112=CARTESIAN_POINT('Ctrl Pts',(-18.0561033284103,36.3843745128559,9.13865780454879));
#61113=CARTESIAN_POINT('Ctrl Pts',(-18.1396985224861,36.3763844063414,9.13041001537733));
#61114=CARTESIAN_POINT('Ctrl Pts',(-18.1745375629788,36.3730091784098,9.1255045472892));
#61115=CARTESIAN_POINT('Ctrl Pts',(-18.2285537059165,36.3676688940035,9.11559673799094));
#61116=CARTESIAN_POINT('Ctrl Pts',(-18.2478953351182,36.3657350109207,9.1115805093617));
#61117=CARTESIAN_POINT('Ctrl Pts',(-18.2848405354528,36.3619933362698,9.10300553632668));
#61118=CARTESIAN_POINT('Ctrl Pts',(-18.302455407725,36.3601882264317,9.09851651474221));
#61119=CARTESIAN_POINT('Ctrl Pts',(-18.3444389857517,36.3558306483336,9.08685222768028));
#61120=CARTESIAN_POINT('Ctrl Pts',(-18.3686993613928,36.3532672408232,9.079321167836));
#61121=CARTESIAN_POINT('Ctrl Pts',(-18.4529635048526,36.3441925586253,9.05036601957254));
#61122=CARTESIAN_POINT('Ctrl Pts',(-18.5115569067452,36.3375662304837,9.02516353539409));
#61123=CARTESIAN_POINT('Ctrl Pts',(-18.630387694666,36.3234718212738,8.96309175365081));
#61124=CARTESIAN_POINT('Ctrl Pts',(-18.6899572876904,36.3160106517275,8.92537443526061));
#61125=CARTESIAN_POINT('Ctrl Pts',(-18.7650544803624,36.3062300926824,8.86857619830278));
#61126=CARTESIAN_POINT('Ctrl Pts',(-18.7836076873836,36.303780808727,8.85370721682863));
#61127=CARTESIAN_POINT('Ctrl Pts',(-18.8046205043817,36.3009767161073,8.83587543275746));
#61128=CARTESIAN_POINT('Ctrl Pts',(-18.8074956526641,36.3005923650223,8.83341334503232));
#61129=CARTESIAN_POINT('Ctrl Pts',(-18.8103597855904,36.3002088453023,8.83093840930324));
#61130=CARTESIAN_POINT('Origin',(-17.98,42.93984859951,7.87));
#61131=CARTESIAN_POINT('',(-18.8103597331144,35.3371716890844,8.83093845464843));
#61132=CARTESIAN_POINT('',(-18.8103598667433,35.5078191442546,8.83093833917793));
#61133=CARTESIAN_POINT('',(-18.810359785549,42.93984859951,8.83093840933902));
#61134=CARTESIAN_POINT('',(-19.249999602058,36.0238536116147,7.87100537183017));
#61135=CARTESIAN_POINT('Ctrl Pts',(-18.8103597331144,35.3371716890844,8.83093845464842));
#61136=CARTESIAN_POINT('Ctrl Pts',(-18.8029956697976,35.3381039032762,8.83730183996292));
#61137=CARTESIAN_POINT('Ctrl Pts',(-18.7955565796168,35.3390391032005,8.8435821986446));
#61138=CARTESIAN_POINT('Ctrl Pts',(-18.7713328197171,35.3420651495102,8.86356004602031));
#61139=CARTESIAN_POINT('Ctrl Pts',(-18.7542732367335,35.3441671036122,8.87691112805407));
#61140=CARTESIAN_POINT('Ctrl Pts',(-18.7222434781508,35.3480696082538,8.90068274911866));
#61141=CARTESIAN_POINT('Ctrl Pts',(-18.7073739413221,35.3498647060492,8.91122974093067));
#61142=CARTESIAN_POINT('Ctrl Pts',(-18.6760355446539,35.3536185461378,8.93245925463771));
#61143=CARTESIAN_POINT('Ctrl Pts',(-18.6595358478061,35.3555787676672,8.94308716685412));
#61144=CARTESIAN_POINT('Ctrl Pts',(-18.6134743921102,35.3610126113409,8.9712683202844));
#61145=CARTESIAN_POINT('Ctrl Pts',(-18.5834385311958,35.3645141104188,8.98800853788757));
#61146=CARTESIAN_POINT('Ctrl Pts',(-18.5107815449443,35.3728988762175,9.02472227621389));
#61147=CARTESIAN_POINT('Ctrl Pts',(-18.4676577743919,35.3778103169822,9.04358487544163));
#61148=CARTESIAN_POINT('Ctrl Pts',(-18.3440389127559,35.3916826599067,9.0896654591862));
#61149=CARTESIAN_POINT('Ctrl Pts',(-18.2617063306697,35.4006992645921,9.11127041491082));
#61150=CARTESIAN_POINT('Ctrl Pts',(-18.1628460393603,35.4109699236396,9.12686011022758));
#61151=CARTESIAN_POINT('Ctrl Pts',(-18.1478226825295,35.4125153797218,9.12895418272427));
#61152=CARTESIAN_POINT('Ctrl Pts',(-18.1225131219588,35.4150897212408,9.13202085461177));
#61153=CARTESIAN_POINT('Ctrl Pts',(-18.112246771305,35.4161257696643,9.13313794059962));
#61154=CARTESIAN_POINT('Ctrl Pts',(-18.0893249091597,35.418420224268,9.13534950290855));
#61155=CARTESIAN_POINT('Ctrl Pts',(-18.0766646765985,35.4196752017724,9.13637959906825));
#61156=CARTESIAN_POINT('Ctrl Pts',(-18.0344920141824,35.4238215958568,9.13917476513125));
#61157=CARTESIAN_POINT('Ctrl Pts',(-18.0049307616604,35.42667267917,9.14009955023809));
#61158=CARTESIAN_POINT('Ctrl Pts',(-17.9244403009356,35.4343547962777,9.1398055063515));
#61159=CARTESIAN_POINT('Ctrl Pts',(-17.8735728240804,35.4391227063776,9.13655716953619));
#61160=CARTESIAN_POINT('Ctrl Pts',(-17.7496979184924,35.4508161047859,9.12112850845784));
#61161=CARTESIAN_POINT('Ctrl Pts',(-17.6773085518082,35.4577276824075,9.10561213661262));
#61162=CARTESIAN_POINT('Ctrl Pts',(-17.5820503463708,35.4673069610003,9.0763168395228));
#61163=CARTESIAN_POINT('Ctrl Pts',(-17.5576545089222,35.4698038877865,9.06799345243712));
#61164=CARTESIAN_POINT('Ctrl Pts',(-17.5164624164574,35.4741088464869,9.05252497425862));
#61165=CARTESIAN_POINT('Ctrl Pts',(-17.4995353348952,35.4759042050252,9.04574913369533));
#61166=CARTESIAN_POINT('Ctrl Pts',(-17.4647004079522,35.4796585465066,9.03092703092976));
#61167=CARTESIAN_POINT('Ctrl Pts',(-17.4468217270627,35.4816190081759,9.02282525080045));
#61168=CARTESIAN_POINT('Ctrl Pts',(-17.3981610543737,35.4870535516632,8.99940049174118));
#61169=CARTESIAN_POINT('Ctrl Pts',(-17.367805238143,35.4905555138391,8.98323808586637));
#61170=CARTESIAN_POINT('Ctrl Pts',(-17.2975490308109,35.4989417154952,8.94208868379074));
#61171=CARTESIAN_POINT('Ctrl Pts',(-17.2583099030781,35.5038541378178,8.91607641032244));
#61172=CARTESIAN_POINT('Ctrl Pts',(-17.1525867695386,35.5177235100106,8.83720692267497));
#61173=CARTESIAN_POINT('Ctrl Pts',(-17.0898175600356,35.5267359911759,8.77976900616148));
#61174=CARTESIAN_POINT('Ctrl Pts',(-17.0231318561428,35.5370032824597,8.70518470306968));
#61175=CARTESIAN_POINT('Ctrl Pts',(-17.0132230894874,35.5385491513627,8.69369449099255));
#61176=CARTESIAN_POINT('Ctrl Pts',(-16.9969186064675,35.5411240291385,8.67408807170242));
#61177=CARTESIAN_POINT('Ctrl Pts',(-16.9904121689215,35.5421602058701,8.66606696708533));
#61178=CARTESIAN_POINT('Ctrl Pts',(-16.9761238419704,35.5444547445802,8.6480063936147));
#61179=CARTESIAN_POINT('Ctrl Pts',(-16.9683934507036,35.5457096803836,8.63792807407111));
#61180=CARTESIAN_POINT('Ctrl Pts',(-16.9431783347996,35.5498557426464,8.60401268460402));
#61181=CARTESIAN_POINT('Ctrl Pts',(-16.9263729915382,35.5527065446568,8.57967905411403));
#61182=CARTESIAN_POINT('Ctrl Pts',(-16.8829791824265,35.5603875253468,8.51190131502678));
#61183=CARTESIAN_POINT('Ctrl Pts',(-16.858128629912,35.5651546029993,8.46740899265991));
#61184=CARTESIAN_POINT('Ctrl Pts',(-16.8039153275726,35.5768481598991,8.35496188064153));
#61185=CARTESIAN_POINT('Ctrl Pts',(-16.7776933687063,35.5837607076116,8.28571603037241));
#61186=CARTESIAN_POINT('Ctrl Pts',(-16.7506495586745,35.5933409564831,8.18978383798157));
#61187=CARTESIAN_POINT('Ctrl Pts',(-16.7444140584049,35.5958378199638,8.16477342713037));
#61188=CARTESIAN_POINT('Ctrl Pts',(-16.7350739721055,35.6001426482953,8.12177681882658));
#61189=CARTESIAN_POINT('Ctrl Pts',(-16.7315882065427,35.6019379398526,8.10388092929744));
#61190=CARTESIAN_POINT('Ctrl Pts',(-16.7251522593938,35.605692110058,8.06657656947097));
#61191=CARTESIAN_POINT('Ctrl Pts',(-16.7222645201945,35.6076524669644,8.0471625003438));
#61192=CARTESIAN_POINT('Ctrl Pts',(-16.71555945905,35.6130865515487,7.99357955754699));
#61193=CARTESIAN_POINT('Ctrl Pts',(-16.7126782946446,35.616588154165,7.95931358674854));
#61194=CARTESIAN_POINT('Ctrl Pts',(-16.70915422217,35.6249731437658,7.8779816692115));
#61195=CARTESIAN_POINT('Ctrl Pts',(-16.7097307103118,35.629884702584,7.83091533601337));
#61196=CARTESIAN_POINT('Ctrl Pts',(-16.7186646166168,35.6437564561438,7.69929521739378));
#61197=CARTESIAN_POINT('Ctrl Pts',(-16.7328922086987,35.652772319966,7.61537917200997));
#61198=CARTESIAN_POINT('Ctrl Pts',(-16.7594082120656,35.6630424204436,7.51887932323717));
#61199=CARTESIAN_POINT('Ctrl Pts',(-16.7636888660913,35.6645879821681,7.50432617793841));
#61200=CARTESIAN_POINT('Ctrl Pts',(-16.7713206211406,35.6671624774018,7.4799989787617));
#61201=CARTESIAN_POINT('Ctrl Pts',(-16.7745318614785,35.6681985749207,7.47018348886641));
#61202=CARTESIAN_POINT('Ctrl Pts',(-16.7819589917268,35.6704930831391,7.44838519445449));
#61203=CARTESIAN_POINT('Ctrl Pts',(-16.7862354811186,35.671748065688,7.436424604497));
#61204=CARTESIAN_POINT('Ctrl Pts',(-16.8010612671239,35.6758946422749,7.39684301050707));
#61205=CARTESIAN_POINT('Ctrl Pts',(-16.812396474241,35.6787458960329,7.36952370122193));
#61206=CARTESIAN_POINT('Ctrl Pts',(-16.8458244073198,35.6864287648063,7.29629339669386));
#61207=CARTESIAN_POINT('Ctrl Pts',(-16.8697415813981,35.6911972380777,7.25127494863602));
#61208=CARTESIAN_POINT('Ctrl Pts',(-16.9348281978171,35.7028902799841,7.14475794261385));
#61209=CARTESIAN_POINT('Ctrl Pts',(-16.9787807774362,35.7098009532432,7.08519551597135));
#61210=CARTESIAN_POINT('Ctrl Pts',(-17.0447073304089,35.7193791961335,7.01046999822976));
#61211=CARTESIAN_POINT('Ctrl Pts',(-17.0623404177004,35.7218760406653,6.99166926813579));
#61212=CARTESIAN_POINT('Ctrl Pts',(-17.0934023613919,35.7261808299377,6.96050728330895));
#61213=CARTESIAN_POINT('Ctrl Pts',(-17.1065486499346,35.7279761013246,6.94787472257021));
#61214=CARTESIAN_POINT('Ctrl Pts',(-17.1344024598995,35.7317302204077,6.92223948785534));
#61215=CARTESIAN_POINT('Ctrl Pts',(-17.1491485408131,35.7336905462279,6.90928623935327));
#61216=CARTESIAN_POINT('Ctrl Pts',(-17.1905335461279,35.7391245130915,6.87459834739053));
#61217=CARTESIAN_POINT('Ctrl Pts',(-17.2177616433662,35.742626027706,6.85359759321332));
#61218=CARTESIAN_POINT('Ctrl Pts',(-17.2841857517224,35.7510107725956,6.80653627524804));
#61219=CARTESIAN_POINT('Ctrl Pts',(-17.3240432455883,35.7559221728098,6.78149998640374));
#61220=CARTESIAN_POINT('Ctrl Pts',(-17.4394770515388,35.7697938540374,6.71763626619782));
#61221=CARTESIAN_POINT('Ctrl Pts',(-17.517700762349,35.7788098129969,6.68408719351732));
#61222=CARTESIAN_POINT('Ctrl Pts',(-17.613160724782,35.7890799663786,6.65403989419658));
#61223=CARTESIAN_POINT('Ctrl Pts',(-17.6277094375507,35.7906254940437,6.64974532635992));
#61224=CARTESIAN_POINT('Ctrl Pts',(-17.6522876320247,35.7931999554031,6.64296648724193));
#61225=CARTESIAN_POINT('Ctrl Pts',(-17.6622760933924,35.7942360524507,6.64034224483409));
#61226=CARTESIAN_POINT('Ctrl Pts',(-17.6846191907843,35.7965305994794,6.63476257766453));
#61227=CARTESIAN_POINT('Ctrl Pts',(-17.6969880241741,35.7977856207197,6.6318701272081));
#61228=CARTESIAN_POINT('Ctrl Pts',(-17.7382870306109,35.8019324462834,6.62286366361214));
#61229=CARTESIAN_POINT('Ctrl Pts',(-17.7673898961388,35.8047839047061,6.61757371819956));
#61230=CARTESIAN_POINT('Ctrl Pts',(-17.8470543708132,35.8124675966635,6.60595108007677));
#61231=CARTESIAN_POINT('Ctrl Pts',(-17.8978553997377,35.8172366733466,6.60163594318235));
#61232=CARTESIAN_POINT('Ctrl Pts',(-18.0226432308793,35.8289294517286,6.59856762193126));
#61233=CARTESIAN_POINT('Ctrl Pts',(-18.0965122990164,35.8358392745671,6.60320029460235));
#61234=CARTESIAN_POINT('Ctrl Pts',(-18.1950373029715,35.8454166261403,6.61807221981021));
#61235=CARTESIAN_POINT('Ctrl Pts',(-18.2203956408775,35.847913485061,6.62269333116675));
#61236=CARTESIAN_POINT('Ctrl Pts',(-18.2634221350487,35.8522183148961,6.63189488441529));
#61237=CARTESIAN_POINT('Ctrl Pts',(-18.281165026514,35.8540136126846,6.63609079573032));
#61238=CARTESIAN_POINT('Ctrl Pts',(-18.317808554755,35.8577678059678,6.64559378189925));
#61239=CARTESIAN_POINT('Ctrl Pts',(-18.3366885688891,35.8597281798652,6.65096006614578));
#61240=CARTESIAN_POINT('Ctrl Pts',(-18.3882768002448,35.8651623590966,6.66692398557671));
#61241=CARTESIAN_POINT('Ctrl Pts',(-18.4206878282985,35.8686640406985,6.67841470592225));
#61242=CARTESIAN_POINT('Ctrl Pts',(-18.4962523687805,35.8770493167417,6.70870917533902));
#61243=CARTESIAN_POINT('Ctrl Pts',(-18.5389038394608,35.8819610858919,6.72862435320042));
#61244=CARTESIAN_POINT('Ctrl Pts',(-18.6551505210169,35.8958321242142,6.79098314601182));
#61245=CARTESIAN_POINT('Ctrl Pts',(-18.7257473666319,35.9048470247851,6.83851127054129));
#61246=CARTESIAN_POINT('Ctrl Pts',(-18.8027503731567,35.9151163154596,6.90241956968076));
#61247=CARTESIAN_POINT('Ctrl Pts',(-18.8142486176276,35.9166619557591,6.91231561261081));
#61248=CARTESIAN_POINT('Ctrl Pts',(-18.8332728057225,35.9192365503464,6.92929167066815));
#61249=CARTESIAN_POINT('Ctrl Pts',(-18.8408941347874,35.9202726695755,6.93626129529115));
#61250=CARTESIAN_POINT('Ctrl Pts',(-18.8576976349681,35.9225671958382,6.95200862618872));
#61251=CARTESIAN_POINT('Ctrl Pts',(-18.8668346050775,35.9238221751267,6.96083239585717));
#61252=CARTESIAN_POINT('Ctrl Pts',(-18.8967938895666,35.9279686598064,6.99064627004785));
#61253=CARTESIAN_POINT('Ctrl Pts',(-18.9170175954944,35.9308198283914,7.01222818276626));
#61254=CARTESIAN_POINT('Ctrl Pts',(-18.9699733069114,35.9385023302184,7.07285127875576));
#61255=CARTESIAN_POINT('Ctrl Pts',(-19.0011406911917,35.9432705304673,7.1131870611411));
#61256=CARTESIAN_POINT('Ctrl Pts',(-19.0713902291101,35.9549636675338,7.21637312914291));
#61257=CARTESIAN_POINT('Ctrl Pts',(-19.1075608186877,35.9618747021449,7.28096248809144));
#61258=CARTESIAN_POINT('Ctrl Pts',(-19.1484957617063,35.971453340069,7.37182145462762));
#61259=CARTESIAN_POINT('Ctrl Pts',(-19.1583635555908,35.9739501980182,7.39563376928951));
#61260=CARTESIAN_POINT('Ctrl Pts',(-19.1739632914659,35.9782550179995,7.43677483999959));
#61261=CARTESIAN_POINT('Ctrl Pts',(-19.1800588512636,35.9800503067591,7.45395787733186));
#61262=CARTESIAN_POINT('Ctrl Pts',(-19.1919441142103,35.9838044719827,7.48989914072911));
#61263=CARTESIAN_POINT('Ctrl Pts',(-19.1976728906673,35.9857648267163,7.50867214411029));
#61264=CARTESIAN_POINT('Ctrl Pts',(-19.2084990379349,35.9898052828975,7.54733683714307));
#61265=CARTESIAN_POINT('Ctrl Pts',(-19.2135535197071,35.9918861425367,7.56723442577343));
#61266=CARTESIAN_POINT('Ctrl Pts',(-19.2393872838271,36.0037323841713,7.680354649335));
#61267=CARTESIAN_POINT('Ctrl Pts',(-19.2500751712369,36.0137975274248,7.77554533972636));
#61268=CARTESIAN_POINT('Ctrl Pts',(-19.249999602058,36.0238536116147,7.87100537183017));
#61269=CARTESIAN_POINT('Ctrl Pts',(-19.2499996010994,36.0238537391044,7.87100658206029));
#61270=CARTESIAN_POINT('Ctrl Pts',(-19.2499608072807,36.0290098734858,7.91995255092519));
#61271=CARTESIAN_POINT('Ctrl Pts',(-19.2470924523388,36.0341450524481,7.96886265353495));
#61272=CARTESIAN_POINT('Ctrl Pts',(-19.2400018586021,36.0404184819091,8.02950420490857));
#61273=CARTESIAN_POINT('Ctrl Pts',(-19.2384256559987,36.041654431005,8.04149688136434));
#61274=CARTESIAN_POINT('Ctrl Pts',(-19.2353003526182,36.0438503076806,8.06290412787031));
#61275=CARTESIAN_POINT('Ctrl Pts',(-19.2338160821336,36.044813277187,8.07232704043072));
#61276=CARTESIAN_POINT('Ctrl Pts',(-19.2304817502714,36.0468198382188,8.09204686891696));
#61277=CARTESIAN_POINT('Ctrl Pts',(-19.2286105127149,36.0478618398658,8.10233859804876));
#61278=CARTESIAN_POINT('Ctrl Pts',(-19.2233848830273,36.0505693722261,8.12918996442249));
#61279=CARTESIAN_POINT('Ctrl Pts',(-19.2198267922409,36.052224025085,8.14570823927836));
#61280=CARTESIAN_POINT('Ctrl Pts',(-19.2016843495377,36.059883368015,8.22245925370173));
#61281=CARTESIAN_POINT('Ctrl Pts',(-19.1830315643831,36.0657090962037,8.28165247600621));
#61282=CARTESIAN_POINT('Ctrl Pts',(-19.1363887348613,36.0775431016332,8.39895421121359));
#61283=CARTESIAN_POINT('Ctrl Pts',(-19.1081565416069,36.0835343947072,8.45676183324533));
#61284=CARTESIAN_POINT('Ctrl Pts',(-19.057635922448,36.0930337232955,8.54295863544918));
#61285=CARTESIAN_POINT('Ctrl Pts',(-19.0383114149812,36.0964556001011,8.57295728453371));
#61286=CARTESIAN_POINT('Ctrl Pts',(-19.0063172954067,36.1018514283087,8.61830895193234));
#61287=CARTESIAN_POINT('Ctrl Pts',(-18.9945051729102,36.1037930576693,8.63424644238579));
#61288=CARTESIAN_POINT('Ctrl Pts',(-18.9711775239964,36.1075399483639,8.66422708704646));
#61289=CARTESIAN_POINT('Ctrl Pts',(-18.9597244168299,36.1093423737212,8.67831276719533));
#61290=CARTESIAN_POINT('Ctrl Pts',(-18.9316618286343,36.1136766319416,8.71135290560143));
#61291=CARTESIAN_POINT('Ctrl Pts',(-18.9147831451959,36.1162190718351,8.73006696652725));
#61292=CARTESIAN_POINT('Ctrl Pts',(-18.8696590608875,36.1228626166517,8.7771997277421));
#61293=CARTESIAN_POINT('Ctrl Pts',(-18.8406242357173,36.1269929008927,8.8047865100712));
#61294=CARTESIAN_POINT('Ctrl Pts',(-18.8103594475449,36.1311618021068,8.83093870141285));
#61295=CARTESIAN_POINT('Ctrl Pts',(-18.8103597855904,36.3002088453023,8.83093840930324));
#61296=CARTESIAN_POINT('Ctrl Pts',(-18.8164268746474,36.2993964359777,8.82569575616366));
#61297=CARTESIAN_POINT('Ctrl Pts',(-18.822444535654,36.298587756557,8.82039545161663));
#61298=CARTESIAN_POINT('Ctrl Pts',(-18.83620292553,36.2967328724837,8.80804380032832));
#61299=CARTESIAN_POINT('Ctrl Pts',(-18.8439068972887,36.295690000473,8.80095354923604));
#61300=CARTESIAN_POINT('Ctrl Pts',(-18.8638623439902,36.2929748083373,8.78212670967425));
#61301=CARTESIAN_POINT('Ctrl Pts',(-18.8759681958865,36.2913134927087,8.77023823162753));
#61302=CARTESIAN_POINT('Ctrl Pts',(-18.929109337216,36.283934304214,8.71591690495378));
#61303=CARTESIAN_POINT('Ctrl Pts',(-18.9674006316583,36.2783769485685,8.67089086844673));
#61304=CARTESIAN_POINT('Ctrl Pts',(-19.0383431120129,36.2671604116637,8.57461064378817));
#61305=CARTESIAN_POINT('Ctrl Pts',(-19.0707272129343,36.2615158872613,8.52336048350766));
#61306=CARTESIAN_POINT('Ctrl Pts',(-19.1181189855404,36.2520090259425,8.4349483288327));
#61307=CARTESIAN_POINT('Ctrl Pts',(-19.1352478205279,36.2482064136738,8.39903992315327));
#61308=CARTESIAN_POINT('Ctrl Pts',(-19.1585969639633,36.2423613587935,8.34352717998947));
#61309=CARTESIAN_POINT('Ctrl Pts',(-19.1660735342583,36.2403613467927,8.32447579442566));
#61310=CARTESIAN_POINT('Ctrl Pts',(-19.1792522966141,36.2365734494003,8.288351095454));
#61311=CARTESIAN_POINT('Ctrl Pts',(-19.1850581854163,36.2347895534342,8.27132081305205));
#61312=CARTESIAN_POINT('Ctrl Pts',(-19.1975830718585,36.2306556863584,8.23185595201631));
#61313=CARTESIAN_POINT('Ctrl Pts',(-19.2040469118179,36.2282980054184,8.20934825354585));
#61314=CARTESIAN_POINT('Ctrl Pts',(-19.2366090703395,36.215036324851,8.08288583400888));
#61315=CARTESIAN_POINT('Ctrl Pts',(-19.2500815441936,36.203733902395,7.97615196007877));
#61316=CARTESIAN_POINT('Ctrl Pts',(-19.2499635734042,36.1874934391101,7.82187826498927));
#61317=CARTESIAN_POINT('Ctrl Pts',(-19.2473017254069,36.1825553388251,7.77475981211089));
#61318=CARTESIAN_POINT('Ctrl Pts',(-19.2403638736094,36.1761966483956,7.71314614950596));
#61319=CARTESIAN_POINT('Ctrl Pts',(-19.2384448668738,36.1746853386944,7.69842840176448));
#61320=CARTESIAN_POINT('Ctrl Pts',(-19.23475855701,36.172148419923,7.67356447320316));
#61321=CARTESIAN_POINT('Ctrl Pts',(-19.2331251927494,36.1711161823326,7.6634007742838));
#61322=CARTESIAN_POINT('Ctrl Pts',(-19.2291658921259,36.1688057287158,7.6405417357144));
#61323=CARTESIAN_POINT('Ctrl Pts',(-19.2267697600024,36.1675313161604,7.62786008781158));
#61324=CARTESIAN_POINT('Ctrl Pts',(-19.2179438796925,36.1632180532542,7.58476084343394));
#61325=CARTESIAN_POINT('Ctrl Pts',(-19.2105902430604,36.1602241808432,7.55454067269639));
#61326=CARTESIAN_POINT('Ctrl Pts',(-19.186925812673,36.1519315152939,7.47080433941823));
#61327=CARTESIAN_POINT('Ctrl Pts',(-19.1681791134797,36.1467087713969,7.41805032324011));
#61328=CARTESIAN_POINT('Ctrl Pts',(-19.1193460620872,36.1351649166607,7.30491689039958));
#61329=CARTESIAN_POINT('Ctrl Pts',(-19.0878131164039,36.1288521283137,7.24535881711062));
#61330=CARTESIAN_POINT('Ctrl Pts',(-19.0380002451793,36.1199258353162,7.16701436413346));
#61331=CARTESIAN_POINT('Ctrl Pts',(-19.0236391327178,36.1174488551599,7.14586570978843));
#61332=CARTESIAN_POINT('Ctrl Pts',(-18.9979776289267,36.1131671268238,7.11042594435977));
#61333=CARTESIAN_POINT('Ctrl Pts',(-18.9869894115542,36.1113746988024,7.09591768001499));
#61334=CARTESIAN_POINT('Ctrl Pts',(-18.9634689139916,36.107616390796,7.06621100168647));
#61335=CARTESIAN_POINT('Ctrl Pts',(-18.9508872715427,36.1056488911378,7.05105821188776));
#61336=CARTESIAN_POINT('Ctrl Pts',(-18.9151062214748,36.1001633652424,7.00994883224409));
#61337=CARTESIAN_POINT('Ctrl Pts',(-18.891186297287,36.0966165171022,6.98464662372967));
#61338=CARTESIAN_POINT('Ctrl Pts',(-18.8318728322982,36.0880833013343,6.92685754241105));
#61339=CARTESIAN_POINT('Ctrl Pts',(-18.7956172279711,36.0830671822959,6.89533467703813));
#61340=CARTESIAN_POINT('Ctrl Pts',(-18.69231568615,36.069322501654,6.81532489133015));
#61341=CARTESIAN_POINT('Ctrl Pts',(-18.6221714168987,36.0605488861438,6.77120448919014));
#61342=CARTESIAN_POINT('Ctrl Pts',(-18.5344484750624,36.0504779286096,6.72731702848951));
#61343=CARTESIAN_POINT('Ctrl Pts',(-18.5205409689291,36.0489068764641,6.72067279454311));
#61344=CARTESIAN_POINT('Ctrl Pts',(-18.4970946746568,36.0463043885496,6.70999126977089));
#61345=CARTESIAN_POINT('Ctrl Pts',(-18.4876218807714,36.0452653873125,6.70581478180152));
#61346=CARTESIAN_POINT('Ctrl Pts',(-18.4665503301956,36.042982278355,6.6968306336465));
#61347=CARTESIAN_POINT('Ctrl Pts',(-18.4549295716298,36.041741329982,6.69207829850181));
#61348=CARTESIAN_POINT('Ctrl Pts',(-18.4166700514419,36.0377083413326,6.67709030895712));
#61349=CARTESIAN_POINT('Ctrl Pts',(-18.3897540981057,36.0349536417919,6.66757900410528));
#61350=CARTESIAN_POINT('Ctrl Pts',(-18.3169525702975,36.027659387109,6.64458241206052));
#61351=CARTESIAN_POINT('Ctrl Pts',(-18.2705870755116,36.0231753831898,6.63276709074159));
#61352=CARTESIAN_POINT('Ctrl Pts',(-18.1464765668155,36.0113264641109,6.60850453180685));
#61353=CARTESIAN_POINT('Ctrl Pts',(-18.0680663209311,36.0039861333247,6.60061933193078));
#61354=CARTESIAN_POINT('Ctrl Pts',(-17.9637535984537,35.9939582351488,6.59984421703849));
#61355=CARTESIAN_POINT('Ctrl Pts',(-17.9380728503237,35.9914696700677,6.60043253173901));
#61356=CARTESIAN_POINT('Ctrl Pts',(-17.8942394906364,35.9871746699727,6.60276799484169));
#61357=CARTESIAN_POINT('Ctrl Pts',(-17.8760735574333,35.9853807628617,6.60412835236113));
#61358=CARTESIAN_POINT('Ctrl Pts',(-17.8383847868328,35.9816254872065,6.60776734598386));
#61359=CARTESIAN_POINT('Ctrl Pts',(-17.8188732099629,35.9796625848725,6.61010945415574));
#61360=CARTESIAN_POINT('Ctrl Pts',(-17.7652353021889,35.9742091622604,6.61781423415897));
#61361=CARTESIAN_POINT('Ctrl Pts',(-17.7312644369128,35.97069040714,6.62411753660487));
#61362=CARTESIAN_POINT('Ctrl Pts',(-17.6513758523523,35.962249225731,6.64233813743481));
#61363=CARTESIAN_POINT('Ctrl Pts',(-17.6057873463636,35.957298031662,6.65545838547015));
#61364=CARTESIAN_POINT('Ctrl Pts',(-17.4817090961854,35.9434753734014,6.69881735860065));
#61365=CARTESIAN_POINT('Ctrl Pts',(-17.4053158317851,35.9345523988724,6.7343489850474));
#61366=CARTESIAN_POINT('Ctrl Pts',(-17.3198558260985,35.9243585501369,6.78494582764722));
#61367=CARTESIAN_POINT('Ctrl Pts',(-17.3068642069141,35.9228031947767,6.79295721126881));
#61368=CARTESIAN_POINT('Ctrl Pts',(-17.285321667145,35.9202180860495,6.80678373750636));
#61369=CARTESIAN_POINT('Ctrl Pts',(-17.2766922227958,35.9191810129989,6.81247221497463));
#61370=CARTESIAN_POINT('Ctrl Pts',(-17.2576649619155,35.9168914696714,6.82535085005714));
#61371=CARTESIAN_POINT('Ctrl Pts',(-17.2473033964975,35.9156423184911,6.83259193723455));
#61372=CARTESIAN_POINT('Ctrl Pts',(-17.2134185257701,35.9115427840077,6.85703311962151));
#61373=CARTESIAN_POINT('Ctrl Pts',(-17.1903767653524,35.9087314870191,6.8748896369118));
#61374=CARTESIAN_POINT('Ctrl Pts',(-17.1298202301443,35.9012114130481,6.9252482458142));
#61375=CARTESIAN_POINT('Ctrl Pts',(-17.0935616311797,35.8965625404014,6.95918201285587));
#61376=CARTESIAN_POINT('Ctrl Pts',(-17.0071557819574,35.8848118837662,7.05010884769546));
#61377=CARTESIAN_POINT('Ctrl Pts',(-16.9599647513936,35.8777277220064,7.10962294529209));
#61378=CARTESIAN_POINT('Ctrl Pts',(-16.9042250413927,35.8679657750806,7.19452090244234));
#61379=CARTESIAN_POINT('Ctrl Pts',(-16.8907449286172,35.865469717203,7.21648110642693));
#61380=CARTESIAN_POINT('Ctrl Pts',(-16.8688844325569,35.861166123642,7.25465097661411));
#61381=CARTESIAN_POINT('Ctrl Pts',(-16.8601681089293,35.8593712506906,7.27065980086283));
#61382=CARTESIAN_POINT('Ctrl Pts',(-16.8427895410929,35.8556178684879,7.30428149450014));
#61383=CARTESIAN_POINT('Ctrl Pts',(-16.8341851579288,35.853657880225,7.32191853526637));
#61384=CARTESIAN_POINT('Ctrl Pts',(-16.8116424244363,35.8482247272423,7.370978970431));
#61385=CARTESIAN_POINT('Ctrl Pts',(-16.7985671545369,35.8447236954916,7.40277705829569));
#61386=CARTESIAN_POINT('Ctrl Pts',(-16.7706921627854,35.8363402297381,7.47924890907114));
#61387=CARTESIAN_POINT('Ctrl Pts',(-16.7570544639594,35.8314296349592,7.52429050096402));
#61388=CARTESIAN_POINT('Ctrl Pts',(-16.725887094001,35.8175569260029,7.65248894201771));
#61389=CARTESIAN_POINT('Ctrl Pts',(-16.7141513430886,35.8085390473888,7.73680857212909));
#61390=CARTESIAN_POINT('Ctrl Pts',(-16.7103427577419,35.7982674782518,7.83682750871485));
#61391=CARTESIAN_POINT('Ctrl Pts',(-16.7100371452135,35.7967223108948,7.85199026394879));
#61392=CARTESIAN_POINT('Ctrl Pts',(-16.7099800648641,35.7941484287091,7.87748038396702));
#61393=CARTESIAN_POINT('Ctrl Pts',(-16.7100828340201,35.7931125538241,7.88780509562494));
#61394=CARTESIAN_POINT('Ctrl Pts',(-16.7105927749681,35.7908185660214,7.91082305528718));
#61395=CARTESIAN_POINT('Ctrl Pts',(-16.7110643870074,35.7895638792921,7.92351339288237));
#61396=CARTESIAN_POINT('Ctrl Pts',(-16.7132667046723,35.7854186868468,7.96570875292727));
#61397=CARTESIAN_POINT('Ctrl Pts',(-16.7158370151808,35.782568489306,7.99516309626957));
#61398=CARTESIAN_POINT('Ctrl Pts',(-16.7256250195747,35.7748896784937,8.07502115993411));
#61399=CARTESIAN_POINT('Ctrl Pts',(-16.7348483212888,35.7701241291193,8.12512441530049));
#61400=CARTESIAN_POINT('Ctrl Pts',(-16.764785644149,35.7584295870054,8.24632604656152));
#61401=CARTESIAN_POINT('Ctrl Pts',(-16.7887489485983,35.7515145704087,8.31641463520439));
#61402=CARTESIAN_POINT('Ctrl Pts',(-16.8290996474445,35.7419319202978,8.40758019795731));
#61403=CARTESIAN_POINT('Ctrl Pts',(-16.8402435992797,35.7394352841977,8.43082013124674));
#61404=CARTESIAN_POINT('Ctrl Pts',(-16.8604634632196,35.7351310255058,8.46989182320388));
#61405=CARTESIAN_POINT('Ctrl Pts',(-16.8691881569258,35.7333360760363,8.48589708537482));
#61406=CARTESIAN_POINT('Ctrl Pts',(-16.8880132002418,35.7295828326834,8.5187293755671));
#61407=CARTESIAN_POINT('Ctrl Pts',(-16.8981651185921,35.7276230639687,8.53552096282337));
#61408=CARTESIAN_POINT('Ctrl Pts',(-16.927154037602,35.7221914437242,8.58105267893841));
#61409=CARTESIAN_POINT('Ctrl Pts',(-16.9467730912697,35.7186917529854,8.60927134511065));
#61410=CARTESIAN_POINT('Ctrl Pts',(-16.9958829819392,35.7103126427103,8.67412864765872));
#61411=CARTESIAN_POINT('Ctrl Pts',(-17.0263113784383,35.7054051079809,8.70999177571336));
#61412=CARTESIAN_POINT('Ctrl Pts',(-17.1171405413213,35.6915286050961,8.80573234895545));
#61413=CARTESIAN_POINT('Ctrl Pts',(-17.1816721347875,35.6825035459852,8.86136100023632));
#61414=CARTESIAN_POINT('Ctrl Pts',(-17.2636950793387,35.6722261089264,8.91882646908317));
#61415=CARTESIAN_POINT('Ctrl Pts',(-17.2762634913481,35.6706817201561,8.92730066870284));
#61416=CARTESIAN_POINT('Ctrl Pts',(-17.2976432801477,35.6681086889838,8.94116566584799));
#61417=CARTESIAN_POINT('Ctrl Pts',(-17.3063735263717,35.6670728988364,8.94667729097374));
#61418=CARTESIAN_POINT('Ctrl Pts',(-17.3259938012349,35.6647785381793,8.95873193959987));
#61419=CARTESIAN_POINT('Ctrl Pts',(-17.3369164084793,35.6635234023712,8.9652191045742));
#61420=CARTESIAN_POINT('Ctrl Pts',(-17.3735977247526,35.6593745232478,8.98626684396428));
#61421=CARTESIAN_POINT('Ctrl Pts',(-17.3997701741929,35.6565211869616,9.00009255500328));
#61422=CARTESIAN_POINT('Ctrl Pts',(-17.472304236726,35.6488294347508,9.03522356350001));
#61423=CARTESIAN_POINT('Ctrl Pts',(-17.5195049131126,35.6440543430188,9.054671313635));
#61424=CARTESIAN_POINT('Ctrl Pts',(-17.6375461686839,35.632364055603,9.09518181083352));
#61425=CARTESIAN_POINT('Ctrl Pts',(-17.7092870250348,35.6254625802331,9.11300340188724));
#61426=CARTESIAN_POINT('Ctrl Pts',(-17.8076171125583,35.6158944157863,9.12851029873159));
#61427=CARTESIAN_POINT('Ctrl Pts',(-17.8331853995243,35.6133978857198,9.13174850380631));
#61428=CARTESIAN_POINT('Ctrl Pts',(-17.876977140758,35.609093740034,9.13594571153269));
#61429=CARTESIAN_POINT('Ctrl Pts',(-17.8951559364666,35.6072987954106,9.13729383045634));
#61430=CARTESIAN_POINT('Ctrl Pts',(-17.932950590581,35.6035454968264,9.13927985469515));
#61431=CARTESIAN_POINT('Ctrl Pts',(-17.9525646351676,35.6015856671171,9.13985518317132));
#61432=CARTESIAN_POINT('Ctrl Pts',(-18.0065440733122,35.596153669798,9.14018744941228));
#61433=CARTESIAN_POINT('Ctrl Pts',(-18.0408953839286,35.592653656559,9.13900430669479));
#61434=CARTESIAN_POINT('Ctrl Pts',(-18.1220291241248,35.584273512291,9.1329083680634));
#61435=CARTESIAN_POINT('Ctrl Pts',(-18.168668276846,35.579365255559,9.12678680855988));
#61436=CARTESIAN_POINT('Ctrl Pts',(-18.2983541043188,35.5654896172384,9.10238368134162));
#61437=CARTESIAN_POINT('Ctrl Pts',(-18.3800714473173,35.5564662210263,9.07833118362491));
#61438=CARTESIAN_POINT('Ctrl Pts',(-18.4728195645737,35.5461901391829,9.04058046776377));
#61439=CARTESIAN_POINT('Ctrl Pts',(-18.4867565930735,35.5446455670261,9.0346147801621));
#61440=CARTESIAN_POINT('Ctrl Pts',(-18.5100011279264,35.5420723404975,9.02416869811904));
#61441=CARTESIAN_POINT('Ctrl Pts',(-18.5193661869721,35.5410365353539,9.01982204437786));
#61442=CARTESIAN_POINT('Ctrl Pts',(-18.5401327217626,35.5387422913517,9.00987395976245));
#61443=CARTESIAN_POINT('Ctrl Pts',(-18.5515049490686,35.5374872849198,9.00421490542589));
#61444=CARTESIAN_POINT('Ctrl Pts',(-18.5890711574812,35.5333393875388,8.98481262596709));
#61445=CARTESIAN_POINT('Ctrl Pts',(-18.6148723179907,35.5304868784653,8.97032379447077));
#61446=CARTESIAN_POINT('Ctrl Pts',(-18.6836917195907,35.5227985276337,8.92844985984082));
#61447=CARTESIAN_POINT('Ctrl Pts',(-18.7256057145195,35.5180259431793,8.89935473245868));
#61448=CARTESIAN_POINT('Ctrl Pts',(-18.7808448467063,35.5114400758792,8.85586055815525));
#61449=CARTESIAN_POINT('Ctrl Pts',(-18.795748290919,35.5096311151527,8.84356440024732));
#61450=CARTESIAN_POINT('Ctrl Pts',(-18.8103598667433,35.5078191442546,8.83093833917793));
#61451=CARTESIAN_POINT('Origin',(-17.98,42.93984859951,7.87));
#61452=CARTESIAN_POINT('',(-18.8103597424409,34.5453270911211,8.83093844658932));
#61453=CARTESIAN_POINT('',(-18.810359785549,34.7139132859163,8.83093840933901));
#61454=CARTESIAN_POINT('',(-18.810359785549,42.93984859951,8.83093840933902));
#61455=CARTESIAN_POINT('Ctrl Pts',(-18.8103597424409,34.5453270911211,8.83093844658933));
#61456=CARTESIAN_POINT('Ctrl Pts',(-18.7582784971811,34.5519273472422,8.87594254602299));
#61457=CARTESIAN_POINT('Ctrl Pts',(-18.7025978955493,34.5583389621438,8.91666128726311));
#61458=CARTESIAN_POINT('Ctrl Pts',(-18.6044300911063,34.5691275162025,8.9768541522636));
#61459=CARTESIAN_POINT('Ctrl Pts',(-18.563713770624,34.573469711912,8.99885637855351));
#61460=CARTESIAN_POINT('Ctrl Pts',(-18.4911605351903,34.5811062412763,9.03308617899149));
#61461=CARTESIAN_POINT('Ctrl Pts',(-18.4598640189898,34.5843694085406,9.04634375194037));
#61462=CARTESIAN_POINT('Ctrl Pts',(-18.4098461168205,34.5895694162822,9.06520371504832));
#61463=CARTESIAN_POINT('Ctrl Pts',(-18.3914611272229,34.5914775361062,9.07165687377777));
#61464=CARTESIAN_POINT('Ctrl Pts',(-18.355699923058,34.5951885374251,9.08329225970602));
#61465=CARTESIAN_POINT('Ctrl Pts',(-18.3383467571686,34.5969890583393,9.08853028430628));
#61466=CARTESIAN_POINT('Ctrl Pts',(-18.2961909528124,34.6013667488425,9.10027664080755));
#61467=CARTESIAN_POINT('Ctrl Pts',(-18.2712930498596,34.6039554378379,9.1064082839928));
#61468=CARTESIAN_POINT('Ctrl Pts',(-18.1685704784758,34.6146612288439,9.12843125013388));
#61469=CARTESIAN_POINT('Ctrl Pts',(-18.0895377763885,34.6229731015943,9.13775564639213));
#61470=CARTESIAN_POINT('Ctrl Pts',(-17.9624772255803,34.6363774925223,9.14077487216361));
#61471=CARTESIAN_POINT('Ctrl Pts',(-17.9147568068693,34.6414168289293,9.13922007761438));
#61472=CARTESIAN_POINT('Ctrl Pts',(-17.8388559332839,34.6493687218697,9.13245400583687));
#61473=CARTESIAN_POINT('Ctrl Pts',(-17.8105666896419,34.6523178104545,9.12896961935409));
#61474=CARTESIAN_POINT('Ctrl Pts',(-17.770066662084,34.6564999099261,9.12259102232216));
#61475=CARTESIAN_POINT('Ctrl Pts',(-17.7577463207581,34.6577667321182,9.1204637635419));
#61476=CARTESIAN_POINT('Ctrl Pts',(-17.7353154079887,34.660061063118,9.11624875756492));
#61477=CARTESIAN_POINT('Ctrl Pts',(-17.7251963607594,34.6610912911448,9.11421928858266));
#61478=CARTESIAN_POINT('Ctrl Pts',(-17.7001212278364,34.6636341012551,9.10887146293338));
#61479=CARTESIAN_POINT('Ctrl Pts',(-17.6851982998348,34.6651386474236,9.10540546612928));
#61480=CARTESIAN_POINT('Ctrl Pts',(-17.5892586478978,34.674777785137,9.081284861242));
#61481=CARTESIAN_POINT('Ctrl Pts',(-17.5103717906956,34.6825561351185,9.05293894812749));
#61482=CARTESIAN_POINT('Ctrl Pts',(-17.3917946895006,34.6948573568254,8.99658118356185));
#61483=CARTESIAN_POINT('Ctrl Pts',(-17.3499455762797,34.6993288234307,8.97372165576177));
#61484=CARTESIAN_POINT('Ctrl Pts',(-17.2800366682171,34.7071624624334,8.93026103435852));
#61485=CARTESIAN_POINT('Ctrl Pts',(-17.2513563524533,34.7104912566938,8.91075937964797));
#61486=CARTESIAN_POINT('Ctrl Pts',(-17.2076887698448,34.7157791761104,8.87837663626398));
#61487=CARTESIAN_POINT('Ctrl Pts',(-17.1921415677685,34.7177083223952,8.86627659903483));
#61488=CARTESIAN_POINT('Ctrl Pts',(-17.1627424760259,34.7214531395402,8.84227740064588));
#61489=CARTESIAN_POINT('Ctrl Pts',(-17.1488533809411,34.723266310387,8.83043136831113));
#61490=CARTESIAN_POINT('Ctrl Pts',(-17.1160070178157,34.7276665580663,8.80117054063338));
#61491=CARTESIAN_POINT('Ctrl Pts',(-17.0973155360445,34.7302650629381,8.78347158662414));
#61492=CARTESIAN_POINT('Ctrl Pts',(-17.0254233369961,34.7406567513275,8.71112926161933));
#61493=CARTESIAN_POINT('Ctrl Pts',(-16.9766622122373,34.7486249179249,8.65231948592174));
#61494=CARTESIAN_POINT('Ctrl Pts',(-16.9056933617137,34.7618219789575,8.54909514508476));
#61495=CARTESIAN_POINT('Ctrl Pts',(-16.8802727595058,34.7670001873093,8.50710705356034));
#61496=CARTESIAN_POINT('Ctrl Pts',(-16.8438101129522,34.775136787827,8.43816409611634));
#61497=CARTESIAN_POINT('Ctrl Pts',(-16.8311541505679,34.7781326271269,8.41211761480097));
#61498=CARTESIAN_POINT('Ctrl Pts',(-16.8142684713525,34.7823741707503,8.37411270525194));
#61499=CARTESIAN_POINT('Ctrl Pts',(-16.8093108953179,34.7836543310606,8.36249028807224));
#61500=CARTESIAN_POINT('Ctrl Pts',(-16.8006015595804,34.7859667131828,8.34119724755845));
#61501=CARTESIAN_POINT('Ctrl Pts',(-16.7967937163622,34.787001760402,8.33155220348613));
#61502=CARTESIAN_POINT('Ctrl Pts',(-16.7876269695703,34.7895567082208,8.30747402249677));
#61503=CARTESIAN_POINT('Ctrl Pts',(-16.7824115344412,34.7910685242448,8.29298807496062));
#61504=CARTESIAN_POINT('Ctrl Pts',(-16.7508127296122,34.8006414901204,8.19994714233014));
#61505=CARTESIAN_POINT('Ctrl Pts',(-16.7319030157318,34.8083541747029,8.11904946444439));
#61506=CARTESIAN_POINT('Ctrl Pts',(-16.7147190815839,34.8206084640349,7.98940313888672));
#61507=CARTESIAN_POINT('Ctrl Pts',(-16.7111174353948,34.8251014430528,7.94161960789952));
#61508=CARTESIAN_POINT('Ctrl Pts',(-16.7095721672306,34.8329647416264,7.85900178640592));
#61509=CARTESIAN_POINT('Ctrl Pts',(-16.7103489075829,34.8363012606013,7.82424560786309));
#61510=CARTESIAN_POINT('Ctrl Pts',(-16.7137967816126,34.841596540539,7.7699137009731));
#61511=CARTESIAN_POINT('Ctrl Pts',(-16.715500969673,34.8435251032127,7.75029221378086));
#61512=CARTESIAN_POINT('Ctrl Pts',(-16.7196584425836,34.84726574084,7.71261181284371));
#61513=CARTESIAN_POINT('Ctrl Pts',(-16.7220456171656,34.8490752747315,7.69455039120294));
#61514=CARTESIAN_POINT('Ctrl Pts',(-16.7287229801233,34.8534601084332,7.65122554098748));
#61515=CARTESIAN_POINT('Ctrl Pts',(-16.7333907122903,34.8560466933605,7.62602974709626));
#61516=CARTESIAN_POINT('Ctrl Pts',(-16.7558234819504,34.866836993304,7.52252558737143));
#61517=CARTESIAN_POINT('Ctrl Pts',(-16.780229679866,34.8752391929057,7.44586257015318));
#61518=CARTESIAN_POINT('Ctrl Pts',(-16.8300833161191,34.8886434046107,7.32889929835048));
#61519=CARTESIAN_POINT('Ctrl Pts',(-16.8508429649672,34.8935927622566,7.28681633197213));
#61520=CARTESIAN_POINT('Ctrl Pts',(-16.8877523411963,34.9014272139768,7.22139245582048));
#61521=CARTESIAN_POINT('Ctrl Pts',(-16.9024386638579,34.9043474033965,7.1972752165736));
#61522=CARTESIAN_POINT('Ctrl Pts',(-16.9247780382346,34.9085022707195,7.16320219648806));
#61523=CARTESIAN_POINT('Ctrl Pts',(-16.9317924709225,34.9097697903486,7.15284064129368));
#61524=CARTESIAN_POINT('Ctrl Pts',(-16.9448929367575,34.9120685326634,7.13409193200277));
#61525=CARTESIAN_POINT('Ctrl Pts',(-16.950929882046,34.9131024179989,7.12567344040614));
#61526=CARTESIAN_POINT('Ctrl Pts',(-16.9662462111649,34.9156649159831,7.10485753645008));
#61527=CARTESIAN_POINT('Ctrl Pts',(-16.9756505664244,34.9171852417243,7.09255416205871));
#61528=CARTESIAN_POINT('Ctrl Pts',(-17.0362275249785,34.9266755801127,7.01623817326308));
#61529=CARTESIAN_POINT('Ctrl Pts',(-17.0932797509064,34.9343054734622,6.95712100496252));
#61530=CARTESIAN_POINT('Ctrl Pts',(-17.192401465746,34.9465127958986,6.87254145042423));
#61531=CARTESIAN_POINT('Ctrl Pts',(-17.2309175522031,34.9510451173478,6.84330145160162));
#61532=CARTESIAN_POINT('Ctrl Pts',(-17.2999942708169,34.958965891441,6.7968209763161));
#61533=CARTESIAN_POINT('Ctrl Pts',(-17.3297747032316,34.9623197173172,6.7785204597929));
#61534=CARTESIAN_POINT('Ctrl Pts',(-17.3774719532837,34.9676339506004,6.75185492942376));
#61535=CARTESIAN_POINT('Ctrl Pts',(-17.3948954246397,34.9695636781307,6.74263981984578));
#61536=CARTESIAN_POINT('Ctrl Pts',(-17.4287882394581,34.9733014371869,6.72571154580774));
#61537=CARTESIAN_POINT('Ctrl Pts',(-17.4452227994205,34.9751068530225,6.7179393552003));
#61538=CARTESIAN_POINT('Ctrl Pts',(-17.485071867192,34.9794721250435,6.70013038357828));
#61539=CARTESIAN_POINT('Ctrl Pts',(-17.5086314127971,34.9820430575475,6.69044067927907));
#61540=CARTESIAN_POINT('Ctrl Pts',(-17.6094686881542,34.9930185163473,6.65247095108091));
#61541=CARTESIAN_POINT('Ctrl Pts',(-17.6890925513004,35.0016339805726,6.63103361726451));
#61542=CARTESIAN_POINT('Ctrl Pts',(-17.8153177617025,35.0151280362244,6.60989229414256));
#61543=CARTESIAN_POINT('Ctrl Pts',(-17.8608018147034,35.019954053307,6.60477910414765));
#61544=CARTESIAN_POINT('Ctrl Pts',(-17.934235990077,35.0276233928326,6.60051999286205));
#61545=CARTESIAN_POINT('Ctrl Pts',(-17.9620559272994,35.0305004308103,6.59982197968922));
#61546=CARTESIAN_POINT('Ctrl Pts',(-18.0023232713462,35.0346061401043,6.6001352313657));
#61547=CARTESIAN_POINT('Ctrl Pts',(-18.0147659640791,35.0358666883445,6.60041493694181));
#61548=CARTESIAN_POINT('Ctrl Pts',(-18.0375706508963,35.0381598992813,6.60126312890693));
#61549=CARTESIAN_POINT('Ctrl Pts',(-18.0479323017599,35.0391951057469,6.60177571074422));
#61550=CARTESIAN_POINT('Ctrl Pts',(-18.0738559734803,35.0417700405367,6.60337679294815));
#61551=CARTESIAN_POINT('Ctrl Pts',(-18.0894064426217,35.0433012896209,6.60462511246133));
#61552=CARTESIAN_POINT('Ctrl Pts',(-18.1854685485735,35.0527012443381,6.61412090268889));
#61553=CARTESIAN_POINT('Ctrl Pts',(-18.2650761425341,35.0602400872971,6.62976366321933));
#61554=CARTESIAN_POINT('Ctrl Pts',(-18.3894177446848,35.0723950200306,6.66681382525117));
#61555=CARTESIAN_POINT('Ctrl Pts',(-18.4353252783679,35.0769696586715,6.68342587210011));
#61556=CARTESIAN_POINT('Ctrl Pts',(-18.5124730463806,35.0849532609214,6.71648009005298));
#61557=CARTESIAN_POINT('Ctrl Pts',(-18.544192813886,35.0883267981926,6.73165835359463));
#61558=CARTESIAN_POINT('Ctrl Pts',(-18.5926914165297,35.093665707833,6.7573906596634));
#61559=CARTESIAN_POINT('Ctrl Pts',(-18.6099237814297,35.095599961785,6.76705565007722));
#61560=CARTESIAN_POINT('Ctrl Pts',(-18.6425747631823,35.0993432015768,6.78638313170576));
#61561=CARTESIAN_POINT('Ctrl Pts',(-18.6580250047332,35.1011495162876,6.79598284968859));
#61562=CARTESIAN_POINT('Ctrl Pts',(-18.6945722295729,35.10551174424,6.8197936555465));
#61563=CARTESIAN_POINT('Ctrl Pts',(-18.7154577407295,35.1080786384736,6.83431254224653));
#61564=CARTESIAN_POINT('Ctrl Pts',(-18.7876516225825,35.1172289600729,6.88778429350393));
#61565=CARTESIAN_POINT('Ctrl Pts',(-18.8364102981971,35.1239304278364,6.92999612845889));
#61566=CARTESIAN_POINT('Ctrl Pts',(-18.9310181066678,35.138057438036,7.02539364014778));
#61567=CARTESIAN_POINT('Ctrl Pts',(-18.9760980848497,35.1454731876961,7.07906080627513));
#61568=CARTESIAN_POINT('Ctrl Pts',(-19.0301070089641,35.1551793704443,7.15534805556078));
#61569=CARTESIAN_POINT('Ctrl Pts',(-19.0431509260181,35.1575999794428,7.17490110336863));
#61570=CARTESIAN_POINT('Ctrl Pts',(-19.061898831167,35.161187353366,7.20476827642656));
#61571=CARTESIAN_POINT('Ctrl Pts',(-19.0680134478401,35.1623762189782,7.21481674045736));
#61572=CARTESIAN_POINT('Ctrl Pts',(-19.0793201371124,35.1646091493566,7.23399257344724));
#61573=CARTESIAN_POINT('Ctrl Pts',(-19.0845398081925,35.165654646545,7.24310125223147));
#61574=CARTESIAN_POINT('Ctrl Pts',(-19.0979726723103,35.1683873982777,7.26723127769947));
#61575=CARTESIAN_POINT('Ctrl Pts',(-19.105996381601,35.1700633786177,7.28235615901021));
#61576=CARTESIAN_POINT('Ctrl Pts',(-19.1428132450866,35.1779937768631,7.35528183623477));
#61577=CARTESIAN_POINT('Ctrl Pts',(-19.1674805005846,35.1840542108112,7.41506896214857));
#61578=CARTESIAN_POINT('Ctrl Pts',(-19.2050970514825,35.1954307883825,7.53049402873927));
#61579=CARTESIAN_POINT('Ctrl Pts',(-19.2190544804919,35.2007355109395,7.58562262149037));
#61580=CARTESIAN_POINT('Ctrl Pts',(-19.2361847440921,35.2097678230603,7.67927779760022));
#61581=CARTESIAN_POINT('Ctrl Pts',(-19.2413768717436,35.2134440816518,7.71734731961988));
#61582=CARTESIAN_POINT('Ctrl Pts',(-19.2466615981022,35.2191406475658,7.7757714159675));
#61583=CARTESIAN_POINT('Ctrl Pts',(-19.2480037007771,35.2211220256234,7.79599236003234));
#61584=CARTESIAN_POINT('Ctrl Pts',(-19.2496250406539,35.2248961886384,7.83425648268014));
#61585=CARTESIAN_POINT('Ctrl Pts',(-19.2500045800062,35.2266853465713,7.85229056311728));
#61586=CARTESIAN_POINT('Ctrl Pts',(-19.2499937487628,35.2309070600604,7.89455639469));
#61587=CARTESIAN_POINT('Ctrl Pts',(-19.2492940751784,35.2333486649948,7.91877993259425));
#61588=CARTESIAN_POINT('Ctrl Pts',(-19.2435720632792,35.2434726577152,8.01820835210988));
#61589=CARTESIAN_POINT('Ctrl Pts',(-19.2325539622436,35.2513313838714,8.09289910684355));
#61590=CARTESIAN_POINT('Ctrl Pts',(-19.1976127157057,35.2671125093263,8.23860514393419));
#61591=CARTESIAN_POINT('Ctrl Pts',(-19.1738965453011,35.275002471338,8.30939017136547));
#61592=CARTESIAN_POINT('Ctrl Pts',(-19.1376021076899,35.2843391281057,8.3926109659689));
#61593=CARTESIAN_POINT('Ctrl Pts',(-19.1308094942068,35.2860006878031,8.40740344350387));
#61594=CARTESIAN_POINT('Ctrl Pts',(-19.119228242271,35.2886947545547,8.43139686737016));
#61595=CARTESIAN_POINT('Ctrl Pts',(-19.114608242428,35.289736378826,8.44067644774265));
#61596=CARTESIAN_POINT('Ctrl Pts',(-19.1043597959818,35.291976041947,8.46064449327679));
#61597=CARTESIAN_POINT('Ctrl Pts',(-19.0986916046772,35.2931716665292,8.47131107114716));
#61598=CARTESIAN_POINT('Ctrl Pts',(-19.0806262279321,35.2968575851035,8.50416706076701));
#61599=CARTESIAN_POINT('Ctrl Pts',(-19.0677135440715,35.2993189743541,8.52606821481939));
#61600=CARTESIAN_POINT('Ctrl Pts',(-19.0331663233633,35.3055271128824,8.58083591132089));
#61601=CARTESIAN_POINT('Ctrl Pts',(-19.0106459031221,35.3092368971343,8.61311277935803));
#61602=CARTESIAN_POINT('Ctrl Pts',(-18.9343301341607,35.3209909553499,8.7123309709433));
#61603=CARTESIAN_POINT('Ctrl Pts',(-18.8752576533315,35.3289562841321,8.77485929635222));
#61604=CARTESIAN_POINT('Ctrl Pts',(-18.8103597331144,35.3371716890844,8.83093845464842));
#61605=CARTESIAN_POINT('',(-19.2499996766479,35.3992235994469,7.87090626388281));
#61606=CARTESIAN_POINT('Ctrl Pts',(-18.8103598667433,35.5078191442546,8.83093833917793));
#61607=CARTESIAN_POINT('Ctrl Pts',(-18.8515678132402,35.5027089767599,8.7953299930782));
#61608=CARTESIAN_POINT('Ctrl Pts',(-18.8904541978799,35.497572108699,8.75709794336919));
#61609=CARTESIAN_POINT('Ctrl Pts',(-18.9439507250691,35.4898573324745,8.69726237873332));
#61610=CARTESIAN_POINT('Ctrl Pts',(-18.9605359892294,35.487360783695,8.67753513813323));
#61611=CARTESIAN_POINT('Ctrl Pts',(-18.9878084884195,35.483056640536,8.64301636285372));
#61612=CARTESIAN_POINT('Ctrl Pts',(-18.9987984684321,35.4812617180433,8.62847336212095));
#61613=CARTESIAN_POINT('Ctrl Pts',(-19.0209607232215,35.4775085024284,8.59779512631827));
#61614=CARTESIAN_POINT('Ctrl Pts',(-19.0320794515118,35.475548734079,8.58162749378194));
#61615=CARTESIAN_POINT('Ctrl Pts',(-19.0607753997425,35.4702736331078,8.53775789192916));
#61616=CARTESIAN_POINT('Ctrl Pts',(-19.0776597715214,35.4669341866036,8.50962379455912));
#61617=CARTESIAN_POINT('Ctrl Pts',(-19.1259370268866,35.4566062555776,8.42162882851243));
#61618=CARTESIAN_POINT('Ctrl Pts',(-19.1536546971673,35.4495123832065,8.35989594194129));
#61619=CARTESIAN_POINT('Ctrl Pts',(-19.1973008243931,35.435801773586,8.23740060329115));
#61620=CARTESIAN_POINT('Ctrl Pts',(-19.2139032321815,35.4292084285488,8.1770652332666));
#61621=CARTESIAN_POINT('Ctrl Pts',(-19.2292579596607,35.4210399546256,8.09921288195888));
#61622=CARTESIAN_POINT('Ctrl Pts',(-19.2321897530893,35.4193178642095,8.08261448104668));
#61623=CARTESIAN_POINT('Ctrl Pts',(-19.2364031339202,35.4165548032125,8.05563510989243));
#61624=CARTESIAN_POINT('Ctrl Pts',(-19.2378883742103,35.4155037624647,8.04528864374251));
#61625=CARTESIAN_POINT('Ctrl Pts',(-19.240484634935,35.4135075085774,8.02546537682624));
#61626=CARTESIAN_POINT('Ctrl Pts',(-19.2416168867057,35.4125609966872,8.01599263969534));
#61627=CARTESIAN_POINT('Ctrl Pts',(-19.243943451768,35.4104255878687,7.99447279776066));
#61628=CARTESIAN_POINT('Ctrl Pts',(-19.2450725099584,35.4092400452403,7.9824193440969));
#61629=CARTESIAN_POINT('Ctrl Pts',(-19.2486494174628,35.4048342121886,7.93729296580199));
#61630=CARTESIAN_POINT('Ctrl Pts',(-19.2499742154868,35.4016628870377,7.90414157193482));
#61631=CARTESIAN_POINT('Ctrl Pts',(-19.2499996272734,35.3985194419833,7.870972998107));
#61632=CARTESIAN_POINT('Ctrl Pts',(-19.2499996766479,35.3992235994469,7.87090626388281));
#61633=CARTESIAN_POINT('Ctrl Pts',(-19.2500344912314,35.394352505386,7.82211858663167));
#61634=CARTESIAN_POINT('Ctrl Pts',(-19.2472537597015,35.3894814113251,7.77322280597972));
#61635=CARTESIAN_POINT('Ctrl Pts',(-19.2416465304584,35.3846103172642,7.72457636993151));
#61636=CARTESIAN_POINT('Ctrl Pts',(-19.2360459798721,35.3797450250644,7.67598787566496));
#61637=CARTESIAN_POINT('Ctrl Pts',(-19.2276256512387,35.3748797328647,7.62764869637825));
#61638=CARTESIAN_POINT('Ctrl Pts',(-19.2164265935117,35.370014440665,7.57991504889593));
#61639=CARTESIAN_POINT('Ctrl Pts',(-19.2052357867004,35.3651527329735,7.5322165692205));
#61640=CARTESIAN_POINT('Ctrl Pts',(-19.1912704296199,35.3602910252821,7.48512328742696));
#61641=CARTESIAN_POINT('Ctrl Pts',(-19.1746228287216,35.3554293175907,7.43898225431278));
#61642=CARTESIAN_POINT('Ctrl Pts',(-19.1579799320472,35.3505689837046,7.39285425957897));
#61643=CARTESIAN_POINT('Ctrl Pts',(-19.1386564860787,35.3457086498184,7.34767851120752));
#61644=CARTESIAN_POINT('Ctrl Pts',(-19.1167940742142,35.3408483159322,7.30378517077739));
#61645=CARTESIAN_POINT('Ctrl Pts',(-19.0949127015831,35.3359837667904,7.25985376266356));
#61646=CARTESIAN_POINT('Ctrl Pts',(-19.070488219198,35.3311192176485,7.2172074898685));
#61647=CARTESIAN_POINT('Ctrl Pts',(-19.0437087262131,35.3262546685067,7.17615293776065));
#61648=CARTESIAN_POINT('Ctrl Pts',(-19.0169162706987,35.3213877646951,7.13507851332577));
#61649=CARTESIAN_POINT('Ctrl Pts',(-18.9877668730102,35.3165208608835,7.09559779715689));
#61650=CARTESIAN_POINT('Ctrl Pts',(-18.9564904780592,35.3116539570719,7.05798624010442));
#61651=CARTESIAN_POINT('Ctrl Pts',(-18.9251571018419,35.3067781864347,7.02030615999646));
#61652=CARTESIAN_POINT('Ctrl Pts',(-18.8916893857305,35.3019024157974,6.98450244311401));
#61653=CARTESIAN_POINT('Ctrl Pts',(-18.8563545143047,35.2970266451602,6.95081407470642));
#61654=CARTESIAN_POINT('Ctrl Pts',(-18.8398140587157,35.2947442690135,6.9350443566057));
#61655=CARTESIAN_POINT('Ctrl Pts',(-18.8228649403526,35.2924618928668,6.91973758270855));
#61656=CARTESIAN_POINT('Ctrl Pts',(-18.8055368501529,35.2901795167202,6.90491507677324));
#61657=CARTESIAN_POINT('Ctrl Pts',(-18.767971321095,35.2852315584356,6.87278139839276));
#61658=CARTESIAN_POINT('Ctrl Pts',(-18.728443728258,35.2802836001511,6.84277327078661));
#61659=CARTESIAN_POINT('Ctrl Pts',(-18.6872241374823,35.2753356418666,6.81513791452987));
#61660=CARTESIAN_POINT('Ctrl Pts',(-18.6460804186891,35.2703967911786,6.78755342605774));
#61661=CARTESIAN_POINT('Ctrl Pts',(-18.6032513303603,35.2654579404907,6.7623333493862));
#61662=CARTESIAN_POINT('Ctrl Pts',(-18.5590397616473,35.2605190898028,6.73968457746013));
#61663=CARTESIAN_POINT('Ctrl Pts',(-18.5148731026843,35.255585255959,6.71705881197143));
#61664=CARTESIAN_POINT('Ctrl Pts',(-18.469327228762,35.2506514221152,6.69699942920419));
#61665=CARTESIAN_POINT('Ctrl Pts',(-18.4227319086503,35.2457175882714,6.67966876162019));
#61666=CARTESIAN_POINT('Ctrl Pts',(-18.3761640900494,35.2407866664772,6.66234832295057));
#61667=CARTESIAN_POINT('Ctrl Pts',(-18.3285485649792,35.2358557446831,6.64775359959792));
#61668=CARTESIAN_POINT('Ctrl Pts',(-18.280235100339,35.2309248228889,6.63599883123053));
#61669=CARTESIAN_POINT('Ctrl Pts',(-18.2319295917507,35.2259947130976,6.62424599858743));
#61670=CARTESIAN_POINT('Ctrl Pts',(-18.18292690417,35.2210646033062,6.61533232101275));
#61671=CARTESIAN_POINT('Ctrl Pts',(-18.1335894622256,35.2161344935149,6.60932150129652));
#61672=CARTESIAN_POINT('Ctrl Pts',(-18.0842038074302,35.21119956599,6.60330480777039));
#61673=CARTESIAN_POINT('Ctrl Pts',(-18.0344832902771,35.2062646384652,6.6001967012733));
#61674=CARTESIAN_POINT('Ctrl Pts',(-17.9847961574757,35.2013297109403,6.60000905638132));
#61675=CARTESIAN_POINT('Ctrl Pts',(-17.9350822971657,35.1963921288385,6.59982131055213));
#61676=CARTESIAN_POINT('Ctrl Pts',(-17.8854024046964,35.1914545467366,6.60255712443852));
#61677=CARTESIAN_POINT('Ctrl Pts',(-17.8361218523175,35.1865169646348,6.60817628861261));
#61678=CARTESIAN_POINT('Ctrl Pts',(-17.7867492134293,35.18157015608,6.61380595285597));
#61679=CARTESIAN_POINT('Ctrl Pts',(-17.7377779441546,35.1766233475252,6.62232962690223));
#61680=CARTESIAN_POINT('Ctrl Pts',(-17.6895638312621,35.1716765389703,6.63365586025215));
#61681=CARTESIAN_POINT('Ctrl Pts',(-17.6650865304908,35.1691651473136,6.63940595298807));
#61682=CARTESIAN_POINT('Ctrl Pts',(-17.6408041417708,35.1666537556569,6.64587757037487));
#61683=CARTESIAN_POINT('Ctrl Pts',(-17.6167614138093,35.1641423640002,6.65305393319909));
#61684=CARTESIAN_POINT('Ctrl Pts',(-17.5693934527408,35.1591945268656,6.66719249831603));
#61685=CARTESIAN_POINT('Ctrl Pts',(-17.5227474291937,35.1542466897311,6.68413207344764));
#61686=CARTESIAN_POINT('Ctrl Pts',(-17.4771774928875,35.1492988525965,6.70377981223909));
#61687=CARTESIAN_POINT('Ctrl Pts',(-17.4316914400847,35.144360123263,6.72339138417806));
#61688=CARTESIAN_POINT('Ctrl Pts',(-17.3872780450423,35.1394213939295,6.7457010174851));
#61689=CARTESIAN_POINT('Ctrl Pts',(-17.3442753732749,35.134482664596,6.77056641902512));
#61690=CARTESIAN_POINT('Ctrl Pts',(-17.3013163845637,35.129548952132,6.79540656174545));
#61691=CARTESIAN_POINT('Ctrl Pts',(-17.259765754346,35.1246152396679,6.8227970601231));
#61692=CARTESIAN_POINT('Ctrl Pts',(-17.2199386839969,35.1196815272039,6.85254887295969));
#61693=CARTESIAN_POINT('Ctrl Pts',(-17.1801351193651,35.1147507265897,6.88228312644039));
#61694=CARTESIAN_POINT('Ctrl Pts',(-17.142053537651,35.1098199259756,6.91437560618114));
#61695=CARTESIAN_POINT('Ctrl Pts',(-17.1059795762881,35.1048891253614,6.94859438956857));
#61696=CARTESIAN_POINT('Ctrl Pts',(-17.0699115524682,35.0999591363255,6.98280754076345));
#61697=CARTESIAN_POINT('Ctrl Pts',(-17.0358508897038,35.0950291472895,7.01914592315566));
#61698=CARTESIAN_POINT('Ctrl Pts',(-17.0040476272454,35.0900991582536,7.0573395751517));
#61699=CARTESIAN_POINT('Ctrl Pts',(-16.9722132754166,35.0851643498927,7.09557056346179));
#61700=CARTESIAN_POINT('Ctrl Pts',(-16.9426410804493,35.0802295415318,7.1356600198791));
#61701=CARTESIAN_POINT('Ctrl Pts',(-16.9155406916189,35.0752947331709,7.17730498716906));
#61702=CARTESIAN_POINT('Ctrl Pts',(-16.8884257206899,35.0703572695027,7.21897236266217));
#61703=CARTESIAN_POINT('Ctrl Pts',(-16.8637854760545,35.0654198058345,7.26219643912664));
#61704=CARTESIAN_POINT('Ctrl Pts',(-16.8417842860779,35.0604823421662,7.3066484325213));
#61705=CARTESIAN_POINT('Ctrl Pts',(-16.8197419720682,35.0555356495236,7.35118351438731));
#61706=CARTESIAN_POINT('Ctrl Pts',(-16.8003487719911,35.050588956881,7.39695058922179));
#61707=CARTESIAN_POINT('Ctrl Pts',(-16.7837207625441,35.0456422642383,7.44360114208405));
#61708=CARTESIAN_POINT('Ctrl Pts',(-16.7752756459888,35.0431299132523,7.46729425806099));
#61709=CARTESIAN_POINT('Ctrl Pts',(-16.7675430004651,35.0406175622662,7.49121502811406));
#61710=CARTESIAN_POINT('Ctrl Pts',(-16.760533003051,35.0381052112801,7.5153166999249));
#61711=CARTESIAN_POINT('Ctrl Pts',(-16.7467269258535,35.0331571764077,7.56278455503975));
#61712=CARTESIAN_POINT('Ctrl Pts',(-16.7356659974402,35.0282091415352,7.6111646853601));
#61713=CARTESIAN_POINT('Ctrl Pts',(-16.7274642386308,35.0232611066628,7.66010915577047));
#61714=CARTESIAN_POINT('Ctrl Pts',(-16.7192775789955,35.0183221809633,7.70896352098631));
#61715=CARTESIAN_POINT('Ctrl Pts',(-16.7139397392205,35.0133832552638,7.75837962969513));
#61716=CARTESIAN_POINT('Ctrl Pts',(-16.7115144718757,35.0084443295642,7.80799625060427));
#61717=CARTESIAN_POINT('Ctrl Pts',(-16.7090916685677,35.0035104217424,7.85756246173853));
#61718=CARTESIAN_POINT('Ctrl Pts',(-16.7095756062566,34.9985765139205,7.90732823709241));
#61719=CARTESIAN_POINT('Ctrl Pts',(-16.7129783607682,34.9936426060986,7.95692620846578));
#61720=CARTESIAN_POINT('Ctrl Pts',(-16.716379106136,34.9887116114841,8.00649489490266));
#61721=CARTESIAN_POINT('Ctrl Pts',(-16.7226952167604,34.9837806168697,8.05589542796928));
#61722=CARTESIAN_POINT('Ctrl Pts',(-16.7318867077665,34.9788496222552,8.10476202791346));
#61723=CARTESIAN_POINT('Ctrl Pts',(-16.7410766827878,34.9739194409269,8.15362056811811));
#61724=CARTESIAN_POINT('Ctrl Pts',(-16.7531409944929,34.9689892595987,8.2019448119657));
#61725=CARTESIAN_POINT('Ctrl Pts',(-16.7679883939252,34.9640590782704,8.24937826339945));
#61726=CARTESIAN_POINT('Ctrl Pts',(-16.7828502946507,34.9591240816878,8.29685804256821));
#61727=CARTESIAN_POINT('Ctrl Pts',(-16.8005005453532,34.9541890851052,8.3434447685477));
#61728=CARTESIAN_POINT('Ctrl Pts',(-16.8207982721191,34.9492540885226,8.38879798966256));
#61729=CARTESIAN_POINT('Ctrl Pts',(-16.8411069118241,34.9443164386715,8.43417559463809));
#61730=CARTESIAN_POINT('Ctrl Pts',(-16.864065608919,34.9393787888205,8.47831788748006));
#61731=CARTESIAN_POINT('Ctrl Pts',(-16.8894872135768,34.9344411389694,8.52090849022546));
#61732=CARTESIAN_POINT('Ctrl Pts',(-16.9149563064051,34.9294942654694,8.56357865324362));
#61733=CARTESIAN_POINT('Ctrl Pts',(-16.9428971811849,34.9245473919694,8.60469088746089));
#61734=CARTESIAN_POINT('Ctrl Pts',(-16.9730799447014,34.9196005184694,8.64395865667199));
#61735=CARTESIAN_POINT('Ctrl Pts',(-16.9883994157531,34.9170896984997,8.66388928540193));
#61736=CARTESIAN_POINT('Ctrl Pts',(-17.0042957956781,34.9145788785299,8.68334529920754));
#61737=CARTESIAN_POINT('Ctrl Pts',(-17.020735385823,34.9120680585602,8.7022928571049));
#61738=CARTESIAN_POINT('Ctrl Pts',(-17.0531329800926,34.9071199712936,8.73963291776023));
#61739=CARTESIAN_POINT('Ctrl Pts',(-17.0877856780777,34.902171884027,8.77516103834506));
#61740=CARTESIAN_POINT('Ctrl Pts',(-17.1244629481944,34.8972237967604,8.80859275140382));
#61741=CARTESIAN_POINT('Ctrl Pts',(-17.161072725266,34.892284814901,8.84196294385018));
#61742=CARTESIAN_POINT('Ctrl Pts',(-17.1996992836833,34.8873458330415,8.87324401392446));
#61743=CARTESIAN_POINT('Ctrl Pts',(-17.2400736637485,34.8824068511821,8.90218652235024));
#61744=CARTESIAN_POINT('Ctrl Pts',(-17.2804070430736,34.8774728849269,8.93109963925923));
#61745=CARTESIAN_POINT('Ctrl Pts',(-17.3224842870685,34.8725389186717,8.95767857817394));
#61746=CARTESIAN_POINT('Ctrl Pts',(-17.3660032597972,34.8676049524165,8.98171399335457));
#61747=CARTESIAN_POINT('Ctrl Pts',(-17.4094965560649,34.8626738972317,9.00573522749272));
#61748=CARTESIAN_POINT('Ctrl Pts',(-17.4544294171664,34.8577428420468,9.02721564641119));
#61749=CARTESIAN_POINT('Ctrl Pts',(-17.5004728137367,34.852811786862,9.04599050916));
#61750=CARTESIAN_POINT('Ctrl Pts',(-17.5465086350115,34.8478815429597,9.06476228297218));
#61751=CARTESIAN_POINT('Ctrl Pts',(-17.5936541215318,34.8429512990573,9.08082917843513));
#61752=CARTESIAN_POINT('Ctrl Pts',(-17.6415602480993,34.8380210551549,9.09407456240763));
#61753=CARTESIAN_POINT('Ctrl Pts',(-17.6895131876216,34.8330859935121,9.10733288951712));
#61754=CARTESIAN_POINT('Ctrl Pts',(-17.7382277218037,34.8281509318693,9.11776405488851));
#61755=CARTESIAN_POINT('Ctrl Pts',(-17.7873413986063,34.8232158702265,9.1253018215987));
#61756=CARTESIAN_POINT('Ctrl Pts',(-17.8364814957183,34.8182781538067,9.13284364319018));
#61757=CARTESIAN_POINT('Ctrl Pts',(-17.8860206168876,34.813340437387,9.13748891546799));
#61758=CARTESIAN_POINT('Ctrl Pts',(-17.9355914456565,34.8084027209673,9.13922333743952));
#61759=CARTESIAN_POINT('Ctrl Pts',(-17.9852548879054,34.803455779382,9.14096099984214));
#61760=CARTESIAN_POINT('Ctrl Pts',(-18.0349496078833,34.7985088377967,9.13977697070298));
#61761=CARTESIAN_POINT('Ctrl Pts',(-18.0843101863803,34.7935618962114,9.13570904437683));
#61762=CARTESIAN_POINT('Ctrl Pts',(-18.109358258,34.7910515660877,9.13364477136659));
#61763=CARTESIAN_POINT('Ctrl Pts',(-18.1343204007753,34.7885412359639,9.13083870360194));
#61764=CARTESIAN_POINT('Ctrl Pts',(-18.1591499362204,34.7860309058402,9.12730079947171));
#61765=CARTESIAN_POINT('Ctrl Pts',(-18.2080779265591,34.7810841597235,9.12032916121915));
#61766=CARTESIAN_POINT('Ctrl Pts',(-18.256706745439,34.7761374136069,9.11048175221321));
#61767=CARTESIAN_POINT('Ctrl Pts',(-18.3046725750274,34.7711906674902,9.09779791457107));
#61768=CARTESIAN_POINT('Ctrl Pts',(-18.3525545270608,34.7662525717185,9.08513625707881));
#61769=CARTESIAN_POINT('Ctrl Pts',(-18.3997752627025,34.7613144759467,9.0696481430095));
#61770=CARTESIAN_POINT('Ctrl Pts',(-18.4459794440344,34.756376380175,9.05142420736049));
#61771=CARTESIAN_POINT('Ctrl Pts',(-18.4921354873705,34.7514434291764,9.03321925838572));
#61772=CARTESIAN_POINT('Ctrl Pts',(-18.5372765661141,34.7465104781779,9.01228433207194));
#61773=CARTESIAN_POINT('Ctrl Pts',(-18.5810630567823,34.7415775271793,8.988759671141));
#61774=CARTESIAN_POINT('Ctrl Pts',(-18.6248340498064,34.736646322133,8.96524333644988));
#61775=CARTESIAN_POINT('Ctrl Pts',(-18.6672509155311,34.7317151170866,8.93913932917656));
#61776=CARTESIAN_POINT('Ctrl Pts',(-18.7079966954101,34.7267839120402,8.91063481177208));
#61777=CARTESIAN_POINT('Ctrl Pts',(-18.7434460223,34.7224937033323,8.88583553296801));
#61778=CARTESIAN_POINT('Ctrl Pts',(-18.7776306342101,34.7182034946243,8.85922010858513));
#61779=CARTESIAN_POINT('Ctrl Pts',(-18.810359785549,34.7139132859163,8.83093840933901));
#61780=CARTESIAN_POINT('Origin',(-17.98,41.616,7.87));
#61781=CARTESIAN_POINT('',(-19.6843398922845,41.2062399153875,7.87060594373627));
#61782=CARTESIAN_POINT('',(-17.1849388579978,41.466,9.37753196187617));
#61783=CARTESIAN_POINT('Ctrl Pts',(-19.6843398922843,41.2062399154299,7.87060594430517));
#61784=CARTESIAN_POINT('Ctrl Pts',(-19.6843297548994,41.2083658452999,7.89911937250543));
#61785=CARTESIAN_POINT('Ctrl Pts',(-19.6836041205795,41.2104917751699,7.92762031499746));
#61786=CARTESIAN_POINT('Ctrl Pts',(-19.6821646062297,41.2126177050399,7.95608419656944));
#61787=CARTESIAN_POINT('Ctrl Pts',(-19.6790461708081,41.217223129787,8.01774580941962));
#61788=CARTESIAN_POINT('Ctrl Pts',(-19.6725665498035,41.2218285545341,8.0793623765154));
#61789=CARTESIAN_POINT('Ctrl Pts',(-19.662730990455,41.2264339792812,8.1405388130422));
#61790=CARTESIAN_POINT('Ctrl Pts',(-19.6527449850825,41.2311098492178,8.20265101247922));
#61791=CARTESIAN_POINT('Ctrl Pts',(-19.639299442682,41.2357857191544,8.26430897234697));
#61792=CARTESIAN_POINT('Ctrl Pts',(-19.6224549301031,41.240461589091,8.32510069015551));
#61793=CARTESIAN_POINT('Ctrl Pts',(-19.6059100966222,41.2450542710768,8.38481086837807));
#61794=CARTESIAN_POINT('Ctrl Pts',(-19.5860863879309,41.2496469530625,8.44368486568653));
#61795=CARTESIAN_POINT('Ctrl Pts',(-19.5630928339961,41.2542396350482,8.50134136134915));
#61796=CARTESIAN_POINT('Ctrl Pts',(-19.5401135995693,41.2588294568868,8.55896195074625));
#61797=CARTESIAN_POINT('Ctrl Pts',(-19.5139686221421,41.2634192787255,8.61536607210285));
#61798=CARTESIAN_POINT('Ctrl Pts',(-19.4848161204918,41.2680091005641,8.67018952699211));
#61799=CARTESIAN_POINT('Ctrl Pts',(-19.4556711671333,41.2725977339862,8.72499878675562));
#61800=CARTESIAN_POINT('Ctrl Pts',(-19.4235204735083,41.2771863674083,8.77822774507018));
#61801=CARTESIAN_POINT('Ctrl Pts',(-19.388568653054,41.2817750008305,8.82953592180468));
#61802=CARTESIAN_POINT('Ctrl Pts',(-19.3524639576039,41.2865149889079,8.88253648289208));
#61803=CARTESIAN_POINT('Ctrl Pts',(-19.3133703749539,41.2912549769854,8.93348681834103));
#61804=CARTESIAN_POINT('Ctrl Pts',(-19.2715611413291,41.2959949650628,8.98204525708659));
#61805=CARTESIAN_POINT('Ctrl Pts',(-19.231038090852,41.3005891362416,9.02910988596817));
#61806=CARTESIAN_POINT('Ctrl Pts',(-19.1879644814571,41.3051833074203,9.07392733321175));
#61807=CARTESIAN_POINT('Ctrl Pts',(-19.1426275072298,41.309777478599,9.11622314014492));
#61808=CARTESIAN_POINT('Ctrl Pts',(-19.0951320706632,41.3145903751258,9.16053262152224));
#61809=CARTESIAN_POINT('Ctrl Pts',(-19.0451528230316,41.3194032716526,9.20207392159138));
#61810=CARTESIAN_POINT('Ctrl Pts',(-18.993057510963,41.3242161681794,9.24057991926101));
#61811=CARTESIAN_POINT('Ctrl Pts',(-18.9409621988943,41.3290290647063,9.27908591693065));
#61812=CARTESIAN_POINT('Ctrl Pts',(-18.8867513907459,41.3338419612331,9.31455632656212));
#61813=CARTESIAN_POINT('Ctrl Pts',(-18.8308232061203,41.3386548577599,9.34677848966159));
#61814=CARTESIAN_POINT('Ctrl Pts',(-18.7773644336064,41.3432552491776,9.37757793896555));
#61815=CARTESIAN_POINT('Ctrl Pts',(-18.7221236056583,41.3478556405953,9.40553281345446));
#61816=CARTESIAN_POINT('Ctrl Pts',(-18.6654351944846,41.352456032013,9.43043373129454));
#61817=CARTESIAN_POINT('Ctrl Pts',(-18.607808944907,41.3571325311158,9.45574660347523));
#61818=CARTESIAN_POINT('Ctrl Pts',(-18.5486871913394,41.3618090302186,9.47790320675449));
#61819=CARTESIAN_POINT('Ctrl Pts',(-18.4884499478873,41.3664855293214,9.49673092000287));
#61820=CARTESIAN_POINT('Ctrl Pts',(-18.429352925331,41.3710735077401,9.51520224655699));
#61821=CARTESIAN_POINT('Ctrl Pts',(-18.3691827828313,41.3756614861588,9.53046945305033));
#61822=CARTESIAN_POINT('Ctrl Pts',(-18.3083186592228,41.3802494645776,9.54241791834642));
#61823=CARTESIAN_POINT('Ctrl Pts',(-18.2474906919437,41.3848347175079,9.55435928565732));
#61824=CARTESIAN_POINT('Ctrl Pts',(-18.1859700586657,41.3894199704383,9.5629857235566));
#61825=CARTESIAN_POINT('Ctrl Pts',(-18.124148111573,41.3940052233687,9.56823324591469));
#61826=CARTESIAN_POINT('Ctrl Pts',(-18.0623402869642,41.398589428853,9.57347956953909));
#61827=CARTESIAN_POINT('Ctrl Pts',(-18.0002317912689,41.4031736343372,9.57534846713863));
#61828=CARTESIAN_POINT('Ctrl Pts',(-17.9382191172373,41.4077578398214,9.57382780627491));
#61829=CARTESIAN_POINT('Ctrl Pts',(-17.8740378725548,41.4125023540429,9.57225396820878));
#61830=CARTESIAN_POINT('Ctrl Pts',(-17.8099598551421,41.4172468682645,9.56704906035075));
#61831=CARTESIAN_POINT('Ctrl Pts',(-17.7464220591415,41.421991382486,9.5582583277284));
#61832=CARTESIAN_POINT('Ctrl Pts',(-17.684951616891,41.4265815226202,9.54975362256054));
#61833=CARTESIAN_POINT('Ctrl Pts',(-17.623987280821,41.4311716627544,9.53789304749754));
#61834=CARTESIAN_POINT('Ctrl Pts',(-17.5639146254392,41.4357618028886,9.52276973492276));
#61835=CARTESIAN_POINT('Ctrl Pts',(-17.5008114542963,41.4405835041538,9.50688348891632));
#61836=CARTESIAN_POINT('Ctrl Pts',(-17.4386929277687,41.445405205419,9.48739676187291));
#61837=CARTESIAN_POINT('Ctrl Pts',(-17.3779852245854,41.4502269066842,9.46447579027794));
#61838=CARTESIAN_POINT('Ctrl Pts',(-17.3172775214021,41.4550486079494,9.44155481868298));
#61839=CARTESIAN_POINT('Ctrl Pts',(-17.2579811963998,41.4598703092146,9.41519993318898));
#61840=CARTESIAN_POINT('Ctrl Pts',(-17.2004925879047,41.4646920104799,9.38563288103963));
#61841=CARTESIAN_POINT('Ctrl Pts',(-17.1952942499942,41.4651280069866,9.38295931610016));
#61842=CARTESIAN_POINT('Ctrl Pts',(-17.1901096143734,41.4655640034933,9.38025898032286));
#61843=CARTESIAN_POINT('Ctrl Pts',(-17.1849388579978,41.466,9.37753196187617));
#61844=CARTESIAN_POINT('',(-18.7752089275578,41.466,9.37745401161438));
#61845=CARTESIAN_POINT('Origin',(-17.98,41.466,7.87));
#61846=CARTESIAN_POINT('',(-19.6846890250508,41.3288850845701,7.87133229203072));
#61847=CARTESIAN_POINT('Ctrl Pts',(-18.7752089275578,41.466,9.3774540116144));
#61848=CARTESIAN_POINT('Ctrl Pts',(-19.276531813104,41.42398761576,9.11299723143809));
#61849=CARTESIAN_POINT('Ctrl Pts',(-19.6623171952346,41.3782826439501,8.53412813453988));
#61850=CARTESIAN_POINT('Ctrl Pts',(-19.6866056581082,41.3325776721401,7.92091522847425));
#61851=CARTESIAN_POINT('Ctrl Pts',(-19.6862873905421,41.3288850845701,7.87133354122607));
#61852=CARTESIAN_POINT('',(-19.6843397066618,40.5351350846263,7.8709999479683));
#61853=CARTESIAN_POINT('Ctrl Pts',(-19.6843394794834,41.3288850845701,7.87133201884495));
#61854=CARTESIAN_POINT('Ctrl Pts',(-19.6843866948718,41.3243806806803,7.81091917197142));
#61855=CARTESIAN_POINT('Ctrl Pts',(-19.6812175888757,41.3198762767905,7.75035564495815));
#61856=CARTESIAN_POINT('Ctrl Pts',(-19.6748105177055,41.3153718729006,7.69002182167091));
#61857=CARTESIAN_POINT('Ctrl Pts',(-19.6684144011613,41.310875170511,7.62979115541847));
#61858=CARTESIAN_POINT('Ctrl Pts',(-19.6587913527375,41.3063784681213,7.56978993681637));
#61859=CARTESIAN_POINT('Ctrl Pts',(-19.6459717276017,41.3018817657316,7.51039877860063));
#61860=CARTESIAN_POINT('Ctrl Pts',(-19.6331641670414,41.2973892951978,7.45106351352582));
#61861=CARTESIAN_POINT('Ctrl Pts',(-19.6171660950037,41.292896824664,7.39233768859054));
#61862=CARTESIAN_POINT('Ctrl Pts',(-19.5980594616066,41.2884043541301,7.33459509312552));
#61863=CARTESIAN_POINT('Ctrl Pts',(-19.5789631759451,41.2839143166203,7.27688376978966));
#61864=CARTESIAN_POINT('Ctrl Pts',(-19.5567618295966,41.2794242791104,7.22015512428743));
#61865=CARTESIAN_POINT('Ctrl Pts',(-19.5315874972659,41.2749342416005,7.16476877981176));
#61866=CARTESIAN_POINT('Ctrl Pts',(-19.5064167450557,41.270444842633,7.10939031200142));
#61867=CARTESIAN_POINT('Ctrl Pts',(-19.4782740666417,41.2659554436654,7.05535424892268));
#61868=CARTESIAN_POINT('Ctrl Pts',(-19.4473391225447,41.2614660446978,7.00299899939525));
#61869=CARTESIAN_POINT('Ctrl Pts',(-19.4163750901459,41.2569724243231,6.95059451993223));
#61870=CARTESIAN_POINT('Ctrl Pts',(-19.3826138226266,41.2524788039485,6.89987446610507));
#61871=CARTESIAN_POINT('Ctrl Pts',(-19.3462794884679,41.2479851835738,6.85115006257451));
#61872=CARTESIAN_POINT('Ctrl Pts',(-19.309926421075,41.243489246381,6.80240053774533));
#61873=CARTESIAN_POINT('Ctrl Pts',(-19.2709979904377,41.2389933091883,6.7556491157724));
#61874=CARTESIAN_POINT('Ctrl Pts',(-19.2297579082109,41.2344973719955,6.7111730040837));
#61875=CARTESIAN_POINT('Ctrl Pts',(-19.1884442914886,41.2299934181729,6.66661758779002));
#61876=CARTESIAN_POINT('Ctrl Pts',(-19.144811183237,41.2254894643503,6.62434594199744));
#61877=CARTESIAN_POINT('Ctrl Pts',(-19.0991572632189,41.2209855105278,6.58459661748367));
#61878=CARTESIAN_POINT('Ctrl Pts',(-19.0753035348257,41.2186322385385,6.56382798271176));
#61879=CARTESIAN_POINT('Ctrl Pts',(-19.0508986500405,41.2162789665492,6.54374723572351));
#61880=CARTESIAN_POINT('Ctrl Pts',(-19.0259882433092,41.2139256945599,6.52438362433455));
#61881=CARTESIAN_POINT('Ctrl Pts',(-18.9772850169631,41.2093247284022,6.48652513577091));
#61882=CARTESIAN_POINT('Ctrl Pts',(-18.9264242815211,41.2047237622444,6.45123686267388));
#61883=CARTESIAN_POINT('Ctrl Pts',(-18.8737080489061,41.2001227960866,6.41877267152234));
#61884=CARTESIAN_POINT('Ctrl Pts',(-18.8201272098375,41.1954463688263,6.38577603053915));
#61885=CARTESIAN_POINT('Ctrl Pts',(-18.7646298188562,41.1907699415661,6.35569734333755));
#61886=CARTESIAN_POINT('Ctrl Pts',(-18.7075679961142,41.1860935143058,6.32876035392596));
#61887=CARTESIAN_POINT('Ctrl Pts',(-18.6515825471548,41.181505299855,6.30233148479151));
#61888=CARTESIAN_POINT('Ctrl Pts',(-18.5940916556415,41.1769170854042,6.27892704307211));
#61889=CARTESIAN_POINT('Ctrl Pts',(-18.535454767159,41.1723288709535,6.25871329762815));
#61890=CARTESIAN_POINT('Ctrl Pts',(-18.4768543255166,41.1677435083921,6.23851211641068));
#61891=CARTESIAN_POINT('Ctrl Pts',(-18.4171097787433,41.1631581458306,6.22149786398388));
#61892=CARTESIAN_POINT('Ctrl Pts',(-18.3565997339616,41.1585727832692,6.20778837809981));
#61893=CARTESIAN_POINT('Ctrl Pts',(-18.2961051769494,41.1539885943483,6.19408240120928));
#61894=CARTESIAN_POINT('Ctrl Pts',(-18.234846006181,41.1494044054274,6.18367962387388));
#61895=CARTESIAN_POINT('Ctrl Pts',(-18.1732131575983,41.1448202165064,6.17664725726418));
#61896=CARTESIAN_POINT('Ctrl Pts',(-18.1094275867881,41.1400759102842,6.16936926300203));
#61897=CARTESIAN_POINT('Ctrl Pts',(-18.04524231703,41.135331604062,6.16570161710359));
#61898=CARTESIAN_POINT('Ctrl Pts',(-17.9810963851869,41.1305872978398,6.16566035264695));
#61899=CARTESIAN_POINT('Ctrl Pts',(-17.9190393268576,41.1259974870833,6.16562043194241));
#61900=CARTESIAN_POINT('Ctrl Pts',(-17.8570196058036,41.1214076763267,6.16897422181227));
#61901=CARTESIAN_POINT('Ctrl Pts',(-17.7954320279454,41.1168178655701,6.17568317623543));
#61902=CARTESIAN_POINT('Ctrl Pts',(-17.7307348442592,41.1119963116151,6.18273087110756));
#61903=CARTESIAN_POINT('Ctrl Pts',(-17.6665152310406,41.1071747576601,6.19348144054158));
#61904=CARTESIAN_POINT('Ctrl Pts',(-17.6032185001076,41.1023532037051,6.20782957042942));
#61905=CARTESIAN_POINT('Ctrl Pts',(-17.5399217691746,41.0975316497501,6.22217770031727));
#61906=CARTESIAN_POINT('Ctrl Pts',(-17.4775485166543,41.092710095795,6.24012314150737));
#61907=CARTESIAN_POINT('Ctrl Pts',(-17.4165222859492,41.08788854184,6.26150141393656));
#61908=CARTESIAN_POINT('Ctrl Pts',(-17.3582416607155,41.0832839123905,6.28191786550494));
#61909=CARTESIAN_POINT('Ctrl Pts',(-17.3009568035062,41.078679282941,6.30554629026167));
#61910=CARTESIAN_POINT('Ctrl Pts',(-17.2450450522227,41.0740746534915,6.33226918469528));
#61911=CARTESIAN_POINT('Ctrl Pts',(-17.1882670556202,41.0693986841427,6.35940609911008));
#61912=CARTESIAN_POINT('Ctrl Pts',(-17.1329056035329,41.0647227147939,6.38973409954295));
#61913=CARTESIAN_POINT('Ctrl Pts',(-17.0793386582792,41.0600467454451,6.42307775498139));
#61914=CARTESIAN_POINT('Ctrl Pts',(-17.0267296199213,41.0554543937687,6.45582514499298));
#61915=CARTESIAN_POINT('Ctrl Pts',(-16.975851882681,41.0508620420924,6.49148093951536));
#61916=CARTESIAN_POINT('Ctrl Pts',(-16.9270400206117,41.0462696904161,6.52983205626807));
#61917=CARTESIAN_POINT('Ctrl Pts',(-16.8782567130356,41.0416800252235,6.56816073796811));
#61918=CARTESIAN_POINT('Ctrl Pts',(-16.8315372819656,41.0370903600309,6.60918130230569));
#61919=CARTESIAN_POINT('Ctrl Pts',(-16.7871858627384,41.0325006948383,6.65263839819519));
#61920=CARTESIAN_POINT('Ctrl Pts',(-16.7428442520281,41.0279120446709,6.69608588335138));
#61921=CARTESIAN_POINT('Ctrl Pts',(-16.7008699753855,41.0233233945036,6.74196847535455));
#61922=CARTESIAN_POINT('Ctrl Pts',(-16.661531204894,41.0187347443362,6.78999311486839));
#61923=CARTESIAN_POINT('Ctrl Pts',(-16.6208925062568,41.0139944647348,6.83960470231698));
#61924=CARTESIAN_POINT('Ctrl Pts',(-16.5830669622976,41.0092541851335,6.89150198562179));
#61925=CARTESIAN_POINT('Ctrl Pts',(-16.5483043515794,41.0045139055321,6.94532578391436));
#61926=CARTESIAN_POINT('Ctrl Pts',(-16.5146099480799,40.9999192882037,6.99749565090883));
#61927=CARTESIAN_POINT('Ctrl Pts',(-16.4837931429944,40.9953246708752,7.05147484627626));
#61928=CARTESIAN_POINT('Ctrl Pts',(-16.4560352914342,40.9907300535467,7.10690996425982));
#61929=CARTESIAN_POINT('Ctrl Pts',(-16.4269574370992,40.9859169428089,7.16498125563029));
#61930=CARTESIAN_POINT('Ctrl Pts',(-16.4012370162303,40.9811038320712,7.22464983658376));
#61931=CARTESIAN_POINT('Ctrl Pts',(-16.3790253705987,40.9762907213334,7.2854873212552));
#61932=CARTESIAN_POINT('Ctrl Pts',(-16.3568137249671,40.9714776105956,7.34632480592664));
#61933=CARTESIAN_POINT('Ctrl Pts',(-16.3381109649799,40.9666644998578,7.40833056814371));
#61934=CARTESIAN_POINT('Ctrl Pts',(-16.3230075849423,40.96185138912,7.47106269660345));
#61935=CARTESIAN_POINT('Ctrl Pts',(-16.3085974875573,40.9572592121183,7.53091526457315));
#61936=CARTESIAN_POINT('Ctrl Pts',(-16.297404288211,40.9526670351166,7.59167509726248));
#61937=CARTESIAN_POINT('Ctrl Pts',(-16.2895355067767,40.948074858115,7.65296398282477));
#61938=CARTESIAN_POINT('Ctrl Pts',(-16.2815204783959,40.9433973322102,7.71539196628199));
#61939=CARTESIAN_POINT('Ctrl Pts',(-16.2769549193851,40.9387198063054,7.77836837361361));
#61940=CARTESIAN_POINT('Ctrl Pts',(-16.2758986568412,40.9340422804006,7.84147899292875));
#61941=CARTESIAN_POINT('Ctrl Pts',(-16.2748645615653,40.9294629194556,7.90326514039034));
#61942=CARTESIAN_POINT('Ctrl Pts',(-16.277193903632,40.9248835585105,7.96517938415097));
#61943=CARTESIAN_POINT('Ctrl Pts',(-16.2828906552653,40.9203041975655,8.0268269989961));
#61944=CARTESIAN_POINT('Ctrl Pts',(-16.2885838605718,40.9157276873521,8.08843623713104));
#61945=CARTESIAN_POINT('Ctrl Pts',(-16.2976402723845,40.9111511771387,8.1497786683519));
#61946=CARTESIAN_POINT('Ctrl Pts',(-16.310011835137,40.9065746669254,8.21046198733116));
#61947=CARTESIAN_POINT('Ctrl Pts',(-16.3223802683048,40.9019993144135,8.27112995549418));
#61948=CARTESIAN_POINT('Ctrl Pts',(-16.3380620859271,40.8974239619016,8.33113864254121));
#61949=CARTESIAN_POINT('Ctrl Pts',(-16.3569580144493,40.8928486093897,8.3901053246598));
#61950=CARTESIAN_POINT('Ctrl Pts',(-16.376587056374,40.8880957449739,8.45135976230815));
#61951=CARTESIAN_POINT('Ctrl Pts',(-16.3996846056663,40.8833428805581,8.51148910210795));
#61952=CARTESIAN_POINT('Ctrl Pts',(-16.4260830286562,40.8785900161422,8.57008348200035));
#61953=CARTESIAN_POINT('Ctrl Pts',(-16.4515275362989,40.8740088979823,8.62656053548045));
#61954=CARTESIAN_POINT('Ctrl Pts',(-16.4800381188257,40.8694277798224,8.68161123322365));
#61955=CARTESIAN_POINT('Ctrl Pts',(-16.5114173684656,40.8648466616624,8.73489299335561));
#61956=CARTESIAN_POINT('Ctrl Pts',(-16.5428188313569,40.8602623005464,8.78821247144266));
#61957=CARTESIAN_POINT('Ctrl Pts',(-16.5770927170495,40.8556779394304,8.83976009758077));
#61958=CARTESIAN_POINT('Ctrl Pts',(-16.6139988800237,40.8510935783143,8.88922312366992));
#61959=CARTESIAN_POINT('Ctrl Pts',(-16.6509666238722,40.8465015678264,8.93876868276023));
#61960=CARTESIAN_POINT('Ctrl Pts',(-16.6905750740438,40.8419095573385,8.98622231814517));
#61961=CARTESIAN_POINT('Ctrl Pts',(-16.7325454664175,40.8373175468506,9.03130617075968));
#61962=CARTESIAN_POINT('Ctrl Pts',(-16.737125488584,40.836816443367,9.03622594950479));
#61963=CARTESIAN_POINT('Ctrl Pts',(-16.7417336040733,40.8363153398835,9.04111754694237));
#61964=CARTESIAN_POINT('Ctrl Pts',(-16.7463694267337,40.8358142364,9.04598063092151));
#61965=CARTESIAN_POINT('Ctrl Pts',(-16.7889058330266,40.8312163164769,9.09060229381292));
#61966=CARTESIAN_POINT('Ctrl Pts',(-16.8339535664908,40.8266183965537,9.13300456901429));
#61967=CARTESIAN_POINT('Ctrl Pts',(-16.8812518847845,40.8220204766306,9.17289194291406));
#61968=CARTESIAN_POINT('Ctrl Pts',(-16.929361716829,40.817343668591,9.21346367840577));
#61969=CARTESIAN_POINT('Ctrl Pts',(-16.9797997930329,40.8126668605514,9.2514329514709));
#61970=CARTESIAN_POINT('Ctrl Pts',(-17.032250656482,40.8079900525118,9.28652603839862));
#61971=CARTESIAN_POINT('Ctrl Pts',(-17.0836748790441,40.8034047854314,9.32093223486302));
#61972=CARTESIAN_POINT('Ctrl Pts',(-17.1370333614423,40.7988195183511,9.35257352756306));
#61973=CARTESIAN_POINT('Ctrl Pts',(-17.1919955569535,40.7942342512708,9.38123255435389));
#61974=CARTESIAN_POINT('Ctrl Pts',(-17.2469241148445,40.789651790437,9.40987404142584));
#61975=CARTESIAN_POINT('Ctrl Pts',(-17.3034539893868,40.7850693296032,9.43553664692506));
#61976=CARTESIAN_POINT('Ctrl Pts',(-17.3612285269365,40.7804868687695,9.45804807853));
#61977=CARTESIAN_POINT('Ctrl Pts',(-17.418988908309,40.7759055307509,9.48055399428266));
#61978=CARTESIAN_POINT('Ctrl Pts',(-17.477992873332,40.7713241927323,9.49991008424874));
#61979=CARTESIAN_POINT('Ctrl Pts',(-17.5378641048536,40.7667428547137,9.51599231037787));
#61980=CARTESIAN_POINT('Ctrl Pts',(-17.5999022192742,40.7619957071275,9.53265659069048));
#61981=CARTESIAN_POINT('Ctrl Pts',(-17.662871036358,40.7572485595414,9.54580527134963));
#61982=CARTESIAN_POINT('Ctrl Pts',(-17.7263375990724,40.7525014119553,9.55535759468299));
#61983=CARTESIAN_POINT('Ctrl Pts',(-17.7876647122538,40.7479142900937,9.56458791044543));
#61984=CARTESIAN_POINT('Ctrl Pts',(-17.8494560127494,40.7433271682322,9.57046051341741));
#61985=CARTESIAN_POINT('Ctrl Pts',(-17.9113157728559,40.7387400463706,9.57295546405114));
#61986=CARTESIAN_POINT('Ctrl Pts',(-17.9764125800368,40.7339128859222,9.57558097245999));
#61987=CARTESIAN_POINT('Ctrl Pts',(-18.0415845644202,40.7290857254738,9.57446561933227));
#61988=CARTESIAN_POINT('Ctrl Pts',(-18.106373948019,40.7242585650253,9.56964833446866));
#61989=CARTESIAN_POINT('Ctrl Pts',(-18.1711633316178,40.7194314045769,9.56483104960505));
#61990=CARTESIAN_POINT('Ctrl Pts',(-18.2355694820098,40.7146042441284,9.55631199444223));
#61991=CARTESIAN_POINT('Ctrl Pts',(-18.2991476115092,40.70977708368,9.5441922343829));
#61992=CARTESIAN_POINT('Ctrl Pts',(-18.3597066094884,40.7051791503632,9.53264800477561));
#61993=CARTESIAN_POINT('Ctrl Pts',(-18.4197622963201,40.7005812170465,9.51779011094725));
#61994=CARTESIAN_POINT('Ctrl Pts',(-18.4789249876019,40.6959832837297,9.49967748108222));
#61995=CARTESIAN_POINT('Ctrl Pts',(-18.5391025569833,40.6913064773643,9.48125414676847));
#61996=CARTESIAN_POINT('Ctrl Pts',(-18.5983556664829,40.6866296709989,9.45946336625983));
#61997=CARTESIAN_POINT('Ctrl Pts',(-18.6562832944428,40.6819528646335,9.43442185527358));
#61998=CARTESIAN_POINT('Ctrl Pts',(-18.7130778238389,40.6773675393586,9.40987017100962));
#61999=CARTESIAN_POINT('Ctrl Pts',(-18.7685977698348,40.6727822140837,9.38219399544168));
#62000=CARTESIAN_POINT('Ctrl Pts',(-18.822481286114,40.6681968888088,9.35155327887583));
#62001=CARTESIAN_POINT('Ctrl Pts',(-18.8763320202996,40.6636143531915,9.3209312037593));
#62002=CARTESIAN_POINT('Ctrl Pts',(-18.9285478574583,40.6590318175742,9.28734841497482));
#62003=CARTESIAN_POINT('Ctrl Pts',(-18.9787906759488,40.6544492819569,9.25101123139448));
#62004=CARTESIAN_POINT('Ctrl Pts',(-19.0290213649992,40.6498678526389,9.214682820206));
#62005=CARTESIAN_POINT('Ctrl Pts',(-19.0772795688207,40.6452864233208,9.17560163236285));
#62006=CARTESIAN_POINT('Ctrl Pts',(-19.1232570588381,40.6407049940028,9.13401666643163));
#62007=CARTESIAN_POINT('Ctrl Pts',(-19.1708970425558,40.6359579054159,9.09092803547077));
#62008=CARTESIAN_POINT('Ctrl Pts',(-19.2160877418717,40.631210816829,9.0451514317453));
#62009=CARTESIAN_POINT('Ctrl Pts',(-19.2585266288888,40.6264637282421,8.99700687434557));
#62010=CARTESIAN_POINT('Ctrl Pts',(-19.2995365939041,40.621876474651,8.95048334949812));
#62011=CARTESIAN_POINT('Ctrl Pts',(-19.3379768509753,40.6172892210598,8.90174926454744));
#62012=CARTESIAN_POINT('Ctrl Pts',(-19.3736161279271,40.6127019674687,8.85112635454431));
#62013=CARTESIAN_POINT('Ctrl Pts',(-19.4111180892393,40.6078749613839,8.79785764162936));
#62014=CARTESIAN_POINT('Ctrl Pts',(-19.4455179006577,40.6030479552991,8.74249778810949));
#62015=CARTESIAN_POINT('Ctrl Pts',(-19.4766001645925,40.5982209492143,8.68545250195326));
#62016=CARTESIAN_POINT('Ctrl Pts',(-19.5076824285273,40.5933939431296,8.62840721579704));
#62017=CARTESIAN_POINT('Ctrl Pts',(-19.5354469380275,40.5885669370448,8.56967711579668));
#62018=CARTESIAN_POINT('Ctrl Pts',(-19.5597375386922,40.58373993096,8.50969066309164));
#62019=CARTESIAN_POINT('Ctrl Pts',(-19.5856975325918,40.578581184569,8.44558158782522));
#62020=CARTESIAN_POINT('Ctrl Pts',(-19.6077811078423,40.573422438178,8.37981635125834));
#62021=CARTESIAN_POINT('Ctrl Pts',(-19.625800376658,40.568263691787,8.3128498117788));
#62022=CARTESIAN_POINT('Ctrl Pts',(-19.6437505923802,40.5631247146442,8.24613990017688));
#62023=CARTESIAN_POINT('Ctrl Pts',(-19.6576674377672,40.5579857375013,8.17823812217481));
#62024=CARTESIAN_POINT('Ctrl Pts',(-19.6674119112357,40.5528467603585,8.10961610425827));
#62025=CARTESIAN_POINT('Ctrl Pts',(-19.6770963151771,40.5477394622928,8.04141710480199));
#62026=CARTESIAN_POINT('Ctrl Pts',(-19.6826595011998,40.5426321642272,7.97250698363599));
#62027=CARTESIAN_POINT('Ctrl Pts',(-19.6840133521854,40.5375248661615,7.90336661765679));
#62028=CARTESIAN_POINT('Ctrl Pts',(-19.6842245145942,40.5367282723164,7.89258267881568));
#62029=CARTESIAN_POINT('Ctrl Pts',(-19.6843333742035,40.5359316784714,7.88179316972827));
#62030=CARTESIAN_POINT('Ctrl Pts',(-19.6843397066618,40.5351350846263,7.8709999479683));
#62031=CARTESIAN_POINT('',(-19.6843394289759,39.7413850845213,7.86860485198167));
#62032=CARTESIAN_POINT('Ctrl Pts',(-19.6843397066623,40.5351350845702,7.870999947208));
#62033=CARTESIAN_POINT('Ctrl Pts',(-19.6843764767214,40.5305095784063,7.80832796688859));
#62034=CARTESIAN_POINT('Ctrl Pts',(-19.6809520465325,40.5258840722424,7.74564882250062));
#62035=CARTESIAN_POINT('Ctrl Pts',(-19.6740904775037,40.5212585660785,7.68336589370801));
#62036=CARTESIAN_POINT('Ctrl Pts',(-19.6672272265936,40.5166319261284,7.62106769836471));
#62037=CARTESIAN_POINT('Ctrl Pts',(-19.6569252202841,40.5120052861783,7.55916640317225));
#62038=CARTESIAN_POINT('Ctrl Pts',(-19.6432602041901,40.5073786462282,7.4980587025382));
#62039=CARTESIAN_POINT('Ctrl Pts',(-19.629576420193,40.5027456519256,7.4368670749337));
#62040=CARTESIAN_POINT('Ctrl Pts',(-19.612520516517,40.4981126576229,7.37647170126624));
#62041=CARTESIAN_POINT('Ctrl Pts',(-19.5922188435867,40.4934796633203,7.3172566273723));
#62042=CARTESIAN_POINT('Ctrl Pts',(-19.5719019880193,40.4888432042258,7.25799726939485));
#62043=CARTESIAN_POINT('Ctrl Pts',(-19.5483347177753,40.4842067451313,7.19992042690849));
#62044=CARTESIAN_POINT('Ctrl Pts',(-19.5216913956772,40.4795702860367,7.1433897357627));
#62045=CARTESIAN_POINT('Ctrl Pts',(-19.4949939983899,40.4749244168018,7.0867443101328));
#62046=CARTESIAN_POINT('Ctrl Pts',(-19.4652083192726,40.4702785475669,7.03165173711978));
#62047=CARTESIAN_POINT('Ctrl Pts',(-19.4325540921733,40.4656326783319,6.97844997621524));
#62048=CARTESIAN_POINT('Ctrl Pts',(-19.4139752396213,40.4629893783013,6.94818045955054));
#62049=CARTESIAN_POINT('Ctrl Pts',(-19.3944685912067,40.4603460782706,6.91852247669673));
#62050=CARTESIAN_POINT('Ctrl Pts',(-19.374080442917,40.45770277824,6.88953350170625));
#62051=CARTESIAN_POINT('Ctrl Pts',(-19.338621087469,40.4531055134953,6.83911546699063));
#62052=CARTESIAN_POINT('Ctrl Pts',(-19.3003502955231,40.4485082487506,6.79052003030235));
#62053=CARTESIAN_POINT('Ctrl Pts',(-19.2594821054512,40.4439109840059,6.74407798785612));
#62054=CARTESIAN_POINT('Ctrl Pts',(-19.2179060732883,40.439234094069,6.69683156350846));
#62055=CARTESIAN_POINT('Ctrl Pts',(-19.1736420396137,40.4345572041321,6.65181432598553));
#62056=CARTESIAN_POINT('Ctrl Pts',(-19.1269615127042,40.4298803141952,6.60934377248382));
#62057=CARTESIAN_POINT('Ctrl Pts',(-19.0812019895078,40.4252956989879,6.56771116019797));
#62058=CARTESIAN_POINT('Ctrl Pts',(-19.0331208560809,40.4207110837805,6.52852601220936));
#62059=CARTESIAN_POINT('Ctrl Pts',(-18.9830127669683,40.4161264685732,6.49205216902143));
#62060=CARTESIAN_POINT('Ctrl Pts',(-18.9329353153014,40.4115446565241,6.4556006269311));
#62061=CARTESIAN_POINT('Ctrl Pts',(-18.8808337760716,40.4069628444749,6.42185740148218));
#62062=CARTESIAN_POINT('Ctrl Pts',(-18.827035295064,40.4023810324258,6.39104562459966));
#62063=CARTESIAN_POINT('Ctrl Pts',(-18.7732499487917,40.3978003390121,6.36024137031863));
#62064=CARTESIAN_POINT('Ctrl Pts',(-18.7177689247181,40.3932196455984,6.33236739669762));
#62065=CARTESIAN_POINT('Ctrl Pts',(-18.6609459569101,40.3886389521846,6.30760202273307));
#62066=CARTESIAN_POINT('Ctrl Pts',(-18.6020503339371,40.3838911749626,6.28193331544677));
#62067=CARTESIAN_POINT('Ctrl Pts',(-18.5417134868834,40.3791433977405,6.25960465799173));
#62068=CARTESIAN_POINT('Ctrl Pts',(-18.4803519018833,40.3743956205185,6.2407600514713));
#62069=CARTESIAN_POINT('Ctrl Pts',(-18.4210747686482,40.3698091251898,6.22255559584208));
#62070=CARTESIAN_POINT('Ctrl Pts',(-18.3608419357492,40.3652226298612,6.20760232376056));
#62071=CARTESIAN_POINT('Ctrl Pts',(-18.3000417372015,40.3606361345325,6.19597845830795));
#62072=CARTESIAN_POINT('Ctrl Pts',(-18.2360345242219,40.3558077163638,6.1837414714322));
#62073=CARTESIAN_POINT('Ctrl Pts',(-18.17139907354,40.350979298195,6.17519494178607));
#62074=CARTESIAN_POINT('Ctrl Pts',(-18.1065943178466,40.3461508800263,6.1703680650538));
#62075=CARTESIAN_POINT('Ctrl Pts',(-18.0417895621532,40.3413224618575,6.16554118832153));
#62076=CARTESIAN_POINT('Ctrl Pts',(-17.976816152265,40.3364940436887,6.16443389803849));
#62077=CARTESIAN_POINT('Ctrl Pts',(-17.912129343232,40.33166562552,6.16701191737878));
#62078=CARTESIAN_POINT('Ctrl Pts',(-17.8505401687129,40.3270684241169,6.16946648401203));
#62079=CARTESIAN_POINT('Ctrl Pts',(-17.7889578794678,40.3224712227139,6.17527149008939));
#62080=CARTESIAN_POINT('Ctrl Pts',(-17.7277764699386,40.3178740213108,6.18442646957086));
#62081=CARTESIAN_POINT('Ctrl Pts',(-17.6655344279044,40.3131971234562,6.19374015851809));
#62082=CARTESIAN_POINT('Ctrl Pts',(-17.6037078310183,40.3085202256015,6.20652115043136));
#62083=CARTESIAN_POINT('Ctrl Pts',(-17.5427106807571,40.3038433277469,6.2227134776014));
#62084=CARTESIAN_POINT('Ctrl Pts',(-17.4829178855075,40.299258772655,6.23858609622287));
#62085=CARTESIAN_POINT('Ctrl Pts',(-17.4239225966,40.294674217563,6.25773642800875));
#62086=CARTESIAN_POINT('Ctrl Pts',(-17.36610626441,40.2900896624711,6.28005996433722));
#62087=CARTESIAN_POINT('Ctrl Pts',(-17.3083252657952,40.2855079091605,6.30236985797478));
#62088=CARTESIAN_POINT('Ctrl Pts',(-17.2517222691486,40.2809261558499,6.32784892791736));
#62089=CARTESIAN_POINT('Ctrl Pts',(-17.1966621383518,40.2763444025394,6.35634329185628));
#62090=CARTESIAN_POINT('Ctrl Pts',(-17.1416154327199,40.2717637663855,6.38483070809043));
#62091=CARTESIAN_POINT('Ctrl Pts',(-17.0881112980373,40.2671831302316,6.41633172495502));
#62092=CARTESIAN_POINT('Ctrl Pts',(-17.0364913621257,40.2626024940777,6.45064582085491));
#62093=CARTESIAN_POINT('Ctrl Pts',(-16.9829872339476,40.2578546589712,6.4862124242015));
#62094=CARTESIAN_POINT('Ctrl Pts',(-16.9315080360422,40.2531068238647,6.52480117070112));
#62095=CARTESIAN_POINT('Ctrl Pts',(-16.8824006114525,40.2483589887583,6.56614018473609));
#62096=CARTESIAN_POINT('Ctrl Pts',(-16.8349624902802,40.2437725463014,6.60607396610043));
#62097=CARTESIAN_POINT('Ctrl Pts',(-16.7897378088916,40.2391861038445,6.64857361098501));
#62098=CARTESIAN_POINT('Ctrl Pts',(-16.7470028516324,40.2345996613876,6.69335524999374));
#62099=CARTESIAN_POINT('Ctrl Pts',(-16.7020121892007,40.2297711299563,6.7405006254192));
#62100=CARTESIAN_POINT('Ctrl Pts',(-16.6597817923486,40.2249425985251,6.79017508808613));
#62101=CARTESIAN_POINT('Ctrl Pts',(-16.620585057557,40.2201140670938,6.84200882792571));
#62102=CARTESIAN_POINT('Ctrl Pts',(-16.5813883227654,40.2152855356625,6.89384256776529));
#62103=CARTESIAN_POINT('Ctrl Pts',(-16.5452255471153,40.2104570042313,6.94783500177105));
#62104=CARTESIAN_POINT('Ctrl Pts',(-16.5123147928673,40.2056284728,7.00358499068649));
#62105=CARTESIAN_POINT('Ctrl Pts',(-16.4809818950911,40.2010314380252,7.05666213047317));
#62106=CARTESIAN_POINT('Ctrl Pts',(-16.4524675419473,40.1964344032503,7.1115501949038));
#62107=CARTESIAN_POINT('Ctrl Pts',(-16.4269849961933,40.1918373684755,7.16791792961851));
#62108=CARTESIAN_POINT('Ctrl Pts',(-16.4010596333957,40.1871604497923,7.22526518160277));
#62109=CARTESIAN_POINT('Ctrl Pts',(-16.3782728046745,40.1824835311092,7.28414361158134));
#62110=CARTESIAN_POINT('Ctrl Pts',(-16.3588020123882,40.177806612426,7.34417500956728));
#62111=CARTESIAN_POINT('Ctrl Pts',(-16.3397164722956,40.173222232,7.4030186167629));
#62112=CARTESIAN_POINT('Ctrl Pts',(-16.3238171057571,40.1686378515739,7.46296947427151));
#62113=CARTESIAN_POINT('Ctrl Pts',(-16.3112229569419,40.1640534711478,7.52365044223742));
#62114=CARTESIAN_POINT('Ctrl Pts',(-16.2986365120407,40.1594718950138,7.5842942913029));
#62115=CARTESIAN_POINT('Ctrl Pts',(-16.2893513791435,40.1548903188799,7.64566686782294));
#62116=CARTESIAN_POINT('Ctrl Pts',(-16.2834361246219,40.1503087427459,7.70737819223101));
#62117=CARTESIAN_POINT('Ctrl Pts',(-16.2775223153285,40.1457282859929,7.76907443919016));
#62118=CARTESIAN_POINT('Ctrl Pts',(-16.2749767985288,40.1411478292399,7.83110876319327));
#62119=CARTESIAN_POINT('Ctrl Pts',(-16.2758163540269,40.1365673724869,7.89308541526515));
#62120=CARTESIAN_POINT('Ctrl Pts',(-16.2766866194582,40.1318193681197,7.95732909893502));
#62121=CARTESIAN_POINT('Ctrl Pts',(-16.2811944559054,40.1270713637524,8.02151022654404));
#62122=CARTESIAN_POINT('Ctrl Pts',(-16.2892995083944,40.1223233593852,8.08518987728147));
#62123=CARTESIAN_POINT('Ctrl Pts',(-16.2971284553907,40.1177370998168,8.14670022666516));
#62124=CARTESIAN_POINT('Ctrl Pts',(-16.3083132948938,40.1131508402485,8.20774221166161));
#62125=CARTESIAN_POINT('Ctrl Pts',(-16.3227653397069,40.1085645806801,8.26792978818296));
#62126=CARTESIAN_POINT('Ctrl Pts',(-16.3379819105069,40.1037357039134,8.33130134087745));
#62127=CARTESIAN_POINT('Ctrl Pts',(-16.3568207839431,40.0989068271467,8.39372495573301));
#62128=CARTESIAN_POINT('Ctrl Pts',(-16.3791194418188,40.09407795038,8.45477027458433));
#62129=CARTESIAN_POINT('Ctrl Pts',(-16.4014180996945,40.0892490736134,8.51581559343565));
#62130=CARTESIAN_POINT('Ctrl Pts',(-16.4271762130323,40.0844201968467,8.57548205017607));
#62131=CARTESIAN_POINT('Ctrl Pts',(-16.4561749107507,40.07959132008,8.63336880534534));
#62132=CARTESIAN_POINT('Ctrl Pts',(-16.4837819774528,40.0749941783639,8.68847760804556));
#62133=CARTESIAN_POINT('Ctrl Pts',(-16.5144390938614,40.0703970366478,8.7422000535105));
#62134=CARTESIAN_POINT('Ctrl Pts',(-16.5479835516064,40.0657998949317,8.79417732450549));
#62135=CARTESIAN_POINT('Ctrl Pts',(-16.5821100289745,40.0611229896162,8.84705643722659));
#62136=CARTESIAN_POINT('Ctrl Pts',(-16.6192248450111,40.0564460843007,8.89812872126577));
#62137=CARTESIAN_POINT('Ctrl Pts',(-16.6591064655308,40.0517691789852,8.94703997428014));
#62138=CARTESIAN_POINT('Ctrl Pts',(-16.6982000360492,40.0471846880499,8.99498475420501));
#62139=CARTESIAN_POINT('Ctrl Pts',(-16.7399517260247,40.0426001971145,9.04085271512015));
#62140=CARTESIAN_POINT('Ctrl Pts',(-16.78410918698,40.0380157061792,9.08433932610881));
#62141=CARTESIAN_POINT('Ctrl Pts',(-16.8282396470474,40.0334340185148,9.1277993464131));
#62142=CARTESIAN_POINT('Ctrl Pts',(-16.8747725992589,40.0288523308503,9.16888054760084));
#62143=CARTESIAN_POINT('Ctrl Pts',(-16.923417536701,40.0242706431859,9.20731385016716));
#62144=CARTESIAN_POINT('Ctrl Pts',(-16.9720505983018,40.0196900740633,9.2457377698907));
#62145=CARTESIAN_POINT('Ctrl Pts',(-17.0227942223191,40.0151095049406,9.28151475881925));
#62146=CARTESIAN_POINT('Ctrl Pts',(-17.0753249742169,40.010528935818,9.31441612194144));
#62147=CARTESIAN_POINT('Ctrl Pts',(-17.1297746751559,40.0057810384465,9.34851937228089));
#62148=CARTESIAN_POINT('Ctrl Pts',(-17.1861441389438,40.001033141075,9.37953247427002));
#62149=CARTESIAN_POINT('Ctrl Pts',(-17.24404273101,39.9962852437035,9.40725135674708));
#62150=CARTESIAN_POINT('Ctrl Pts',(-17.2999715986737,39.9916988709733,9.43402723599598));
#62151=CARTESIAN_POINT('Ctrl Pts',(-17.3573267010973,39.987112498243,9.45772931458685));
#62152=CARTESIAN_POINT('Ctrl Pts',(-17.4157355711229,39.9825261255128,9.47822277371764));
#62153=CARTESIAN_POINT('Ctrl Pts',(-17.4772300402698,39.9776974658207,9.49979885265356));
#62154=CARTESIAN_POINT('Ctrl Pts',(-17.5398920824226,39.9728688061285,9.51781771632805));
#62155=CARTESIAN_POINT('Ctrl Pts',(-17.6032720539256,39.9680401464364,9.53218256826576));
#62156=CARTESIAN_POINT('Ctrl Pts',(-17.6666520254286,39.9632114867443,9.54654742020348));
#62157=CARTESIAN_POINT('Ctrl Pts',(-17.7307492725042,39.9583828270522,9.55725822984731));
#62158=CARTESIAN_POINT('Ctrl Pts',(-17.795108396834,39.95355416736,9.56428153819804));
#62159=CARTESIAN_POINT('Ctrl Pts',(-17.8563815022406,39.9489570418185,9.57096807903211));
#62160=CARTESIAN_POINT('Ctrl Pts',(-17.9181436440668,39.9443599162769,9.57434018552573));
#62161=CARTESIAN_POINT('Ctrl Pts',(-17.9800051116147,39.9397627907354,9.57433999999233));
#62162=CARTESIAN_POINT('Ctrl Pts',(-18.042940167196,39.9350858833981,9.57433981123906));
#62163=CARTESIAN_POINT('Ctrl Pts',(-18.1059775118455,39.9304089760608,9.57084901194266));
#62164=CARTESIAN_POINT('Ctrl Pts',(-18.168699409273,39.9257320687235,9.56386167337833));
#62165=CARTESIAN_POINT('Ctrl Pts',(-18.2301816966983,39.9211475938755,9.55701242972387));
#62166=CARTESIAN_POINT('Ctrl Pts',(-18.2913603616633,39.9165631190275,9.54680365645155));
#62167=CARTESIAN_POINT('Ctrl Pts',(-18.3518426985217,39.9119786441795,9.53328224999732));
#62168=CARTESIAN_POINT('Ctrl Pts',(-18.4122880532494,39.9073969725243,9.51976911125306));
#62169=CARTESIAN_POINT('Ctrl Pts',(-18.4720374283351,39.9028153008691,9.5029474664673));
#62170=CARTESIAN_POINT('Ctrl Pts',(-18.5307072137617,39.8982336292138,9.4829154969529));
#62171=CARTESIAN_POINT('Ctrl Pts',(-18.5893626772443,39.8936530759954,9.46288841746398));
#62172=CARTESIAN_POINT('Ctrl Pts',(-18.6469385926822,39.8890725227769,9.43965273337322));
#62173=CARTESIAN_POINT('Ctrl Pts',(-18.7030674270037,39.8844919695584,9.41335619077589));
#62174=CARTESIAN_POINT('Ctrl Pts',(-18.7612470407707,39.8797440566485,9.38609885129586));
#62175=CARTESIAN_POINT('Ctrl Pts',(-18.8178712281102,39.8749961437387,9.3555528437369));
#62176=CARTESIAN_POINT('Ctrl Pts',(-18.8725566990867,39.8702482308288,9.32193573360373));
#62177=CARTESIAN_POINT('Ctrl Pts',(-18.9253814059612,39.8656618735524,9.28946250155435));
#62178=CARTESIAN_POINT('Ctrl Pts',(-18.9763968279962,39.8610755162759,9.25412418089979));
#62179=CARTESIAN_POINT('Ctrl Pts',(-19.0252877213073,39.8564891589995,9.21616062016546));
#62180=CARTESIAN_POINT('Ctrl Pts',(-19.0767619063556,39.8516604682729,9.17619114491172));
#62181=CARTESIAN_POINT('Ctrl Pts',(-19.1258803315661,39.8468317775464,9.13331172815551));
#62182=CARTESIAN_POINT('Ctrl Pts',(-19.1723178427938,39.8420030868198,9.08784769054079));
#62183=CARTESIAN_POINT('Ctrl Pts',(-19.2187553540215,39.8371743960932,9.04238365292608));
#62184=CARTESIAN_POINT('Ctrl Pts',(-19.2625115710664,39.8323457053667,8.99433552723391));
#62185=CARTESIAN_POINT('Ctrl Pts',(-19.3033114389676,39.8275170146401,8.94406781494346));
#62186=CARTESIAN_POINT('Ctrl Pts',(-19.3420164456719,39.8229362520896,8.89638108845889));
#62187=CARTESIAN_POINT('Ctrl Pts',(-19.3782245727256,39.8183554895392,8.84649586219358));
#62188=CARTESIAN_POINT('Ctrl Pts',(-19.4116758245007,39.8137747269888,8.79470490922245));
#62189=CARTESIAN_POINT('Ctrl Pts',(-19.4450771820822,39.8092007968718,8.7429912050149));
#62190=CARTESIAN_POINT('Ctrl Pts',(-19.4757295390519,39.8046268667549,8.68937783439572));
#62191=CARTESIAN_POINT('Ctrl Pts',(-19.5034132813638,39.800052936638,8.63419029682698));
#62192=CARTESIAN_POINT('Ctrl Pts',(-19.5310660730067,39.7954841202154,8.57906445941373));
#62193=CARTESIAN_POINT('Ctrl Pts',(-19.5557566030015,39.7909153037929,8.52236840080617));
#62194=CARTESIAN_POINT('Ctrl Pts',(-19.5773098418524,39.7863464873703,8.46445445975392));
#62195=CARTESIAN_POINT('Ctrl Pts',(-19.5988492724775,39.7817805979904,8.40657762165346));
#62196=CARTESIAN_POINT('Ctrl Pts',(-19.6172552172746,39.7772147086105,8.34748492686722));
#62197=CARTESIAN_POINT('Ctrl Pts',(-19.6324005160062,39.7726488192305,8.28754924296698));
#62198=CARTESIAN_POINT('Ctrl Pts',(-19.6475403841638,39.7680845670188,8.22763504990537));
#62199=CARTESIAN_POINT('Ctrl Pts',(-19.6594218054773,39.763520314807,8.16687896538041));
#62200=CARTESIAN_POINT('Ctrl Pts',(-19.6679679164472,39.7589560625952,8.10566745351237));
#62201=CARTESIAN_POINT('Ctrl Pts',(-19.6765164524315,39.7543905152473,8.04443857248084));
#62202=CARTESIAN_POINT('Ctrl Pts',(-19.6817277211054,39.7498249678993,7.98275451434472));
#62203=CARTESIAN_POINT('Ctrl Pts',(-19.683576521035,39.7452594205514,7.92100855397197));
#62204=CARTESIAN_POINT('Ctrl Pts',(-19.6840994865959,39.7439679752243,7.9035426236221));
#62205=CARTESIAN_POINT('Ctrl Pts',(-19.6843537271266,39.7426765298973,7.88607175389086));
#62206=CARTESIAN_POINT('Ctrl Pts',(-19.6843394289765,39.7413850845702,7.86860485264345));
#62207=CARTESIAN_POINT('',(-19.6843399884914,38.9476350846074,7.8698019364786));
#62208=CARTESIAN_POINT('Ctrl Pts',(-19.6843394289759,39.7413850845213,7.86860485198167));
#62209=CARTESIAN_POINT('Ctrl Pts',(-19.684279410828,39.7359640951663,7.79528553776752));
#62210=CARTESIAN_POINT('Ctrl Pts',(-19.6794842803753,39.7305431058113,7.72216833145521));
#62211=CARTESIAN_POINT('Ctrl Pts',(-19.6700551719018,39.7251221164563,7.64979929262621));
#62212=CARTESIAN_POINT('Ctrl Pts',(-19.6605095703009,39.7196341527945,7.57653616124495));
#62213=CARTESIAN_POINT('Ctrl Pts',(-19.6462148775261,39.7141461891327,7.5040398728715));
#62214=CARTESIAN_POINT('Ctrl Pts',(-19.6273250408721,39.7086582254709,7.43285580718068));
#62215=CARTESIAN_POINT('Ctrl Pts',(-19.6190889492313,39.7062654376206,7.40181909155751));
#62216=CARTESIAN_POINT('Ctrl Pts',(-19.6099799283487,39.7038726497703,7.37103155567359));
#62217=CARTESIAN_POINT('Ctrl Pts',(-19.600013546114,39.70147986192,7.34053711555268));
#62218=CARTESIAN_POINT('Ctrl Pts',(-19.5808657271779,39.6968827405744,7.28194995681868));
#62219=CARTESIAN_POINT('Ctrl Pts',(-19.558496309674,39.6922856192287,7.22428251621042));
#62220=CARTESIAN_POINT('Ctrl Pts',(-19.5330131080486,39.6876884978831,7.16791373619111));
#62221=CARTESIAN_POINT('Ctrl Pts',(-19.5070876261949,39.6830115900213,7.11056663338234));
#62222=CARTESIAN_POINT('Ctrl Pts',(-19.4779393198059,39.6783346821595,7.05456423330453));
#62223=CARTESIAN_POINT('Ctrl Pts',(-19.4457348669613,39.6736577742977,7.00028962557989));
#62224=CARTESIAN_POINT('Ctrl Pts',(-19.4141669253492,39.6690733040998,6.94708773899801));
#62225=CARTESIAN_POINT('Ctrl Pts',(-19.3796628177758,39.6644888339019,6.89554642685218));
#62226=CARTESIAN_POINT('Ctrl Pts',(-19.3424270458154,39.659904363704,6.84600420878273));
#62227=CARTESIAN_POINT('Ctrl Pts',(-19.3052140430898,39.6553226968554,6.79649228519452));
#62228=CARTESIAN_POINT('Ctrl Pts',(-19.2652729933165,39.6507410300069,6.74897743790462));
#62229=CARTESIAN_POINT('Ctrl Pts',(-19.2228513827234,39.6461593631584,6.70376877247154));
#62230=CARTESIAN_POINT('Ctrl Pts',(-19.1804401291069,39.6415788148957,6.65857114445736));
#62231=CARTESIAN_POINT('Ctrl Pts',(-19.1355498650892,39.6369982666331,6.61567895164971));
#62232=CARTESIAN_POINT('Ctrl Pts',(-19.0884666183234,39.6324177183705,6.57536623261146));
#62233=CARTESIAN_POINT('Ctrl Pts',(-19.0396629915074,39.6276698009396,6.5335805225973));
#62234=CARTESIAN_POINT('Ctrl Pts',(-18.9885034211213,39.6229218835088,6.49456686603282));
#62235=CARTESIAN_POINT('Ctrl Pts',(-18.9353440481846,39.6181739660779,6.45858489975546));
#62236=CARTESIAN_POINT('Ctrl Pts',(-18.8839936192567,39.6135876140741,6.42382735278048));
#62237=CARTESIAN_POINT('Ctrl Pts',(-18.8307778008058,39.6090012620703,6.39189867932567));
#62238=CARTESIAN_POINT('Ctrl Pts',(-18.7760450056889,39.6044149100665,6.36298733100289));
#62239=CARTESIAN_POINT('Ctrl Pts',(-18.7184200664199,39.5995862099221,6.33254827362012));
#62240=CARTESIAN_POINT('Ctrl Pts',(-18.659113969525,39.5947575097777,6.30545454127591));
#62241=CARTESIAN_POINT('Ctrl Pts',(-18.5985570975186,39.5899288096332,6.2818684082516));
#62242=CARTESIAN_POINT('Ctrl Pts',(-18.5380002255122,39.5851001094888,6.25828227522728));
#62243=CARTESIAN_POINT('Ctrl Pts',(-18.4761932205006,39.5802714093444,6.23820386849679));
#62244=CARTESIAN_POINT('Ctrl Pts',(-18.4135815295858,39.5754427092,6.22173367054894));
#62245=CARTESIAN_POINT('Ctrl Pts',(-18.3539726614825,39.5708455909013,6.2060533743812));
#62246=CARTESIAN_POINT('Ctrl Pts',(-18.2933896582679,39.5662484726026,6.19357863723256));
#62247=CARTESIAN_POINT('Ctrl Pts',(-18.2322093762423,39.5616513543039,6.18442435170193));
#62248=CARTESIAN_POINT('Ctrl Pts',(-18.1699672178508,39.5569744460612,6.17511117969463));
#62249=CARTESIAN_POINT('Ctrl Pts',(-18.1071073384429,39.5522975378185,6.16923504833745));
#62250=CARTESIAN_POINT('Ctrl Pts',(-18.0440419983898,39.5476206295759,6.16686364079612));
#62251=CARTESIAN_POINT('Ctrl Pts',(-17.982223172164,39.5430361624552,6.16453910515444));
#62252=CARTESIAN_POINT('Ctrl Pts',(-17.9202074668202,39.5384516953346,6.16558202959813));
#62253=CARTESIAN_POINT('Ctrl Pts',(-17.8583902029577,39.5338672282139,6.1700041491629));
#62254=CARTESIAN_POINT('Ctrl Pts',(-17.7966107396829,39.5292855644453,6.17442356464944));
#62255=CARTESIAN_POINT('Ctrl Pts',(-17.7350299840039,39.5247039006766,6.1822180417638));
#62256=CARTESIAN_POINT('Ctrl Pts',(-17.6740418505353,39.520122236908,6.19334724931603));
#62257=CARTESIAN_POINT('Ctrl Pts',(-17.613068606923,39.5155416917228,6.20447373974457));
#62258=CARTESIAN_POINT('Ctrl Pts',(-17.5526881988819,39.5109611465375,6.21893325305502));
#62259=CARTESIAN_POINT('Ctrl Pts',(-17.4932859760176,39.5063806013523,6.23663405984485));
#62260=CARTESIAN_POINT('Ctrl Pts',(-17.4317131686996,39.5016326809463,6.25498166222892));
#62261=CARTESIAN_POINT('Ctrl Pts',(-17.3711919934313,39.4968847605403,6.27681191536764));
#62262=CARTESIAN_POINT('Ctrl Pts',(-17.3121337194731,39.4921368401342,6.30196636932268));
#62263=CARTESIAN_POINT('Ctrl Pts',(-17.2550851949196,39.4875504911655,6.3262648187677));
#62264=CARTESIAN_POINT('Ctrl Pts',(-17.1994020424159,39.4829641421968,6.35366454761002));
#62265=CARTESIAN_POINT('Ctrl Pts',(-17.1454315278639,39.4783777932282,6.38397499990192));
#62266=CARTESIAN_POINT('Ctrl Pts',(-17.0886090409689,39.4735490871035,6.41588715216574));
#62267=CARTESIAN_POINT('Ctrl Pts',(-17.0336857643878,39.4687203809788,6.45102584457634));
#62268=CARTESIAN_POINT('Ctrl Pts',(-16.9810314190361,39.4638916748541,6.48911745255183));
#62269=CARTESIAN_POINT('Ctrl Pts',(-16.9283770736844,39.4590629687294,6.52720906052732));
#62270=CARTESIAN_POINT('Ctrl Pts',(-16.8779921144322,39.4542342626047,6.56825311340285));
#62271=CARTESIAN_POINT('Ctrl Pts',(-16.8302025118619,39.44940555648,6.61192982235833));
#62272=CARTESIAN_POINT('Ctrl Pts',(-16.7847049478526,39.4448084400745,6.65351175136677));
#62273=CARTESIAN_POINT('Ctrl Pts',(-16.7413725326871,39.4402113236689,6.69765036902677));
#62274=CARTESIAN_POINT('Ctrl Pts',(-16.7005061503624,39.4356142072634,6.74409133392642));
#62275=CARTESIAN_POINT('Ctrl Pts',(-16.6589304509126,39.4309372987841,6.79133837388919));
#62276=CARTESIAN_POINT('Ctrl Pts',(-16.619907662227,39.4262603903048,6.84096815918623));
#62277=CARTESIAN_POINT('Ctrl Pts',(-16.5837182001836,39.4215834818255,6.89267100160617));
#62278=CARTESIAN_POINT('Ctrl Pts',(-16.5482440558587,39.4169990167072,6.94335189019769));
#62279=CARTESIAN_POINT('Ctrl Pts',(-16.5154925571735,39.4124145515888,6.99602419278973));
#62280=CARTESIAN_POINT('Ctrl Pts',(-16.4856879253843,39.4078300864705,7.05036211699453));
#62281=CARTESIAN_POINT('Ctrl Pts',(-16.4559015190412,39.4032484247394,7.10466681371581));
#62282=CARTESIAN_POINT('Ctrl Pts',(-16.4290586508097,39.3986667630082,7.16063466705732));
#62283=CARTESIAN_POINT('Ctrl Pts',(-16.4053390325209,39.394085101277,7.21791283320578));
#62284=CARTESIAN_POINT('Ctrl Pts',(-16.3816252053903,39.3895045581612,7.27517701485755));
#62285=CARTESIAN_POINT('Ctrl Pts',(-16.3610333091326,39.3849240150453,7.33375040411154));
#62286=CARTESIAN_POINT('Ctrl Pts',(-16.3436952254678,39.3803434719295,7.39325948311146));
#62287=CARTESIAN_POINT('Ctrl Pts',(-16.3257235848103,39.375595549582,7.45494310422659));
#62288=CARTESIAN_POINT('Ctrl Pts',(-16.3112483819578,39.3708476272346,7.51763158045874));
#62289=CARTESIAN_POINT('Ctrl Pts',(-16.3003594938038,39.3660997048871,7.5808934356591));
#62290=CARTESIAN_POINT('Ctrl Pts',(-16.2898411630142,39.3615133580437,7.64200244054137));
#62291=CARTESIAN_POINT('Ctrl Pts',(-16.282668953038,39.3569270112002,7.70364589102187));
#62292=CARTESIAN_POINT('Ctrl Pts',(-16.2788710588162,39.3523406643567,7.76542867952014));
#62293=CARTESIAN_POINT('Ctrl Pts',(-16.2748724667317,39.3475119542573,7.83047634926123));
#62294=CARTESIAN_POINT('Ctrl Pts',(-16.2746147232969,39.3426832441578,7.8956778461991));
#62295=CARTESIAN_POINT('Ctrl Pts',(-16.2780684035736,39.3378545340584,7.96057415020563));
#62296=CARTESIAN_POINT('Ctrl Pts',(-16.2815220838503,39.333025823959,8.02547045421216));
#62297=CARTESIAN_POINT('Ctrl Pts',(-16.2886870390274,39.3281971138595,8.0900609278755));
#62298=CARTESIAN_POINT('Ctrl Pts',(-16.2994713322898,39.3233684037601,8.1538982786211));
#62299=CARTESIAN_POINT('Ctrl Pts',(-16.3097383953178,39.3187712855504,8.21467389809844));
#62300=CARTESIAN_POINT('Ctrl Pts',(-16.3233276849758,39.3141741673408,8.27501667102926));
#62301=CARTESIAN_POINT('Ctrl Pts',(-16.3401886515697,39.3095770491311,8.33453587284437));
#62302=CARTESIAN_POINT('Ctrl Pts',(-16.3573422661242,39.3049001408773,8.39508812178211));
#62303=CARTESIAN_POINT('Ctrl Pts',(-16.3778822159995,39.3002232326235,8.45478739934842));
#62304=CARTESIAN_POINT('Ctrl Pts',(-16.4017003494219,39.2955463243697,8.51323016765784));
#62305=CARTESIAN_POINT('Ctrl Pts',(-16.4250477063735,39.29096185738,8.57051778750443));
#62306=CARTESIAN_POINT('Ctrl Pts',(-16.4515446352578,39.2863773903903,8.62659762266767));
#62307=CARTESIAN_POINT('Ctrl Pts',(-16.4810389818213,39.2817929234006,8.6811046181478));
#62308=CARTESIAN_POINT('Ctrl Pts',(-16.5105152928122,39.2772112597782,8.73557828300733));
#62309=CARTESIAN_POINT('Ctrl Pts',(-16.5429851453509,39.2726295961559,8.78848056844859));
#62310=CARTESIAN_POINT('Ctrl Pts',(-16.5782495209855,39.2680479325335,8.83946914864923));
#62311=CARTESIAN_POINT('Ctrl Pts',(-16.6135052869354,39.2634673875097,8.89044528015084));
#62312=CARTESIAN_POINT('Ctrl Pts',(-16.651553932126,39.2588868424858,8.93950821541387));
#62313=CARTESIAN_POINT('Ctrl Pts',(-16.6921531316782,39.254306297462,8.9863446060038));
#62314=CARTESIAN_POINT('Ctrl Pts',(-16.7342358472203,39.2495583769268,9.03489242280685));
#62315=CARTESIAN_POINT('Ctrl Pts',(-16.7790587895914,39.2448104563917,9.08104734483284));
#62316=CARTESIAN_POINT('Ctrl Pts',(-16.8263081600114,39.2400625358565,9.12449988997354));
#62317=CARTESIAN_POINT('Ctrl Pts',(-16.871949634076,39.2354761870853,9.16647374474567));
#62318=CARTESIAN_POINT('Ctrl Pts',(-16.9198545831394,39.230889838314,9.20592592255711));
#62319=CARTESIAN_POINT('Ctrl Pts',(-16.9697063184792,39.2263034895428,9.24261848766481));
#62320=CARTESIAN_POINT('Ctrl Pts',(-17.0221923823066,39.2214747831257,9.28125000773333));
#62321=CARTESIAN_POINT('Ctrl Pts',(-17.0768361526629,39.2166460767085,9.3168218107131));
#62322=CARTESIAN_POINT('Ctrl Pts',(-17.1332359974883,39.2118173702914,9.34910971859778));
#62323=CARTESIAN_POINT('Ctrl Pts',(-17.1896358423137,39.2069886638743,9.38139762648245));
#62324=CARTESIAN_POINT('Ctrl Pts',(-17.2477911453543,39.2021599574571,9.41040141867307));
#62325=CARTESIAN_POINT('Ctrl Pts',(-17.307276231525,39.19733125104,9.43595579980049));
#62326=CARTESIAN_POINT('Ctrl Pts',(-17.3639083642674,39.1927341333355,9.46028457188976));
#62327=CARTESIAN_POINT('Ctrl Pts',(-17.4219782762463,39.188137015631,9.48158723566076));
#62328=CARTESIAN_POINT('Ctrl Pts',(-17.4811302627633,39.1835398979265,9.49969439493097));
#62329=CARTESIAN_POINT('Ctrl Pts',(-17.5413089302432,39.1788629896096,9.51811583402182));
#62330=CARTESIAN_POINT('Ctrl Pts',(-17.6026071429664,39.1741860812926,9.53322948742616));
#62331=CARTESIAN_POINT('Ctrl Pts',(-17.6646271955617,39.1695091729757,9.54490740932767));
#62332=CARTESIAN_POINT('Ctrl Pts',(-17.7254213853687,39.1649247065002,9.55635451023976));
#62333=CARTESIAN_POINT('Ctrl Pts',(-17.786908615016,39.1603402400248,9.56450036319615));
#62334=CARTESIAN_POINT('Ctrl Pts',(-17.8486996531526,39.1557557735493,9.56927486137992));
#62335=CARTESIAN_POINT('Ctrl Pts',(-17.9104529065007,39.1511741104431,9.57404643999138));
#62336=CARTESIAN_POINT('Ctrl Pts',(-17.9725090934622,39.1465924473369,9.57545071245706));
#62337=CARTESIAN_POINT('Ctrl Pts',(-18.0344726682356,39.1420107842307,9.5734692729883));
#62338=CARTESIAN_POINT('Ctrl Pts',(-18.0964211147838,39.1374302397241,9.57148831728218));
#62339=CARTESIAN_POINT('Ctrl Pts',(-18.1582764854426,39.1328496952175,9.56612330684676));
#62340=CARTESIAN_POINT('Ctrl Pts',(-18.2196440990188,39.1282691507109,9.55740793568285));
#62341=CARTESIAN_POINT('Ctrl Pts',(-18.2832541311443,39.1235212296783,9.54837409833094));
#62342=CARTESIAN_POINT('Ctrl Pts',(-18.3463394845881,39.1187733086458,9.53574032947628));
#62343=CARTESIAN_POINT('Ctrl Pts',(-18.4084699699796,39.1140253876132,9.51960247345403));
#62344=CARTESIAN_POINT('Ctrl Pts',(-18.4684861415732,39.1094390393559,9.50401379214759));
#62345=CARTESIAN_POINT('Ctrl Pts',(-18.5276109124083,39.1048526910985,9.48515592536526));
#62346=CARTESIAN_POINT('Ctrl Pts',(-18.5854726409809,39.1002663428412,9.46316594133305));
#62347=CARTESIAN_POINT('Ctrl Pts',(-18.6463919917205,39.095437635421,9.44001392733237));
#62348=CARTESIAN_POINT('Ctrl Pts',(-18.705910516523,39.0906089280008,9.41338984409157));
#62349=CARTESIAN_POINT('Ctrl Pts',(-18.7636220728151,39.0857802205807,9.38350959118104));
#62350=CARTESIAN_POINT('Ctrl Pts',(-18.8213336291072,39.0809515131605,9.35362933827051));
#62351=CARTESIAN_POINT('Ctrl Pts',(-18.877237697375,39.0761228057403,9.32049331386066));
#62352=CARTESIAN_POINT('Ctrl Pts',(-18.9309645721965,39.0712940983201,9.28436954790013));
#62353=CARTESIAN_POINT('Ctrl Pts',(-18.9819503591381,39.066711746405,9.2500887779705));
#62354=CARTESIAN_POINT('Ctrl Pts',(-19.0311881697655,39.06212939449,9.21297482694768));
#62355=CARTESIAN_POINT('Ctrl Pts',(-19.0783440253598,39.0575470425749,9.17323261068636));
#62356=CARTESIAN_POINT('Ctrl Pts',(-19.125472229701,39.0529673776596,9.13351369846791));
#62357=CARTESIAN_POINT('Ctrl Pts',(-19.170520476064,39.0483877127443,9.09116986210096));
#62358=CARTESIAN_POINT('Ctrl Pts',(-19.2131832258037,39.043808047829,9.0464497299912));
#62359=CARTESIAN_POINT('Ctrl Pts',(-19.2557543917755,39.039238214042,9.00182559821491));
#62360=CARTESIAN_POINT('Ctrl Pts',(-19.2959499050033,39.0346683802551,8.95483569878509));
#62361=CARTESIAN_POINT('Ctrl Pts',(-19.3335001504166,39.0300985464681,8.90576646905679));
#62362=CARTESIAN_POINT('Ctrl Pts',(-19.3710276077472,39.0255314859719,8.85672701792641));
#62363=CARTESIAN_POINT('Ctrl Pts',(-19.4059126688167,39.0209644254758,8.80561114451897));
#62364=CARTESIAN_POINT('Ctrl Pts',(-19.4379256173855,39.0163973649796,8.75273876643729));
#62365=CARTESIAN_POINT('Ctrl Pts',(-19.4699310998572,39.0118313696186,8.69987871931291));
#62366=CARTESIAN_POINT('Ctrl Pts',(-19.4990655340768,39.0072653742576,8.64526341917988));
#62367=CARTESIAN_POINT('Ctrl Pts',(-19.5251433765955,39.0026993788966,8.58924041972287));
#62368=CARTESIAN_POINT('Ctrl Pts',(-19.5513508421705,38.9981106877058,8.53293895120119));
#62369=CARTESIAN_POINT('Ctrl Pts',(-19.5744710062061,38.993521996515,8.47521621476008));
#62370=CARTESIAN_POINT('Ctrl Pts',(-19.5943640075944,38.9889333053243,8.41644641693734));
#62371=CARTESIAN_POINT('Ctrl Pts',(-19.6141837333932,38.9843615165127,8.35789309683448));
#62372=CARTESIAN_POINT('Ctrl Pts',(-19.6307999302125,38.9797897277011,8.29830092486713));
#62373=CARTESIAN_POINT('Ctrl Pts',(-19.6441247463646,38.9752179388895,8.2380538875451));
#62374=CARTESIAN_POINT('Ctrl Pts',(-19.6575234573653,38.9706207965091,8.17747274086993));
#62375=CARTESIAN_POINT('Ctrl Pts',(-19.6675940856779,38.9660236541288,8.11622996014002));
#62376=CARTESIAN_POINT('Ctrl Pts',(-19.6742999999685,38.9614265117484,8.05472234761063));
#62377=CARTESIAN_POINT('Ctrl Pts',(-19.6810059142591,38.9568293693681,7.99321473508123));
#62378=CARTESIAN_POINT('Ctrl Pts',(-19.6843471518562,38.9522322269878,7.93144281335181));
#62379=CARTESIAN_POINT('Ctrl Pts',(-19.6843399884914,38.9476350846074,7.8698019364786));
#62380=CARTESIAN_POINT('',(-19.6843393239652,38.1538850846314,7.87151802034673));
#62381=CARTESIAN_POINT('Ctrl Pts',(-19.6843399884913,38.9476350845702,7.86980193597941));
#62382=CARTESIAN_POINT('Ctrl Pts',(-19.684338753266,38.9468423715801,7.85917282777021));
#62383=CARTESIAN_POINT('Ctrl Pts',(-19.6842380866645,38.9460496585901,7.84854438188443));
#62384=CARTESIAN_POINT('Ctrl Pts',(-19.6840380186188,38.9452569456001,7.83791781332828));
#62385=CARTESIAN_POINT('Ctrl Pts',(-19.6828777798244,38.94065982785,7.77629199471976));
#62386=CARTESIAN_POINT('Ctrl Pts',(-19.678367839255,38.9360627100999,7.71460262236847));
#62387=CARTESIAN_POINT('Ctrl Pts',(-19.6705003692328,38.9314655923497,7.65324359934786));
#62388=CARTESIAN_POINT('Ctrl Pts',(-19.6624963462916,38.9267886840385,7.59081958927602));
#62389=CARTESIAN_POINT('Ctrl Pts',(-19.6510170464113,38.9221117757273,7.52873803761941));
#62390=CARTESIAN_POINT('Ctrl Pts',(-19.6361097136432,38.917434867416,7.46741404398989));
#62391=CARTESIAN_POINT('Ctrl Pts',(-19.6214970329153,38.9128504008982,7.40730215450473));
#62392=CARTESIAN_POINT('Ctrl Pts',(-19.6035907260735,38.9082659343803,7.34791866715934));
#62393=CARTESIAN_POINT('Ctrl Pts',(-19.5824872499946,38.9036814678624,7.2896471338876));
#62394=CARTESIAN_POINT('Ctrl Pts',(-19.5613966785499,38.8990998047151,7.23141123326809));
#62395=CARTESIAN_POINT('Ctrl Pts',(-19.5371129874217,38.8945181415678,7.17428641613707));
#62396=CARTESIAN_POINT('Ctrl Pts',(-19.5097823452457,38.8899364784205,7.11864069063157));
#62397=CARTESIAN_POINT('Ctrl Pts',(-19.4824583757741,38.8853559338742,7.06300855088364));
#62398=CARTESIAN_POINT('Ctrl Pts',(-19.4520891563378,38.8807753893279,7.00885524262533));
#62399=CARTESIAN_POINT('Ctrl Pts',(-19.4188679733629,38.8761948447816,6.95652652428732));
#62400=CARTESIAN_POINT('Ctrl Pts',(-19.3844328640819,38.8714469237898,6.90228567633601));
#62401=CARTESIAN_POINT('Ctrl Pts',(-19.3469335888698,38.866699002798,6.8500058692463));
#62402=CARTESIAN_POINT('Ctrl Pts',(-19.3066346934272,38.8619510818062,6.80003961484771));
#62403=CARTESIAN_POINT('Ctrl Pts',(-19.2677071774373,38.8573647335131,6.7517737220559));
#62404=CARTESIAN_POINT('Ctrl Pts',(-19.2261679418072,38.85277838522,6.70566678501357));
#62405=CARTESIAN_POINT('Ctrl Pts',(-19.1822949778855,38.8481920369269,6.66200098437487));
#62406=CARTESIAN_POINT('Ctrl Pts',(-19.1361036096275,38.8433633295858,6.61602772664873));
#62407=CARTESIAN_POINT('Ctrl Pts',(-19.0873255031391,38.8385346222446,6.5727611943697));
#62408=CARTESIAN_POINT('Ctrl Pts',(-19.0363246941023,38.8337059149035,6.53248253236469));
#62409=CARTESIAN_POINT('Ctrl Pts',(-18.9853238850656,38.8288772075624,6.49220387035968));
#62410=CARTESIAN_POINT('Ctrl Pts',(-18.9321009503056,38.8240485002212,6.45491338799462));
#62411=CARTESIAN_POINT('Ctrl Pts',(-18.8770524174963,38.8192197928801,6.42083755366625));
#62412=CARTESIAN_POINT('Ctrl Pts',(-18.8246440677802,38.8146226752078,6.38839603068258));
#62413=CARTESIAN_POINT('Ctrl Pts',(-18.7703659552456,38.8100255575355,6.35873453058484));
#62414=CARTESIAN_POINT('Ctrl Pts',(-18.714544800395,38.8054284398633,6.33207322287024));
#62415=CARTESIAN_POINT('Ctrl Pts',(-18.6577547762499,38.8007515315423,6.30494916366897));
#62416=CARTESIAN_POINT('Ctrl Pts',(-18.5993680358662,38.7960746232213,6.2809307968082));
#62417=CARTESIAN_POINT('Ctrl Pts',(-18.5397589719614,38.7913977149004,6.26020351320154));
#62418=CARTESIAN_POINT('Ctrl Pts',(-18.4813281167611,38.7868132484621,6.23988591671902));
#62419=CARTESIAN_POINT('Ctrl Pts',(-18.421723322332,38.7822287820238,6.22273066249775));
#62420=CARTESIAN_POINT('Ctrl Pts',(-18.3613191598753,38.7776443155856,6.20886468524928));
#62421=CARTESIAN_POINT('Ctrl Pts',(-18.3009519341659,38.7730626525183,6.19500718695452));
#62422=CARTESIAN_POINT('Ctrl Pts',(-18.2397868048023,38.7684809894511,6.18443509104636));
#62423=CARTESIAN_POINT('Ctrl Pts',(-18.1782122388083,38.7638993263838,6.17722513487865));
#62424=CARTESIAN_POINT('Ctrl Pts',(-18.116652706087,38.7593187819179,6.17001693900329));
#62425=CARTESIAN_POINT('Ctrl Pts',(-18.0546844405703,38.754738237452,6.16616931252695));
#62426=CARTESIAN_POINT('Ctrl Pts',(-17.9927027640976,38.750157692986,6.16570733869318));
#62427=CARTESIAN_POINT('Ctrl Pts',(-17.9284562296966,38.7454097719172,6.16522848398171));
#62428=CARTESIAN_POINT('Ctrl Pts',(-17.8641958670951,38.7406618508484,6.16838756877484));
#62429=CARTESIAN_POINT('Ctrl Pts',(-17.8003613125996,38.7359139297795,6.17515346488567));
#62430=CARTESIAN_POINT('Ctrl Pts',(-17.7386990628092,38.7313275815667,6.18168911598151));
#62431=CARTESIAN_POINT('Ctrl Pts',(-17.6774346141508,38.7267412333538,6.19158987077987));
#62432=CARTESIAN_POINT('Ctrl Pts',(-17.6169558001157,38.7221548851409,6.20477516697284));
#62433=CARTESIAN_POINT('Ctrl Pts',(-17.5532810660628,38.7173261776441,6.21865722206749));
#62434=CARTESIAN_POINT('Ctrl Pts',(-17.4904779260827,38.7124974701473,6.23618041750083));
#62435=CARTESIAN_POINT('Ctrl Pts',(-17.4289800006369,38.7076687626505,6.25719133313902));
#62436=CARTESIAN_POINT('Ctrl Pts',(-17.3674820751911,38.7028400551537,6.27820224877722));
#62437=CARTESIAN_POINT('Ctrl Pts',(-17.3072899369963,38.6980113476569,6.30270056771319));
#62438=CARTESIAN_POINT('Ctrl Pts',(-17.2488088849698,38.6931826401601,6.33047592129877));
#62439=CARTESIAN_POINT('Ctrl Pts',(-17.1931326450915,38.6885855225027,6.35691914000543));
#62440=CARTESIAN_POINT('Ctrl Pts',(-17.1387783624963,38.6839884048453,6.38644082732598));
#62441=CARTESIAN_POINT('Ctrl Pts',(-17.0861081909103,38.6793912871879,6.41888585244221));
#62442=CARTESIAN_POINT('Ctrl Pts',(-17.0325238404077,38.6747143788651,6.45189401523234));
#62443=CARTESIAN_POINT('Ctrl Pts',(-16.9806831395575,38.6700374705423,6.48792782068988));
#62444=CARTESIAN_POINT('Ctrl Pts',(-16.9309448705333,38.6653605622195,6.52677322430665));
#62445=CARTESIAN_POINT('Ctrl Pts',(-16.8821897082562,38.6607760957974,6.5648508252005));
#62446=CARTESIAN_POINT('Ctrl Pts',(-16.8354550433037,38.6561916293753,6.60562956146449));
#62447=CARTESIAN_POINT('Ctrl Pts',(-16.7910506385862,38.6516071629532,6.64886354096122));
#62448=CARTESIAN_POINT('Ctrl Pts',(-16.7466733868738,38.6470254999025,6.6920710831603));
#62449=CARTESIAN_POINT('Ctrl Pts',(-16.7046239339443,38.6424438368519,6.73773053721606));
#62450=CARTESIAN_POINT('Ctrl Pts',(-16.6651774008687,38.6378621738012,6.78555711611273));
#62451=CARTESIAN_POINT('Ctrl Pts',(-16.6257404985668,38.6332816293523,6.83337201826824));
#62452=CARTESIAN_POINT('Ctrl Pts',(-16.5889055783388,38.6287010849034,6.88335260237634));
#62453=CARTESIAN_POINT('Ctrl Pts',(-16.5549080774639,38.6241205404544,6.93518031261509));
#62454=CARTESIAN_POINT('Ctrl Pts',(-16.519668281622,38.6193726193699,6.98890184745642));
#62455=CARTESIAN_POINT('Ctrl Pts',(-16.4874776552696,38.6146246982854,7.04460766067788));
#62456=CARTESIAN_POINT('Ctrl Pts',(-16.4585484351101,38.6098767772009,7.1019114821232));
#62457=CARTESIAN_POINT('Ctrl Pts',(-16.430603683228,38.6052904290058,7.15726524082667));
#62458=CARTESIAN_POINT('Ctrl Pts',(-16.4057020633575,38.6007040808107,7.21410947465085));
#62459=CARTESIAN_POINT('Ctrl Pts',(-16.3839861867937,38.5961177326157,7.27207463370862));
#62460=CARTESIAN_POINT('Ctrl Pts',(-16.3611227642605,38.5912890250864,7.33310288278007));
#62461=CARTESIAN_POINT('Ctrl Pts',(-16.3417913177011,38.5864603175571,7.39537319680126));
#62462=CARTESIAN_POINT('Ctrl Pts',(-16.326098069667,38.5816316100279,7.4584380478703));
#62463=CARTESIAN_POINT('Ctrl Pts',(-16.3104048216329,38.5768029024986,7.52150289893934));
#62464=CARTESIAN_POINT('Ctrl Pts',(-16.2983498164063,38.5719741949694,7.58536163400675));
#62465=CARTESIAN_POINT('Ctrl Pts',(-16.289976070027,38.5671454874401,7.64955964135714));
#62466=CARTESIAN_POINT('Ctrl Pts',(-16.2820039372485,38.5625483697549,7.71067864538824));
#62467=CARTESIAN_POINT('Ctrl Pts',(-16.2773352205106,38.5579512520697,7.77235620365296));
#62468=CARTESIAN_POINT('Ctrl Pts',(-16.2760359524258,38.5533541343845,7.83420390838896));
#62469=CARTESIAN_POINT('Ctrl Pts',(-16.2747141333794,38.5486772260651,7.89712508305084));
#62470=CARTESIAN_POINT('Ctrl Pts',(-16.2768800061052,38.5440003177458,7.96022185310059));
#62471=CARTESIAN_POINT('Ctrl Pts',(-16.2825482745709,38.5393234094264,8.0230766978926));
#62472=CARTESIAN_POINT('Ctrl Pts',(-16.2881045063467,38.5347389429754,8.08468917937825));
#62473=CARTESIAN_POINT('Ctrl Pts',(-16.2970258922303,38.5301544765243,8.14606868051974));
#62474=CARTESIAN_POINT('Ctrl Pts',(-16.3092737966711,38.5255700100732,8.20682159834258));
#62475=CARTESIAN_POINT('Ctrl Pts',(-16.3215142115988,38.5209883469932,8.26753736615562));
#62476=CARTESIAN_POINT('Ctrl Pts',(-16.3370770112835,38.5164066839133,8.32762681238334));
#62477=CARTESIAN_POINT('Ctrl Pts',(-16.3558720955259,38.5118250208333,8.38670435019317));
#62478=CARTESIAN_POINT('Ctrl Pts',(-16.3746625909961,38.5072444763548,8.44576746437193));
#62479=CARTESIAN_POINT('Ctrl Pts',(-16.3966836501738,38.5026639318762,8.50381867567267));
#62480=CARTESIAN_POINT('Ctrl Pts',(-16.4217952812562,38.4980833873977,8.5604874293457));
#62481=CARTESIAN_POINT('Ctrl Pts',(-16.4478245104311,38.4933354663412,8.61922690236418));
#62482=CARTESIAN_POINT('Ctrl Pts',(-16.4771743701782,38.4885875452847,8.67648037150759));
#62483=CARTESIAN_POINT('Ctrl Pts',(-16.5096353933687,38.4838396242283,8.73186005776232));
#62484=CARTESIAN_POINT('Ctrl Pts',(-16.5409917605711,38.4792532760032,8.7853551607221));
#62485=CARTESIAN_POINT('Ctrl Pts',(-16.5752505814897,38.4746669277781,8.83710156953606));
#62486=CARTESIAN_POINT('Ctrl Pts',(-16.6121786835575,38.470080579553,8.88677907230902));
#62487=CARTESIAN_POINT('Ctrl Pts',(-16.6510582002527,38.4652518720808,8.93908171420726));
#62488=CARTESIAN_POINT('Ctrl Pts',(-16.6928965253649,38.4604231646087,8.9890902262784));
#62489=CARTESIAN_POINT('Ctrl Pts',(-16.7373752360294,38.4555944571365,9.03647268787872));
#62490=CARTESIAN_POINT('Ctrl Pts',(-16.7818539466939,38.4507657496644,9.08385514947904));
#62491=CARTESIAN_POINT('Ctrl Pts',(-16.8289725182177,38.4459370421923,9.12861116928819));
#62492=CARTESIAN_POINT('Ctrl Pts',(-16.8783723022766,38.4411083347201,9.17045809283064));
#62493=CARTESIAN_POINT('Ctrl Pts',(-16.9254028216628,38.4365112170463,9.2102979946927));
#62494=CARTESIAN_POINT('Ctrl Pts',(-16.9746939146925,38.4319140993725,9.2476651759781));
#62495=CARTESIAN_POINT('Ctrl Pts',(-17.0259550395338,38.4273169816987,9.28229354208289));
#62496=CARTESIAN_POINT('Ctrl Pts',(-17.0781058867199,38.4226400733779,9.31752294125477));
#62497=CARTESIAN_POINT('Ctrl Pts',(-17.1322954609214,38.4179631650572,9.34991712971022));
#62498=CARTESIAN_POINT('Ctrl Pts',(-17.1881809263176,38.4132862567364,9.37923735381575));
#62499=CARTESIAN_POINT('Ctrl Pts',(-17.2429617821702,38.408701790297,9.40797804621053));
#62500=CARTESIAN_POINT('Ctrl Pts',(-17.2993716261166,38.4041173238577,9.43376493771716));
#62501=CARTESIAN_POINT('Ctrl Pts',(-17.3570587952702,38.3995328574183,9.45641706087959));
#62502=CARTESIAN_POINT('Ctrl Pts',(-17.4147106890981,38.3949511943502,9.4790553324172));
#62503=CARTESIAN_POINT('Ctrl Pts',(-17.4736378865083,38.390369531282,9.4985624508343));
#62504=CARTESIAN_POINT('Ctrl Pts',(-17.533467553412,38.3857878682138,9.5148050370011));
#62505=CARTESIAN_POINT('Ctrl Pts',(-17.5932826130535,38.3812073237471,9.53104365758143));
#62506=CARTESIAN_POINT('Ctrl Pts',(-17.6539992137182,38.3766267792804,9.54401919480753));
#62507=CARTESIAN_POINT('Ctrl Pts',(-17.7152300980239,38.3720462348137,9.55364834054133));
#62508=CARTESIAN_POINT('Ctrl Pts',(-17.778698405713,38.3672983137459,9.56362934263113));
#62509=CARTESIAN_POINT('Ctrl Pts',(-17.8427187439572,38.3625503926781,9.57001450583138));
#62510=CARTESIAN_POINT('Ctrl Pts',(-17.9068517104591,38.3578024716103,9.57276955673316));
#62511=CARTESIAN_POINT('Ctrl Pts',(-17.9688022172439,38.3532161233971,9.57543085261408));
#62512=CARTESIAN_POINT('Ctrl Pts',(-18.0308572821878,38.3486297751839,9.57470522713874));
#62513=CARTESIAN_POINT('Ctrl Pts',(-18.0926214200226,38.3440434269707,9.57061496269793));
#62514=CARTESIAN_POINT('Ctrl Pts',(-18.1576493990214,38.3392147194756,9.56630855384191));
#62515=CARTESIAN_POINT('Ctrl Pts',(-18.2223542086077,38.3343860119805,9.55827211271781));
#62516=CARTESIAN_POINT('Ctrl Pts',(-18.2862842989164,38.3295573044854,9.54659320165545));
#62517=CARTESIAN_POINT('Ctrl Pts',(-18.3502143892252,38.3247285969903,9.53491429059309));
#62518=CARTESIAN_POINT('Ctrl Pts',(-18.4133691469486,38.3198998894952,9.51959313825781));
#62519=CARTESIAN_POINT('Ctrl Pts',(-18.4753166045076,38.3150711820001,9.50077781959992));
#62520=CARTESIAN_POINT('Ctrl Pts',(-18.5342929977205,38.3104740643271,9.48286490314912));
#62521=CARTESIAN_POINT('Ctrl Pts',(-18.5924175507923,38.3058769466541,9.46171178475844));
#62522=CARTESIAN_POINT('Ctrl Pts',(-18.6493091405794,38.3012798289812,9.43741829450116));
#62523=CARTESIAN_POINT('Ctrl Pts',(-18.7071881788355,38.2966029206603,9.41270315018474));
#62524=CARTESIAN_POINT('Ctrl Pts',(-18.7637905101237,38.2919260123394,9.38473764481648));
#62525=CARTESIAN_POINT('Ctrl Pts',(-18.8187296274891,38.2872491040185,9.35368037244278));
#62526=CARTESIAN_POINT('Ctrl Pts',(-18.8725828404318,38.2826646375801,9.32323696558139));
#62527=CARTESIAN_POINT('Ctrl Pts',(-18.9248375251718,38.2780801711417,9.2898231632124));
#62528=CARTESIAN_POINT('Ctrl Pts',(-18.9751509413837,38.2734957047033,9.25363631040213));
#62529=CARTESIAN_POINT('Ctrl Pts',(-19.0254335912709,38.2689140416361,9.21747158561546));
#62530=CARTESIAN_POINT('Ctrl Pts',(-19.0737769139927,38.2643323785689,9.17853746933835));
#62531=CARTESIAN_POINT('Ctrl Pts',(-19.1198666738557,38.2597507155017,9.13707489969342));
#62532=CARTESIAN_POINT('Ctrl Pts',(-19.1659451810197,38.255170171036,9.09562245303071));
#62533=CARTESIAN_POINT('Ctrl Pts',(-19.209770839256,38.2505896265704,9.05164311877771));
#62534=CARTESIAN_POINT('Ctrl Pts',(-19.2510636625165,38.2460090821047,9.00541710460519));
#62535=CARTESIAN_POINT('Ctrl Pts',(-19.2938653571655,38.241261161036,8.95750195646996));
#62536=CARTESIAN_POINT('Ctrl Pts',(-19.3339450943942,38.2365132399673,8.90717315076404));
#62537=CARTESIAN_POINT('Ctrl Pts',(-19.3710358126974,38.2317653188985,8.85478129723972));
#62538=CARTESIAN_POINT('Ctrl Pts',(-19.4068643252429,38.2271789706864,8.80417235065824));
#62539=CARTESIAN_POINT('Ctrl Pts',(-19.4399037766589,38.2225926224744,8.75163900632939));
#62540=CARTESIAN_POINT('Ctrl Pts',(-19.4699584385784,38.2180062742623,8.69752564123957));
#62541=CARTESIAN_POINT('Ctrl Pts',(-19.5016012979122,38.2131775667652,8.64055272954281));
#62542=CARTESIAN_POINT('Ctrl Pts',(-19.5299348738889,38.2083488592682,8.58182875448926));
#62543=CARTESIAN_POINT('Ctrl Pts',(-19.5547878867937,38.2035201517712,8.52178059744654));
#62544=CARTESIAN_POINT('Ctrl Pts',(-19.5796408996986,38.1986914442742,8.46173244040382));
#62545=CARTESIAN_POINT('Ctrl Pts',(-19.6010132090966,38.1938627367771,8.40036074067821));
#62546=CARTESIAN_POINT('Ctrl Pts',(-19.6187949975821,38.1890340292801,8.33810873896993));
#62547=CARTESIAN_POINT('Ctrl Pts',(-19.6403677510782,38.1831758718387,8.2625850036274));
#62548=CARTESIAN_POINT('Ctrl Pts',(-19.6567316249322,38.1773177143972,8.18551169491221));
#62549=CARTESIAN_POINT('Ctrl Pts',(-19.6677069478144,38.1714595569558,8.10752914326218));
#62550=CARTESIAN_POINT('Ctrl Pts',(-19.6786822706967,38.1656013995144,8.02954659161215));
#62551=CARTESIAN_POINT('Ctrl Pts',(-19.6842688386404,38.1597432420729,7.95065458203133));
#62552=CARTESIAN_POINT('Ctrl Pts',(-19.6843393239652,38.1538850846314,7.87151802034673));
#62553=CARTESIAN_POINT('',(-19.6843398591675,37.3601350845258,7.86930714147356));
#62554=CARTESIAN_POINT('Ctrl Pts',(-19.684339323966,38.1538850845701,7.87151801951866));
#62555=CARTESIAN_POINT('Ctrl Pts',(-19.6843939994145,38.1493409108528,7.81013177524482));
#62556=CARTESIAN_POINT('Ctrl Pts',(-19.6811279138394,38.1447967371355,7.74867522821752));
#62557=CARTESIAN_POINT('Ctrl Pts',(-19.6745449565224,38.1402525634182,7.6875384261698));
#62558=CARTESIAN_POINT('Ctrl Pts',(-19.6679653226271,38.1357106838378,7.62643248918267));
#62559=CARTESIAN_POINT('Ctrl Pts',(-19.6580721916101,38.1311688042574,7.56564649212944));
#62560=CARTESIAN_POINT('Ctrl Pts',(-19.6449214208484,38.1266269246771,7.5055668813074));
#62561=CARTESIAN_POINT('Ctrl Pts',(-19.6317722530837,38.1220855987235,7.44549459381499));
#62562=CARTESIAN_POINT('Ctrl Pts',(-19.6153663460452,38.1175442727699,7.38612902791419));
#62563=CARTESIAN_POINT('Ctrl Pts',(-19.5958105189662,38.1130029468163,7.32784577618699));
#62564=CARTESIAN_POINT('Ctrl Pts',(-19.5762357963367,38.1084572328687,7.2695062090652));
#62565=CARTESIAN_POINT('Ctrl Pts',(-19.5535052420422,38.103911518921,7.21225153699297));
#62566=CARTESIAN_POINT('Ctrl Pts',(-19.5277749423548,38.0993658049733,7.15644021734786));
#62567=CARTESIAN_POINT('Ctrl Pts',(-19.5020316447147,38.0948177947067,7.10060070398162));
#62568=CARTESIAN_POINT('Ctrl Pts',(-19.473285828702,38.0902697844401,7.04620645300395));
#62569=CARTESIAN_POINT('Ctrl Pts',(-19.4417395089391,38.0857217741735,6.99359116640328));
#62570=CARTESIAN_POINT('Ctrl Pts',(-19.4101351427099,38.0811653953895,6.9408790656105));
#62571=CARTESIAN_POINT('Ctrl Pts',(-19.3757202766866,38.0766090166055,6.88995289366633));
#62572=CARTESIAN_POINT('Ctrl Pts',(-19.3387395567511,38.0720526378215,6.84111630758394));
#62573=CARTESIAN_POINT('Ctrl Pts',(-19.3142399422629,38.0690340507344,6.8087622178305));
#62574=CARTESIAN_POINT('Ctrl Pts',(-19.2886150194716,38.0660154636472,6.77732458050104));
#62575=CARTESIAN_POINT('Ctrl Pts',(-19.2619447992417,38.0629968765601,6.74688274552598));
#62576=CARTESIAN_POINT('Ctrl Pts',(-19.2213277366001,38.0583997588854,6.70052175159917));
#62577=CARTESIAN_POINT('Ctrl Pts',(-19.178109068014,38.0538026412107,6.65627172587807));
#62578=CARTESIAN_POINT('Ctrl Pts',(-19.1325367588251,38.049205523536,6.61443882858826));
#62579=CARTESIAN_POINT('Ctrl Pts',(-19.0861734661884,38.0445286152154,6.57187985158207));
#62580=CARTESIAN_POINT('Ctrl Pts',(-19.037374329153,38.0398517068947,6.53182317146351));
#62581=CARTESIAN_POINT('Ctrl Pts',(-18.9864430772941,38.035174798574,6.49455564715733));
#62582=CARTESIAN_POINT('Ctrl Pts',(-18.9365185119837,38.0305903321338,6.45802473768087));
#62583=CARTESIAN_POINT('Ctrl Pts',(-18.8845457805321,38.0260058656936,6.4241740441216));
#62584=CARTESIAN_POINT('Ctrl Pts',(-18.8308458937871,38.0214213992534,6.39323458172068));
#62585=CARTESIAN_POINT('Ctrl Pts',(-18.7771788441709,38.0168397361843,6.36231403859829));
#62586=CARTESIAN_POINT('Ctrl Pts',(-18.721787173621,38.0122580731153,6.33430145038162));
#62587=CARTESIAN_POINT('Ctrl Pts',(-18.6650198733706,38.0076764100463,6.30938390092651));
#62588=CARTESIAN_POINT('Ctrl Pts',(-18.6082664327135,38.0030958655787,6.28447243502831));
#62589=CARTESIAN_POINT('Ctrl Pts',(-18.5501384950162,37.9985153211112,6.26265471234632));
#62590=CARTESIAN_POINT('Ctrl Pts',(-18.4910067256778,37.9939347766437,6.24407043144173));
#62591=CARTESIAN_POINT('Ctrl Pts',(-18.4297142362459,37.9891868555767,6.22480706669403));
#62592=CARTESIAN_POINT('Ctrl Pts',(-18.3673436697886,37.9844389345097,6.20901825874842));
#62593=CARTESIAN_POINT('Ctrl Pts',(-18.3043245188214,37.9796910134428,6.19680292789783));
#62594=CARTESIAN_POINT('Ctrl Pts',(-18.2434499241491,37.9751046652287,6.18500328758365));
#62595=CARTESIAN_POINT('Ctrl Pts',(-18.1819707144308,37.9705183170147,6.17653780523465));
#62596=CARTESIAN_POINT('Ctrl Pts',(-18.1202813180055,37.9659319688007,6.17144296904147));
#62597=CARTESIAN_POINT('Ctrl Pts',(-18.0553320300569,37.9611032613073,6.1660789032192));
#62598=CARTESIAN_POINT('Ctrl Pts',(-17.9901503705743,37.9562745538138,6.16445162514072));
#62599=CARTESIAN_POINT('Ctrl Pts',(-17.925195875559,37.9514458463204,6.16654135842861));
#62600=CARTESIAN_POINT('Ctrl Pts',(-17.8602413805436,37.946617138827,6.16863109171649));
#62601=CARTESIAN_POINT('Ctrl Pts',(-17.7955146903895,37.9417884313335,6.17443770098243));
#62602=CARTESIAN_POINT('Ctrl Pts',(-17.7314649292784,37.9369597238401,6.18387866562889));
#62603=CARTESIAN_POINT('Ctrl Pts',(-17.6704870611287,37.9323626061653,6.19286683182079));
#62604=CARTESIAN_POINT('Ctrl Pts',(-17.6098721581796,37.9277654884906,6.20518558302436));
#62605=CARTESIAN_POINT('Ctrl Pts',(-17.5500119205432,37.9231683708158,6.22079258820333));
#62606=CARTESIAN_POINT('Ctrl Pts',(-17.4891127086272,37.9184914624952,6.23667047899189));
#62607=CARTESIAN_POINT('Ctrl Pts',(-17.4289951475099,37.9138145541745,6.25595187527877));
#62608=CARTESIAN_POINT('Ctrl Pts',(-17.3700649579288,37.9091376458538,6.27853712576962));
#62609=CARTESIAN_POINT('Ctrl Pts',(-17.312299558667,37.9045531794136,6.3006759653238));
#62610=CARTESIAN_POINT('Ctrl Pts',(-17.2556755183872,37.8999687129733,6.32598905149395));
#62611=CARTESIAN_POINT('Ctrl Pts',(-17.2005610075826,37.895384246533,6.35433193188636));
#62612=CARTESIAN_POINT('Ctrl Pts',(-17.1454801989402,37.8908025834639,6.3826574807931));
#62613=CARTESIAN_POINT('Ctrl Pts',(-17.091907541249,37.8862209203948,6.41400891796747));
#62614=CARTESIAN_POINT('Ctrl Pts',(-17.0401894652584,37.8816392573258,6.44819445971376));
#62615=CARTESIAN_POINT('Ctrl Pts',(-16.9884840161057,37.8770587128582,6.48237165514613));
#62616=CARTESIAN_POINT('Ctrl Pts',(-16.9386326742921,37.8724781683906,6.51938130096242));
#62617=CARTESIAN_POINT('Ctrl Pts',(-16.8909538092563,37.867897623923,6.55898770790408));
#62618=CARTESIAN_POINT('Ctrl Pts',(-16.841532722014,37.8631497028561,6.60004136325739));
#62619=CARTESIAN_POINT('Ctrl Pts',(-16.7944464418052,37.8584017817892,6.64388490591297));
#62620=CARTESIAN_POINT('Ctrl Pts',(-16.7500109741647,37.8536538607223,6.69021110705151));
#62621=CARTESIAN_POINT('Ctrl Pts',(-16.7070876557729,37.8490675125082,6.73496081684271));
#62622=CARTESIAN_POINT('Ctrl Pts',(-16.6666379116302,37.8444811642942,6.78202647117671));
#62623=CARTESIAN_POINT('Ctrl Pts',(-16.6289062771767,37.8398948160801,6.83109644925646));
#62624=CARTESIAN_POINT('Ctrl Pts',(-16.5891807662652,37.8350661085868,6.88275946300789));
#62625=CARTESIAN_POINT('Ctrl Pts',(-16.5524689747073,37.8302374010934,6.93664397959055));
#62626=CARTESIAN_POINT('Ctrl Pts',(-16.5190034677509,37.8254086936001,6.99235316421911));
#62627=CARTESIAN_POINT('Ctrl Pts',(-16.4855379607946,37.8205799861068,7.04806234884768));
#62628=CARTESIAN_POINT('Ctrl Pts',(-16.4553189719353,37.8157512786134,7.10559559003678));
#62629=CARTESIAN_POINT('Ctrl Pts',(-16.4285207017313,37.8109225711201,7.16453077838679));
#62630=CARTESIAN_POINT('Ctrl Pts',(-16.4030077043532,37.806325453445,7.22063937399411));
#62631=CARTESIAN_POINT('Ctrl Pts',(-16.3804899460733,37.8017283357699,7.27824899691806));
#62632=CARTESIAN_POINT('Ctrl Pts',(-16.3611442575079,37.7971312180948,7.33700757922819));
#62633=CARTESIAN_POINT('Ctrl Pts',(-16.3414627922477,37.7924543097742,7.39678601474696));
#62634=CARTESIAN_POINT('Ctrl Pts',(-16.3250648660629,37.7877774014536,7.45775323064423));
#62635=CARTESIAN_POINT('Ctrl Pts',(-16.3120867506042,37.7831004931329,7.51951429688232));
#62636=CARTESIAN_POINT('Ctrl Pts',(-16.2993651553313,37.7785160266923,7.58005461884215));
#62637=CARTESIAN_POINT('Ctrl Pts',(-16.2899295218182,37.7739315602517,7.64135717253982));
#62638=CARTESIAN_POINT('Ctrl Pts',(-16.2838581174722,37.769347093811,7.70303428515065));
#62639=CARTESIAN_POINT('Ctrl Pts',(-16.2777904257503,37.7647654307416,7.76467368261133));
#62640=CARTESIAN_POINT('Ctrl Pts',(-16.2750829338365,37.7601837676721,7.82668667925809));
#62641=CARTESIAN_POINT('Ctrl Pts',(-16.275762352157,37.7556021046027,7.88867820319456));
#62642=CARTESIAN_POINT('Ctrl Pts',(-16.2764416045992,37.7510215601347,7.95065459205662));
#62643=CARTESIAN_POINT('Ctrl Pts',(-16.2805061201738,37.7464410156668,8.01260900979874));
#62644=CARTESIAN_POINT('Ctrl Pts',(-16.2879305028511,37.7418604711988,8.07414615455166));
#62645=CARTESIAN_POINT('Ctrl Pts',(-16.2956261781505,37.7371125501323,8.13793191364476));
#62646=CARTESIAN_POINT('Ctrl Pts',(-16.3069320119322,37.7323646290657,8.20126872867588));
#62647=CARTESIAN_POINT('Ctrl Pts',(-16.3217612174133,37.7276167079991,8.26372449190449));
#62648=CARTESIAN_POINT('Ctrl Pts',(-16.3360857816018,37.7230303597847,8.32405487106394));
#62649=CARTESIAN_POINT('Ctrl Pts',(-16.3536975343428,37.7184440115703,8.38356271747965));
#62650=CARTESIAN_POINT('Ctrl Pts',(-16.3744672442257,37.7138576633558,8.44187359244485));
#62651=CARTESIAN_POINT('Ctrl Pts',(-16.396334500928,37.7090289558632,8.50326582558571));
#62652=CARTESIAN_POINT('Ctrl Pts',(-16.4217024861552,37.7042002483706,8.56333047484713));
#62653=CARTESIAN_POINT('Ctrl Pts',(-16.4503638792474,37.699371540878,8.62165695213241));
#62654=CARTESIAN_POINT('Ctrl Pts',(-16.4790252723396,37.6945428333853,8.67998342941768));
#62655=CARTESIAN_POINT('Ctrl Pts',(-16.5109796861268,37.6897141258927,8.73657120696363));
#62656=CARTESIAN_POINT('Ctrl Pts',(-16.5459669156816,37.6848854184001,8.79104503075598));
#62657=CARTESIAN_POINT('Ctrl Pts',(-16.5792761214321,37.6802883007252,8.84290623348067));
#62658=CARTESIAN_POINT('Ctrl Pts',(-16.6154706772694,37.6756911830504,8.89306470453681));
#62659=CARTESIAN_POINT('Ctrl Pts',(-16.6543506546144,37.6710940653755,8.94118095981901));
#62660=CARTESIAN_POINT('Ctrl Pts',(-16.6939054588227,37.6664171570549,8.99013235297523));
#62661=CARTESIAN_POINT('Ctrl Pts',(-16.7362395867746,37.6617402487342,9.03696946441502));
#62662=CARTESIAN_POINT('Ctrl Pts',(-16.7810951033588,37.6570633404136,9.08136364664361));
#62663=CARTESIAN_POINT('Ctrl Pts',(-16.8250640239252,37.6524788739732,9.12488035140286));
#62664=CARTESIAN_POINT('Ctrl Pts',(-16.871455187435,37.6478944075328,9.1660494443908));
#62665=CARTESIAN_POINT('Ctrl Pts',(-16.9199853038366,37.6433099410924,9.2045949496074));
#62666=CARTESIAN_POINT('Ctrl Pts',(-16.9684857443899,37.6387282780232,9.24311688450012));
#62667=CARTESIAN_POINT('Ctrl Pts',(-17.019122146548,37.634146614954,9.279018096759));
#62668=CARTESIAN_POINT('Ctrl Pts',(-17.0715770468266,37.6295649518848,9.31206191744591));
#62669=CARTESIAN_POINT('Ctrl Pts',(-17.1240191403734,37.6249844074171,9.34509767056718));
#62670=CARTESIAN_POINT('Ctrl Pts',(-17.178278420132,37.6204038629494,9.37527714578282));
#62671=CARTESIAN_POINT('Ctrl Pts',(-17.2340089748521,37.6158233184818,9.40240733031358));
#62672=CARTESIAN_POINT('Ctrl Pts',(-17.2917759666773,37.611075397415,9.43052887254254));
#62673=CARTESIAN_POINT('Ctrl Pts',(-17.3511233424126,37.6063274763481,9.45537365085896));
#62674=CARTESIAN_POINT('Ctrl Pts',(-17.4116409768806,37.6015795552813,9.4767802763411));
#62675=CARTESIAN_POINT('Ctrl Pts',(-17.4700991822432,37.5969932070672,9.49745842940434));
#62676=CARTESIAN_POINT('Ctrl Pts',(-17.5296487457302,37.592406858853,9.51492860707238));
#62677=CARTESIAN_POINT('Ctrl Pts',(-17.5899049813651,37.5878205106388,9.52909635405429));
#62678=CARTESIAN_POINT('Ctrl Pts',(-17.653345375101,37.5829918031457,9.54401277618743));
#62679=CARTESIAN_POINT('Ctrl Pts',(-17.7175685644248,37.5781630956526,9.55526794030782));
#62680=CARTESIAN_POINT('Ctrl Pts',(-17.7821171463219,37.5733343881595,9.56281340135887));
#62681=CARTESIAN_POINT('Ctrl Pts',(-17.8466657282189,37.5685056806663,9.57035886240993));
#62682=CARTESIAN_POINT('Ctrl Pts',(-17.9115390493107,37.5636769731732,9.57419465952163));
#62683=CARTESIAN_POINT('Ctrl Pts',(-17.976280718664,37.5588482656801,9.57433594181028));
#62684=CARTESIAN_POINT('Ctrl Pts',(-18.037917310428,37.554251148005,9.57447044805388));
#62685=CARTESIAN_POINT('Ctrl Pts',(-18.0996878045383,37.5496540303299,9.57125732671632));
#62686=CARTESIAN_POINT('Ctrl Pts',(-18.1611985492709,37.5450569126547,9.56468047765416));
#62687=CARTESIAN_POINT('Ctrl Pts',(-18.2237769155815,37.5403800043341,9.55798947640599));
#62688=CARTESIAN_POINT('Ctrl Pts',(-18.2860858994534,37.5357030960135,9.54781677144421));
#62689=CARTESIAN_POINT('Ctrl Pts',(-18.3477095004604,37.5310261876929,9.53420087695902));
#62690=CARTESIAN_POINT('Ctrl Pts',(-18.4081150742713,37.5264417212523,9.52085410874218));
#62691=CARTESIAN_POINT('Ctrl Pts',(-18.4678615913966,37.5218572548116,9.50419914068351));
#62692=CARTESIAN_POINT('Ctrl Pts',(-18.5265635584022,37.517272788371,9.48432435161796));
#62693=CARTESIAN_POINT('Ctrl Pts',(-18.5852296295396,37.5126911253015,9.46446171585568));
#62694=CARTESIAN_POINT('Ctrl Pts',(-18.6428519358873,37.5081094622321,9.44138332603462));
#62695=CARTESIAN_POINT('Ctrl Pts',(-18.6990594801508,37.5035277991626,9.41522758828767));
#62696=CARTESIAN_POINT('Ctrl Pts',(-18.7552533014838,37.4989472546947,9.3890782363982));
#62697=CARTESIAN_POINT('Ctrl Pts',(-18.8100325850791,37.4943667102267,9.3598532427556));
#62698=CARTESIAN_POINT('Ctrl Pts',(-18.8630475886996,37.4897861657588,9.32773858825642));
#62699=CARTESIAN_POINT('Ctrl Pts',(-18.9179998011045,37.4850382446922,9.29445043971674));
#62700=CARTESIAN_POINT('Ctrl Pts',(-18.9710557700258,37.4802903236257,9.25805760831249));
#62701=CARTESIAN_POINT('Ctrl Pts',(-19.0218575044375,37.4755424025591,9.21881717665783));
#62702=CARTESIAN_POINT('Ctrl Pts',(-19.0709304440763,37.4709560543447,9.18091210596905));
#62703=CARTESIAN_POINT('Ctrl Pts',(-19.1178997652097,37.4663697061303,9.14035054174966));
#62704=CARTESIAN_POINT('Ctrl Pts',(-19.1624775100696,37.4617833579158,9.09740448662189));
#62705=CARTESIAN_POINT('Ctrl Pts',(-19.209410904689,37.4569546504232,9.05218900613965));
#62706=CARTESIAN_POINT('Ctrl Pts',(-19.2536925069757,37.4521259429306,9.00433050152082));
#62707=CARTESIAN_POINT('Ctrl Pts',(-19.2950335873058,37.447297235438,8.9541870225462));
#62708=CARTESIAN_POINT('Ctrl Pts',(-19.3363746676359,37.4424685279453,8.90404354357157));
#62709=CARTESIAN_POINT('Ctrl Pts',(-19.3747749045952,37.4376398204527,8.85161566044052));
#62710=CARTESIAN_POINT('Ctrl Pts',(-19.4099995504222,37.4328111129601,8.79729505627508));
#62711=CARTESIAN_POINT('Ctrl Pts',(-19.4442592518619,37.4281146831408,8.74446251141809));
#62712=CARTESIAN_POINT('Ctrl Pts',(-19.4756515793317,37.4234182533215,8.68963005408069));
#62713=CARTESIAN_POINT('Ctrl Pts',(-19.5039428546648,37.4187218235022,8.63313367853616));
#62714=CARTESIAN_POINT('Ctrl Pts',(-19.5333533790022,37.4138395952578,8.57440221421144));
#62715=CARTESIAN_POINT('Ctrl Pts',(-19.5594119799198,37.4089573670135,8.51387279618993));
#62716=CARTESIAN_POINT('Ctrl Pts',(-19.5819054569772,37.4040751387692,8.45195682185774));
#62717=CARTESIAN_POINT('Ctrl Pts',(-19.6034658205024,37.3993954436072,8.3926093536465));
#62718=CARTESIAN_POINT('Ctrl Pts',(-19.6217508084192,37.3947157484452,8.33198859873641));
#62719=CARTESIAN_POINT('Ctrl Pts',(-19.6366201226328,37.3900360532833,8.27048046754878));
#62720=CARTESIAN_POINT('Ctrl Pts',(-19.6514743036184,37.3853611208759,8.20903493619342));
#62721=CARTESIAN_POINT('Ctrl Pts',(-19.6629196009608,37.3806861884685,8.14670428650603));
#62722=CARTESIAN_POINT('Ctrl Pts',(-19.6708654690599,37.3760112560611,8.08388969386272));
#62723=CARTESIAN_POINT('Ctrl Pts',(-19.678804960735,37.3713400752075,8.02112550886222));
#62724=CARTESIAN_POINT('Ctrl Pts',(-19.683250545557,37.3666688943539,7.95787862815727));
#62725=CARTESIAN_POINT('Ctrl Pts',(-19.6841630505933,37.3619977135002,7.89455875796057));
#62726=CARTESIAN_POINT('Ctrl Pts',(-19.6842843374322,37.3613768371902,7.88614251192121));
#62727=CARTESIAN_POINT('Ctrl Pts',(-19.6843432812367,37.3607559608802,7.87772498405695));
#62728=CARTESIAN_POINT('Ctrl Pts',(-19.6843398591677,37.3601350845702,7.86930714207592));
#62729=CARTESIAN_POINT('',(-19.6843396079794,36.5663850846257,7.86884402740817));
#62730=CARTESIAN_POINT('Ctrl Pts',(-19.6843398591675,37.3601350845258,7.86930714147356));
#62731=CARTESIAN_POINT('Ctrl Pts',(-19.684312342679,37.3551426892111,7.80162023799952));
#62732=CARTESIAN_POINT('Ctrl Pts',(-19.6802484007567,37.3501502938964,7.73406057782156));
#62733=CARTESIAN_POINT('Ctrl Pts',(-19.6722183804769,37.3451578985817,7.6670916749466));
#62734=CARTESIAN_POINT('Ctrl Pts',(-19.6641639652474,37.3401503365266,7.59991932264465));
#62735=CARTESIAN_POINT('Ctrl Pts',(-19.6521194773108,37.3351427744715,7.53334165648438));
#62736=CARTESIAN_POINT('Ctrl Pts',(-19.6362060715679,37.3301352124164,7.4678106365136));
#62737=CARTESIAN_POINT('Ctrl Pts',(-19.6202226848285,37.3251056290424,7.40199143649161));
#62738=CARTESIAN_POINT('Ctrl Pts',(-19.6003364347516,37.3200760456684,7.33722843146035));
#62739=CARTESIAN_POINT('Ctrl Pts',(-19.5767183878877,37.3150464622943,7.27395870496986));
#62740=CARTESIAN_POINT('Ctrl Pts',(-19.5637696453067,37.3122889616096,7.23927067990921));
#62741=CARTESIAN_POINT('Ctrl Pts',(-19.5497000125454,37.3095314609248,7.20503111778527));
#62742=CARTESIAN_POINT('Ctrl Pts',(-19.5345435224027,37.30677396024,7.1713088861623));
#62743=CARTESIAN_POINT('Ctrl Pts',(-19.5092756524411,37.3021768425653,7.1150894741849));
#62744=CARTESIAN_POINT('Ctrl Pts',(-19.4809022245421,37.2975797248906,7.06012706266653));
#62745=CARTESIAN_POINT('Ctrl Pts',(-19.4495707280332,37.2929826072159,7.00678698404857));
#62746=CARTESIAN_POINT('Ctrl Pts',(-19.4176954211366,37.2883056988952,6.95252109938666));
#62747=CARTESIAN_POINT('Ctrl Pts',(-19.38275851271,37.2836287905746,6.89993492413997));
#62748=CARTESIAN_POINT('Ctrl Pts',(-19.3449664635909,37.2789518822539,6.84939165745511));
#62749=CARTESIAN_POINT('Ctrl Pts',(-19.3079213968469,37.2743674158137,6.79984740856048));
#62750=CARTESIAN_POINT('Ctrl Pts',(-19.2681333488877,37.2697829493735,6.75226647216188));
#62751=CARTESIAN_POINT('Ctrl Pts',(-19.2258416508355,37.2651984829332,6.70696370794222));
#62752=CARTESIAN_POINT('Ctrl Pts',(-19.1835758138795,37.2606168198642,6.66168864606606));
#62753=CARTESIAN_POINT('Ctrl Pts',(-19.1388097091757,37.2560351567952,6.61868936543772));
#62754=CARTESIAN_POINT('Ctrl Pts',(-19.0918222818161,37.2514534937261,6.5782469085552));
#62755=CARTESIAN_POINT('Ctrl Pts',(-19.0448463263186,37.2468729492586,6.53781432559668));
#62756=CARTESIAN_POINT('Ctrl Pts',(-18.9956505104337,37.2422924047911,6.49993765911998));
#62757=CARTESIAN_POINT('Ctrl Pts',(-18.9445483741916,37.2377118603236,6.46485898592195));
#62758=CARTESIAN_POINT('Ctrl Pts',(-18.891578926793,37.2329639392566,6.42849851116655));
#62759=CARTESIAN_POINT('Ctrl Pts',(-18.8365615891362,37.2282160181896,6.39514485209127));
#62760=CARTESIAN_POINT('Ctrl Pts',(-18.7798780879788,37.2234680971227,6.3650183124133));
#62761=CARTESIAN_POINT('Ctrl Pts',(-18.7251235394868,37.2188817489087,6.33591698585419));
#62762=CARTESIAN_POINT('Ctrl Pts',(-18.6688149218315,37.2142954006947,6.30982681152079));
#62763=CARTESIAN_POINT('Ctrl Pts',(-18.6113187077245,37.2097090524807,6.28689813186988));
#62764=CARTESIAN_POINT('Ctrl Pts',(-18.5507841850613,37.2048803449873,6.26275781759838));
#62765=CARTESIAN_POINT('Ctrl Pts',(-18.4889336801542,37.2000516374938,6.24212260958859));
#62766=CARTESIAN_POINT('Ctrl Pts',(-18.4262123908774,37.1952229300004,6.22510810755617));
#62767=CARTESIAN_POINT('Ctrl Pts',(-18.3634911016007,37.190394222507,6.20809360552376));
#62768=CARTESIAN_POINT('Ctrl Pts',(-18.2998996799295,37.1855655150136,6.19469986745871));
#62769=CARTESIAN_POINT('Ctrl Pts',(-18.2358917336808,37.1807368075201,6.1849794493141));
#62770=CARTESIAN_POINT('Ctrl Pts',(-18.1749536748877,37.1761396898437,6.17572523250032));
#62771=CARTESIAN_POINT('Ctrl Pts',(-18.1133877947718,37.1715425721674,6.16976197005564));
#62772=CARTESIAN_POINT('Ctrl Pts',(-18.051581028338,37.166945454491,6.16716383877307));
#62773=CARTESIAN_POINT('Ctrl Pts',(-17.9887015023952,37.1622685461705,6.16452061258908));
#62774=CARTESIAN_POINT('Ctrl Pts',(-17.925573158648,37.1575916378501,6.16536062015343));
#62775=CARTESIAN_POINT('Ctrl Pts',(-17.8626131167544,37.1529147295296,6.16970733247424));
#62776=CARTESIAN_POINT('Ctrl Pts',(-17.800897517588,37.1483302630877,6.17396812943711));
#62777=CARTESIAN_POINT('Ctrl Pts',(-17.7393441601812,37.1437457966458,6.18159823189687));
#62778=CARTESIAN_POINT('Ctrl Pts',(-17.6783473722258,37.1391613302039,6.19256728070635));
#62779=CARTESIAN_POINT('Ctrl Pts',(-17.6173878834064,37.1345796671331,6.20352962201436));
#62780=CARTESIAN_POINT('Ctrl Pts',(-17.5569847891959,37.1299980040624,6.21782677128591));
#62781=CARTESIAN_POINT('Ctrl Pts',(-17.49752548396,37.1254163409917,6.23537674769628));
#62782=CARTESIAN_POINT('Ctrl Pts',(-17.4380806955638,37.1208357965224,6.25292243932408));
#62783=CARTESIAN_POINT('Ctrl Pts',(-17.3795797267511,37.1162552520532,6.27371923750358));
#62784=CARTESIAN_POINT('Ctrl Pts',(-17.3223959911261,37.111674707584,6.29763496505645));
#62785=CARTESIAN_POINT('Ctrl Pts',(-17.2631227180923,37.1069267865187,6.32242459157439));
#62786=CARTESIAN_POINT('Ctrl Pts',(-17.2052653691306,37.1021788654533,6.35056533045179));
#62787=CARTESIAN_POINT('Ctrl Pts',(-17.1492160376861,37.097430944388,6.38185590631751));
#62788=CARTESIAN_POINT('Ctrl Pts',(-17.0950740779267,37.0928445961723,6.41208165666479));
#62789=CARTESIAN_POINT('Ctrl Pts',(-17.0426194586066,37.0882582479567,6.44524595273187));
#62790=CARTESIAN_POINT('Ctrl Pts',(-16.992177218904,37.083671899741,6.48112239965223));
#62791=CARTESIAN_POINT('Ctrl Pts',(-16.9390694283006,37.0788431922509,6.51889468815235));
#62792=CARTESIAN_POINT('Ctrl Pts',(-16.8881931097297,37.0740144847607,6.55967332189239));
#62793=CARTESIAN_POINT('Ctrl Pts',(-16.8398867992758,37.0691857772705,6.60314692046219));
#62794=CARTESIAN_POINT('Ctrl Pts',(-16.7915804888219,37.0643570697804,6.64662051903199));
#62795=CARTESIAN_POINT('Ctrl Pts',(-16.7458445887407,37.0595283622902,6.69278856607415));
#62796=CARTESIAN_POINT('Ctrl Pts',(-16.7029692247785,37.0546996548001,6.74129842972684));
#62797=CARTESIAN_POINT('Ctrl Pts',(-16.6621502077228,37.0501025371273,6.78748171002631));
#62798=CARTESIAN_POINT('Ctrl Pts',(-16.6237558808871,37.0455054194545,6.83597700623768));
#62799=CARTESIAN_POINT('Ctrl Pts',(-16.5880583831769,37.0409083017818,6.88649943011922));
#62800=CARTESIAN_POINT('Ctrl Pts',(-16.5517412958278,37.0362313934609,6.9378987549708));
#62801=CARTESIAN_POINT('Ctrl Pts',(-16.5182159688866,37.03155448514,6.99139591238914));
#62802=CARTESIAN_POINT('Ctrl Pts',(-16.4877283047894,37.0268775768191,7.04665315736733));
#62803=CARTESIAN_POINT('Ctrl Pts',(-16.4578432475579,37.0222931103807,7.10081820993945));
#62804=CARTESIAN_POINT('Ctrl Pts',(-16.4308771215619,37.0177086439424,7.15667393762248));
#62805=CARTESIAN_POINT('Ctrl Pts',(-16.407018241228,37.0131241775041,7.21387255645679));
#62806=CARTESIAN_POINT('Ctrl Pts',(-16.383173950443,37.0085425144369,7.2710361987107));
#62807=CARTESIAN_POINT('Ctrl Pts',(-16.3624333333595,37.0039608513698,7.32954063499695));
#62808=CARTESIAN_POINT('Ctrl Pts',(-16.3449375712924,36.9993791883026,7.3890159152023));
#62809=CARTESIAN_POINT('Ctrl Pts',(-16.3274460807714,36.994798643837,7.448476674668));
#62810=CARTESIAN_POINT('Ctrl Pts',(-16.3131980161933,36.9902180993713,7.50890731935247));
#62811=CARTESIAN_POINT('Ctrl Pts',(-16.3022848018994,36.9856375549056,7.56992242725872));
#62812=CARTESIAN_POINT('Ctrl Pts',(-16.2909728103965,36.9808896338368,7.63316707394078));
#62813=CARTESIAN_POINT('Ctrl Pts',(-16.2832442686416,36.976141712768,7.69703916222988));
#62814=CARTESIAN_POINT('Ctrl Pts',(-16.2791426724025,36.9713937916992,7.76110010671339));
#62815=CARTESIAN_POINT('Ctrl Pts',(-16.2751806544359,36.966807443487,7.82298104237933));
#62816=CARTESIAN_POINT('Ctrl Pts',(-16.2746026142157,36.9622210952748,7.88503765754329));
#62817=CARTESIAN_POINT('Ctrl Pts',(-16.2773945816838,36.9576347470626,7.94687408614226));
#62818=CARTESIAN_POINT('Ctrl Pts',(-16.2803340868458,36.9528060395655,8.01197817605266));
#62819=CARTESIAN_POINT('Ctrl Pts',(-16.2870095896517,36.9479773320684,8.07683751952399));
#62820=CARTESIAN_POINT('Ctrl Pts',(-16.2973430321799,36.9431486245714,8.14099882702023));
#62821=CARTESIAN_POINT('Ctrl Pts',(-16.307676474708,36.9383199170743,8.20516013451646));
#62822=CARTESIAN_POINT('Ctrl Pts',(-16.3216676412264,36.9334912095772,8.26862278806169));
#62823=CARTESIAN_POINT('Ctrl Pts',(-16.3391775632061,36.9286625020801,8.33095180497942));
#62824=CARTESIAN_POINT('Ctrl Pts',(-16.3558476911547,36.9240653844061,8.39029145755644));
#62825=CARTESIAN_POINT('Ctrl Pts',(-16.3757751995548,36.9194682667322,8.44884752041912));
#62826=CARTESIAN_POINT('Ctrl Pts',(-16.3988682860906,36.9148711490582,8.50623685752226));
#62827=CARTESIAN_POINT('Ctrl Pts',(-16.4223621916703,36.9101942407375,8.56462228231588));
#62828=CARTESIAN_POINT('Ctrl Pts',(-16.4491325591648,36.9055173324167,8.62179955771093));
#62829=CARTESIAN_POINT('Ctrl Pts',(-16.4790289483411,36.900840424096,8.67737893066517));
#62830=CARTESIAN_POINT('Ctrl Pts',(-16.5083344175611,36.8962559576565,8.73185974417645));
#62831=CARTESIAN_POINT('Ctrl Pts',(-16.5406432049823,36.8916714912171,8.78480477720931));
#62832=CARTESIAN_POINT('Ctrl Pts',(-16.5757652085565,36.8870870247777,8.83586721970446));
#62833=CARTESIAN_POINT('Ctrl Pts',(-16.6108657352555,36.8825053617095,8.88689843785039));
#62834=CARTESIAN_POINT('Ctrl Pts',(-16.6487757791845,36.8779236986413,8.93604892953435));
#62835=CARTESIAN_POINT('Ctrl Pts',(-16.6892610560999,36.8733420355731,8.98299946734022));
#62836=CARTESIAN_POINT('Ctrl Pts',(-16.7297364486367,36.8687614911064,9.02993854229032));
#62837=CARTESIAN_POINT('Ctrl Pts',(-16.7727854937313,36.8641809466397,9.07467834424582));
#62838=CARTESIAN_POINT('Ctrl Pts',(-16.8181339268211,36.859600402173,9.11693306299734));
#62839=CARTESIAN_POINT('Ctrl Pts',(-16.8651394263687,36.8548524811053,9.16073180151654));
#62840=CARTESIAN_POINT('Ctrl Pts',(-16.9146152273539,36.8501045600376,9.20185988358829));
#62841=CARTESIAN_POINT('Ctrl Pts',(-16.9662164071788,36.8453566389698,9.24004294185492));
#62842=CARTESIAN_POINT('Ctrl Pts',(-17.0160615868918,36.8407702907567,9.276926621797));
#62843=CARTESIAN_POINT('Ctrl Pts',(-17.0678893257283,36.8361839425435,9.31106227917652));
#62844=CARTESIAN_POINT('Ctrl Pts',(-17.1213594340831,36.8315975943304,9.34224699495769));
#62845=CARTESIAN_POINT('Ctrl Pts',(-17.1776550969888,36.8267688868354,9.37507962427978));
#62846=CARTESIAN_POINT('Ctrl Pts',(-17.2357709504644,36.8219401793403,9.40464048260112));
#62847=CARTESIAN_POINT('Ctrl Pts',(-17.2952838051689,36.8171114718453,9.43074936108783));
#62848=CARTESIAN_POINT('Ctrl Pts',(-17.3547966598735,36.8122827643502,9.45685823957453));
#62849=CARTESIAN_POINT('Ctrl Pts',(-17.4157058795918,36.8074540568551,9.47951498439359));
#62850=CARTESIAN_POINT('Ctrl Pts',(-17.4775706282056,36.8026253493601,9.49860049182058));
#62851=CARTESIAN_POINT('Ctrl Pts',(-17.5364682794436,36.7980282316744,9.51677063855719));
#62852=CARTESIAN_POINT('Ctrl Pts',(-17.596473846165,36.7934311139887,9.5317789719462));
#62853=CARTESIAN_POINT('Ctrl Pts',(-17.6572156305096,36.788833996303,9.54349487194097));
#62854=CARTESIAN_POINT('Ctrl Pts',(-17.7190116896824,36.7841570879837,9.55541412089208));
#62855=CARTESIAN_POINT('Ctrl Pts',(-17.7815692878552,36.7794801796644,9.56392530793355));
#62856=CARTESIAN_POINT('Ctrl Pts',(-17.8444793712416,36.7748032713451,9.56894349369864));
#62857=CARTESIAN_POINT('Ctrl Pts',(-17.9061459995017,36.7702188048939,9.5738624920445));
#62858=CARTESIAN_POINT('Ctrl Pts',(-17.9681507735409,36.7656343384426,9.57542527236441));
#62859=CARTESIAN_POINT('Ctrl Pts',(-18.0300992146251,36.7610498719913,9.57360350560039));
#62860=CARTESIAN_POINT('Ctrl Pts',(-18.0920097746435,36.7564682089113,9.57178285283481));
#62861=CARTESIAN_POINT('Ctrl Pts',(-18.1538635622118,36.7518865458312,9.56658177168102));
#62862=CARTESIAN_POINT('Ctrl Pts',(-18.2152653164343,36.7473048827511,9.55802401241305));
#62863=CARTESIAN_POINT('Ctrl Pts',(-18.2766520795728,36.7427243382726,9.54946834250051));
#62864=CARTESIAN_POINT('Ctrl Pts',(-18.3375865244753,36.738143793794,9.5375576915874));
#62865=CARTESIAN_POINT('Ctrl Pts',(-18.3976797888509,36.7335632493155,9.52236752255226));
#62866=CARTESIAN_POINT('Ctrl Pts',(-18.4599689067945,36.7288153282592,9.50662229319178));
#62867=CARTESIAN_POINT('Ctrl Pts',(-18.5213535991595,36.7240674072029,9.48735331450911));
#62868=CARTESIAN_POINT('Ctrl Pts',(-18.5814163041024,36.7193194861466,9.4647016224861));
#62869=CARTESIAN_POINT('Ctrl Pts',(-18.63943506156,36.7147331379218,9.44282077268526));
#62870=CARTESIAN_POINT('Ctrl Pts',(-18.696219912393,36.710146789697,9.41778403264034));
#62871=CARTESIAN_POINT('Ctrl Pts',(-18.7514158934743,36.7055604414722,9.38976720417808));
#62872=CARTESIAN_POINT('Ctrl Pts',(-18.8095286300586,36.7007317340002,9.36026986505195));
#62873=CARTESIAN_POINT('Ctrl Pts',(-18.8658793526181,36.6959030265282,9.32746906024655));
#62874=CARTESIAN_POINT('Ctrl Pts',(-18.9200871732797,36.6910743190561,9.29162264410602));
#62875=CARTESIAN_POINT('Ctrl Pts',(-18.9742949939413,36.6862456115841,9.25577622796548));
#62876=CARTESIAN_POINT('Ctrl Pts',(-19.0263594384661,36.6814169041121,9.21688465163489));
#62877=CARTESIAN_POINT('Ctrl Pts',(-19.0759413917834,36.6765881966401,9.17525373065001));
#62878=CARTESIAN_POINT('Ctrl Pts',(-19.1230907030207,36.6719964003061,9.13566534981216));
#62879=CARTESIAN_POINT('Ctrl Pts',(-19.1682034839025,36.6674046039722,9.09342518089385));
#62880=CARTESIAN_POINT('Ctrl Pts',(-19.2109609351148,36.6628128076383,9.04877479266453));
#62881=CARTESIAN_POINT('Ctrl Pts',(-19.2530959184682,36.6582878591999,9.00477442988744));
#62882=CARTESIAN_POINT('Ctrl Pts',(-19.2929432957966,36.6537629107615,8.95843392556737));
#62883=CARTESIAN_POINT('Ctrl Pts',(-19.3302301661075,36.6492379623231,8.91002564109415));
#62884=CARTESIAN_POINT('Ctrl Pts',(-19.3674809633399,36.6447173915334,8.86166418908046));
#62885=CARTESIAN_POINT('Ctrl Pts',(-19.4021758408854,36.6401968207438,8.81123933213499));
#62886=CARTESIAN_POINT('Ctrl Pts',(-19.4340805176135,36.6356762499541,8.75905831299012));
#62887=CARTESIAN_POINT('Ctrl Pts',(-19.4659668223746,36.6311582822868,8.70690734172728));
#62888=CARTESIAN_POINT('Ctrl Pts',(-19.4950658374982,36.6266403146195,8.65300265920719));
#62889=CARTESIAN_POINT('Ctrl Pts',(-19.5211864923278,36.6221223469522,8.59768058340608));
#62890=CARTESIAN_POINT('Ctrl Pts',(-19.5480402662957,36.6174775750916,8.54080580255989));
#62891=CARTESIAN_POINT('Ctrl Pts',(-19.5717456588421,36.6128328032311,8.48243335371606));
#62892=CARTESIAN_POINT('Ctrl Pts',(-19.5921466851392,36.6081880313705,8.42295379661841));
#62893=CARTESIAN_POINT('Ctrl Pts',(-19.6120017637458,36.6036675572994,8.36506595977829));
#62894=CARTESIAN_POINT('Ctrl Pts',(-19.628727039104,36.5991470832283,8.30613007263316));
#62895=CARTESIAN_POINT('Ctrl Pts',(-19.6422292726584,36.5946266091571,8.24652181970979));
#62896=CARTESIAN_POINT('Ctrl Pts',(-19.6562884050324,36.5899196884019,8.18445502794113));
#62897=CARTESIAN_POINT('Ctrl Pts',(-19.6668526780841,36.5852127676466,8.12165980555281));
#62898=CARTESIAN_POINT('Ctrl Pts',(-19.6738761962583,36.5805058468914,8.0585689989087));
#62899=CARTESIAN_POINT('Ctrl Pts',(-19.6808997144325,36.5757989261361,7.9954781922646));
#62900=CARTESIAN_POINT('Ctrl Pts',(-19.6843825063727,36.5710920053809,7.93209243945));
#62901=CARTESIAN_POINT('Ctrl Pts',(-19.6843396079794,36.5663850846257,7.86884402740818));
#62902=CARTESIAN_POINT('',(-19.6843394141537,35.7726350845326,7.87141313913839));
#62903=CARTESIAN_POINT('Ctrl Pts',(-19.6843396079789,36.5663850845702,7.86884402666309));
#62904=CARTESIAN_POINT('Ctrl Pts',(-19.6842915046734,36.5611070710201,7.79792165657743));
#62905=CARTESIAN_POINT('Ctrl Pts',(-19.6798165048226,36.5558290574701,7.72714864521007));
#62906=CARTESIAN_POINT('Ctrl Pts',(-19.6709699394029,36.5505510439201,7.65693780336342));
#62907=CARTESIAN_POINT('Ctrl Pts',(-19.6632646347729,36.5459539262461,7.59578458749917));
#62908=CARTESIAN_POINT('Ctrl Pts',(-19.6522218556924,36.5413568085721,7.53492429571754));
#62909=CARTESIAN_POINT('Ctrl Pts',(-19.63787569595,36.5367596908982,7.47474943089457));
#62910=CARTESIAN_POINT('Ctrl Pts',(-19.6232805346711,36.5320827825774,7.41353013090068));
#62911=CARTESIAN_POINT('Ctrl Pts',(-19.6052661997884,36.5274058742567,7.35302081646679));
#62912=CARTESIAN_POINT('Ctrl Pts',(-19.5839237981891,36.5227289659359,7.29362921204945));
#62913=CARTESIAN_POINT('Ctrl Pts',(-19.5630032418838,36.5181444994969,7.23541151810847));
#62914=CARTESIAN_POINT('Ctrl Pts',(-19.5388851643774,36.513560033058,7.17826825427033));
#62915=CARTESIAN_POINT('Ctrl Pts',(-19.511706252538,36.508975566619,7.12257054410726));
#62916=CARTESIAN_POINT('Ctrl Pts',(-19.4845439604262,36.5043939035514,7.06690689273134));
#62917=CARTESIAN_POINT('Ctrl Pts',(-19.4543247680311,36.4998122404838,7.01268749885754));
#62918=CARTESIAN_POINT('Ctrl Pts',(-19.4212331397365,36.4952305774163,6.960262745335));
#62919=CARTESIAN_POINT('Ctrl Pts',(-19.3881495906809,36.4906500329504,6.90785079118619));
#62920=CARTESIAN_POINT('Ctrl Pts',(-19.3521952695133,36.4860694884845,6.85723303787884));
#62921=CARTESIAN_POINT('Ctrl Pts',(-19.3135991259382,36.4814889440186,6.80873273540695));
#62922=CARTESIAN_POINT('Ctrl Pts',(-19.2735926497222,36.4767410229504,6.75846019474391));
#62923=CARTESIAN_POINT('Ctrl Pts',(-19.2307478576811,36.4719931018822,6.71046334262124));
#62924=CARTESIAN_POINT('Ctrl Pts',(-19.1853652729516,36.467245180814,6.66506456838455));
#62925=CARTESIAN_POINT('Ctrl Pts',(-19.1415270681169,36.462658832602,6.62121072497537));
#62926=CARTESIAN_POINT('Ctrl Pts',(-19.0953214707558,36.4580724843901,6.57978126216683));
#62927=CARTESIAN_POINT('Ctrl Pts',(-19.0470548962871,36.4534861361782,6.54102720723496));
#62928=CARTESIAN_POINT('Ctrl Pts',(-18.9962377408532,36.4486574286818,6.50022524739323));
#62929=CARTESIAN_POINT('Ctrl Pts',(-18.9431362676737,36.4438287211855,6.46238967789154));
#62930=CARTESIAN_POINT('Ctrl Pts',(-18.8881423387969,36.4390000136891,6.42776134842927));
#62931=CARTESIAN_POINT('Ctrl Pts',(-18.8331484099201,36.4341713061928,6.393133018967));
#62932=CARTESIAN_POINT('Ctrl Pts',(-18.7762626317917,36.4293425986964,6.36171217583273));
#62933=CARTESIAN_POINT('Ctrl Pts',(-18.7179033614849,36.4245138912001,6.33368184782277));
#62934=CARTESIAN_POINT('Ctrl Pts',(-18.6623430613862,36.419916773447,6.30699588297241));
#62935=CARTESIAN_POINT('Ctrl Pts',(-18.6052191482576,36.4153196556939,6.28327296643721));
#62936=CARTESIAN_POINT('Ctrl Pts',(-18.5468798979243,36.4107225379407,6.26269728522304));
#62937=CARTESIAN_POINT('Ctrl Pts',(-18.4875280737191,36.4060456296299,6.24176447913884));
#62938=CARTESIAN_POINT('Ctrl Pts',(-18.4269187586668,36.401368721319,6.2240895165564));
#62939=CARTESIAN_POINT('Ctrl Pts',(-18.365443933186,36.3966918130082,6.20981693480204));
#62940=CARTESIAN_POINT('Ctrl Pts',(-18.3051841931071,36.392107346489,6.19582645886256));
#62941=CARTESIAN_POINT('Ctrl Pts',(-18.2440933657748,36.3875228799699,6.18510520861257));
#62942=CARTESIAN_POINT('Ctrl Pts',(-18.1825573944324,36.3829384134508,6.17773957749974));
#62943=CARTESIAN_POINT('Ctrl Pts',(-18.1210590519331,36.3783567503029,6.17037845042205));
#62944=CARTESIAN_POINT('Ctrl Pts',(-18.0591166095782,36.373775087155,6.16636893417111));
#62945=CARTESIAN_POINT('Ctrl Pts',(-17.9971244910363,36.3691934240071,6.16574603201085));
#62946=CARTESIAN_POINT('Ctrl Pts',(-17.9351475077161,36.3646128794609,6.16512328193061));
#62947=CARTESIAN_POINT('Ctrl Pts',(-17.873121381107,36.3600323349146,6.16788550967169));
#62948=CARTESIAN_POINT('Ctrl Pts',(-17.8114418593283,36.3554517903684,6.17401562836997));
#62949=CARTESIAN_POINT('Ctrl Pts',(-17.7475085227582,36.3507038693777,6.18036974608442));
#62950=CARTESIAN_POINT('Ctrl Pts',(-17.683948197553,36.345955948387,6.19034265594962));
#62951=CARTESIAN_POINT('Ctrl Pts',(-17.6211947190923,36.3412080273963,6.2038566670323));
#62952=CARTESIAN_POINT('Ctrl Pts',(-17.560576754033,36.3366216791049,6.21691079361959));
#62953=CARTESIAN_POINT('Ctrl Pts',(-17.5007120907975,36.3320353308135,6.23326866138507));
#62954=CARTESIAN_POINT('Ctrl Pts',(-17.4419778000741,36.3274489825221,6.25280893275195));
#62955=CARTESIAN_POINT('Ctrl Pts',(-17.3801397793381,36.3226202751818,6.27338178195278));
#62956=CARTESIAN_POINT('Ctrl Pts',(-17.3195555144789,36.3177915678415,6.29748247377392));
#62957=CARTESIAN_POINT('Ctrl Pts',(-17.2606398578557,36.3129628605011,6.32491235798932));
#62958=CARTESIAN_POINT('Ctrl Pts',(-17.2017242012325,36.3081341531608,6.35234224220473));
#62959=CARTESIAN_POINT('Ctrl Pts',(-17.1444776886246,36.3033054458204,6.38310094281609));
#62960=CARTESIAN_POINT('Ctrl Pts',(-17.0892809569805,36.2984767384801,6.41693619479307));
#62961=CARTESIAN_POINT('Ctrl Pts',(-17.0367315180382,36.2938796209698,6.44914867286746));
#62962=CARTESIAN_POINT('Ctrl Pts',(-16.985823826324,36.2892825034595,6.48428163117312));
#62963=CARTESIAN_POINT('Ctrl Pts',(-16.9369014906503,36.2846853859493,6.52214231634328));
#62964=CARTESIAN_POINT('Ctrl Pts',(-16.8871300242321,36.280008477608,6.56066013840899));
#62965=CARTESIAN_POINT('Ctrl Pts',(-16.8394139915803,36.2753315692668,6.60200108286855));
#62966=CARTESIAN_POINT('Ctrl Pts',(-16.7940873857918,36.2706546609256,6.64591417496078));
#62967=CARTESIAN_POINT('Ctrl Pts',(-16.7496566891601,36.2660701946487,6.68895929689248));
#62968=CARTESIAN_POINT('Ctrl Pts',(-16.7075222054155,36.2614857283718,6.73447544024023));
#62969=CARTESIAN_POINT('Ctrl Pts',(-16.6679658003392,36.2569012620949,6.7821851745263));
#62970=CARTESIAN_POINT('Ctrl Pts',(-16.6284335837389,36.2523195991884,6.82986573463028));
#62971=CARTESIAN_POINT('Ctrl Pts',(-16.5914766441364,36.2477379362818,6.87973683486253));
#62972=CARTESIAN_POINT('Ctrl Pts',(-16.5573382667583,36.2431562733753,6.93148605318312));
#62973=CARTESIAN_POINT('Ctrl Pts',(-16.5232082241712,36.2385757290691,6.98322263707437));
#62974=CARTESIAN_POINT('Ctrl Pts',(-16.4918956579468,36.233995184763,7.03683600404243));
#62975=CARTESIAN_POINT('Ctrl Pts',(-16.4636008043483,36.2294146404568,7.09198437353299));
#62976=CARTESIAN_POINT('Ctrl Pts',(-16.434272033143,36.2246667192321,7.14914791055222));
#62977=CARTESIAN_POINT('Ctrl Pts',(-16.4081861061293,36.2199187980073,7.20796031340688));
#62978=CARTESIAN_POINT('Ctrl Pts',(-16.3855129915753,36.2151708767826,7.26801493742372));
#62979=CARTESIAN_POINT('Ctrl Pts',(-16.3636114498346,36.2105845287254,7.32602588477298));
#62980=CARTESIAN_POINT('Ctrl Pts',(-16.3448942508113,36.2059981806682,7.38519533490138));
#62981=CARTESIAN_POINT('Ctrl Pts',(-16.3294639095098,36.201411832611,7.44514067082224));
#62982=CARTESIAN_POINT('Ctrl Pts',(-16.3132181713755,36.1965831248025,7.5082537420573));
#62983=CARTESIAN_POINT('Ctrl Pts',(-16.3006164407995,36.191754416994,7.5722263432863));
#62984=CARTESIAN_POINT('Ctrl Pts',(-16.2917167601815,36.1869257091856,7.63660218992504));
#62985=CARTESIAN_POINT('Ctrl Pts',(-16.2828170795634,36.1820970013771,7.70097803656378));
#62986=CARTESIAN_POINT('Ctrl Pts',(-16.2776194235065,36.1772682935686,7.7657564745557));
#62987=CARTESIAN_POINT('Ctrl Pts',(-16.2761182329847,36.1724395857601,7.83048089534406));
#62988=CARTESIAN_POINT('Ctrl Pts',(-16.2746890411959,36.167842468039,7.89210106239372));
#62989=CARTESIAN_POINT('Ctrl Pts',(-16.2766039256916,36.1632453503179,7.95392542127461));
#62990=CARTESIAN_POINT('Ctrl Pts',(-16.2818872519691,36.1586482325969,8.01556074530885));
#62991=CARTESIAN_POINT('Ctrl Pts',(-16.2872622791266,36.153971324282,8.07826585249882));
#62992=CARTESIAN_POINT('Ctrl Pts',(-16.2961239002959,36.1492944159671,8.14077477207092));
#62993=CARTESIAN_POINT('Ctrl Pts',(-16.3084423481408,36.1446175076523,8.20267078638046));
#62994=CARTESIAN_POINT('Ctrl Pts',(-16.3205173146481,36.1400330411699,8.26334338970927));
#62995=CARTESIAN_POINT('Ctrl Pts',(-16.3359135950058,36.1354485746876,8.32342657259014));
#62996=CARTESIAN_POINT('Ctrl Pts',(-16.3545509274159,36.1308641082052,8.38253307018724));
#62997=CARTESIAN_POINT('Ctrl Pts',(-16.3731768632127,36.1262824450957,8.44160342452705));
#62998=CARTESIAN_POINT('Ctrl Pts',(-16.3950397685123,36.1217007819863,8.49969779331158));
#62999=CARTESIAN_POINT('Ctrl Pts',(-16.4200090607561,36.1171191188768,8.55644235379012));
#63000=CARTESIAN_POINT('Ctrl Pts',(-16.4449722568007,36.1125385743705,8.61317306020581));
#63001=CARTESIAN_POINT('Ctrl Pts',(-16.4730401292783,36.1079580298643,8.66855414677424));
#63002=CARTESIAN_POINT('Ctrl Pts',(-16.5040340848873,36.103377485358,8.72223204177362));
#63003=CARTESIAN_POINT('Ctrl Pts',(-16.5361605828025,36.0986295643315,8.77787136718084));
#63004=CARTESIAN_POINT('Ctrl Pts',(-16.5714309102883,36.093881643305,8.83168008336001));
#63005=CARTESIAN_POINT('Ctrl Pts',(-16.609595561297,36.0891337222785,8.88329487809966));
#63006=CARTESIAN_POINT('Ctrl Pts',(-16.6464614609853,36.0845473740305,8.93315321022147));
#63007=CARTESIAN_POINT('Ctrl Pts',(-16.686027455947,36.0799610257825,8.98096418929041));
#63008=CARTESIAN_POINT('Ctrl Pts',(-16.7280276523126,36.0753746775344,9.02643420747833));
#63009=CARTESIAN_POINT('Ctrl Pts',(-16.7722472903959,36.0705459701187,9.07430702527207));
#63010=CARTESIAN_POINT('Ctrl Pts',(-16.8191650719499,36.065717262703,9.11958415431174));
#63011=CARTESIAN_POINT('Ctrl Pts',(-16.8684290911691,36.0608885552873,9.16196940762575));
#63012=CARTESIAN_POINT('Ctrl Pts',(-16.9176931103883,36.0560598478715,9.20435466093977));
#63013=CARTESIAN_POINT('Ctrl Pts',(-16.9693028039508,36.0512311404558,9.24384770520734));
#63014=CARTESIAN_POINT('Ctrl Pts',(-17.0228715062085,36.0464024330401,9.28020561691283));
#63015=CARTESIAN_POINT('Ctrl Pts',(-17.0738710048934,36.041805314814,9.31481977017882));
#63016=CARTESIAN_POINT('Ctrl Pts',(-17.1268553831708,36.0372081965879,9.34673488681428));
#63017=CARTESIAN_POINT('Ctrl Pts',(-17.1815074563142,36.0326110783618,9.37571726870559));
#63018=CARTESIAN_POINT('Ctrl Pts',(-17.2371080998668,36.0279341701101,9.40520268421062));
#63019=CARTESIAN_POINT('Ctrl Pts',(-17.2944344955896,36.0232572618583,9.43165221332123));
#63020=CARTESIAN_POINT('Ctrl Pts',(-17.3531203679941,36.0185803536066,9.45486490357257));
#63021=CARTESIAN_POINT('Ctrl Pts',(-17.4106462869812,36.0139958866101,9.47761878426245));
#63022=CARTESIAN_POINT('Ctrl Pts',(-17.4694779340439,36.0094114196135,9.49726242038527));
#63023=CARTESIAN_POINT('Ctrl Pts',(-17.529246399954,36.004826952617,9.51365325651294));
#63024=CARTESIAN_POINT('Ctrl Pts',(-17.588978317847,36.0002452889914,9.53003406975394));
#63025=CARTESIAN_POINT('Ctrl Pts',(-17.6496454287661,35.9956636253658,9.54316589266056));
#63026=CARTESIAN_POINT('Ctrl Pts',(-17.7108628315388,35.9910819617402,9.55295573921381));
#63027=CARTESIAN_POINT('Ctrl Pts',(-17.7720652882304,35.9865014167167,9.56274319559964));
#63028=CARTESIAN_POINT('Ctrl Pts',(-17.8338172676042,35.9819208716933,9.56919021502666));
#63029=CARTESIAN_POINT('Ctrl Pts',(-17.8957248501482,35.9773403266698,9.57225513208727));
#63030=CARTESIAN_POINT('Ctrl Pts',(-17.9598945680667,35.9725924061406,9.57543204281681));
#63031=CARTESIAN_POINT('Ctrl Pts',(-18.0242309024963,35.9678444856115,9.57497480613621));
#63032=CARTESIAN_POINT('Ctrl Pts',(-18.0882932978743,35.9630965650824,9.57089605715209));
#63033=CARTESIAN_POINT('Ctrl Pts',(-18.150175649512,35.9585102163204,9.56695610802298));
#63034=CARTESIAN_POINT('Ctrl Pts',(-18.2118018920341,35.9539238675584,9.55963731561465));
#63035=CARTESIAN_POINT('Ctrl Pts',(-18.2727811503428,35.9493375187964,9.54900388135465));
#63036=CARTESIAN_POINT('Ctrl Pts',(-18.3369827518602,35.9445088123837,9.53780854169233));
#63037=CARTESIAN_POINT('Ctrl Pts',(-18.4004664639146,35.9396801059709,9.5229386679061));
#63038=CARTESIAN_POINT('Ctrl Pts',(-18.4627926050996,35.9348513995582,9.50452933166129));
#63039=CARTESIAN_POINT('Ctrl Pts',(-18.5251187462847,35.9300226931455,9.48611999541648));
#63040=CARTESIAN_POINT('Ctrl Pts',(-18.5862867310796,35.9251939867328,9.46417148928455));
#63041=CARTESIAN_POINT('Ctrl Pts',(-18.6458827826311,35.9203652803201,9.43887697267678));
#63042=CARTESIAN_POINT('Ctrl Pts',(-18.7026205415385,35.9157681640155,9.41479560910305));
#63043=CARTESIAN_POINT('Ctrl Pts',(-18.7581668126214,35.9111710477108,9.38758297034592));
#63044=CARTESIAN_POINT('Ctrl Pts',(-18.8121532460799,35.9065739314062,9.35737883897773));
#63045=CARTESIAN_POINT('Ctrl Pts',(-18.8670767225288,35.9018970229143,9.32665045424125));
#63046=CARTESIAN_POINT('Ctrl Pts',(-18.9203851712327,35.8972201144224,9.29282585956303));
#63047=CARTESIAN_POINT('Ctrl Pts',(-18.971711136109,35.8925432059305,9.25610384102974));
#63048=CARTESIAN_POINT('Ctrl Pts',(-19.0220225958897,35.887958740854,9.22010766710573));
#63049=CARTESIAN_POINT('Ctrl Pts',(-19.0704287956415,35.8833742757776,9.18132787790683));
#63050=CARTESIAN_POINT('Ctrl Pts',(-19.1166099179761,35.8787898107012,9.1399971377757));
#63051=CARTESIAN_POINT('Ctrl Pts',(-19.1627628009093,35.8742081489899,9.0986916710744));
#63052=CARTESIAN_POINT('Ctrl Pts',(-19.2066929257736,35.8696264872786,9.05483868525564));
#63053=CARTESIAN_POINT('Ctrl Pts',(-19.2481134527839,35.8650448255673,9.00871116024585));
#63054=CARTESIAN_POINT('Ctrl Pts',(-19.2895238671477,35.8604642824494,8.9625948970762));
#63055=CARTESIAN_POINT('Ctrl Pts',(-19.328425559996,35.8558837393314,8.91420557571092));
#63056=CARTESIAN_POINT('Ctrl Pts',(-19.3645699219587,35.8513031962135,8.86385158188092));
#63057=CARTESIAN_POINT('Ctrl Pts',(-19.4020350479962,35.846555273829,8.81165758472919));
#63058=CARTESIAN_POINT('Ctrl Pts',(-19.4365370373085,35.8418073514446,8.7573529876506));
#63059=CARTESIAN_POINT('Ctrl Pts',(-19.4678476161369,35.8370594290601,8.7013148060487));
#63060=CARTESIAN_POINT('Ctrl Pts',(-19.4980926716629,35.83247308216,8.64718364726638));
#63061=CARTESIAN_POINT('Ctrl Pts',(-19.5253598851062,35.8278867352599,8.59143551198449));
#63062=CARTESIAN_POINT('Ctrl Pts',(-19.549491249346,35.8233003883598,8.53443363387662));
#63063=CARTESIAN_POINT('Ctrl Pts',(-19.5748978235564,35.8184716782332,8.47441951980089));
#63064=CARTESIAN_POINT('Ctrl Pts',(-19.5968277040167,35.8136429681065,8.41301608542877));
#63065=CARTESIAN_POINT('Ctrl Pts',(-19.6151559647572,35.8088142579799,8.35066600308205));
#63066=CARTESIAN_POINT('Ctrl Pts',(-19.6334842254977,35.8039855478533,8.28831592073533));
#63067=CARTESIAN_POINT('Ctrl Pts',(-19.6482107948462,35.7991568377267,8.22501984103038));
#63068=CARTESIAN_POINT('Ctrl Pts',(-19.6592736002429,35.7943281276001,8.16123016864215));
#63069=CARTESIAN_POINT('Ctrl Pts',(-19.6758401992731,35.7870971132568,8.06570485776181));
#63070=CARTESIAN_POINT('Ctrl Pts',(-19.6842587270469,35.7798660989135,7.96872710022575));
#63071=CARTESIAN_POINT('Ctrl Pts',(-19.6843394141533,35.7726350845702,7.87141313964419));
#63072=CARTESIAN_POINT('',(-19.6843399766484,34.9788850846098,7.87028213160167));
#63073=CARTESIAN_POINT('Ctrl Pts',(-19.6843394141537,35.7726350845326,7.8714131391384));
#63074=CARTESIAN_POINT('Ctrl Pts',(-19.6843898638469,35.7681138840299,7.81056746706279));
#63075=CARTESIAN_POINT('Ctrl Pts',(-19.6811777589129,35.7635926835272,7.74960646610825));
#63076=CARTESIAN_POINT('Ctrl Pts',(-19.6746925941157,35.7590714830244,7.68891480720527));
#63077=CARTESIAN_POINT('Ctrl Pts',(-19.6682138803083,35.7545547798968,7.62828352013334));
#63078=CARTESIAN_POINT('Ctrl Pts',(-19.658468608052,35.7500380767691,7.56792156436955));
#63079=CARTESIAN_POINT('Ctrl Pts',(-19.6454982932953,35.7455213736414,7.50821239569258));
#63080=CARTESIAN_POINT('Ctrl Pts',(-19.6325357833295,35.7410073884065,7.44853915656618));
#63081=CARTESIAN_POINT('Ctrl Pts',(-19.6163521865777,35.7364934031715,7.38951843896976));
#63082=CARTESIAN_POINT('Ctrl Pts',(-19.5970403871103,35.7319794179365,7.33152509617046));
#63083=CARTESIAN_POINT('Ctrl Pts',(-19.5777326210722,35.7274663754848,7.27354386576143));
#63084=CARTESIAN_POINT('Ctrl Pts',(-19.5552981152331,35.722953333033,7.21659008277439));
#63085=CARTESIAN_POINT('Ctrl Pts',(-19.5298793954744,35.7184402905813,7.16102278239427));
#63086=CARTESIAN_POINT('Ctrl Pts',(-19.504438441355,35.7139233004636,7.10540687597058));
#63087=CARTESIAN_POINT('Ctrl Pts',(-19.4760082787103,35.7094063103459,7.05118035357585));
#63088=CARTESIAN_POINT('Ctrl Pts',(-19.4447787212475,35.7048893202283,6.99868023471251));
#63089=CARTESIAN_POINT('Ctrl Pts',(-19.4135352439157,35.7003703167644,6.94615671510854));
#63090=CARTESIAN_POINT('Ctrl Pts',(-19.3794901817844,35.6958513133006,6.89536156744597));
#63091=CARTESIAN_POINT('Ctrl Pts',(-19.3428765130795,35.6913323098367,6.84660249868574));
#63092=CARTESIAN_POINT('Ctrl Pts',(-19.3061967613092,35.6868051501402,6.79775542594119));
#63093=CARTESIAN_POINT('Ctrl Pts',(-19.2669394870019,35.6822779904436,6.75095217067773));
#63094=CARTESIAN_POINT('Ctrl Pts',(-19.2253769567209,35.6777508307471,6.70646612800977));
#63095=CARTESIAN_POINT('Ctrl Pts',(-19.1964275659122,35.6745975454581,6.67548043426059));
#63096=CARTESIAN_POINT('Ctrl Pts',(-19.1663605874905,35.6714442601691,6.64561817842495));
#63097=CARTESIAN_POINT('Ctrl Pts',(-19.1352773691066,35.6682909748801,6.61696008202848));
#63098=CARTESIAN_POINT('Ctrl Pts',(-19.0899616695121,35.6636938534647,6.5751799268587));
#63099=CARTESIAN_POINT('Ctrl Pts',(-19.042283529149,35.6590967320493,6.53577536668713));
#63100=CARTESIAN_POINT('Ctrl Pts',(-18.9925220576629,35.6544996106339,6.49902446471642));
#63101=CARTESIAN_POINT('Ctrl Pts',(-18.9418969390844,35.6498227027808,6.46163572369713));
#63102=CARTESIAN_POINT('Ctrl Pts',(-18.8891158098682,35.6451457949278,6.42699406116622));
#63103=CARTESIAN_POINT('Ctrl Pts',(-18.834511174932,35.6404688870747,6.39535241921456));
#63104=CARTESIAN_POINT('Ctrl Pts',(-18.7809857835882,35.6358844168478,6.36433616445523));
#63105=CARTESIAN_POINT('Ctrl Pts',(-18.7257087743786,35.6312999466209,6.33620268827328));
#63106=CARTESIAN_POINT('Ctrl Pts',(-18.6690238994596,35.626715476394,6.31114756901959));
#63107=CARTESIAN_POINT('Ctrl Pts',(-18.61237368686,35.6221338095318,6.28610777075849));
#63108=CARTESIAN_POINT('Ctrl Pts',(-18.5543177802338,35.6175521426695,6.26414280230948));
#63109=CARTESIAN_POINT('Ctrl Pts',(-18.495223083031,35.6129704758072,6.24540158491029));
#63110=CARTESIAN_POINT('Ctrl Pts',(-18.4361428136328,35.6083899275461,6.22666494312673));
#63111=CARTESIAN_POINT('Ctrl Pts',(-18.3760247421643,35.6038093792849,6.21115064377193));
#63112=CARTESIAN_POINT('Ctrl Pts',(-18.3152522857029,35.5992288310237,6.1989581870788));
#63113=CARTESIAN_POINT('Ctrl Pts',(-18.2522592579376,35.5944809136184,6.18632022890303));
#63114=CARTESIAN_POINT('Ctrl Pts',(-18.1885636565305,35.5897329962131,6.1772517441605));
#63115=CARTESIAN_POINT('Ctrl Pts',(-18.1246030549647,35.5849850788078,6.17180543161424));
#63116=CARTESIAN_POINT('Ctrl Pts',(-18.062818949301,35.5803987268432,6.16654444998496));
#63117=CARTESIAN_POINT('Ctrl Pts',(-18.000788120127,35.5758123748785,6.16466301434031));
#63118=CARTESIAN_POINT('Ctrl Pts',(-17.9389066401533,35.5712260229139,6.16615547323809));
#63119=CARTESIAN_POINT('Ctrl Pts',(-17.8737552709548,35.5663973227882,6.16772679539626));
#63120=CARTESIAN_POINT('Ctrl Pts',(-17.8087701168144,35.5615686226626,6.17303842020226));
#63121=CARTESIAN_POINT('Ctrl Pts',(-17.7444060044007,35.556739922537,6.18202182927694));
#63122=CARTESIAN_POINT('Ctrl Pts',(-17.6800418919871,35.5519112224114,6.19100523835162));
#63123=CARTESIAN_POINT('Ctrl Pts',(-17.6162994436632,35.5470825222857,6.20366022899527));
#63124=CARTESIAN_POINT('Ctrl Pts',(-17.553616462983,35.5422538221601,6.21985700166293));
#63125=CARTESIAN_POINT('Ctrl Pts',(-17.4939398764833,35.5376567156154,6.23527694651285));
#63126=CARTESIAN_POINT('Ctrl Pts',(-17.4349782765018,35.5330596090706,6.25396999845588));
#63127=CARTESIAN_POINT('Ctrl Pts',(-17.377116641579,35.5284625025259,6.27585242473006));
#63128=CARTESIAN_POINT('Ctrl Pts',(-17.3182505614296,35.523785592814,6.29811471753664));
#63129=CARTESIAN_POINT('Ctrl Pts',(-17.2605235375668,35.5191086831021,6.32367813162913));
#63130=CARTESIAN_POINT('Ctrl Pts',(-17.2043283990451,35.5144317733902,6.3524004470638));
#63131=CARTESIAN_POINT('Ctrl Pts',(-17.149244140679,35.5098473180493,6.38055497227541));
#63132=CARTESIAN_POINT('Ctrl Pts',(-17.0956322288748,35.5052628627085,6.41174440081137));
#63133=CARTESIAN_POINT('Ctrl Pts',(-17.0438433892217,35.5006784073676,6.44578595860873));
#63134=CARTESIAN_POINT('Ctrl Pts',(-16.9920862177114,35.4960967553563,6.47980670047505));
#63135=CARTESIAN_POINT('Ctrl Pts',(-16.9421503324278,35.4915151033451,6.51667583439566));
#63136=CARTESIAN_POINT('Ctrl Pts',(-16.8943598105172,35.4869334513338,6.55616583444497));
#63137=CARTESIAN_POINT('Ctrl Pts',(-16.846580955954,35.482352917865,6.59564619359614));
#63138=CARTESIAN_POINT('Ctrl Pts',(-16.8009468172885,35.4777723843961,6.63774582456135));
#63139=CARTESIAN_POINT('Ctrl Pts',(-16.7577489016525,35.4731918509273,6.68219652796081));
#63140=CARTESIAN_POINT('Ctrl Pts',(-16.7129722924801,35.4684439191367,6.72827170877109));
#63141=CARTESIAN_POINT('Ctrl Pts',(-16.670813872052,35.4636959873461,6.77687275872741));
#63142=CARTESIAN_POINT('Ctrl Pts',(-16.6315551950533,35.4589480555555,6.82766059097233));
#63143=CARTESIAN_POINT('Ctrl Pts',(-16.593632674264,35.4543617180678,6.87671987598634));
#63144=CARTESIAN_POINT('Ctrl Pts',(-16.5584159132772,35.4497753805801,6.92781899746907));
#63145=CARTESIAN_POINT('Ctrl Pts',(-16.526114930877,35.4451890430925,6.98062210428792));
#63146=CARTESIAN_POINT('Ctrl Pts',(-16.4921068167789,35.4403603141504,7.03621589580741));
#63147=CARTESIAN_POINT('Ctrl Pts',(-16.4613315471435,35.4355315852084,7.09369821844355));
#63148=CARTESIAN_POINT('Ctrl Pts',(-16.4339781823525,35.4307028562663,7.1526497543335));
#63149=CARTESIAN_POINT('Ctrl Pts',(-16.4066248175614,35.4258741273242,7.21160129022345));
#63150=CARTESIAN_POINT('Ctrl Pts',(-16.3826935247805,35.4210453983822,7.27202140649802));
#63151=CARTESIAN_POINT('Ctrl Pts',(-16.3623126417182,35.4162166694401,7.33347185865497));
#63152=CARTESIAN_POINT('Ctrl Pts',(-16.3429092942354,35.4116195425503,7.39197494080935));
#63153=CARTESIAN_POINT('Ctrl Pts',(-16.3266438012761,35.4070224156606,7.4516521121725));
#63154=CARTESIAN_POINT('Ctrl Pts',(-16.3136545618917,35.4024252887708,7.51213449943365));
#63155=CARTESIAN_POINT('Ctrl Pts',(-16.3004399023335,35.397748381602,7.57366652092223));
#63156=CARTESIAN_POINT('Ctrl Pts',(-16.2906165525897,35.3930714744333,7.63603149923745));
#63157=CARTESIAN_POINT('Ctrl Pts',(-16.2842780252214,35.3883945672645,7.69882225654889));
#63158=CARTESIAN_POINT('Ctrl Pts',(-16.2780647689407,35.3838100918568,7.76037205267192));
#63159=CARTESIAN_POINT('Ctrl Pts',(-16.2751998980814,35.3792256164491,7.82233042015416));
#63160=CARTESIAN_POINT('Ctrl Pts',(-16.2757200219049,35.3746411410414,7.88430356123687));
#63161=CARTESIAN_POINT('Ctrl Pts',(-16.2762398276636,35.3700594691206,7.94623880466037));
#63162=CARTESIAN_POINT('Ctrl Pts',(-16.2801405193744,35.3654777971997,8.00818829577254));
#63163=CARTESIAN_POINT('Ctrl Pts',(-16.2874066548916,35.3608961252789,8.06975636083683));
#63164=CARTESIAN_POINT('Ctrl Pts',(-16.2946710161991,35.3563155720885,8.13130939250985));
#63165=CARTESIAN_POINT('Ctrl Pts',(-16.3052991303677,35.3517350188981,8.19248067768262));
#63166=CARTESIAN_POINT('Ctrl Pts',(-16.3192237196464,35.3471544657076,8.25287985349837));
#63167=CARTESIAN_POINT('Ctrl Pts',(-16.3336570702856,35.342406553292,8.31548582811055));
#63168=CARTESIAN_POINT('Ctrl Pts',(-16.351632376275,35.3376586408764,8.37726159848694));
#63169=CARTESIAN_POINT('Ctrl Pts',(-16.3730174056464,35.3329107284608,8.43778673553079));
#63170=CARTESIAN_POINT('Ctrl Pts',(-16.3936747725681,35.3283243719411,8.49625240056126));
#63171=CARTESIAN_POINT('Ctrl Pts',(-16.417513263608,35.3237380154214,8.55355072015488));
#63172=CARTESIAN_POINT('Ctrl Pts',(-16.4443645722589,35.3191516589017,8.60932311519822));
#63173=CARTESIAN_POINT('Ctrl Pts',(-16.472634649994,35.3143229685381,8.66804241129839));
#63174=CARTESIAN_POINT('Ctrl Pts',(-16.5042444537181,35.3094942781745,8.72506948723511));
#63175=CARTESIAN_POINT('Ctrl Pts',(-16.5389441911409,35.3046655878109,8.78001812693671));
#63176=CARTESIAN_POINT('Ctrl Pts',(-16.5736439285637,35.2998368974473,8.83496676663832));
#63177=CARTESIAN_POINT('Ctrl Pts',(-16.611433158618,35.2950082070837,8.88783648650567));
#63178=CARTESIAN_POINT('Ctrl Pts',(-16.6520132617444,35.2901795167201,8.9382818254643));
#63179=CARTESIAN_POINT('Ctrl Pts',(-16.6906474407284,35.2855823749341,8.98630817591898));
#63180=CARTESIAN_POINT('Ctrl Pts',(-16.7319696179128,35.280985233148,9.0323346627571));
#63181=CARTESIAN_POINT('Ctrl Pts',(-16.775744901437,35.2763880913619,9.07604497975203));
#63182=CARTESIAN_POINT('Ctrl Pts',(-16.8202797157512,35.2717111860552,9.12051370032366));
#63183=CARTESIAN_POINT('Ctrl Pts',(-16.8673533156068,35.2670342807485,9.16258463764284));
#63184=CARTESIAN_POINT('Ctrl Pts',(-16.9166742887765,35.2623573754417,9.20195843307931));
#63185=CARTESIAN_POINT('Ctrl Pts',(-16.9650206932943,35.2577728844773,9.24055421331711));
#63186=CARTESIAN_POINT('Ctrl Pts',(-17.0155260471576,35.253188393513,9.27655813834427));
#63187=CARTESIAN_POINT('Ctrl Pts',(-17.0678793219735,35.2486039025486,9.30972591291417));
#63188=CARTESIAN_POINT('Ctrl Pts',(-17.120200584247,35.2440222148704,9.34287340633082));
#63189=CARTESIAN_POINT('Ctrl Pts',(-17.1743670978097,35.2394405271922,9.37318791612522));
#63190=CARTESIAN_POINT('Ctrl Pts',(-17.2300380335726,35.234858839514,9.40046786458009));
#63191=CARTESIAN_POINT('Ctrl Pts',(-17.2856953780302,35.2302782703928,9.42774115300485));
#63192=CARTESIAN_POINT('Ctrl Pts',(-17.3428559586453,35.2256977012716,9.4519811268719));
#63193=CARTESIAN_POINT('Ctrl Pts',(-17.401155301161,35.2211171321504,9.47303264165956));
#63194=CARTESIAN_POINT('Ctrl Pts',(-17.4615843191,35.2163692348045,9.49485316844173));
#63195=CARTESIAN_POINT('Ctrl Pts',(-17.5232363810911,35.2116213374587,9.51324752106772));
#63196=CARTESIAN_POINT('Ctrl Pts',(-17.5856865378925,35.2068734401128,9.52809882974473));
#63197=CARTESIAN_POINT('Ctrl Pts',(-17.6460121247443,35.2022870674219,9.54244489318707));
#63198=CARTESIAN_POINT('Ctrl Pts',(-17.7070818399886,35.1977006947309,9.55348510286701));
#63199=CARTESIAN_POINT('Ctrl Pts',(-17.7685031325249,35.19311432204,9.56116643493426));
#63200=CARTESIAN_POINT('Ctrl Pts',(-17.8331691634683,35.1882856623667,9.56925355320603));
#63201=CARTESIAN_POINT('Ctrl Pts',(-17.8982243040283,35.1834570026934,9.57361701714175));
#63202=CARTESIAN_POINT('Ctrl Pts',(-17.9632086098792,35.1786283430201,9.57425728245996));
#63203=CARTESIAN_POINT('Ctrl Pts',(-18.0281929157302,35.1737996833468,9.57489754777817));
#63204=CARTESIAN_POINT('Ctrl Pts',(-18.0931057414124,35.1689710236735,9.57181472283474));
#63205=CARTESIAN_POINT('Ctrl Pts',(-18.1574949088875,35.1641423640002,9.56507238574612));
#63206=CARTESIAN_POINT('Ctrl Pts',(-18.2187953337298,35.1595453347016,9.55865347796752));
#63207=CARTESIAN_POINT('Ctrl Pts',(-18.279873043712,35.1549483054031,9.5488918016507));
#63208=CARTESIAN_POINT('Ctrl Pts',(-18.3403349184589,35.1503512761045,9.53581318944809));
#63209=CARTESIAN_POINT('Ctrl Pts',(-18.4018475377279,35.1456743567369,9.5225072888892));
#63210=CARTESIAN_POINT('Ctrl Pts',(-18.4627221750685,35.1409974373692,9.50576802473026));
#63211=CARTESIAN_POINT('Ctrl Pts',(-18.522549267284,35.1363205180015,9.48567791597507));
#63212=CARTESIAN_POINT('Ctrl Pts',(-18.5811925734696,35.1317361398489,9.46598532595604));
#63213=CARTESIAN_POINT('Ctrl Pts',(-18.6388289058307,35.1271517616964,9.44307345791211));
#63214=CARTESIAN_POINT('Ctrl Pts',(-18.6950843618617,35.1225673835438,9.41707116546747));
#63215=CARTESIAN_POINT('Ctrl Pts',(-18.7513054207461,35.1179858084887,9.39108477200804));
#63216=CARTESIAN_POINT('Ctrl Pts',(-18.8061468163189,35.1134042334336,9.36201191414382));
#63217=CARTESIAN_POINT('Ctrl Pts',(-18.8592543782398,35.1088226583785,9.33002964831067));
#63218=CARTESIAN_POINT('Ctrl Pts',(-18.9123489786251,35.1042422015116,9.2980551881319));
#63219=CARTESIAN_POINT('Ctrl Pts',(-18.9637101494715,35.0996617446447,9.26317299210534));
#63220=CARTESIAN_POINT('Ctrl Pts',(-19.0130099127576,35.0950812877778,9.22560516218571));
#63221=CARTESIAN_POINT('Ctrl Pts',(-19.0641130225915,35.090333281403,9.18666313060915));
#63222=CARTESIAN_POINT('Ctrl Pts',(-19.1130004910849,35.0855852750282,9.14483548314177));
#63223=CARTESIAN_POINT('Ctrl Pts',(-19.159343662819,35.0808372686534,9.10041592990687));
#63224=CARTESIAN_POINT('Ctrl Pts',(-19.2041081261462,35.0762510060112,9.05750955584162));
#63225=CARTESIAN_POINT('Ctrl Pts',(-19.2464985531242,35.0716647433691,9.012185471226));
#63226=CARTESIAN_POINT('Ctrl Pts',(-19.2862575471968,35.067078480727,8.96474474467405));
#63227=CARTESIAN_POINT('Ctrl Pts',(-19.3281198120402,35.0622496024858,8.91479437984195));
#63228=CARTESIAN_POINT('Ctrl Pts',(-19.3670641114359,35.0574207242447,8.86249772431315));
#63229=CARTESIAN_POINT('Ctrl Pts',(-19.4028413932655,35.0525918460035,8.8082415495011));
#63230=CARTESIAN_POINT('Ctrl Pts',(-19.4386186750951,35.0477629677624,8.75398537468905));
#63231=CARTESIAN_POINT('Ctrl Pts',(-19.4712286803328,35.0429340895213,8.6977702819307));
#63232=CARTESIAN_POINT('Ctrl Pts',(-19.5004796218082,35.0381052112801,8.64001075009758));
#63233=CARTESIAN_POINT('Ctrl Pts',(-19.5303734600336,35.0331702007242,8.58098174065393));
#63234=CARTESIAN_POINT('Ctrl Pts',(-19.5568705363577,35.0282351901684,8.52012166857817));
#63235=CARTESIAN_POINT('Ctrl Pts',(-19.5797592626129,35.0233001796125,8.45783087472852));
#63236=CARTESIAN_POINT('Ctrl Pts',(-19.6024236126755,35.0184135465359,8.39615071211298));
#63237=CARTESIAN_POINT('Ctrl Pts',(-19.621549852988,35.0135269134592,8.33306812440386));
#63238=CARTESIAN_POINT('Ctrl Pts',(-19.6369781019475,35.0086402803826,8.26899674844114));
#63239=CARTESIAN_POINT('Ctrl Pts',(-19.6526354595126,35.0036810810871,8.2039739162472));
#63240=CARTESIAN_POINT('Ctrl Pts',(-19.6644838559723,34.9987218817917,8.13793304788255));
#63241=CARTESIAN_POINT('Ctrl Pts',(-19.6724072407195,34.9937626824962,8.07132701547553));
#63242=CARTESIAN_POINT('Ctrl Pts',(-19.6803306254667,34.9888034832007,8.00472098306851));
#63243=CARTESIAN_POINT('Ctrl Pts',(-19.6843288412817,34.9838442839052,7.93755020982685));
#63244=CARTESIAN_POINT('Ctrl Pts',(-19.6843399766484,34.9788850846098,7.87028213160166));
#63245=CARTESIAN_POINT('',(-19.6843394318536,34.1851350845228,7.86860837179767));
#63246=CARTESIAN_POINT('Ctrl Pts',(-19.6843399766485,34.9788850845702,7.87028213106522));
#63247=CARTESIAN_POINT('Ctrl Pts',(-19.6843506246404,34.9741429314013,7.80595813210616));
#63248=CARTESIAN_POINT('Ctrl Pts',(-19.6807154430222,34.9694007782325,7.74168452333965));
#63249=CARTESIAN_POINT('Ctrl Pts',(-19.6734774373292,34.9646586250636,7.67788283560038));
#63250=CARTESIAN_POINT('Ctrl Pts',(-19.6662229716926,34.9599056877676,7.61393605648821));
#63251=CARTESIAN_POINT('Ctrl Pts',(-19.6553493709468,34.9551527504716,7.55046379591763));
#63252=CARTESIAN_POINT('Ctrl Pts',(-19.6409512267573,34.9503998131755,7.48787978601849));
#63253=CARTESIAN_POINT('Ctrl Pts',(-19.6265360234759,34.945641244543,7.42522162584197));
#63254=CARTESIAN_POINT('Ctrl Pts',(-19.6085880846665,34.9408826759105,7.36345425064649));
#63255=CARTESIAN_POINT('Ctrl Pts',(-19.5872517340696,34.936124107278,7.30297557466159));
#63256=CARTESIAN_POINT('Ctrl Pts',(-19.565860394136,34.9313532745739,7.24234102936538));
#63257=CARTESIAN_POINT('Ctrl Pts',(-19.5410633669874,34.9265824418697,7.18300224204036));
#63258=CARTESIAN_POINT('Ctrl Pts',(-19.513052892334,34.9218116091656,7.12533654251973));
#63259=CARTESIAN_POINT('Ctrl Pts',(-19.4939841403159,34.9185637589638,7.08607933828757));
#63260=CARTESIAN_POINT('Ctrl Pts',(-19.473427089533,34.915315908762,7.04759702947158));
#63261=CARTESIAN_POINT('Ctrl Pts',(-19.4514538962117,34.9120680585602,7.01000100760332));
#63262=CARTESIAN_POINT('Ctrl Pts',(-19.4203513175739,34.9074707970321,6.95678465395239));
#63263=CARTESIAN_POINT('Ctrl Pts',(-19.3862942488289,34.902873535504,6.90514851011583));
#63264=CARTESIAN_POINT('Ctrl Pts',(-19.3494682120233,34.8982762739759,6.85544016841895));
#63265=CARTESIAN_POINT('Ctrl Pts',(-19.312004314286,34.893599383637,6.80487083238505));
#63266=CARTESIAN_POINT('Ctrl Pts',(-19.2716747990087,34.888922493298,6.75629722263615));
#63267=CARTESIAN_POINT('Ctrl Pts',(-19.2287235719348,34.884245602959,6.71005850298634));
#63268=CARTESIAN_POINT('Ctrl Pts',(-19.1866197856181,34.879660989087,6.66473208732072));
#63269=CARTESIAN_POINT('Ctrl Pts',(-19.1419971652128,34.8750763752151,6.62164965363058));
#63270=CARTESIAN_POINT('Ctrl Pts',(-19.0951271836689,34.8704917613432,6.58109884015776));
#63271=CARTESIAN_POINT('Ctrl Pts',(-19.0482858525379,34.8659099499276,6.54057281435312));
#63272=CARTESIAN_POINT('Ctrl Pts',(-18.9992002683831,34.8613281385121,6.50257567263456));
#63273=CARTESIAN_POINT('Ctrl Pts',(-18.9481776970915,34.8567463270966,6.46735721494934));
#63274=CARTESIAN_POINT('Ctrl Pts',(-18.8971675750048,34.8521656336159,6.43214735035905));
#63275=CARTESIAN_POINT('Ctrl Pts',(-18.8442218227312,34.8475849401352,6.39971511294401));
#63276=CARTESIAN_POINT('Ctrl Pts',(-18.7896779613946,34.8430042466545,6.37026787910912));
#63277=CARTESIAN_POINT('Ctrl Pts',(-18.7331445635888,34.8382564682533,6.3397465308973));
#63278=CARTESIAN_POINT('Ctrl Pts',(-18.6748947006025,34.8335086898521,6.31243248880869));
#63279=CARTESIAN_POINT('Ctrl Pts',(-18.6153313043008,34.8287609114509,6.28850419874872));
#63280=CARTESIAN_POINT('Ctrl Pts',(-18.5577912669704,34.8241744143167,6.26538874884508));
#63281=CARTESIAN_POINT('Ctrl Pts',(-18.4990260348583,34.8195879171825,6.24543280049305));
#63282=CARTESIAN_POINT('Ctrl Pts',(-18.4394160071978,34.8150014200483,6.22874689096094));
#63283=CARTESIAN_POINT('Ctrl Pts',(-18.3766617562319,34.8101730010136,6.21118085726711));
#63284=CARTESIAN_POINT('Ctrl Pts',(-18.3129717504518,34.8053445819789,6.19723952836195));
#63285=CARTESIAN_POINT('Ctrl Pts',(-18.248800852578,34.8005161629442,6.18699051183503));
#63286=CARTESIAN_POINT('Ctrl Pts',(-18.1846299547043,34.7956877439096,6.17674149530811));
#63287=CARTESIAN_POINT('Ctrl Pts',(-18.1199788188343,34.7908593248749,6.17018477954102));
#63288=CARTESIAN_POINT('Ctrl Pts',(-18.0553039694653,34.7860309058402,6.16732441499187));
#63289=CARTESIAN_POINT('Ctrl Pts',(-17.9937365055766,34.7814344743454,6.16460148029923));
#63290=CARTESIAN_POINT('Ctrl Pts',(-17.9318944866733,34.7768380428507,6.16521660012749));
#63291=CARTESIAN_POINT('Ctrl Pts',(-17.870170437177,34.7722416113559,6.16920245098657));
#63292=CARTESIAN_POINT('Ctrl Pts',(-17.8073645375938,34.7675646172628,6.1732581626719));
#63293=CARTESIAN_POINT('Ctrl Pts',(-17.7446813086675,34.7628876231696,6.18080402050468));
#63294=CARTESIAN_POINT('Ctrl Pts',(-17.6825381119754,34.7582106290764,6.19181906196834));
#63295=CARTESIAN_POINT('Ctrl Pts',(-17.6216334537591,34.7536268493244,6.20261456930127));
#63296=CARTESIAN_POINT('Ctrl Pts',(-17.561248025304,34.7490430695724,6.21674215214675));
#63297=CARTESIAN_POINT('Ctrl Pts',(-17.5017706035719,34.7444592898204,6.2341297484238));
#63298=CARTESIAN_POINT('Ctrl Pts',(-17.442329535482,34.7398783117549,6.25150671709735));
#63299=CARTESIAN_POINT('Ctrl Pts',(-17.3837958614369,34.7352973336894,6.2721396056733));
#63300=CARTESIAN_POINT('Ctrl Pts',(-17.3265459798054,34.7307163556238,6.29590575914542));
#63301=CARTESIAN_POINT('Ctrl Pts',(-17.2693100430223,34.7261364933867,6.31966612369019));
#63302=CARTESIAN_POINT('Ctrl Pts',(-17.2133577480129,34.7215566311496,6.34655804293153));
#63303=CARTESIAN_POINT('Ctrl Pts',(-17.1590462563224,34.7169767689125,6.37641043578171));
#63304=CARTESIAN_POINT('Ctrl Pts',(-17.1027339258694,34.7122281842631,6.4073625926581));
#63305=CARTESIAN_POINT('Ctrl Pts',(-17.04818619406,34.7074795996138,6.44149738242054));
#63306=CARTESIAN_POINT('Ctrl Pts',(-16.9957717532147,34.7027310149644,6.47857282122635));
#63307=CARTESIAN_POINT('Ctrl Pts',(-16.9451554313795,34.6981453342818,6.51437635766619));
#63308=CARTESIAN_POINT('Ctrl Pts',(-16.8965287638021,34.6935596535992,6.55292165238522));
#63309=CARTESIAN_POINT('Ctrl Pts',(-16.8501907821988,34.6889739729166,6.59394907351958));
#63310=CARTESIAN_POINT('Ctrl Pts',(-16.8013836008616,34.6841439362838,6.63716271196092));
#63311=CARTESIAN_POINT('Ctrl Pts',(-16.7551163052492,34.6793138996511,6.68312995311512));
#63312=CARTESIAN_POINT('Ctrl Pts',(-16.711692661252,34.6744838630183,6.73150479575973));
#63313=CARTESIAN_POINT('Ctrl Pts',(-16.6682690172549,34.6696538263856,6.77987963840435));
#63314=CARTESIAN_POINT('Ctrl Pts',(-16.6276893705955,34.6648237897529,6.83066152487718));
#63315=CARTESIAN_POINT('Ctrl Pts',(-16.5902048672717,34.6599937531201,6.88346853844153));
#63316=CARTESIAN_POINT('Ctrl Pts',(-16.554520903842,34.6553957236604,6.93373900686912));
#63317=CARTESIAN_POINT('Ctrl Pts',(-16.521494791712,34.6507976942006,6.98605115161277));
#63318=CARTESIAN_POINT('Ctrl Pts',(-16.4913668687188,34.6461996647409,7.04009263405372));
#63319=CARTESIAN_POINT('Ctrl Pts',(-16.4607228501906,34.6415228703933,7.09505985464775));
#63320=CARTESIAN_POINT('Ctrl Pts',(-16.4330776327838,34.6368460760458,7.15181584110059));
#63321=CARTESIAN_POINT('Ctrl Pts',(-16.4086397103088,34.6321692816983,7.2099987306213));
#63322=CARTESIAN_POINT('Ctrl Pts',(-16.3846795378917,34.6275839165127,7.26704417161848));
#63323=CARTESIAN_POINT('Ctrl Pts',(-16.3638025931529,34.622998551327,7.32546073552173));
#63324=CARTESIAN_POINT('Ctrl Pts',(-16.3461591813918,34.6184131861414,7.38488247295153));
#63325=CARTESIAN_POINT('Ctrl Pts',(-16.3285265842987,34.6138306315914,7.44426778735998));
#63326=CARTESIAN_POINT('Ctrl Pts',(-16.3141237346164,34.6092480770414,7.50465656678885));
#63327=CARTESIAN_POINT('Ctrl Pts',(-16.3030517150819,34.6046655224915,7.56566583282496));
#63328=CARTESIAN_POINT('Ctrl Pts',(-16.2919824191085,34.6000840951855,7.62666009143899));
#63329=CARTESIAN_POINT('Ctrl Pts',(-16.2842424175926,34.5955026678796,7.6882740332079));
#63330=CARTESIAN_POINT('Ctrl Pts',(-16.2798816739943,34.5909212405736,7.75011458312333));
#63331=CARTESIAN_POINT('Ctrl Pts',(-16.2753632824288,34.5861741872258,7.81419076940771));
#63332=CARTESIAN_POINT('Ctrl Pts',(-16.2744732661424,34.581427133878,7.87850968701966));
#63333=CARTESIAN_POINT('Ctrl Pts',(-16.2772082986786,34.5766800805303,7.94263096798809));
#63334=CARTESIAN_POINT('Ctrl Pts',(-16.2798512308894,34.5720928809143,8.00459300925585));
#63335=CARTESIAN_POINT('Ctrl Pts',(-16.2858788120345,34.5675056812983,8.06636999537276));
#63336=CARTESIAN_POINT('Ctrl Pts',(-16.2952351180072,34.5629184816823,8.1275696566054));
#63337=CARTESIAN_POINT('Ctrl Pts',(-16.305080493745,34.5580915014686,8.19196832650925));
#63338=CARTESIAN_POINT('Ctrl Pts',(-16.3186120185535,34.5532645212549,8.25572702750474));
#63339=CARTESIAN_POINT('Ctrl Pts',(-16.3357041636109,34.5484375410413,8.31840387825416));
#63340=CARTESIAN_POINT('Ctrl Pts',(-16.3527963086682,34.5436105608276,8.38108072900357));
#63341=CARTESIAN_POINT('Ctrl Pts',(-16.3734487949792,34.5387835806139,8.44267513964444));
#63342=CARTESIAN_POINT('Ctrl Pts',(-16.3974775887123,34.5339566004002,8.50276982653415));
#63343=CARTESIAN_POINT('Ctrl Pts',(-16.4203658458407,34.5293587347932,8.56001209432588));
#63344=CARTESIAN_POINT('Ctrl Pts',(-16.4464107655711,34.5247608691861,8.61612806925893));
#63345=CARTESIAN_POINT('Ctrl Pts',(-16.4754801685045,34.5201630035791,8.67074647188537));
#63346=CARTESIAN_POINT('Ctrl Pts',(-16.5050487175514,34.51548618875,8.72630271845209));
#63347=CARTESIAN_POINT('Ctrl Pts',(-16.5377464870054,34.5108093739208,8.78030895071487));
#63348=CARTESIAN_POINT('Ctrl Pts',(-16.5733823977776,34.5061325590917,8.83239376386073));
#63349=CARTESIAN_POINT('Ctrl Pts',(-16.6083205706582,34.5015473145592,8.88345877571848));
#63350=CARTESIAN_POINT('Ctrl Pts',(-16.6460825651465,34.4969620700266,8.93267649162326));
#63351=CARTESIAN_POINT('Ctrl Pts',(-16.6864423443792,34.4923768254941,8.9797222297426));
#63352=CARTESIAN_POINT('Ctrl Pts',(-16.7267775270666,34.4877943753568,9.02673929667849));
#63353=CARTESIAN_POINT('Ctrl Pts',(-16.7697070246047,34.4832119252195,9.07158662508624));
#63354=CARTESIAN_POINT('Ctrl Pts',(-16.814963808604,34.4786294750822,9.11397166701559));
#63355=CARTESIAN_POINT('Ctrl Pts',(-16.8602096204161,34.4740481359276,9.15634643299131));
#63356=CARTESIAN_POINT('Ctrl Pts',(-16.9077812273287,34.4694667967729,9.19625974987497));
#63357=CARTESIAN_POINT('Ctrl Pts',(-16.9573754072449,34.4648854576182,9.23345655519069));
#63358=CARTESIAN_POINT('Ctrl Pts',(-17.0087647217844,34.4601382901234,9.27199975383744));
#63359=CARTESIAN_POINT('Ctrl Pts',(-17.0623254112357,34.4553911226285,9.30762561239995));
#63360=CARTESIAN_POINT('Ctrl Pts',(-17.1176855824613,34.4506439551337,9.34009818750481));
#63361=CARTESIAN_POINT('Ctrl Pts',(-17.1711797008059,34.4460568027794,9.37147619333745));
#63362=CARTESIAN_POINT('Ctrl Pts',(-17.2263534091185,34.4414696504252,9.39990994792744));
#63363=CARTESIAN_POINT('Ctrl Pts',(-17.2828467641579,34.4368824980709,9.42523380922449));
#63364=CARTESIAN_POINT('Ctrl Pts',(-17.3422961335553,34.4320553230058,9.45188274136469));
#63365=CARTESIAN_POINT('Ctrl Pts',(-17.4032064466867,34.4272281479407,9.47508714952236));
#63366=CARTESIAN_POINT('Ctrl Pts',(-17.4651382813054,34.4224009728756,9.49471297348881));
#63367=CARTESIAN_POINT('Ctrl Pts',(-17.5270701159241,34.4175737978104,9.51433879745526));
#63368=CARTESIAN_POINT('Ctrl Pts',(-17.5900228249264,34.4127466227453,9.53038595207365));
#63369=CARTESIAN_POINT('Ctrl Pts',(-17.6535459491956,34.4079194476802,9.5427828873806));
#63370=CARTESIAN_POINT('Ctrl Pts',(-17.713973200144,34.4033275306045,9.55457564363122));
#63371=CARTESIAN_POINT('Ctrl Pts',(-17.7751660974045,34.3987356135289,9.56311443212996));
#63372=CARTESIAN_POINT('Ctrl Pts',(-17.8367420124595,34.3941436964532,9.56830856578122));
#63373=CARTESIAN_POINT('Ctrl Pts',(-17.8994663460402,34.3894661380576,9.57359957236249));
#63374=CARTESIAN_POINT('Ctrl Pts',(-17.9625876258848,34.3847885796621,9.57541969358361));
#63375=CARTESIAN_POINT('Ctrl Pts',(-18.0256893124278,34.3801110212666,9.57372747889147));
#63376=CARTESIAN_POINT('Ctrl Pts',(-18.0874648290596,34.3755317682816,9.57207082845016));
#63377=CARTESIAN_POINT('Ctrl Pts',(-18.1492210311112,34.3709525152966,9.56704805752778));
#63378=CARTESIAN_POINT('Ctrl Pts',(-18.2105633826536,34.3663732623116,9.55867266282704));
#63379=CARTESIAN_POINT('Ctrl Pts',(-18.2718683053278,34.36179680342,9.550302378487));
#63380=CARTESIAN_POINT('Ctrl Pts',(-18.3327593735459,34.3572203445283,9.53858359511074));
#63381=CARTESIAN_POINT('Ctrl Pts',(-18.3928467801605,34.3526438856367,9.52358167978213));
#63382=CARTESIAN_POINT('Ctrl Pts',(-18.4529197289901,34.3480685278985,9.50858337410284));
#63383=CARTESIAN_POINT('Ctrl Pts',(-18.5121889051227,34.3434931701604,9.49030362811654));
#63384=CARTESIAN_POINT('Ctrl Pts',(-18.5702763487881,34.3389178124222,9.46885855148645));
#63385=CARTESIAN_POINT('Ctrl Pts',(-18.6306185776935,34.3341648526337,9.44658103949334));
#63386=CARTESIAN_POINT('Ctrl Pts',(-18.6896848739899,34.3294118928452,9.42088755978668));
#63387=CARTESIAN_POINT('Ctrl Pts',(-18.7470731927272,34.3246589330567,9.39196371592734));
#63388=CARTESIAN_POINT('Ctrl Pts',(-18.8023884161351,34.3200776691631,9.36408471685403));
#63389=CARTESIAN_POINT('Ctrl Pts',(-18.8561444038319,34.3154964052694,9.33320509228768));
#63390=CARTESIAN_POINT('Ctrl Pts',(-18.9080076521529,34.3109151413757,9.29953720943028));
#63391=CARTESIAN_POINT('Ctrl Pts',(-18.9599081636949,34.3063305858901,9.2658451365385));
#63392=CARTESIAN_POINT('Ctrl Pts',(-19.0099128202455,34.3017460304045,9.22936112250298));
#63393=CARTESIAN_POINT('Ctrl Pts',(-19.0577198226825,34.2971614749189,9.19033890323557));
#63394=CARTESIAN_POINT('Ctrl Pts',(-19.1056072871779,34.2925692033509,9.15125100722773));
#63395=CARTESIAN_POINT('Ctrl Pts',(-19.1512893491688,34.2879769317829,9.10961673335924));
#63396=CARTESIAN_POINT('Ctrl Pts',(-19.1945007774973,34.2833846602149,9.06572684884901));
#63397=CARTESIAN_POINT('Ctrl Pts',(-19.1992129950831,34.2828838717966,9.06094064543879));
#63398=CARTESIAN_POINT('Ctrl Pts',(-19.2038958721242,34.2823830833784,9.05612764994006));
#63399=CARTESIAN_POINT('Ctrl Pts',(-19.2085490945638,34.2818822949602,9.05128826196086));
#63400=CARTESIAN_POINT('Ctrl Pts',(-19.2507977189333,34.2773354197475,9.00734935992727));
#63401=CARTESIAN_POINT('Ctrl Pts',(-19.2907820667709,34.2727885445347,8.9610410817571));
#63402=CARTESIAN_POINT('Ctrl Pts',(-19.3282210877398,34.268241669322,8.91262876143603));
#63403=CARTESIAN_POINT('Ctrl Pts',(-19.3656073664394,34.2637011995256,8.86428464203401));
#63404=CARTESIAN_POINT('Ctrl Pts',(-19.4004551043781,34.2591607297292,8.81384275911745));
#63405=CARTESIAN_POINT('Ctrl Pts',(-19.4325205974813,34.2546202599328,8.76160459257042));
#63406=CARTESIAN_POINT('Ctrl Pts',(-19.4645533250525,34.2500844297316,8.70941980462916));
#63407=CARTESIAN_POINT('Ctrl Pts',(-19.4938091701776,34.2455485995304,8.65544281204892));
#63408=CARTESIAN_POINT('Ctrl Pts',(-19.5200865495544,34.2410127693292,8.60000565441758));
#63409=CARTESIAN_POINT('Ctrl Pts',(-19.5470628518699,34.2363562955993,8.54309398517029));
#63410=CARTESIAN_POINT('Ctrl Pts',(-19.5708996400718,34.2316998218694,8.48464382257598));
#63411=CARTESIAN_POINT('Ctrl Pts',(-19.5914290092486,34.2270433481395,8.42504178559117));
#63412=CARTESIAN_POINT('Ctrl Pts',(-19.6114150615545,34.2225101096007,8.36701713717319));
#63413=CARTESIAN_POINT('Ctrl Pts',(-19.6282664798948,34.217976871062,8.30790136813938));
#63414=CARTESIAN_POINT('Ctrl Pts',(-19.6418780073849,34.2134436325233,8.24806920553037));
#63415=CARTESIAN_POINT('Ctrl Pts',(-19.6560445748906,34.2087255411978,8.18579725469854));
#63416=CARTESIAN_POINT('Ctrl Pts',(-19.6667011420569,34.2040074498723,8.1227498077348));
#63417=CARTESIAN_POINT('Ctrl Pts',(-19.673787848891,34.1992893585467,8.05936092138871));
#63418=CARTESIAN_POINT('Ctrl Pts',(-19.6808745557251,34.1945712672212,7.99597203504263));
#63419=CARTESIAN_POINT('Ctrl Pts',(-19.6843913902768,34.1898531758957,7.93224234397999));
#63420=CARTESIAN_POINT('Ctrl Pts',(-19.6843394318541,34.1851350845702,7.86860837243737));
#63421=CARTESIAN_POINT('',(-18.5338892852531,34.0285,6.25817448361128));
#63422=CARTESIAN_POINT('Ctrl Pts',(-19.6843394318536,34.1851350845228,7.86860837179767));
#63423=CARTESIAN_POINT('Ctrl Pts',(-19.6842719233823,34.1790049718436,7.78593014688382));
#63424=CARTESIAN_POINT('Ctrl Pts',(-19.6781845294511,34.1728748591644,7.70351110997361));
#63425=CARTESIAN_POINT('Ctrl Pts',(-19.6662118452382,34.1667447464852,7.62207975359352));
#63426=CARTESIAN_POINT('Ctrl Pts',(-19.6591158625868,34.1631115450702,7.57381693450569));
#63427=CARTESIAN_POINT('Ctrl Pts',(-19.649953449709,34.1594783436552,7.5259004991251));
#63428=CARTESIAN_POINT('Ctrl Pts',(-19.6387602520471,34.1558451422402,7.47847827412956));
#63429=CARTESIAN_POINT('Ctrl Pts',(-19.6245873402614,34.1512447550488,7.41843189311805));
#63430=CARTESIAN_POINT('Ctrl Pts',(-19.607121248674,34.1466443678575,7.35903532165387));
#63431=CARTESIAN_POINT('Ctrl Pts',(-19.5864384974648,34.1420439806661,7.30067567286909));
#63432=CARTESIAN_POINT('Ctrl Pts',(-19.5654135544815,34.137367481035,7.24135047595436));
#63433=CARTESIAN_POINT('Ctrl Pts',(-19.5410645761215,34.1326909814039,7.18309736177195));
#63434=CARTESIAN_POINT('Ctrl Pts',(-19.5135260599372,34.1280144817729,7.12631145020672));
#63435=CARTESIAN_POINT('Ctrl Pts',(-19.4865088438649,34.1234265076006,7.07060048770063));
#63436=CARTESIAN_POINT('Ctrl Pts',(-19.4564220270362,34.1188385334284,7.01630214098928));
#63437=CARTESIAN_POINT('Ctrl Pts',(-19.4234417677024,34.1142505592562,6.96377116639769));
#63438=CARTESIAN_POINT('Ctrl Pts',(-19.3904811002752,34.1096653105678,6.91127139780543));
#63439=CARTESIAN_POINT('Ctrl Pts',(-19.354630668445,34.1050800618793,6.86053734884721));
#63440=CARTESIAN_POINT('Ctrl Pts',(-19.3161118896715,34.1004948131909,6.8118979945778));
#63441=CARTESIAN_POINT('Ctrl Pts',(-19.2776019099619,34.0959106119369,6.76326975127296));
#63442=CARTESIAN_POINT('Ctrl Pts',(-19.2364251088108,34.091326410683,6.71673565079938));
#63443=CARTESIAN_POINT('Ctrl Pts',(-19.192844206647,34.086742209429,6.67259289880058));
#63444=CARTESIAN_POINT('Ctrl Pts',(-19.1477392085214,34.0819976911032,6.62690640202541));
#63445=CARTESIAN_POINT('Ctrl Pts',(-19.1000592002055,34.0772531727775,6.58378207147794));
#63446=CARTESIAN_POINT('Ctrl Pts',(-19.0501364505395,34.0725086544518,6.54350732650842));
#63447=CARTESIAN_POINT('Ctrl Pts',(-19.0018381420728,34.0679185184686,6.50454308537656));
#63448=CARTESIAN_POINT('Ctrl Pts',(-18.9514412861617,34.0633283824854,6.46824606480622));
#63449=CARTESIAN_POINT('Ctrl Pts',(-18.8992778243817,34.0587382465022,6.43483341830988));
#63450=CARTESIAN_POINT('Ctrl Pts',(-18.8444827028466,34.0539165370052,6.39973509540149));
#63451=CARTESIAN_POINT('Ctrl Pts',(-18.7877385472706,34.0490948275082,6.36782022212208));
#63452=CARTESIAN_POINT('Ctrl Pts',(-18.7294583783504,34.0442731180112,6.33928546922675));
#63453=CARTESIAN_POINT('Ctrl Pts',(-18.6711782094302,34.0394514085142,6.31075071633142));
#63454=CARTESIAN_POINT('Ctrl Pts',(-18.6113626481108,34.0346296990172,6.28559626162566));
#63455=CARTESIAN_POINT('Ctrl Pts',(-18.5504447240674,34.0298079895202,6.26395901285688));
#63456=CARTESIAN_POINT('Ctrl Pts',(-18.5449363038492,34.0293719930134,6.26200249414));
#63457=CARTESIAN_POINT('Ctrl Pts',(-18.5394177624311,34.0289359965067,6.26007429487589));
#63458=CARTESIAN_POINT('Ctrl Pts',(-18.5338892852531,34.0285,6.25817448361128));
#63459=CARTESIAN_POINT('',(-19.6230207093981,34.0285,7.41694615762715));
#63460=CARTESIAN_POINT('Origin',(-17.98,34.0285,7.87));
#63461=CARTESIAN_POINT('',(-19.6817804353622,34.0624899145464,7.87021334420357));
#63462=CARTESIAN_POINT('Ctrl Pts',(-19.6230207093982,34.0285,7.41694615762719));
#63463=CARTESIAN_POINT('Ctrl Pts',(-19.6439594234565,34.0343385372865,7.49288137240387));
#63464=CARTESIAN_POINT('Ctrl Pts',(-19.6596181661918,34.040177074573,7.57022718668484));
#63465=CARTESIAN_POINT('Ctrl Pts',(-19.6698639770707,34.0460156118594,7.64833679917736));
#63466=CARTESIAN_POINT('Ctrl Pts',(-19.6795006474282,34.0515070326815,7.72180258887821));
#63467=CARTESIAN_POINT('Ctrl Pts',(-19.6843492737208,34.0569984535036,7.79594416842021));
#63468=CARTESIAN_POINT('Ctrl Pts',(-19.684339986675,34.0624898743257,7.87021312113508));
#63469=CARTESIAN_POINT('',(-19.6836712649746,34.8562399466723,7.87062608132905));
#63470=CARTESIAN_POINT('Ctrl Pts',(-19.6817242086285,34.0624899154299,7.87021334910381));
#63471=CARTESIAN_POINT('Ctrl Pts',(-19.6788237970149,34.0931723278599,8.28454169889619));
#63472=CARTESIAN_POINT('Ctrl Pts',(-19.32074390439,34.1658671245298,9.26764861307284));
#63473=CARTESIAN_POINT('Ctrl Pts',(-17.6674941309001,34.2805743054401,9.86139173961966));
#63474=CARTESIAN_POINT('Ctrl Pts',(-16.1387855091513,34.40661145816,8.68643802656981));
#63475=CARTESIAN_POINT('Ctrl Pts',(-16.2948985422798,34.53264861088,6.76609642493242));
#63476=CARTESIAN_POINT('Ctrl Pts',(-17.9941440978388,34.6586857636,5.85535067860367));
#63477=CARTESIAN_POINT('Ctrl Pts',(-19.4371160993711,34.7665495317833,6.65484857269287));
#63478=CARTESIAN_POINT('Ctrl Pts',(-19.6807260588958,34.8324009157266,7.5478711651106));
#63479=CARTESIAN_POINT('Ctrl Pts',(-19.6817736577327,34.8562399154299,7.87062496082499));
#63480=CARTESIAN_POINT('',(-19.6843395660614,35.6499899153767,7.87121620626328));
#63481=CARTESIAN_POINT('Ctrl Pts',(-19.6843398848609,34.8562399576805,7.87062647613745));
#63482=CARTESIAN_POINT('Ctrl Pts',(-19.6843151234373,34.8612080553341,7.93799038569272));
#63483=CARTESIAN_POINT('Ctrl Pts',(-19.6802923106048,34.8661761529877,8.0052332769274));
#63484=CARTESIAN_POINT('Ctrl Pts',(-19.672339476806,34.8711442506413,8.07189584157179));
#63485=CARTESIAN_POINT('Ctrl Pts',(-19.6643644321827,34.8761262232918,8.13874458268597));
#63486=CARTESIAN_POINT('Ctrl Pts',(-19.6524375222774,34.8811081959424,8.20500940461969));
#63487=CARTESIAN_POINT('Ctrl Pts',(-19.6366776310176,34.886090168593,8.27024250459691));
#63488=CARTESIAN_POINT('Ctrl Pts',(-19.620850813758,34.891093297703,8.33575262364476));
#63489=CARTESIAN_POINT('Ctrl Pts',(-19.6011585501973,34.8960964268129,8.40022190399817));
#63490=CARTESIAN_POINT('Ctrl Pts',(-19.5777696675149,34.9010995559229,8.46321743498425));
#63491=CARTESIAN_POINT('Ctrl Pts',(-19.5627158479965,34.904319726962,8.50376333736041));
#63492=CARTESIAN_POINT('Ctrl Pts',(-19.5461316374502,34.907539898001,8.54369915558196));
#63493=CARTESIAN_POINT('Ctrl Pts',(-19.5280720831781,34.91076006904,8.58291490437828));
#63494=CARTESIAN_POINT('Ctrl Pts',(-19.5022938886773,34.9153565388155,8.63889143540082));
#63495=CARTESIAN_POINT('Ctrl Pts',(-19.4734226123672,34.9199530085909,8.69358328884918));
#63496=CARTESIAN_POINT('Ctrl Pts',(-19.4416089489638,34.9245494783663,8.74662655441696));
#63497=CARTESIAN_POINT('Ctrl Pts',(-19.4092379836671,34.9292264676744,8.80059901546763));
#63498=CARTESIAN_POINT('Ctrl Pts',(-19.3738206871155,34.9339034569825,8.85286405197072));
#63499=CARTESIAN_POINT('Ctrl Pts',(-19.3355668076366,34.9385804462905,8.90306024298394));
#63500=CARTESIAN_POINT('Ctrl Pts',(-19.2980751762118,34.9431642417566,8.95225622305252));
#63501=CARTESIAN_POINT('Ctrl Pts',(-19.2578592916959,34.9477480372227,8.99946462368427));
#63502=CARTESIAN_POINT('Ctrl Pts',(-19.2151612444391,34.9523318326888,9.04437282659111));
#63503=CARTESIAN_POINT('Ctrl Pts',(-19.1724893732809,34.9569128180525,9.08925349846036));
#63504=CARTESIAN_POINT('Ctrl Pts',(-19.1273387067944,34.9614938034163,9.13183640037992));
#63505=CARTESIAN_POINT('Ctrl Pts',(-19.0799906443404,34.96607478878,9.17184308500047));
#63506=CARTESIAN_POINT('Ctrl Pts',(-19.0326542016859,34.9706546499134,9.21183995148637));
#63507=CARTESIAN_POINT('Ctrl Pts',(-18.9831218223752,34.9752345110467,9.24926152721103));
#63508=CARTESIAN_POINT('Ctrl Pts',(-18.931709148148,34.9798143721801,9.283868640621));
#63509=CARTESIAN_POINT('Ctrl Pts',(-18.8784025704177,34.9845629429784,9.31975058624508));
#63510=CARTESIAN_POINT('Ctrl Pts',(-18.8230749130192,34.9893115137768,9.35260629089814));
#63511=CARTESIAN_POINT('Ctrl Pts',(-18.7661101301898,34.9940600845751,9.38221879991389));
#63512=CARTESIAN_POINT('Ctrl Pts',(-18.7110996723638,34.9986457433042,9.41081537480491));
#63513=CARTESIAN_POINT('Ctrl Pts',(-18.6545631187334,35.0032314020333,9.43638754236675));
#63514=CARTESIAN_POINT('Ctrl Pts',(-18.5968682145621,35.0078170607625,9.45878835640968));
#63515=CARTESIAN_POINT('Ctrl Pts',(-18.5360987697057,35.0126470875954,9.48238290177329));
#63516=CARTESIAN_POINT('Ctrl Pts',(-18.4740446787157,35.0174771144283,9.50245843256857));
#63517=CARTESIAN_POINT('Ctrl Pts',(-18.4111526444799,35.0223071412612,9.51890334245462));
#63518=CARTESIAN_POINT('Ctrl Pts',(-18.3482606102441,35.0271371680942,9.53534825234067));
#63519=CARTESIAN_POINT('Ctrl Pts',(-18.2845312868417,35.0319671949271,9.54816248925614));
#63520=CARTESIAN_POINT('Ctrl Pts',(-18.2204192144078,35.03679722176,9.55729767289105));
#63521=CARTESIAN_POINT('Ctrl Pts',(-18.1593967423115,35.041394486619,9.56599262638878));
#63522=CARTESIAN_POINT('Ctrl Pts',(-18.0977766951745,35.0459917514779,9.57139077173162));
#63523=CARTESIAN_POINT('Ctrl Pts',(-18.0359466975418,35.0505890163369,9.57342149881765));
#63524=CARTESIAN_POINT('Ctrl Pts',(-17.9730457984822,35.0552659062595,9.57548739828953));
#63525=CARTESIAN_POINT('Ctrl Pts',(-17.909928118726,35.0599427961822,9.57406795243933));
#63526=CARTESIAN_POINT('Ctrl Pts',(-17.8470109542982,35.0646196861048,9.5691435340557));
#63527=CARTESIAN_POINT('Ctrl Pts',(-17.7853351396093,35.069204301429,9.56431627398382));
#63528=CARTESIAN_POINT('Ctrl Pts',(-17.7238525319013,35.0737889167531,9.55612113212566));
#63529=CARTESIAN_POINT('Ctrl Pts',(-17.6629571844191,35.0783735320773,9.54459209620986));
#63530=CARTESIAN_POINT('Ctrl Pts',(-17.6020990699957,35.0829553442439,9.53307010945774));
#63531=CARTESIAN_POINT('Ctrl Pts',(-17.5418280029354,35.0875371564105,9.51821836506025));
#63532=CARTESIAN_POINT('Ctrl Pts',(-17.4825306284952,35.0921189685771,9.50012240645132));
#63533=CARTESIAN_POINT('Ctrl Pts',(-17.4232477313223,35.0966996621088,9.48203086591371));
#63534=CARTESIAN_POINT('Ctrl Pts',(-17.3649385415053,35.1012803556404,9.46069683204308));
#63535=CARTESIAN_POINT('Ctrl Pts',(-17.3079752627805,35.105861049172,9.43625591400802));
#63536=CARTESIAN_POINT('Ctrl Pts',(-17.2489342138832,35.110608826281,9.41092349865015));
#63537=CARTESIAN_POINT('Ctrl Pts',(-17.1913397195808,35.11535660339,9.38225333882373));
#63538=CARTESIAN_POINT('Ctrl Pts',(-17.1355819578834,35.120104380499,9.35045027128507));
#63539=CARTESIAN_POINT('Ctrl Pts',(-17.0817182835261,35.1246908759453,9.31972755176912));
#63540=CARTESIAN_POINT('Ctrl Pts',(-17.0295689526653,35.1292773713916,9.28608172025399));
#63541=CARTESIAN_POINT('Ctrl Pts',(-16.9794569339345,35.1338638668379,9.24974215292145));
#63542=CARTESIAN_POINT('Ctrl Pts',(-16.9267016716432,35.1386922847782,9.2114857933746));
#63543=CARTESIAN_POINT('Ctrl Pts',(-16.8762051016778,35.1435207027186,9.17024405891093));
#63544=CARTESIAN_POINT('Ctrl Pts',(-16.828302823352,35.1483491206589,9.12633134518765));
#63545=CARTESIAN_POINT('Ctrl Pts',(-16.7804005450262,35.1531775385993,9.08241863146438));
#63546=CARTESIAN_POINT('Ctrl Pts',(-16.7350929556611,35.1580059565396,9.03583545820782));
#63547=CARTESIAN_POINT('Ctrl Pts',(-16.6926668877745,35.16283437448,8.98693701423482));
#63548=CARTESIAN_POINT('Ctrl Pts',(-16.6522724599837,35.1674315759071,8.94038015043522));
#63549=CARTESIAN_POINT('Ctrl Pts',(-16.6143239782576,35.1720287773342,8.89153356176056));
#63550=CARTESIAN_POINT('Ctrl Pts',(-16.5790909528396,35.1766259787614,8.84068464352961));
#63551=CARTESIAN_POINT('Ctrl Pts',(-16.5432471327471,35.181302876613,8.78895421574631));
#63552=CARTESIAN_POINT('Ctrl Pts',(-16.5102142347303,35.1859797744646,8.73515171132269));
#63553=CARTESIAN_POINT('Ctrl Pts',(-16.4802350318256,35.1906566723162,8.67961711681319));
#63554=CARTESIAN_POINT('Ctrl Pts',(-16.4508477515244,35.195241227434,8.62517902182931));
#63555=CARTESIAN_POINT('Ctrl Pts',(-16.4243949291801,35.1998257825519,8.56907708288993));
#63556=CARTESIAN_POINT('Ctrl Pts',(-16.4010616749758,35.2044103376697,8.51166081489345));
#63557=CARTESIAN_POINT('Ctrl Pts',(-16.3777426805329,35.2089920910068,8.454279635971));
#63558=CARTESIAN_POINT('Ctrl Pts',(-16.3575396652213,35.2135738443439,8.39558619130295));
#63559=CARTESIAN_POINT('Ctrl Pts',(-16.3405904038642,35.218155597681,8.33595172678911));
#63560=CARTESIAN_POINT('Ctrl Pts',(-16.323645275198,35.222736233862,8.27633180278007));
#63561=CARTESIAN_POINT('Ctrl Pts',(-16.3099524646705,35.227316870043,8.215771803851));
#63562=CARTESIAN_POINT('Ctrl Pts',(-16.2995998497716,35.231897506224,8.15465798901892));
#63563=CARTESIAN_POINT('Ctrl Pts',(-16.2888693515922,35.2366453413053,8.0913134441677));
#63564=CARTESIAN_POINT('Ctrl Pts',(-16.2817277674087,35.2413931763867,8.02737443498475));
#63565=CARTESIAN_POINT('Ctrl Pts',(-16.2782145559828,35.246141011468,7.96327989135553));
#63566=CARTESIAN_POINT('Ctrl Pts',(-16.2748207687374,35.2507274539531,7.90136410596504));
#63567=CARTESIAN_POINT('Ctrl Pts',(-16.2748125482068,35.2553138964382,7.83930371930836));
#63568=CARTESIAN_POINT('Ctrl Pts',(-16.2781722879367,35.2599003389234,7.77749446474163));
#63569=CARTESIAN_POINT('Ctrl Pts',(-16.2817093667871,35.2647288703028,7.712422695896));
#63570=CARTESIAN_POINT('Ctrl Pts',(-16.2889797411147,35.2695574016822,7.64762994774134));
#63571=CARTESIAN_POINT('Ctrl Pts',(-16.2999012076079,35.2743859330617,7.58356871085268));
#63572=CARTESIAN_POINT('Ctrl Pts',(-16.3108226741011,35.2792144644411,7.51950747396401));
#63573=CARTESIAN_POINT('Ctrl Pts',(-16.3253950114371,35.2840429958206,7.45617836410896));
#63574=CARTESIAN_POINT('Ctrl Pts',(-16.3434752900945,35.2888715272,7.3940150112991));
#63575=CARTESIAN_POINT('Ctrl Pts',(-16.360688737066,35.2934685619264,7.33483198666555));
#63576=CARTESIAN_POINT('Ctrl Pts',(-16.3811521205907,35.2980655966527,7.27646232160108));
#63577=CARTESIAN_POINT('Ctrl Pts',(-16.4047701441574,35.3026626313791,7.21928828436697));
#63578=CARTESIAN_POINT('Ctrl Pts',(-16.4287985847493,35.3073395500683,7.16112071783878));
#63579=CARTESIAN_POINT('Ctrl Pts',(-16.4560922934411,35.3120164687575,7.10419126539392));
#63580=CARTESIAN_POINT('Ctrl Pts',(-16.4864972678719,35.3166933874467,7.04888829948308));
#63581=CARTESIAN_POINT('Ctrl Pts',(-16.5163006442759,35.3212777678224,6.99467956751886));
#63582=CARTESIAN_POINT('Ctrl Pts',(-16.5490930309837,35.3258621481981,6.942034012477));
#63583=CARTESIAN_POINT('Ctrl Pts',(-16.5846811669062,35.3304465285739,6.89129667947134));
#63584=CARTESIAN_POINT('Ctrl Pts',(-16.6202475333548,35.3350281046569,6.84059038279334));
#63585=CARTESIAN_POINT('Ctrl Pts',(-16.6586059662633,35.33960968074,6.79179040955657));
#63586=CARTESIAN_POINT('Ctrl Pts',(-16.6995192765142,35.3441912568231,6.74521381926106));
#63587=CARTESIAN_POINT('Ctrl Pts',(-16.7404225907294,35.3487717135247,6.69864860866713));
#63588=CARTESIAN_POINT('Ctrl Pts',(-16.7838792073069,35.3533521702264,6.65430608495941));
#63589=CARTESIAN_POINT('Ctrl Pts',(-16.8296122643484,35.357932626928,6.61246952591105));
#63590=CARTESIAN_POINT('Ctrl Pts',(-16.8770181827825,35.362680631344,6.56910263477996));
#63591=CARTESIAN_POINT('Ctrl Pts',(-16.9268699213697,35.36742863576,6.52842903170431));
#63592=CARTESIAN_POINT('Ctrl Pts',(-16.9788200298526,35.372176640176,6.49071993308988));
#63593=CARTESIAN_POINT('Ctrl Pts',(-17.0290004127111,35.3767628996925,6.45429542771381));
#63594=CARTESIAN_POINT('Ctrl Pts',(-17.0811380077813,35.3813491592089,6.42063691214574));
#63595=CARTESIAN_POINT('Ctrl Pts',(-17.1348907892762,35.3859354187253,6.38994417079969));
#63596=CARTESIAN_POINT('Ctrl Pts',(-17.1914871423834,35.3907642955911,6.35762775518849));
#63597=CARTESIAN_POINT('Ctrl Pts',(-17.2498737426217,35.3955931724569,6.32859990749813));
#63598=CARTESIAN_POINT('Ctrl Pts',(-17.3096257081861,35.4004220493226,6.30303696773824));
#63599=CARTESIAN_POINT('Ctrl Pts',(-17.3693776737504,35.4052509261884,6.27747402797836));
#63600=CARTESIAN_POINT('Ctrl Pts',(-17.4304943668391,35.4100798030542,6.25537614417692));
#63601=CARTESIAN_POINT('Ctrl Pts',(-17.4925338173321,35.41490867992,6.23685837835318));
#63602=CARTESIAN_POINT('Ctrl Pts',(-17.5515960289201,35.4195058216566,6.21922926986613));
#63603=CARTESIAN_POINT('Ctrl Pts',(-17.6117371016633,35.4241029633933,6.20477204542772));
#63604=CARTESIAN_POINT('Ctrl Pts',(-17.6725841503931,35.4287001051299,6.19361390753489));
#63605=CARTESIAN_POINT('Ctrl Pts',(-17.7344869373383,35.4333770104428,6.18226216826233));
#63606=CARTESIAN_POINT('Ctrl Pts',(-17.7971199510101,35.4380539157558,6.17432533261754));
#63607=CARTESIAN_POINT('Ctrl Pts',(-17.8600733785421,35.4427308210687,6.16988458007531));
#63608=CARTESIAN_POINT('Ctrl Pts',(-17.9217828637429,35.447315312025,6.16553157557615));
#63609=CARTESIAN_POINT('Ctrl Pts',(-17.9837996829887,35.4518998029814,6.16453778560315));
#63610=CARTESIAN_POINT('Ctrl Pts',(-18.0457291105473,35.4564842939378,6.16692791707848));
#63611=CARTESIAN_POINT('Ctrl Pts',(-18.1076206702255,35.4610659816234,6.16931658706422));
#63612=CARTESIAN_POINT('Ctrl Pts',(-18.1694244365405,35.4656476693089,6.17508505606959));
#63613=CARTESIAN_POINT('Ctrl Pts',(-18.2307453797122,35.4702293569945,6.18420594669663));
#63614=CARTESIAN_POINT('Ctrl Pts',(-18.292051352411,35.4748099261384,6.19332461061223));
#63615=CARTESIAN_POINT('Ctrl Pts',(-18.3528742326574,35.4793904952823,6.20579399657293));
#63616=CARTESIAN_POINT('Ctrl Pts',(-18.4128258636383,35.4839710644262,6.2215350754821));
#63617=CARTESIAN_POINT('Ctrl Pts',(-18.474967527914,35.4887189617773,6.2378511760603));
#63618=CARTESIAN_POINT('Ctrl Pts',(-18.5361724781148,35.4934668591285,6.2576825394613));
#63619=CARTESIAN_POINT('Ctrl Pts',(-18.5960244732915,35.4982147564796,6.28088430757671));
#63620=CARTESIAN_POINT('Ctrl Pts',(-18.6538402893248,35.5028011292311,6.30329674601002));
#63621=CARTESIAN_POINT('Ctrl Pts',(-18.710393281511,35.5073875019826,6.32885365136161));
#63622=CARTESIAN_POINT('Ctrl Pts',(-18.7653301112277,35.511973874734,6.35737597136661));
#63623=CARTESIAN_POINT('Ctrl Pts',(-18.8231691198259,35.516802534385,6.38740505605384));
#63624=CARTESIAN_POINT('Ctrl Pts',(-18.8792159148823,35.521631194036,6.42072123326522));
#63625=CARTESIAN_POINT('Ctrl Pts',(-18.9330920032162,35.526459853687,6.45706317586196));
#63626=CARTESIAN_POINT('Ctrl Pts',(-18.9869680915501,35.531288513338,6.49340511845869));
#63627=CARTESIAN_POINT('Ctrl Pts',(-19.0386730031194,35.536117172989,6.53277237100758));
#63628=CARTESIAN_POINT('Ctrl Pts',(-19.0878704529053,35.54094583264,6.57485603302973));
#63629=CARTESIAN_POINT('Ctrl Pts',(-19.1341625502696,35.5454893360873,6.61445444693653));
#63630=CARTESIAN_POINT('Ctrl Pts',(-19.1784373949638,35.5500328395347,6.65663099304316));
#63631=CARTESIAN_POINT('Ctrl Pts',(-19.2203879253897,35.5545763429821,6.70114901285603));
#63632=CARTESIAN_POINT('Ctrl Pts',(-19.2621522608043,35.5590996803513,6.74546944200395));
#63633=CARTESIAN_POINT('Ctrl Pts',(-19.3016124668893,35.5636230177204,6.79211026620416));
#63634=CARTESIAN_POINT('Ctrl Pts',(-19.3384978864176,35.5681463550896,6.84079723659574));
#63635=CARTESIAN_POINT('Ctrl Pts',(-19.3753474306025,35.5726652929892,6.88943685326857));
#63636=CARTESIAN_POINT('Ctrl Pts',(-19.4096268323428,35.5771842308888,6.94011825861442));
#63637=CARTESIAN_POINT('Ctrl Pts',(-19.4411043180265,35.5817031687884,6.99253261744701));
#63638=CARTESIAN_POINT('Ctrl Pts',(-19.4725635320018,35.5862194835842,7.04491655136303));
#63639=CARTESIAN_POINT('Ctrl Pts',(-19.501223783586,35.5907357983799,7.09903099590914));
#63640=CARTESIAN_POINT('Ctrl Pts',(-19.5268967318177,35.5952521131756,7.15453837510904));
#63641=CARTESIAN_POINT('Ctrl Pts',(-19.5528264412119,35.5998135966923,7.21060089659642));
#63642=CARTESIAN_POINT('Ctrl Pts',(-19.5757084782704,35.6043750802091,7.26808390292818));
#63643=CARTESIAN_POINT('Ctrl Pts',(-19.5953974763933,35.6089365637258,7.32661631524103));
#63644=CARTESIAN_POINT('Ctrl Pts',(-19.6149016598431,35.6134552299759,7.38459930149502));
#63645=CARTESIAN_POINT('Ctrl Pts',(-19.6312723962809,35.6179738962259,7.44361154905003));
#63646=CARTESIAN_POINT('Ctrl Pts',(-19.6444185667383,35.6224925624759,7.50327712057099));
#63647=CARTESIAN_POINT('Ctrl Pts',(-19.6577515898165,35.627075454626,7.56379074654537));
#63648=CARTESIAN_POINT('Ctrl Pts',(-19.6677675384883,35.6316583467761,7.62497587102851));
#63649=CARTESIAN_POINT('Ctrl Pts',(-19.674425515394,35.6362412389263,7.68643255086586));
#63650=CARTESIAN_POINT('Ctrl Pts',(-19.6810834922998,35.6408241310764,7.74788923070321));
#63651=CARTESIAN_POINT('Ctrl Pts',(-19.6843835229444,35.6454070232265,7.80961690595762));
#63652=CARTESIAN_POINT('Ctrl Pts',(-19.6843395660614,35.6499899153767,7.87121620626327));
#63653=CARTESIAN_POINT('',(-19.6843394477967,36.443739915472,7.86862803641127));
#63654=CARTESIAN_POINT('Ctrl Pts',(-19.6843395660609,35.6499899154299,7.87121620697879));
#63655=CARTESIAN_POINT('Ctrl Pts',(-19.6842852362621,35.6556542720732,7.94735162419525));
#63656=CARTESIAN_POINT('Ctrl Pts',(-19.6791290596449,35.6613186287166,8.02330707152566));
#63657=CARTESIAN_POINT('Ctrl Pts',(-19.6689440442991,35.66698298536,8.09856695042523));
#63658=CARTESIAN_POINT('Ctrl Pts',(-19.6606780378931,35.6715800926505,8.15964674461064));
#63659=CARTESIAN_POINT('Ctrl Pts',(-19.6490774011019,35.676177199941,8.2204030153502));
#63660=CARTESIAN_POINT('Ctrl Pts',(-19.6341798253407,35.6807743072315,8.28044359056506));
#63661=CARTESIAN_POINT('Ctrl Pts',(-19.6190236388585,35.6854512168502,8.34152642505003));
#63662=CARTESIAN_POINT('Ctrl Pts',(-19.6004549338115,35.6901281264689,8.40186794066396));
#63663=CARTESIAN_POINT('Ctrl Pts',(-19.5785685526927,35.6948050360876,8.46106126411898));
#63664=CARTESIAN_POINT('Ctrl Pts',(-19.55711482541,35.6993894917333,8.51908444353228));
#63665=CARTESIAN_POINT('Ctrl Pts',(-19.5324735819567,35.7039739473791,8.57600391221258));
#63666=CARTESIAN_POINT('Ctrl Pts',(-19.5047849065872,35.7085584030249,8.63144981728524));
#63667=CARTESIAN_POINT('Ctrl Pts',(-19.477113163443,35.7131400551766,8.686861815985));
#63668=CARTESIAN_POINT('Ctrl Pts',(-19.4463979105317,35.7177217073284,8.74080158335486));
#63669=CARTESIAN_POINT('Ctrl Pts',(-19.4128268173985,35.7223033594801,8.79292044453666));
#63670=CARTESIAN_POINT('Ctrl Pts',(-19.3792639213525,35.7268838929253,8.84502657980423));
#63671=CARTESIAN_POINT('Ctrl Pts',(-19.3428468448988,35.7314644263705,8.89531226371593));
#63672=CARTESIAN_POINT('Ctrl Pts',(-19.3038074921772,35.7360449598156,8.94345636113232));
#63673=CARTESIAN_POINT('Ctrl Pts',(-19.2633414251559,35.7407928913377,8.99335991067695));
#63674=CARTESIAN_POINT('Ctrl Pts',(-19.2200580231003,35.7455408228597,9.04096181964529));
#63675=CARTESIAN_POINT('Ctrl Pts',(-19.1742607568843,35.7502887543817,9.08594246581251));
#63676=CARTESIAN_POINT('Ctrl Pts',(-19.1300221872733,35.7548750914384,9.12939220879997));
#63677=CARTESIAN_POINT('Ctrl Pts',(-19.0834385756392,35.7594614284952,9.170395965748));
#63678=CARTESIAN_POINT('Ctrl Pts',(-19.0348186262504,35.764047765552,9.20870553196557));
#63679=CARTESIAN_POINT('Ctrl Pts',(-18.9836290724174,35.7688764943066,9.24903979036904));
#63680=CARTESIAN_POINT('Ctrl Pts',(-18.9301824890949,35.7737052230613,9.28638679929457));
#63681=CARTESIAN_POINT('Ctrl Pts',(-18.8748729381879,35.7785339518159,9.3205093105868));
#63682=CARTESIAN_POINT('Ctrl Pts',(-18.8195633872809,35.7833626805706,9.35463182187903));
#63683=CARTESIAN_POINT('Ctrl Pts',(-18.7623914774936,35.7881914093252,9.38552959481498));
#63684=CARTESIAN_POINT('Ctrl Pts',(-18.7037772347804,35.7930201380799,9.41302344441478));
#63685=CARTESIAN_POINT('Ctrl Pts',(-18.6479743930322,35.797617259429,9.43919856614713));
#63686=CARTESIAN_POINT('Ctrl Pts',(-18.5906351878047,35.8022143807782,9.46239641294078));
#63687=CARTESIAN_POINT('Ctrl Pts',(-18.5321095708365,35.8068115021273,9.48243600102166));
#63688=CARTESIAN_POINT('Ctrl Pts',(-18.4725681975944,35.8114884099887,9.50282339128514));
#63689=CARTESIAN_POINT('Ctrl Pts',(-18.4117992776774,35.81616531785,9.51994153812279));
#63690=CARTESIAN_POINT('Ctrl Pts',(-18.3501961007209,35.8208422257114,9.53364950714117));
#63691=CARTESIAN_POINT('Ctrl Pts',(-18.2898104917995,35.8254266959129,9.5470865423258));
#63692=CARTESIAN_POINT('Ctrl Pts',(-18.228623824416,35.8300111661145,9.55724685912381));
#63693=CARTESIAN_POINT('Ctrl Pts',(-18.1670228187882,35.834595636316,9.56404760879159));
#63694=CARTESIAN_POINT('Ctrl Pts',(-18.1054594814475,35.8391773031682,9.57084419988131));
#63695=CARTESIAN_POINT('Ctrl Pts',(-18.0434828131926,35.8437589700204,9.5742852415339));
#63696=CARTESIAN_POINT('Ctrl Pts',(-17.9814875427819,35.8483406368726,9.57433935083846));
#63697=CARTESIAN_POINT('Ctrl Pts',(-17.9195074081365,35.8529211851389,9.57439344693257));
#63698=CARTESIAN_POINT('Ctrl Pts',(-17.8575091891972,35.8575017334052,9.57106225174645));
#63699=CARTESIAN_POINT('Ctrl Pts',(-17.7958884611795,35.8620822816714,9.56436648245684));
#63700=CARTESIAN_POINT('Ctrl Pts',(-17.732016166547,35.8668301990988,9.55742605571059));
#63701=CARTESIAN_POINT('Ctrl Pts',(-17.6685500690245,35.8715781165262,9.54687041744939));
#63702=CARTESIAN_POINT('Ctrl Pts',(-17.605923271481,35.8763260339536,9.53278123539465));
#63703=CARTESIAN_POINT('Ctrl Pts',(-17.5454275819437,35.8809123859611,9.51917148977694));
#63704=CARTESIAN_POINT('Ctrl Pts',(-17.4857154745479,35.8854987379686,9.50226504846101));
#63705=CARTESIAN_POINT('Ctrl Pts',(-17.4271628914053,35.890085089976,9.48218670350573));
#63706=CARTESIAN_POINT('Ctrl Pts',(-17.3655163222364,35.8949137901134,9.46104739564517));
#63707=CARTESIAN_POINT('Ctrl Pts',(-17.3051558190442,35.8997424902507,9.4363919073577));
#63708=CARTESIAN_POINT('Ctrl Pts',(-17.2464943920001,35.904571190388,9.40842268529577));
#63709=CARTESIAN_POINT('Ctrl Pts',(-17.1878329649559,35.9093998905254,9.38045346323384));
#63710=CARTESIAN_POINT('Ctrl Pts',(-17.1308711463604,35.9142285906627,9.34917088828989));
#63711=CARTESIAN_POINT('Ctrl Pts',(-17.0759872408914,35.9190572908,9.31483070529693));
#63712=CARTESIAN_POINT('Ctrl Pts',(-17.0237355377478,35.9236544090989,9.2821374588468));
#63713=CARTESIAN_POINT('Ctrl Pts',(-16.9731523080326,35.9282515273978,9.24653891649767));
#63714=CARTESIAN_POINT('Ctrl Pts',(-16.924579377696,35.9328486456967,9.20823097618292));
#63715=CARTESIAN_POINT('Ctrl Pts',(-16.8751633906599,35.9375255539393,9.16925814360195));
#63716=CARTESIAN_POINT('Ctrl Pts',(-16.8278286522298,35.9422024621819,9.12748116553173));
#63717=CARTESIAN_POINT('Ctrl Pts',(-16.7829068386722,35.9468793704246,9.0831540704718));
#63718=CARTESIAN_POINT('Ctrl Pts',(-16.7388729242615,35.9514638375454,9.03970311968939));
#63719=CARTESIAN_POINT('Ctrl Pts',(-16.697157797824,35.9560483046663,8.99380231765614));
#63720=CARTESIAN_POINT('Ctrl Pts',(-16.6580407679681,35.9606327717871,8.94573166935142));
#63721=CARTESIAN_POINT('Ctrl Pts',(-16.6189476577524,35.965214435556,8.89769041572762));
#63722=CARTESIAN_POINT('Ctrl Pts',(-16.5824498145957,35.9697960993248,8.84748234079259));
#63723=CARTESIAN_POINT('Ctrl Pts',(-16.5487876471297,35.9743777630936,8.79542208564061));
#63724=CARTESIAN_POINT('Ctrl Pts',(-16.515133698063,35.9789583082791,8.74337454066144));
#63725=CARTESIAN_POINT('Ctrl Pts',(-16.4843143266433,35.9835388534645,8.68947614044453));
#63726=CARTESIAN_POINT('Ctrl Pts',(-16.4565266249892,35.9881193986499,8.63407048839299));
#63727=CARTESIAN_POINT('Ctrl Pts',(-16.427723547981,35.9928673190557,8.57664028842207));
#63728=CARTESIAN_POINT('Ctrl Pts',(-16.4021783051839,35.9976152394616,8.5175910447526));
#63729=CARTESIAN_POINT('Ctrl Pts',(-16.3800571267117,36.0023631598674,8.45733094402891));
#63730=CARTESIAN_POINT('Ctrl Pts',(-16.3586887305708,36.0069495088363,8.39912149079511));
#63731=CARTESIAN_POINT('Ctrl Pts',(-16.3405151730133,36.0115358578053,8.33978279836506));
#63732=CARTESIAN_POINT('Ctrl Pts',(-16.3256354543646,36.0161222067742,8.27969840827669));
#63733=CARTESIAN_POINT('Ctrl Pts',(-16.3099694444177,36.0209509128985,8.21643896937226));
#63734=CARTESIAN_POINT('Ctrl Pts',(-16.2979551716987,36.0257796190228,8.15235346972648));
#63735=CARTESIAN_POINT('Ctrl Pts',(-16.2896464898562,36.0306083251471,8.08789870661546));
#63736=CARTESIAN_POINT('Ctrl Pts',(-16.2813378080138,36.0354370312714,8.02344394350444));
#63737=CARTESIAN_POINT('Ctrl Pts',(-16.2767346856514,36.0402657373957,7.95862057072215));
#63738=CARTESIAN_POINT('Ctrl Pts',(-16.2758273748365,36.04509444352,7.89388512598626));
#63739=CARTESIAN_POINT('Ctrl Pts',(-16.2749635795829,36.0496915599244,7.83225445986492));
#63740=CARTESIAN_POINT('Ctrl Pts',(-16.27744559109,36.0542886763289,7.77045029018436));
#63741=CARTESIAN_POINT('Ctrl Pts',(-16.2832941663669,36.0588857927333,7.70886605039501));
#63742=CARTESIAN_POINT('Ctrl Pts',(-16.2892442552701,36.0635627012128,7.64621289395288));
#63743=CARTESIAN_POINT('Ctrl Pts',(-16.298678991754,36.0682396096922,7.58378790397998));
#63744=CARTESIAN_POINT('Ctrl Pts',(-16.3115647867247,36.0729165181717,7.52200750769174));
#63745=CARTESIAN_POINT('Ctrl Pts',(-16.3241958822037,36.0775009832888,7.46144825729071));
#63746=CARTESIAN_POINT('Ctrl Pts',(-16.3401427422826,36.082085448406,7.40150887309082));
#63747=CARTESIAN_POINT('Ctrl Pts',(-16.3593215557563,36.0866699135232,7.34257586710154));
#63748=CARTESIAN_POINT('Ctrl Pts',(-16.3784886414409,36.0912515752532,7.2836788984752));
#63749=CARTESIAN_POINT('Ctrl Pts',(-16.4008836045432,36.0958332369832,7.22578757090005));
#63750=CARTESIAN_POINT('Ctrl Pts',(-16.4263724385346,36.1004148987132,7.16927449321788));
#63751=CARTESIAN_POINT('Ctrl Pts',(-16.4518550494127,36.1049954418279,7.11277521323577));
#63752=CARTESIAN_POINT('Ctrl Pts',(-16.4804298224537,36.1095759849426,7.05765397899624));
#63753=CARTESIAN_POINT('Ctrl Pts',(-16.5119149281939,36.1141565280573,7.00426270870425));
#63754=CARTESIAN_POINT('Ctrl Pts',(-16.5445505422352,36.1189044504059,6.94892044926253));
#63755=CARTESIAN_POINT('Ctrl Pts',(-16.5803130608027,36.1236523727544,6.89543756585259));
#63756=CARTESIAN_POINT('Ctrl Pts',(-16.6189496548617,36.128400295103,6.84417506678822));
#63757=CARTESIAN_POINT('Ctrl Pts',(-16.6562714154448,36.1329866419453,6.79465707060959));
#63758=CARTESIAN_POINT('Ctrl Pts',(-16.6962743728658,36.1375729887876,6.74721111209977));
#63759=CARTESIAN_POINT('Ctrl Pts',(-16.7386899508729,36.1421593356299,6.70212834714767));
#63760=CARTESIAN_POINT('Ctrl Pts',(-16.7833469593884,36.1469880457316,6.65466320549543));
#63761=CARTESIAN_POINT('Ctrl Pts',(-16.8306781869341,36.1518167558333,6.60981840046909));
#63762=CARTESIAN_POINT('Ctrl Pts',(-16.880329024369,36.156645465935,6.56788687858741));
#63763=CARTESIAN_POINT('Ctrl Pts',(-16.9299798618039,36.1614741760366,6.52595535670574));
#63764=CARTESIAN_POINT('Ctrl Pts',(-16.9819497427688,36.1663028861383,6.48693744610878));
#63765=CARTESIAN_POINT('Ctrl Pts',(-17.0358497883043,36.17113159624,6.45107251300325));
#63766=CARTESIAN_POINT('Ctrl Pts',(-17.0871647100218,36.1757287144503,6.41692771374697));
#63767=CARTESIAN_POINT('Ctrl Pts',(-17.1404396653232,36.1803258326605,6.38550004795636));
#63768=CARTESIAN_POINT('Ctrl Pts',(-17.1953553387445,36.1849229508708,6.35702029386931));
#63769=CARTESIAN_POINT('Ctrl Pts',(-17.2512241579779,36.1895998591245,6.32804622993145));
#63770=CARTESIAN_POINT('Ctrl Pts',(-17.3087908038339,36.1942767673782,6.30212375768071));
#63771=CARTESIAN_POINT('Ctrl Pts',(-17.3676871725774,36.1989536756319,6.27945046069801));
#63772=CARTESIAN_POINT('Ctrl Pts',(-17.4254194272433,36.2035381426222,6.25722531195888));
#63773=CARTESIAN_POINT('Ctrl Pts',(-17.4844288198954,36.2081226096125,6.23812225639109));
#63774=CARTESIAN_POINT('Ctrl Pts',(-17.5443451489424,36.2127070766028,6.22228045883105));
#63775=CARTESIAN_POINT('Ctrl Pts',(-17.6042248396019,36.2172887402257,6.20644834841187));
#63776=CARTESIAN_POINT('Ctrl Pts',(-17.665009875857,36.2218704038487,6.19387367158885));
#63777=CARTESIAN_POINT('Ctrl Pts',(-17.7263145196248,36.2264520674717,6.18464587915572));
#63778=CARTESIAN_POINT('Ctrl Pts',(-17.7876041960597,36.2310326124961,6.17542033965863));
#63779=CARTESIAN_POINT('Ctrl Pts',(-17.8494127249925,36.2356131575205,6.16954013817003));
#63780=CARTESIAN_POINT('Ctrl Pts',(-17.9113458212266,36.240193702545,6.16704332429244));
#63781=CARTESIAN_POINT('Ctrl Pts',(-17.9755419851792,36.2449416230795,6.16445527553028));
#63782=CARTESIAN_POINT('Ctrl Pts',(-18.0398714169071,36.2496895436141,6.16550274986414));
#63783=CARTESIAN_POINT('Ctrl Pts',(-18.1038936953115,36.2544374641487,6.17016907080085));
#63784=CARTESIAN_POINT('Ctrl Pts',(-18.1657372952182,36.2590238129205,6.17467659680957));
#63785=CARTESIAN_POINT('Ctrl Pts',(-18.2272937973692,36.2636101616924,6.18256047419938));
#63786=CARTESIAN_POINT('Ctrl Pts',(-18.2881729321403,36.2681965104642,6.19375291812453));
#63787=CARTESIAN_POINT('Ctrl Pts',(-18.3522691191712,36.2730252168802,6.2055368073315));
#63788=CARTESIAN_POINT('Ctrl Pts',(-18.4156137347041,36.2778539232961,6.22098848966207));
#63789=CARTESIAN_POINT('Ctrl Pts',(-18.4777683550696,36.2826826297121,6.23996886523866));
#63790=CARTESIAN_POINT('Ctrl Pts',(-18.5399229754351,36.287511336128,6.25894924081525));
#63791=CARTESIAN_POINT('Ctrl Pts',(-18.6008870178212,36.292340042544,6.28145801170677));
#63792=CARTESIAN_POINT('Ctrl Pts',(-18.6602484949544,36.29716874896,6.30729823039958));
#63793=CARTESIAN_POINT('Ctrl Pts',(-18.7167629470633,36.3017658666645,6.33189913105645));
#63794=CARTESIAN_POINT('Ctrl Pts',(-18.7720572323024,36.3063629843689,6.3596202454074));
#63795=CARTESIAN_POINT('Ctrl Pts',(-18.8257642986772,36.3109601020734,6.39031841713051));
#63796=CARTESIAN_POINT('Ctrl Pts',(-18.8804035403833,36.3156370103903,6.42154940660611));
#63797=CARTESIAN_POINT('Ctrl Pts',(-18.9333994157732,36.3203139187073,6.45586165797432));
#63798=CARTESIAN_POINT('Ctrl Pts',(-18.9843863082443,36.3249908270242,6.49305302229481));
#63799=CARTESIAN_POINT('Ctrl Pts',(-19.0343654148208,36.3295752934997,6.52950927744225));
#63800=CARTESIAN_POINT('Ctrl Pts',(-19.0824138018446,36.3341597599751,6.56873155216557));
#63801=CARTESIAN_POINT('Ctrl Pts',(-19.1282137998569,36.3387442264506,6.61048425757431));
#63802=CARTESIAN_POINT('Ctrl Pts',(-19.1739857914902,36.3433258895568,6.65221143149514));
#63803=CARTESIAN_POINT('Ctrl Pts',(-19.2175117448531,36.347907552663,6.69646562570516));
#63804=CARTESIAN_POINT('Ctrl Pts',(-19.2585073365847,36.3524892157692,6.74297123998581));
#63805=CARTESIAN_POINT('Ctrl Pts',(-19.2994929193627,36.3570697602757,6.78946550005701));
#63806=CARTESIAN_POINT('Ctrl Pts',(-19.3379490304058,36.3616503047823,6.8382097072997));
#63807=CARTESIAN_POINT('Ctrl Pts',(-19.3736298999924,36.3662308492889,6.88889320792929));
#63808=CARTESIAN_POINT('Ctrl Pts',(-19.4106145752701,36.3709787703215,6.94142872162177));
#63809=CARTESIAN_POINT('Ctrl Pts',(-19.444616876485,36.3757266913541,6.99604755945913));
#63810=CARTESIAN_POINT('Ctrl Pts',(-19.4754119986822,36.3804746123866,7.05237062809768));
#63811=CARTESIAN_POINT('Ctrl Pts',(-19.5051591562389,36.385060960644,7.10677701058069));
#63812=CARTESIAN_POINT('Ctrl Pts',(-19.5319137604025,36.3896473089013,7.16277298205991));
#63813=CARTESIAN_POINT('Ctrl Pts',(-19.555521143059,36.3942336571586,7.21999387435651));
#63814=CARTESIAN_POINT('Ctrl Pts',(-19.5803760248537,36.3990623645789,7.2802385247234));
#63815=CARTESIAN_POINT('Ctrl Pts',(-19.6017416168723,36.4038910719991,7.34184053833335));
#63816=CARTESIAN_POINT('Ctrl Pts',(-19.619497059826,36.4087197794193,7.40435611630556));
#63817=CARTESIAN_POINT('Ctrl Pts',(-19.6372525027796,36.4135484868395,7.46687169427777));
#63818=CARTESIAN_POINT('Ctrl Pts',(-19.651397730968,36.4183771942597,7.53030018536893));
#63819=CARTESIAN_POINT('Ctrl Pts',(-19.661874824937,36.4232059016799,7.59418863539891));
#63820=CARTESIAN_POINT('Ctrl Pts',(-19.676726058949,36.4300505729299,7.68475022861004));
#63821=CARTESIAN_POINT('Ctrl Pts',(-19.6842653206136,36.4368952441799,7.77654262605148));
#63822=CARTESIAN_POINT('Ctrl Pts',(-19.6843394477962,36.4437399154299,7.86862803584488));
#63823=CARTESIAN_POINT('',(-19.6843399609503,37.2374899153791,7.86963516025695));
#63824=CARTESIAN_POINT('Ctrl Pts',(-19.6843394477967,36.443739915472,7.86862803641127));
#63825=CARTESIAN_POINT('Ctrl Pts',(-19.6843884176661,36.4482616412974,7.92946148777897));
#63826=CARTESIAN_POINT('Ctrl Pts',(-19.6811761431254,36.4527833671228,7.99041301810678));
#63827=CARTESIAN_POINT('Ctrl Pts',(-19.6746912185231,36.4573050929483,8.05109806586693));
#63828=CARTESIAN_POINT('Ctrl Pts',(-19.6682129609578,36.4618221700668,8.11172072439519));
#63829=CARTESIAN_POINT('Ctrl Pts',(-19.6584687697771,36.4663392471853,8.17207692326294));
#63830=CARTESIAN_POINT('Ctrl Pts',(-19.6454992584212,36.4708563243038,8.23178316129772));
#63831=CARTESIAN_POINT('Ctrl Pts',(-19.6325379840047,36.4753705326256,8.29145147988756));
#63832=CARTESIAN_POINT('Ctrl Pts',(-19.6163555582859,36.4798847409475,8.35047014286125));
#63833=CARTESIAN_POINT('Ctrl Pts',(-19.5970439853245,36.4843989492693,8.40846409827013));
#63834=CARTESIAN_POINT('Ctrl Pts',(-19.5777370902191,36.4889120641113,8.46644400576209));
#63835=CARTESIAN_POINT('Ctrl Pts',(-19.5553027178393,36.4934251789532,8.52339919969336));
#63836=CARTESIAN_POINT('Ctrl Pts',(-19.5298825606297,36.4979382937952,8.578970298289));
#63837=CARTESIAN_POINT('Ctrl Pts',(-19.5044407789576,36.5024552478613,8.63458867020125));
#63838=CARTESIAN_POINT('Ctrl Pts',(-19.4760083566962,36.5069722019275,8.68882011513211));
#63839=CARTESIAN_POINT('Ctrl Pts',(-19.4447743476152,36.5114891559936,8.74132711777411));
#63840=CARTESIAN_POINT('Ctrl Pts',(-19.4135273527354,36.516007988021,8.79385595063864));
#63841=CARTESIAN_POINT('Ctrl Pts',(-19.3794767452545,36.5205268200483,8.84465847661094));
#63842=CARTESIAN_POINT('Ctrl Pts',(-19.342854838816,36.5250456520757,8.89342636467692));
#63843=CARTESIAN_POINT('Ctrl Pts',(-19.3061658589121,36.5295727603986,8.94228357172081));
#63844=CARTESIAN_POINT('Ctrl Pts',(-19.2668965152215,36.5340998687216,8.9890982968607));
#63845=CARTESIAN_POINT('Ctrl Pts',(-19.2253185702707,36.5386269770445,9.033596362206));
#63846=CARTESIAN_POINT('Ctrl Pts',(-19.1928184511077,36.5421656694963,9.06837904393669));
#63847=CARTESIAN_POINT('Ctrl Pts',(-19.1589085972443,36.5457043619481,9.10174690959737));
#63848=CARTESIAN_POINT('Ctrl Pts',(-19.1237326718399,36.5492430543999,9.13358632905155));
#63849=CARTESIAN_POINT('Ctrl Pts',(-19.0780356034287,36.5538401721501,9.17494894033305));
#63850=CARTESIAN_POINT('Ctrl Pts',(-19.02999799142,36.5584372899004,9.21391438730474));
#63851=CARTESIAN_POINT('Ctrl Pts',(-18.9799014841208,36.5630344076506,9.25020717924991));
#63852=CARTESIAN_POINT('Ctrl Pts',(-18.9289354693085,36.5677113159618,9.28712989246045));
#63853=CARTESIAN_POINT('Ctrl Pts',(-18.8758387360898,36.572388224273,9.32128586270452));
#63854=CARTESIAN_POINT('Ctrl Pts',(-18.8209460962525,36.5770651325842,9.35242520850049));
#63855=CARTESIAN_POINT('Ctrl Pts',(-18.7671384411369,36.5816495991022,9.38294906714675));
#63856=CARTESIAN_POINT('Ctrl Pts',(-18.711605691783,36.5862340656202,9.41057420322532));
#63857=CARTESIAN_POINT('Ctrl Pts',(-18.6546933796397,36.5908185321382,9.43510820043547));
#63858=CARTESIAN_POINT('Ctrl Pts',(-18.597815868994,36.5954001952856,9.4596271952707));
#63859=CARTESIAN_POINT('Ctrl Pts',(-18.5395609347949,36.599981858433,9.48105859813366));
#63860=CARTESIAN_POINT('Ctrl Pts',(-18.4802968307819,36.6045635215804,9.49925686026162));
#63861=CARTESIAN_POINT('Ctrl Pts',(-18.4210471959441,36.6091440661268,9.51745067933173));
#63862=CARTESIAN_POINT('Ctrl Pts',(-18.3607893668345,36.6137246106732,9.53241277529591));
#63863=CARTESIAN_POINT('Ctrl Pts',(-18.2999076567283,36.6183051552197,9.54404716981531));
#63864=CARTESIAN_POINT('Ctrl Pts',(-18.236801284441,36.6230530762113,9.55610669361312));
#63865=CARTESIAN_POINT('Ctrl Pts',(-18.1730251143417,36.627800997203,9.56459044266918));
#63866=CARTESIAN_POINT('Ctrl Pts',(-18.1090171864571,36.6325489181947,9.56944973482557));
#63867=CARTESIAN_POINT('Ctrl Pts',(-18.0471874611272,36.6371352664879,9.57414366430051));
#63868=CARTESIAN_POINT('Ctrl Pts',(-17.985142028619,36.6417216147811,9.57545593148886));
#63869=CARTESIAN_POINT('Ctrl Pts',(-17.9232768925918,36.6463079630743,9.57339582149481));
#63870=CARTESIAN_POINT('Ctrl Pts',(-17.8581425815048,36.6511366704153,9.5712268479203));
#63871=CARTESIAN_POINT('Ctrl Pts',(-17.79320879456,36.6559653777562,9.56531924259274));
#63872=CARTESIAN_POINT('Ctrl Pts',(-17.7289297131063,36.6607940850972,9.55574569453376));
#63873=CARTESIAN_POINT('Ctrl Pts',(-17.6646506316526,36.6656227924381,9.54617214647477));
#63874=CARTESIAN_POINT('Ctrl Pts',(-17.601026876175,36.6704514997791,9.53293286408911));
#63875=CARTESIAN_POINT('Ctrl Pts',(-17.5384950431571,36.67528020712,9.51616165934064));
#63876=CARTESIAN_POINT('Ctrl Pts',(-17.4789622998473,36.6798773247923,9.50019481846777));
#63877=CARTESIAN_POINT('Ctrl Pts',(-17.4201745493426,36.6844744424645,9.48096155356177));
#63878=CARTESIAN_POINT('Ctrl Pts',(-17.3625159870928,36.6890715601368,9.45854912716101));
#63879=CARTESIAN_POINT('Ctrl Pts',(-17.3038566642767,36.6937484684578,9.43574769569905));
#63880=CARTESIAN_POINT('Ctrl Pts',(-17.2463666384539,36.6984253767787,9.40965573658915));
#63881=CARTESIAN_POINT('Ctrl Pts',(-17.1904374154254,36.7031022850997,9.38041906788806));
#63882=CARTESIAN_POINT('Ctrl Pts',(-17.1356136668515,36.7076867515379,9.35176027938338));
#63883=CARTESIAN_POINT('Ctrl Pts',(-17.0822900553124,36.7122712179762,9.32008021122148));
#63884=CARTESIAN_POINT('Ctrl Pts',(-17.0308156159192,36.7168556844144,9.28556484860887));
#63885=CARTESIAN_POINT('Ctrl Pts',(-16.9793726528064,36.7214373474817,9.25107059191304));
#63886=CARTESIAN_POINT('Ctrl Pts',(-16.9297770416608,36.7260190105489,9.21374476148654));
#63887=CARTESIAN_POINT('Ctrl Pts',(-16.8823507596549,36.7306006736161,9.17381784800244));
#63888=CARTESIAN_POINT('Ctrl Pts',(-16.8349360566544,36.735181218082,9.13390068257217));
#63889=CARTESIAN_POINT('Ctrl Pts',(-16.7896900206579,36.7397617625479,9.09138402245842));
#63890=CARTESIAN_POINT('Ctrl Pts',(-16.7469016870263,36.7443423070139,9.04653873125422));
#63891=CARTESIAN_POINT('Ctrl Pts',(-16.702549834913,36.7490902280827,9.00005475876336));
#63892=CARTESIAN_POINT('Ctrl Pts',(-16.6608392231333,36.7538381491515,8.95106905795808));
#63893=CARTESIAN_POINT('Ctrl Pts',(-16.6220482810392,36.7585860702204,8.89992328091535));
#63894=CARTESIAN_POINT('Ctrl Pts',(-16.584577403708,36.7631724184332,8.85051800653634));
#63895=CARTESIAN_POINT('Ctrl Pts',(-16.5498308984838,36.7677587666461,8.79909779660216));
#63896=CARTESIAN_POINT('Ctrl Pts',(-16.5180156953963,36.772345114859,8.74600041592022));
#63897=CARTESIAN_POINT('Ctrl Pts',(-16.4845192615167,36.7771738223558,8.69009717694659));
#63898=CARTESIAN_POINT('Ctrl Pts',(-16.4542728327011,36.7820025298526,8.63233516249499));
#63899=CARTESIAN_POINT('Ctrl Pts',(-16.4274616124387,36.7868312373494,8.57313540001092));
#63900=CARTESIAN_POINT('Ctrl Pts',(-16.4006503921763,36.7916599448463,8.51393563752685));
#63901=CARTESIAN_POINT('Ctrl Pts',(-16.377274541817,36.7964886523431,8.45329876136088));
#63902=CARTESIAN_POINT('Ctrl Pts',(-16.3574583728186,36.8013173598399,8.39166416750968));
#63903=CARTESIAN_POINT('Ctrl Pts',(-16.338592607919,36.8059144774973,8.33298563295686));
#63904=CARTESIAN_POINT('Ctrl Pts',(-16.3228753258776,36.8105115951546,8.27316184919246));
#63905=CARTESIAN_POINT('Ctrl Pts',(-16.3104415356123,36.815108712812,8.21256294252501));
#63906=CARTESIAN_POINT('Ctrl Pts',(-16.2977919361219,36.8197856211348,8.15091224048277));
#63907=CARTESIAN_POINT('Ctrl Pts',(-16.2885411492661,36.8244625294577,8.08845972777955));
#63908=CARTESIAN_POINT('Ctrl Pts',(-16.2827789484866,36.8291394377805,8.02561342454811));
#63909=CARTESIAN_POINT('Ctrl Pts',(-16.2771306410648,36.8337239042026,7.96400931622946));
#63910=CARTESIAN_POINT('Ctrl Pts',(-16.2748343156635,36.8383083706247,7.90202737426948));
#63911=CARTESIAN_POINT('Ctrl Pts',(-16.2759229669212,36.8428928370467,7.84006171458732));
#63912=CARTESIAN_POINT('Ctrl Pts',(-16.2770109524758,36.8474745000974,7.77813394650358));
#63913=CARTESIAN_POINT('Ctrl Pts',(-16.2814798014819,36.852056163148,7.71622294889516));
#63914=CARTESIAN_POINT('Ctrl Pts',(-16.2893104421463,36.8566378261987,7.65472423600295));
#63915=CARTESIAN_POINT('Ctrl Pts',(-16.2971391709792,36.8612183706476,7.59324053786974));
#63916=CARTESIAN_POINT('Ctrl Pts',(-16.3083279978462,36.8657989150965,7.53216942940354));
#63917=CARTESIAN_POINT('Ctrl Pts',(-16.3228060662602,36.8703794595454,7.47190063856369));
#63918=CARTESIAN_POINT('Ctrl Pts',(-16.3378131744878,36.8751273806299,7.40942957950931));
#63919=CARTESIAN_POINT('Ctrl Pts',(-16.3563544867805,36.8798753017145,7.3478211889271));
#63920=CARTESIAN_POINT('Ctrl Pts',(-16.3782939177123,36.884623222799,7.28749466821109));
#63921=CARTESIAN_POINT('Ctrl Pts',(-16.3994867445648,36.8892095709941,7.22922107341622));
#63922=CARTESIAN_POINT('Ctrl Pts',(-16.4238498405645,36.8937959191891,7.17214395764723));
#63923=CARTESIAN_POINT('Ctrl Pts',(-16.4512116161967,36.8983822673842,7.11662033930563));
#63924=CARTESIAN_POINT('Ctrl Pts',(-16.480019287658,36.9032109749135,7.05816265084882));
#63925=CARTESIAN_POINT('Ctrl Pts',(-16.5121510421769,36.9080396824428,7.0014277657604));
#63926=CARTESIAN_POINT('Ctrl Pts',(-16.5473535501985,36.9128683899721,6.94679959625704));
#63927=CARTESIAN_POINT('Ctrl Pts',(-16.5825560582201,36.9176970975014,6.89217142675367));
#63928=CARTESIAN_POINT('Ctrl Pts',(-16.6208288742422,36.9225258050307,6.83965045237918));
#63929=CARTESIAN_POINT('Ctrl Pts',(-16.6618702166072,36.92735451256,6.78957938295643));
#63930=CARTESIAN_POINT('Ctrl Pts',(-16.7009431734319,36.9319516302452,6.74190977419162));
#63931=CARTESIAN_POINT('Ctrl Pts',(-16.7426856445409,36.9365487479304,6.69626457493456));
#63932=CARTESIAN_POINT('Ctrl Pts',(-16.7868598506812,36.9411458656157,6.65295792197494));
#63933=CARTESIAN_POINT('Ctrl Pts',(-16.8318007737431,36.945822773935,6.60889960992414));
#63934=CARTESIAN_POINT('Ctrl Pts',(-16.879258387699,36.9504996822544,6.56726226763398));
#63935=CARTESIAN_POINT('Ctrl Pts',(-16.9289385453971,36.9551765905737,6.52834257194767));
#63936=CARTESIAN_POINT('Ctrl Pts',(-16.9776367452975,36.9597610570248,6.49019214714203));
#63937=CARTESIAN_POINT('Ctrl Pts',(-17.0284700086245,36.9643455234759,6.45465324414821));
#63938=CARTESIAN_POINT('Ctrl Pts',(-17.0811250827108,36.9689299899269,6.4219672936469));
#63939=CARTESIAN_POINT('Ctrl Pts',(-17.1337479585654,36.9735116530069,6.3893013303894));
#63940=CARTESIAN_POINT('Ctrl Pts',(-17.1881900046145,36.9780933160869,6.35948512835093));
#63941=CARTESIAN_POINT('Ctrl Pts',(-17.2441085604581,36.9826749791669,6.33271712921499));
#63942=CARTESIAN_POINT('Ctrl Pts',(-17.300013463928,36.9872555236454,6.30595566541822));
#63943=CARTESIAN_POINT('Ctrl Pts',(-17.3573937026054,36.991836068124,6.28224114686672));
#63944=CARTESIAN_POINT('Ctrl Pts',(-17.4158833977731,36.9964166126025,6.2617253671428));
#63945=CARTESIAN_POINT('Ctrl Pts',(-17.4765103508726,37.001164533659,6.24045992522937));
#63946=CARTESIAN_POINT('Ctrl Pts',(-17.5383288825202,37.0059124547154,6.22263176937869));
#63947=CARTESIAN_POINT('Ctrl Pts',(-17.6009129797018,37.0106603757719,6.20835386840596));
#63948=CARTESIAN_POINT('Ctrl Pts',(-17.6613673258495,37.015246723997,6.19456184764446));
#63949=CARTESIAN_POINT('Ctrl Pts',(-17.722535434032,37.0198330722221,6.18408233538082));
#63950=CARTESIAN_POINT('Ctrl Pts',(-17.7840242866189,37.0244194204472,6.17696475070223));
#63951=CARTESIAN_POINT('Ctrl Pts',(-17.8487624328227,37.0292481279193,6.16947104707702));
#63952=CARTESIAN_POINT('Ctrl Pts',(-17.9138555181008,37.0340768353914,6.16570448675005));
#63953=CARTESIAN_POINT('Ctrl Pts',(-17.978843604896,37.0389055428635,6.16566039230722));
#63954=CARTESIAN_POINT('Ctrl Pts',(-18.0438316916913,37.0437342503356,6.1656162978644));
#63955=CARTESIAN_POINT('Ctrl Pts',(-18.1087141355099,37.0485629578078,6.16929455501697));
#63956=CARTESIAN_POINT('Ctrl Pts',(-18.1730393448705,37.0533916652799,6.17662743410319));
#63957=CARTESIAN_POINT('Ctrl Pts',(-18.2342794507435,37.0579887829537,6.1836086207337));
#63958=CARTESIAN_POINT('Ctrl Pts',(-18.295266142784,37.0625859006275,6.19393051412742));
#63959=CARTESIAN_POINT('Ctrl Pts',(-18.3556065421868,37.0671830183013,6.20756366706376));
#63960=CARTESIAN_POINT('Ctrl Pts',(-18.4169942498921,37.071859926622,6.22143344611464));
#63961=CARTESIAN_POINT('Ctrl Pts',(-18.4777124781656,37.0765368349428,6.23873056012735));
#63962=CARTESIAN_POINT('Ctrl Pts',(-18.5373524530954,37.0812137432636,6.25936873287877));
#63963=CARTESIAN_POINT('Ctrl Pts',(-18.5958136083621,37.0857982097029,6.27959897984085));
#63964=CARTESIAN_POINT('Ctrl Pts',(-18.6532382425253,37.0903826761423,6.30303923706746));
#63965=CARTESIAN_POINT('Ctrl Pts',(-18.709253640683,37.0949671425816,6.32955721847559));
#63966=CARTESIAN_POINT('Ctrl Pts',(-18.7652347857919,37.0995488056498,6.35605898431197));
#63967=CARTESIAN_POINT('Ctrl Pts',(-18.8198079444288,37.104130468718,6.38563452521911));
#63968=CARTESIAN_POINT('Ctrl Pts',(-18.8726205756487,37.1087121317862,6.41810353553407));
#63969=CARTESIAN_POINT('Ctrl Pts',(-18.9254203127977,37.1132926762528,6.45056461862197));
#63970=CARTESIAN_POINT('Ctrl Pts',(-18.9764599423223,37.1178732207195,6.48591750224651));
#63971=CARTESIAN_POINT('Ctrl Pts',(-19.0254135278729,37.1224537651862,6.52393707749591));
#63972=CARTESIAN_POINT('Ctrl Pts',(-19.0761559149126,37.127201686254,6.56334591712811));
#63973=CARTESIAN_POINT('Ctrl Pts',(-19.1246563563058,37.1319496073218,6.60561980035016));
#63974=CARTESIAN_POINT('Ctrl Pts',(-19.1705889294188,37.1366975283896,6.65046203964559));
#63975=CARTESIAN_POINT('Ctrl Pts',(-19.2149584064208,37.1412838766029,6.69377828714254));
#63976=CARTESIAN_POINT('Ctrl Pts',(-19.2569316840539,37.1458702248161,6.73949044725619));
#63977=CARTESIAN_POINT('Ctrl Pts',(-19.2962541270393,37.1504565730293,6.78729509622795));
#63978=CARTESIAN_POINT('Ctrl Pts',(-19.3376545105999,37.1552852805244,6.83762591631826));
#63979=CARTESIAN_POINT('Ctrl Pts',(-19.3761157400387,37.1601139880195,6.89027599323749));
#63980=CARTESIAN_POINT('Ctrl Pts',(-19.4113923459179,37.1649426955146,6.94485634215672));
#63981=CARTESIAN_POINT('Ctrl Pts',(-19.4466689517971,37.1697714030097,6.99943669107596));
#63982=CARTESIAN_POINT('Ctrl Pts',(-19.4787606806699,37.1746001105048,7.05594670850606));
#63983=CARTESIAN_POINT('Ctrl Pts',(-19.5074795664588,37.1794288179999,7.11397023229836));
#63984=CARTESIAN_POINT('Ctrl Pts',(-19.536746626648,37.1843496938979,7.17310128549139));
#63985=CARTESIAN_POINT('Ctrl Pts',(-19.5626186445621,37.189270569796,7.23401934030263));
#63986=CARTESIAN_POINT('Ctrl Pts',(-19.5848908154516,37.194191445694,7.29632735285786));
#63987=CARTESIAN_POINT('Ctrl Pts',(-19.6071102296406,37.1991006653786,7.35848777471911));
#63988=CARTESIAN_POINT('Ctrl Pts',(-19.6257466238498,37.2040098850632,7.42203123622437));
#63989=CARTESIAN_POINT('Ctrl Pts',(-19.6406421908275,37.2089191047479,7.48653898549725));
#63990=CARTESIAN_POINT('Ctrl Pts',(-19.6554847312632,37.2138108481629,7.55081709444244));
#63991=CARTESIAN_POINT('Ctrl Pts',(-19.6666128741679,37.2187025915779,7.61605227192819));
#63992=CARTESIAN_POINT('Ctrl Pts',(-19.67391847149,37.223594334993,7.68181113862676));
#63993=CARTESIAN_POINT('Ctrl Pts',(-19.6808359448899,37.2282261951217,7.7440764389353));
#63994=CARTESIAN_POINT('Ctrl Pts',(-19.6843265124556,37.2328580552504,7.80681084541127));
#63995=CARTESIAN_POINT('Ctrl Pts',(-19.6843399609503,37.2374899153791,7.86963516025696));
#63996=CARTESIAN_POINT('',(-19.6843392863112,38.0312399154724,7.87155972316893));
#63997=CARTESIAN_POINT('Ctrl Pts',(-19.6843399609504,37.2374899154299,7.86963516094604));
#63998=CARTESIAN_POINT('Ctrl Pts',(-19.6843536852301,37.2422167689179,7.93374791986184));
#63999=CARTESIAN_POINT('Ctrl Pts',(-19.6807454522696,37.2469436224059,7.997816708416));
#64000=CARTESIAN_POINT('Ctrl Pts',(-19.6735561124232,37.2516704758939,8.06142238550903));
#64001=CARTESIAN_POINT('Ctrl Pts',(-19.666351501998,37.2564073694956,8.12516316478537));
#64002=CARTESIAN_POINT('Ctrl Pts',(-19.6555506461615,37.2611442630972,8.1884384083136));
#64003=CARTESIAN_POINT('Ctrl Pts',(-19.641246022369,37.2658811566989,8.25083656437254));
#64004=CARTESIAN_POINT('Ctrl Pts',(-19.626925838286,37.2706232030009,8.31330259592769));
#64005=CARTESIAN_POINT('Ctrl Pts',(-19.6090944222083,37.275365249303,8.37488919608283));
#64006=CARTESIAN_POINT('Ctrl Pts',(-19.5878940580458,37.280107295605,8.43520043674885));
#64007=CARTESIAN_POINT('Ctrl Pts',(-19.5666396590223,37.2848614282943,8.49566539692065));
#64008=CARTESIAN_POINT('Ctrl Pts',(-19.5419993287653,37.2896155609837,8.5548480739591));
#64009=CARTESIAN_POINT('Ctrl Pts',(-19.5141633684383,37.294369693673,8.61237294841746));
#64010=CARTESIAN_POINT('Ctrl Pts',(-19.492506734948,37.2980684526886,8.65712783052259));
#64011=CARTESIAN_POINT('Ctrl Pts',(-19.4689167756715,37.3017672117043,8.70087966610814));
#64012=CARTESIAN_POINT('Ctrl Pts',(-19.4435012733911,37.3054659707199,8.7434637132604));
#64013=CARTESIAN_POINT('Ctrl Pts',(-19.4119128259435,37.3100630883962,8.79639062065462));
#64014=CARTESIAN_POINT('Ctrl Pts',(-19.3773846770101,37.3146602060725,8.84771045137129));
#64015=CARTESIAN_POINT('Ctrl Pts',(-19.3401055008303,37.3192573237488,8.89707733993657));
#64016=CARTESIAN_POINT('Ctrl Pts',(-19.3021792823753,37.3239342320692,8.94730107318484));
#64017=CARTESIAN_POINT('Ctrl Pts',(-19.2614058188731,37.3286111403897,8.99550292036121));
#64018=CARTESIAN_POINT('Ctrl Pts',(-19.2180321156265,37.3332880487102,9.04134594218678));
#64019=CARTESIAN_POINT('Ctrl Pts',(-19.1755157194584,37.337872515152,9.08628284938134));
#64020=CARTESIAN_POINT('Ctrl Pts',(-19.1305013054072,37.3424569815939,9.12895294194383));
#64021=CARTESIAN_POINT('Ctrl Pts',(-19.0832629494496,37.3470414480358,9.16907109119239));
#64022=CARTESIAN_POINT('Ctrl Pts',(-19.036053479437,37.3516231111065,9.20916470845568));
#64023=CARTESIAN_POINT('Ctrl Pts',(-18.9866231512652,37.3562047741772,9.24670914778248));
#64024=CARTESIAN_POINT('Ctrl Pts',(-18.9352814865172,37.360786437248,9.28145744431685));
#64025=CARTESIAN_POINT('Ctrl Pts',(-18.8839523567072,37.3653669817172,9.31619725714222));
#64026=CARTESIAN_POINT('Ctrl Pts',(-18.830713238088,37.3699475261864,9.34814199716612));
#64027=CARTESIAN_POINT('Ctrl Pts',(-18.7759035180666,37.3745280706556,9.37708739810577));
#64028=CARTESIAN_POINT('Ctrl Pts',(-18.7190910089807,37.379275991721,9.40709048612073));
#64029=CARTESIAN_POINT('Ctrl Pts',(-18.6605913795709,37.3840239127864,9.43387046693361));
#64030=CARTESIAN_POINT('Ctrl Pts',(-18.6008092348783,37.3887718338517,9.45725257268333));
#64031=CARTESIAN_POINT('Ctrl Pts',(-18.5430614903669,37.3933581820674,9.47983897997796));
#64032=CARTESIAN_POINT('Ctrl Pts',(-18.4841176462316,37.3979445302831,9.49925497493416));
#64033=CARTESIAN_POINT('Ctrl Pts',(-18.4243590797133,37.4025308784989,9.51539352249738));
#64034=CARTESIAN_POINT('Ctrl Pts',(-18.3614426537952,37.407359585989,9.53238488944856));
#64035=CARTESIAN_POINT('Ctrl Pts',(-18.297623641445,37.4121882934792,9.54574267457664));
#64036=CARTESIAN_POINT('Ctrl Pts',(-18.233357608423,37.4170170009694,9.55540344067946));
#64037=CARTESIAN_POINT('Ctrl Pts',(-18.169091575401,37.4218457084596,9.56506420678228));
#64038=CARTESIAN_POINT('Ctrl Pts',(-18.1043791760181,37.4266744159498,9.57102797151584));
#64039=CARTESIAN_POINT('Ctrl Pts',(-18.039677052535,37.4315031234399,9.57329489079276));
#64040=CARTESIAN_POINT('Ctrl Pts',(-17.9780781099484,37.4361002411146,9.57545308627184));
#64041=CARTESIAN_POINT('Ctrl Pts',(-17.9162354219735,37.4406973587893,9.57426985564187));
#64042=CARTESIAN_POINT('Ctrl Pts',(-17.8545418994593,37.445294476464,9.5697161823695));
#64043=CARTESIAN_POINT('Ctrl Pts',(-17.7917775829474,37.4499713847847,9.56508347250123));
#64044=CARTESIAN_POINT('Ctrl Pts',(-17.7291681861668,37.4546482931054,9.55696209132066));
#64045=CARTESIAN_POINT('Ctrl Pts',(-17.6671307498133,37.459325201426,9.54537687338927));
#64046=CARTESIAN_POINT('Ctrl Pts',(-17.6063195203642,37.4639096678663,9.5340206441952));
#64047=CARTESIAN_POINT('Ctrl Pts',(-17.5460583715777,37.4684941343065,9.51933635953746));
#64048=CARTESIAN_POINT('Ctrl Pts',(-17.4867354908501,37.4730786007467,9.50139969339616));
#64049=CARTESIAN_POINT('Ctrl Pts',(-17.4274488856753,37.4776602638157,9.48347399540867));
#64050=CARTESIAN_POINT('Ctrl Pts',(-17.3690998971863,37.4822419268848,9.46230000647829));
#64051=CARTESIAN_POINT('Ctrl Pts',(-17.3120638670408,37.4868235899538,9.43800387687261));
#64052=CARTESIAN_POINT('Ctrl Pts',(-17.2550417620984,37.4914041344213,9.41371367910577));
#64053=CARTESIAN_POINT('Ctrl Pts',(-17.1993324472942,37.4959846788889,9.38630305328262));
#64054=CARTESIAN_POINT('Ctrl Pts',(-17.1452915827475,37.5005652233564,9.35594639666704));
#64055=CARTESIAN_POINT('Ctrl Pts',(-17.0892760236635,37.5053131444233,9.32448048459283));
#64056=CARTESIAN_POINT('Ctrl Pts',(-17.0350537472118,37.5100610654903,9.28984930279165));
#64057=CARTESIAN_POINT('Ctrl Pts',(-16.9829909923909,37.5148089865573,9.25229804107014));
#64058=CARTESIAN_POINT('Ctrl Pts',(-16.932699945168,37.5193953347713,9.21602465747729));
#64059=CARTESIAN_POINT('Ctrl Pts',(-16.8844241595334,37.5239816829853,9.17702714293662));
#64060=CARTESIAN_POINT('Ctrl Pts',(-16.8384603688678,37.5285680311993,9.13556789867421));
#64061=CARTESIAN_POINT('Ctrl Pts',(-16.7900676847417,37.5333967386927,9.09191779752615));
#64062=CARTESIAN_POINT('Ctrl Pts',(-16.7442385827226,37.5382254461862,9.04553902894649));
#64063=CARTESIAN_POINT('Ctrl Pts',(-16.7012733928838,37.5430541536796,8.99677996958283));
#64064=CARTESIAN_POINT('Ctrl Pts',(-16.658308203045,37.547882861173,8.94802091021918));
#64065=CARTESIAN_POINT('Ctrl Pts',(-16.6182072653493,37.5527115686665,8.89688211941023));
#64066=CARTESIAN_POINT('Ctrl Pts',(-16.5812180614224,37.5575402761599,8.84374736143876));
#64067=CARTESIAN_POINT('Ctrl Pts',(-16.5460028980728,37.5621373938347,8.79316100155934));
#64068=CARTESIAN_POINT('Ctrl Pts',(-16.5134630960846,37.5667345115094,8.74055796574083));
#64069=CARTESIAN_POINT('Ctrl Pts',(-16.4838360902121,37.5713316291842,8.68625265123493));
#64070=CARTESIAN_POINT('Ctrl Pts',(-16.4536948582306,37.5760085375049,8.6310047774069));
#64071=CARTESIAN_POINT('Ctrl Pts',(-16.4265688806328,37.5806854458255,8.5739953506703));
#64072=CARTESIAN_POINT('Ctrl Pts',(-16.4026634297552,37.5853623541462,8.51558824320787));
#64073=CARTESIAN_POINT('Ctrl Pts',(-16.3792304843616,37.5899468205864,8.45833558703483));
#64074=CARTESIAN_POINT('Ctrl Pts',(-16.3588921153774,37.5945312870267,8.399740493246));
#64075=CARTESIAN_POINT('Ctrl Pts',(-16.3417952332691,37.599115753467,8.34017015841104));
#64076=CARTESIAN_POINT('Ctrl Pts',(-16.3247088057923,37.6036974165361,8.28063625044553));
#64077=CARTESIAN_POINT('Ctrl Pts',(-16.3108600750346,37.6082790796052,8.22012877221842));
#64078=CARTESIAN_POINT('Ctrl Pts',(-16.3003465747455,37.6128607426743,8.15903149764472));
#64079=CARTESIAN_POINT('Ctrl Pts',(-16.289835641301,37.6174412871418,8.09794913981678));
#64080=CARTESIAN_POINT('Ctrl Pts',(-16.2826584081404,37.6220218316094,8.03627777297429));
#64081=CARTESIAN_POINT('Ctrl Pts',(-16.2788611987016,37.626602376077,7.97441079598));
#64082=CARTESIAN_POINT('Ctrl Pts',(-16.2749252363249,37.6313502971439,7.91028315231327));
#64083=CARTESIAN_POINT('Ctrl Pts',(-16.2746211964079,37.6360982182108,7.84594590356721));
#64084=CARTESIAN_POINT('Ctrl Pts',(-16.2779416574722,37.6408461392777,7.78183972418737));
#64085=CARTESIAN_POINT('Ctrl Pts',(-16.2811491224778,37.6454324874918,7.71991509292971));
#64086=CARTESIAN_POINT('Ctrl Pts',(-16.2877382238244,37.6500188357059,7.65820657356212));
#64087=CARTESIAN_POINT('Ctrl Pts',(-16.2976493894911,37.6546051839199,7.597105773384));
#64088=CARTESIAN_POINT('Ctrl Pts',(-16.3080842971102,37.6594338914132,7.53277618524577));
#64089=CARTESIAN_POINT('Ctrl Pts',(-16.3222019775441,37.6642625989066,7.46912095870547));
#64090=CARTESIAN_POINT('Ctrl Pts',(-16.339872570839,37.6690913063999,7.40658134293734));
#64091=CARTESIAN_POINT('Ctrl Pts',(-16.3575431641339,37.6739200138932,7.34404172716922));
#64092=CARTESIAN_POINT('Ctrl Pts',(-16.378766384666,37.6787487213866,7.28261831111605));
#64093=CARTESIAN_POINT('Ctrl Pts',(-16.4033539822187,37.6835774288799,7.22272712847324));
#64094=CARTESIAN_POINT('Ctrl Pts',(-16.4267623330982,37.688174546555,7.16570838905066));
#64095=CARTESIAN_POINT('Ctrl Pts',(-16.4533158395462,37.6927716642301,7.10984400516698));
#64096=CARTESIAN_POINT('Ctrl Pts',(-16.4828790869993,37.6973687819052,7.05550395491687));
#64097=CARTESIAN_POINT('Ctrl Pts',(-16.5129554539252,37.7020456902258,7.00022074245233));
#64098=CARTESIAN_POINT('Ctrl Pts',(-16.546146922841,37.7067225985464,6.94651580982375));
#64099=CARTESIAN_POINT('Ctrl Pts',(-16.5822590694252,37.7113995068671,6.89475893923818));
#64100=CARTESIAN_POINT('Ctrl Pts',(-16.6176574379125,37.7159839733077,6.8440250740422));
#64101=CARTESIAN_POINT('Ctrl Pts',(-16.6558617716258,37.7205684397483,6.79516340035851));
#64102=CARTESIAN_POINT('Ctrl Pts',(-16.6966432065147,37.725152906189,6.74849646624937));
#64103=CARTESIAN_POINT('Ctrl Pts',(-16.7373997038234,37.7297345692584,6.70185806866457));
#64104=CARTESIAN_POINT('Ctrl Pts',(-16.780729843283,37.7343162323279,6.65741213206746));
#64105=CARTESIAN_POINT('Ctrl Pts',(-16.8263640578861,37.7388978953973,6.61544870624472));
#64106=CARTESIAN_POINT('Ctrl Pts',(-16.8719871310106,37.7434784398653,6.5734955256868));
#64107=CARTESIAN_POINT('Ctrl Pts',(-16.9199127880098,37.7480589843332,6.5340239971402));
#64108=CARTESIAN_POINT('Ctrl Pts',(-16.9698356062,37.7526395288012,6.49728636158201));
#64109=CARTESIAN_POINT('Ctrl Pts',(-17.021582642354,37.7573874498677,6.45920630471912));
#64110=CARTESIAN_POINT('Ctrl Pts',(-17.0754751896956,37.7621353709343,6.42406420237983));
#64111=CARTESIAN_POINT('Ctrl Pts',(-17.1311389606862,37.7668832920008,6.39209277302832));
#64112=CARTESIAN_POINT('Ctrl Pts',(-17.1849084806745,37.7714696402153,6.36120933881292));
#64113=CARTESIAN_POINT('Ctrl Pts',(-17.2403300993967,37.7760559884297,6.33328440733841));
#64114=CARTESIAN_POINT('Ctrl Pts',(-17.2970424780434,37.7806423366441,6.30848027268211));
#64115=CARTESIAN_POINT('Ctrl Pts',(-17.3567517445214,37.7854710441368,6.2823653975651));
#64116=CARTESIAN_POINT('Ctrl Pts',(-17.4178913695572,37.7902997516294,6.25971053018776));
#64117=CARTESIAN_POINT('Ctrl Pts',(-17.4800201908903,37.795128459122,6.24064582546255));
#64118=CARTESIAN_POINT('Ctrl Pts',(-17.5421490122234,37.7999571666146,6.22158112073734));
#64119=CARTESIAN_POINT('Ctrl Pts',(-17.6052663801343,37.8047858741073,6.20610665802978));
#64120=CARTESIAN_POINT('Ctrl Pts',(-17.6689206569898,37.8096145815999,6.19428985861147));
#64121=CARTESIAN_POINT('Ctrl Pts',(-17.7295220087304,37.8142116992748,6.18303980514496));
#64122=CARTESIAN_POINT('Ctrl Pts',(-17.7908588977324,37.8188088169496,6.17505831790774));
#64123=CARTESIAN_POINT('Ctrl Pts',(-17.85254703312,37.8234059346245,6.17043223823424));
#64124=CARTESIAN_POINT('Ctrl Pts',(-17.9153058690002,37.8280828429451,6.16572586523116));
#64125=CARTESIAN_POINT('Ctrl Pts',(-17.9784277562297,37.8327597512658,6.16449267828212));
#64126=CARTESIAN_POINT('Ctrl Pts',(-18.041496570692,37.8374366595864,6.16676983135187));
#64127=CARTESIAN_POINT('Ctrl Pts',(-18.1033187924494,37.8420211260268,6.16900197513409));
#64128=CARTESIAN_POINT('Ctrl Pts',(-18.1650894869301,37.8466055924672,6.17460693477934));
#64129=CARTESIAN_POINT('Ctrl Pts',(-18.2264135422485,37.8511900589076,6.1835673147746));
#64130=CARTESIAN_POINT('Ctrl Pts',(-18.2877000983088,37.8557717219768,6.1925222155562));
#64131=CARTESIAN_POINT('Ctrl Pts',(-18.3485400540762,37.860353385046,6.20482839479221));
#64132=CARTESIAN_POINT('Ctrl Pts',(-18.4085435323183,37.8649350481152,6.22041663547788));
#64133=CARTESIAN_POINT('Ctrl Pts',(-18.4685323608623,37.8695155925829,6.23600107033385));
#64134=CARTESIAN_POINT('Ctrl Pts',(-18.5276846247953,37.8740961370506,6.25486584798509));
#64135=CARTESIAN_POINT('Ctrl Pts',(-18.5856227719727,37.8786766815183,6.27689112309669));
#64136=CARTESIAN_POINT('Ctrl Pts',(-18.6456780233723,37.8834246025851,6.29972121861085));
#64137=CARTESIAN_POINT('Ctrl Pts',(-18.7044281437849,37.8881725236519,6.32594710978269));
#64138=CARTESIAN_POINT('Ctrl Pts',(-18.7614746425419,37.8929204447187,6.35538050366964));
#64139=CARTESIAN_POINT('Ctrl Pts',(-18.816579835745,37.8975067929329,6.38381227235143));
#64140=CARTESIAN_POINT('Ctrl Pts',(-18.8700950818171,37.902093141147,6.41523640411495));
#64141=CARTESIAN_POINT('Ctrl Pts',(-18.9216880834359,37.9066794893612,6.44943729842194));
#64142=CARTESIAN_POINT('Ctrl Pts',(-18.97600744644,37.9115081968543,6.48544549206514));
#64143=CARTESIAN_POINT('Ctrl Pts',(-19.0281952502118,37.9163369043475,6.52453167765242));
#64144=CARTESIAN_POINT('Ctrl Pts',(-19.0779029174026,37.9211656118406,6.56639575807732));
#64145=CARTESIAN_POINT('Ctrl Pts',(-19.1276105845934,37.9259943193337,6.60825983850221));
#64146=CARTESIAN_POINT('Ctrl Pts',(-19.1748376962107,37.9308230268268,6.65290131089329));
#64147=CARTESIAN_POINT('Ctrl Pts',(-19.2192827047016,37.9356517343199,6.69997725944003));
#64148=CARTESIAN_POINT('Ctrl Pts',(-19.261067270979,37.9401913992931,6.74423527983224));
#64149=CARTESIAN_POINT('Ctrl Pts',(-19.3005741516839,37.9447310642663,6.79083660250622));
#64150=CARTESIAN_POINT('Ctrl Pts',(-19.3375250314245,37.9492707292395,6.83951437435744));
#64151=CARTESIAN_POINT('Ctrl Pts',(-19.3744237645193,37.9538039876453,6.88812345007625));
#64152=CARTESIAN_POINT('Ctrl Pts',(-19.4087733272311,37.9583372460512,6.93880275965488));
#64153=CARTESIAN_POINT('Ctrl Pts',(-19.4403330309442,37.962870504457,6.99124959497402));
#64154=CARTESIAN_POINT('Ctrl Pts',(-19.4718604788682,37.9673991296182,7.04364282668281));
#64155=CARTESIAN_POINT('Ctrl Pts',(-19.500603449484,37.9719277547794,7.09779955920494));
#64156=CARTESIAN_POINT('Ctrl Pts',(-19.5263636240853,37.9764563799406,7.15338687026699));
#64157=CARTESIAN_POINT('Ctrl Pts',(-19.5523323855609,37.9810216745647,7.20942428633192));
#64158=CARTESIAN_POINT('Ctrl Pts',(-19.5752695249026,37.9855869691888,7.26691510595684));
#64159=CARTESIAN_POINT('Ctrl Pts',(-19.5950191632529,37.9901522638129,7.32549294042587));
#64160=CARTESIAN_POINT('Ctrl Pts',(-19.6145989101356,37.9946782865987,7.38356687330028));
#64161=CARTESIAN_POINT('Ctrl Pts',(-19.6310456517359,37.9992043093846,7.44270867615168));
#64162=CARTESIAN_POINT('Ctrl Pts',(-19.6442568361512,38.0037303321704,7.50254385442078));
#64163=CARTESIAN_POINT('Ctrl Pts',(-19.6576399687168,38.0083152627136,7.56315780830188));
#64164=CARTESIAN_POINT('Ctrl Pts',(-19.6677025592785,38.0129001932569,7.62448278802777));
#64165=CARTESIAN_POINT('Ctrl Pts',(-19.6743915429074,38.0174851238001,7.68611923721124));
#64166=CARTESIAN_POINT('Ctrl Pts',(-19.6810805265363,38.0220700543433,7.74775568639472));
#64167=CARTESIAN_POINT('Ctrl Pts',(-19.6843958943194,38.0266549848866,7.80970304890221));
#64168=CARTESIAN_POINT('Ctrl Pts',(-19.6843392863117,38.0312399154298,7.87155972259389));
#64169=CARTESIAN_POINT('',(-19.6843399030359,38.8249899154737,7.86942509175251));
#64170=CARTESIAN_POINT('Ctrl Pts',(-19.6843392863112,38.0312399154724,7.87155972316893));
#64171=CARTESIAN_POINT('Ctrl Pts',(-19.6842647470063,38.0372771781012,7.95301024480486));
#64172=CARTESIAN_POINT('Ctrl Pts',(-19.6783476784105,38.0433144407299,8.03420097598546));
#64173=CARTESIAN_POINT('Ctrl Pts',(-19.6667212373974,38.0493517033586,8.11443056869534));
#64174=CARTESIAN_POINT('Ctrl Pts',(-19.6588016692553,38.053464097919,8.16908045904026));
#64175=CARTESIAN_POINT('Ctrl Pts',(-19.6482340032239,38.0575764924794,8.22328503262939));
#64176=CARTESIAN_POINT('Ctrl Pts',(-19.6350725347685,38.0616888870398,8.27682888326031));
#64177=CARTESIAN_POINT('Ctrl Pts',(-19.6203597394925,38.0662860047145,8.33668388464538));
#64178=CARTESIAN_POINT('Ctrl Pts',(-19.6023655918517,38.0708831223893,8.39586267089081));
#64179=CARTESIAN_POINT('Ctrl Pts',(-19.5811692648634,38.075480240064,8.45397929831186));
#64180=CARTESIAN_POINT('Ctrl Pts',(-19.5596050402617,38.0801571483847,8.5131046367489));
#64181=CARTESIAN_POINT('Ctrl Pts',(-19.5347264522261,38.0848340567053,8.57113005579009));
#64182=CARTESIAN_POINT('Ctrl Pts',(-19.506671062814,38.089510965026,8.62766107301773));
#64183=CARTESIAN_POINT('Ctrl Pts',(-19.4791702048946,38.0940954314663,8.68307472099748));
#64184=CARTESIAN_POINT('Ctrl Pts',(-19.4486172226179,38.0986798979065,8.73705202681293));
#64185=CARTESIAN_POINT('Ctrl Pts',(-19.415190728452,38.1032643643468,8.78924012562842));
#64186=CARTESIAN_POINT('Ctrl Pts',(-19.3817846743683,38.1078460274159,8.84139631176353));
#64187=CARTESIAN_POINT('Ctrl Pts',(-19.3455088665287,38.112427690485,8.89176503251976));
#64188=CARTESIAN_POINT('Ctrl Pts',(-19.3065869814173,38.1170093535541,8.94001954016465));
#64189=CARTESIAN_POINT('Ctrl Pts',(-19.2676745989861,38.1215898980217,8.98826226659303));
#64190=CARTESIAN_POINT('Ctrl Pts',(-19.2261177412154,38.1261704424893,9.034391408535));
#64191=CARTESIAN_POINT('Ctrl Pts',(-19.1821811405647,38.1307509869569,9.07811230474259));
#64192=CARTESIAN_POINT('Ctrl Pts',(-19.1366390629114,38.1354989080238,9.12343079594752));
#64193=CARTESIAN_POINT('Ctrl Pts',(-19.08854032802,38.1402468290907,9.1661611799655));
#64194=CARTESIAN_POINT('Ctrl Pts',(-19.0382206640004,38.1449947501577,9.20601791226113));
#64195=CARTESIAN_POINT('Ctrl Pts',(-18.9896133897941,38.1495810983717,9.24451831073169));
#64196=CARTESIAN_POINT('Ctrl Pts',(-18.938934397463,38.1541674465858,9.28033726319256));
#64197=CARTESIAN_POINT('Ctrl Pts',(-18.886517030594,38.1587537947999,9.31326079030887));
#64198=CARTESIAN_POINT('Ctrl Pts',(-18.8313297398854,38.1635825022933,9.3479241160471));
#64199=CARTESIAN_POINT('Ctrl Pts',(-18.7742158154267,38.1684112097866,9.37937719856032));
#64200=CARTESIAN_POINT('Ctrl Pts',(-18.71559230145,38.1732399172799,9.40742603127677));
#64201=CARTESIAN_POINT('Ctrl Pts',(-18.6569687874734,38.1780686247733,9.43547486399322));
#64202=CARTESIAN_POINT('Ctrl Pts',(-18.5968363148,38.1828973322666,9.46011927227349));
#64203=CARTESIAN_POINT('Ctrl Pts',(-18.535631571236,38.18772603976,9.48122574229863));
#64204=CARTESIAN_POINT('Ctrl Pts',(-18.4773622706411,38.1923231574347,9.50131992413451));
#64205=CARTESIAN_POINT('Ctrl Pts',(-18.4178818376672,38.1969202751094,9.51829037444914));
#64206=CARTESIAN_POINT('Ctrl Pts',(-18.3575574810139,38.2015173927841,9.53199433937978));
#64207=CARTESIAN_POINT('Ctrl Pts',(-18.2961860945205,38.2061943011047,9.54593615948215));
#64208=CARTESIAN_POINT('Ctrl Pts',(-18.2339416800988,38.2108712094254,9.55649675940762));
#64209=CARTESIAN_POINT('Ctrl Pts',(-18.1712302821058,38.2155481177461,9.56357781480679));
#64210=CARTESIAN_POINT('Ctrl Pts',(-18.1097584122707,38.2201325841863,9.57051890892562));
#64211=CARTESIAN_POINT('Ctrl Pts',(-18.04783838168,38.2247170506265,9.57411669721915));
#64212=CARTESIAN_POINT('Ctrl Pts',(-17.9858635262238,38.2293015170667,9.57432991367875));
#64213=CARTESIAN_POINT('Ctrl Pts',(-17.9239265679857,38.2338831801358,9.57454299975788));
#64214=CARTESIAN_POINT('Ctrl Pts',(-17.8619353593724,38.2384648432048,9.5713756160478));
#64215=CARTESIAN_POINT('Ctrl Pts',(-17.8002857279752,38.2430465062738,9.56483852211076));
#64216=CARTESIAN_POINT('Ctrl Pts',(-17.7386511481802,38.2476270507413,9.55830302418874));
#64217=CARTESIAN_POINT('Ctrl Pts',(-17.6773584860604,38.2522075952089,9.54839950288427));
#64218=CARTESIAN_POINT('Ctrl Pts',(-17.6167988719718,38.2567881396764,9.53519061257235));
#64219=CARTESIAN_POINT('Ctrl Pts',(-17.5540263632502,38.2615360607433,9.52149905930226));
#64220=CARTESIAN_POINT('Ctrl Pts',(-17.4920420944869,38.2662839818103,9.50425596090198));
#64221=CARTESIAN_POINT('Ctrl Pts',(-17.4312680331346,38.2710319028773,9.48358856718186));
#64222=CARTESIAN_POINT('Ctrl Pts',(-17.3725621271581,38.2756182510913,9.46362448965411));
#64223=CARTESIAN_POINT('Ctrl Pts',(-17.3149858427328,38.2802045993053,9.4404657096611));
#64224=CARTESIAN_POINT('Ctrl Pts',(-17.2588997238343,38.2847909475193,9.41427627946355));
#64225=CARTESIAN_POINT('Ctrl Pts',(-17.1998498109263,38.2896196550127,9.38670290475604));
#64226=CARTESIAN_POINT('Ctrl Pts',(-17.1424524967901,38.2944483625061,9.35576999191488));
#64227=CARTESIAN_POINT('Ctrl Pts',(-17.0870969302704,38.2992770699996,9.3217227502755));
#64228=CARTESIAN_POINT('Ctrl Pts',(-17.0317413637507,38.304105777493,9.28767550863611));
#64229=CARTESIAN_POINT('Ctrl Pts',(-16.9784280336437,38.3089344849864,9.2505143735293));
#64230=CARTESIAN_POINT('Ctrl Pts',(-16.9275059132598,38.3137631924799,9.21053386118251));
#64231=CARTESIAN_POINT('Ctrl Pts',(-16.8790260705578,38.3183603101563,9.17247085565352));
#64232=CARTESIAN_POINT('Ctrl Pts',(-16.8325141158567,38.3229574278327,9.13169640086473));
#64233=CARTESIAN_POINT('Ctrl Pts',(-16.7882891113365,38.3275545455091,9.08844162496235));
#64234=CARTESIAN_POINT('Ctrl Pts',(-16.7432965081072,38.3322314538295,9.0444360902866));
#64235=CARTESIAN_POINT('Ctrl Pts',(-16.7006714757945,38.3369083621499,8.99786356601203));
#64236=CARTESIAN_POINT('Ctrl Pts',(-16.6607168045294,38.3415852704704,8.94901190250561));
#64237=CARTESIAN_POINT('Ctrl Pts',(-16.6215518611389,38.3461697369123,8.90112582122455));
#64238=CARTESIAN_POINT('Ctrl Pts',(-16.5849530149872,38.3507542033542,8.85105029095318));
#64239=CARTESIAN_POINT('Ctrl Pts',(-16.5511682235539,38.3553386697962,8.79909342383743));
#64240=CARTESIAN_POINT('Ctrl Pts',(-16.5174040912993,38.3599203328669,8.74716832800546));
#64241=CARTESIAN_POINT('Ctrl Pts',(-16.4864508786603,38.3645019959376,8.69336460234608));
#64242=CARTESIAN_POINT('Ctrl Pts',(-16.4585141813327,38.3690836590084,8.63802066325994));
#64243=CARTESIAN_POINT('Ctrl Pts',(-16.4305843046794,38.3736642034776,8.58269023625722));
#64244=CARTESIAN_POINT('Ctrl Pts',(-16.4056697106306,38.3782447479468,8.52582079657356));
#64245=CARTESIAN_POINT('Ctrl Pts',(-16.3839298447886,38.3828252924161,8.46777495367685));
#64246=CARTESIAN_POINT('Ctrl Pts',(-16.3613955876316,38.3875732134814,8.40760807131273));
#64247=CARTESIAN_POINT('Ctrl Pts',(-16.3422728282833,38.3923211345467,8.3461776709531));
#64248=CARTESIAN_POINT('Ctrl Pts',(-16.3266834593055,38.397069055612,8.2839072986381));
#64249=CARTESIAN_POINT('Ctrl Pts',(-16.3116246001519,38.4016554038277,8.22375600146463));
#64250=CARTESIAN_POINT('Ctrl Pts',(-16.2998625255837,38.4062417520434,8.16282151842348));
#64251=CARTESIAN_POINT('Ctrl Pts',(-16.2914548993661,38.410828100259,8.10149574234817));
#64252=CARTESIAN_POINT('Ctrl Pts',(-16.2826029836846,38.4156568077492,8.03692928983553));
#64253=CARTESIAN_POINT('Ctrl Pts',(-16.2774699332461,38.4204855152393,7.9719296855735));
#64254=CARTESIAN_POINT('Ctrl Pts',(-16.2760607329453,38.4253142227295,7.90695686389569));
#64255=CARTESIAN_POINT('Ctrl Pts',(-16.2746515326445,38.4301429302196,7.84198404221788));
#64256=CARTESIAN_POINT('Ctrl Pts',(-16.2769660817559,38.4349716377098,7.77703864987683));
#64257=CARTESIAN_POINT('Ctrl Pts',(-16.2829461515228,38.4398003451999,7.71257360142368));
#64258=CARTESIAN_POINT('Ctrl Pts',(-16.2886394109438,38.4443974628727,7.65120036352823));
#64259=CARTESIAN_POINT('Ctrl Pts',(-16.2976779631414,38.4489945805455,7.59001030990863));
#64260=CARTESIAN_POINT('Ctrl Pts',(-16.3100406200581,38.4535916982182,7.5293968512415));
#64261=CARTESIAN_POINT('Ctrl Pts',(-16.3226178515145,38.4582686065391,7.46773134485735));
#64262=CARTESIAN_POINT('Ctrl Pts',(-16.3386357245529,38.46294551486,7.40666317686714));
#64263=CARTESIAN_POINT('Ctrl Pts',(-16.3580165685392,38.4676224231809,7.34660284327611));
#64264=CARTESIAN_POINT('Ctrl Pts',(-16.377014338584,38.4722068896193,7.28772963800249));
#64265=CARTESIAN_POINT('Ctrl Pts',(-16.3992431834038,38.4767913560576,7.22982529685084));
#64266=CARTESIAN_POINT('Ctrl Pts',(-16.4245786752141,38.4813758224959,7.1732652312385));
#64267=CARTESIAN_POINT('Ctrl Pts',(-16.4498986745371,38.4859574855631,7.11673975173547));
#64268=CARTESIAN_POINT('Ctrl Pts',(-16.478321346364,38.4905391486302,7.06155738146749));
#64269=CARTESIAN_POINT('Ctrl Pts',(-16.5096738301586,38.4951208116974,7.00807437102755));
#64270=CARTESIAN_POINT('Ctrl Pts',(-16.5410186593234,38.499701356163,6.9546044183297));
#64271=CARTESIAN_POINT('Ctrl Pts',(-16.5752916231351,38.5042819006287,6.90283344081562));
#64272=CARTESIAN_POINT('Ctrl Pts',(-16.6122745088481,38.5088624450944,6.85309203147319));
#64273=CARTESIAN_POINT('Ctrl Pts',(-16.6506087775312,38.5136103661631,6.80153303293523));
#64274=CARTESIAN_POINT('Ctrl Pts',(-16.6918545511307,38.5183582872319,6.75215530333725));
#64275=CARTESIAN_POINT('Ctrl Pts',(-16.7357220538011,38.5231062083007,6.70529092550838));
#64276=CARTESIAN_POINT('Ctrl Pts',(-16.7780967351684,38.527692556513,6.66002135334033));
#64277=CARTESIAN_POINT('Ctrl Pts',(-16.8229171341829,38.5322789047252,6.6170971241885));
#64278=CARTESIAN_POINT('Ctrl Pts',(-16.8698852428082,38.5368652529374,6.5767791907547));
#64279=CARTESIAN_POINT('Ctrl Pts',(-16.9193353167557,38.5416939604345,6.53433071139147));
#64280=CARTESIAN_POINT('Ctrl Pts',(-16.9711658745846,38.5465226679316,6.49477202020484));
#64281=CARTESIAN_POINT('Ctrl Pts',(-17.0249931735315,38.5513513754286,6.45835670334232));
#64282=CARTESIAN_POINT('Ctrl Pts',(-17.0788204724784,38.5561800829257,6.42194138647981));
#64283=CARTESIAN_POINT('Ctrl Pts',(-17.1346439145111,38.5610087904228,6.38866971000909));
#64284=CARTESIAN_POINT('Ctrl Pts',(-17.1920513776488,38.5658374979199,6.35873834028158));
#64285=CARTESIAN_POINT('Ctrl Pts',(-17.246705519273,38.5704346155938,6.33024251011107));
#64286=CARTESIAN_POINT('Ctrl Pts',(-17.3030197188883,38.5750317332678,6.30465679122923));
#64287=CARTESIAN_POINT('Ctrl Pts',(-17.360651936019,38.5796288509418,6.28217670654351));
#64288=CARTESIAN_POINT('Ctrl Pts',(-17.4192844564284,38.5843057592625,6.25930644248358));
#64289=CARTESIAN_POINT('Ctrl Pts',(-17.4792807570035,38.5889826675833,6.23965097722091));
#64290=CARTESIAN_POINT('Ctrl Pts',(-17.5402538143679,38.593659575904,6.22336764035745));
#64291=CARTESIAN_POINT('Ctrl Pts',(-17.6000217029012,38.5982440423434,6.20740615335526));
#64292=CARTESIAN_POINT('Ctrl Pts',(-17.6607275715857,38.6028285087829,6.19468484152293));
#64293=CARTESIAN_POINT('Ctrl Pts',(-17.7219885219032,38.6074129752223,6.18530272370069));
#64294=CARTESIAN_POINT('Ctrl Pts',(-17.7832120115507,38.6119946382905,6.17592634298207));
#64295=CARTESIAN_POINT('Ctrl Pts',(-17.8449894076318,38.6165763013587,6.16988518440796));
#64296=CARTESIAN_POINT('Ctrl Pts',(-17.9069276484411,38.6211579644269,6.16722718278754));
#64297=CARTESIAN_POINT('Ctrl Pts',(-17.9688507671847,38.6257385088936,6.16456983011153));
#64298=CARTESIAN_POINT('Ctrl Pts',(-18.0309341443209,38.6303190533603,6.1652940164994));
#64299=CARTESIAN_POINT('Ctrl Pts',(-18.0927816840925,38.6348995978269,6.16939565820463));
#64300=CARTESIAN_POINT('Ctrl Pts',(-18.1568891803095,38.6396475188947,6.17364717703744));
#64301=CARTESIAN_POINT('Ctrl Pts',(-18.220742684882,38.6443954399624,6.18152778436431));
#64302=CARTESIAN_POINT('Ctrl Pts',(-18.2839060454256,38.6491433610302,6.19297407558686));
#64303=CARTESIAN_POINT('Ctrl Pts',(-18.3449199421671,38.6537297092433,6.20403084686557));
#64304=CARTESIAN_POINT('Ctrl Pts',(-18.4052894175494,38.6583160574564,6.21841431166702));
#64305=CARTESIAN_POINT('Ctrl Pts',(-18.4646336202325,38.6629024056696,6.23601557848909));
#64306=CARTESIAN_POINT('Ctrl Pts',(-18.5271137859259,38.6677311131646,6.25454696011923));
#64307=CARTESIAN_POINT('Ctrl Pts',(-18.5884567040379,38.6725598206597,6.27664544801783));
#64308=CARTESIAN_POINT('Ctrl Pts',(-18.6482412234039,38.6773885281547,6.30212612020491));
#64309=CARTESIAN_POINT('Ctrl Pts',(-18.7080257427699,38.6822172356498,6.32760679239199));
#64310=CARTESIAN_POINT('Ctrl Pts',(-18.7662513155538,38.6870459431449,6.3564692906635));
#64311=CARTESIAN_POINT('Ctrl Pts',(-18.8225292271859,38.6918746506399,6.3884739837122));
#64312=CARTESIAN_POINT('Ctrl Pts',(-18.8761079919265,38.6964717683256,6.41894369855634));
#64313=CARTESIAN_POINT('Ctrl Pts',(-18.9281417848448,38.7010688860113,6.45238622392788));
#64314=CARTESIAN_POINT('Ctrl Pts',(-18.978280853558,38.7056660036971,6.48862019233682));
#64315=CARTESIAN_POINT('Ctrl Pts',(-19.0292901693113,38.7103429120164,6.52548306161227));
#64316=CARTESIAN_POINT('Ctrl Pts',(-19.0783378532749,38.7150198203356,6.5652350186936));
#64317=CARTESIAN_POINT('Ctrl Pts',(-19.1250818520133,38.7196967286549,6.60763619039921));
#64318=CARTESIAN_POINT('Ctrl Pts',(-19.1709019278808,38.7242811951062,6.64919927778709));
#64319=CARTESIAN_POINT('Ctrl Pts',(-19.2145081616957,38.7288656615575,6.69330744776144));
#64320=CARTESIAN_POINT('Ctrl Pts',(-19.255609730549,38.7334501280088,6.73969267412414));
#64321=CARTESIAN_POINT('Ctrl Pts',(-19.2966861660623,38.7380317910889,6.78604953622483));
#64322=CARTESIAN_POINT('Ctrl Pts',(-19.3352606366053,38.742613454169,6.83468031355844));
#64323=CARTESIAN_POINT('Ctrl Pts',(-19.3710797301173,38.747195117249,6.88528074048647));
#64324=CARTESIAN_POINT('Ctrl Pts',(-19.4068900784875,38.7517756617276,6.93586881344735));
#64325=CARTESIAN_POINT('Ctrl Pts',(-19.4399460912709,38.7563562062061,6.98842516605705));
#64326=CARTESIAN_POINT('Ctrl Pts',(-19.4700364182083,38.7609367506847,7.04261477653218));
#64327=CARTESIAN_POINT('Ctrl Pts',(-19.501226268569,38.765684671741,7.09878451657302));
#64328=CARTESIAN_POINT('Ctrl Pts',(-19.529229161916,38.7704325927972,7.15670870806836));
#64329=CARTESIAN_POINT('Ctrl Pts',(-19.5538618699681,38.7751805138535,7.2159865063621));
#64330=CARTESIAN_POINT('Ctrl Pts',(-19.577656321373,38.7797668620783,7.27324706772241));
#64331=CARTESIAN_POINT('Ctrl Pts',(-19.598306184779,38.7843532103032,7.33177006130215));
#64332=CARTESIAN_POINT('Ctrl Pts',(-19.6156964376789,38.788939558528,7.39117644234587));
#64333=CARTESIAN_POINT('Ctrl Pts',(-19.6340056545113,38.793768266,7.45372207167173));
#64334=CARTESIAN_POINT('Ctrl Pts',(-19.6487010506658,38.798596973472,7.51724641394041));
#64335=CARTESIAN_POINT('Ctrl Pts',(-19.6597096334922,38.803425680944,7.58129533645361));
#64336=CARTESIAN_POINT('Ctrl Pts',(-19.6707182163187,38.8082543884159,7.64534425896682));
#64337=CARTESIAN_POINT('Ctrl Pts',(-19.678039989725,38.8130830958879,7.70991710718719));
#64338=CARTESIAN_POINT('Ctrl Pts',(-19.6816655175308,38.8179118033599,7.77455733633969));
#64339=CARTESIAN_POINT('Ctrl Pts',(-19.6834369986343,38.8202711740499,7.80614141198337));
#64340=CARTESIAN_POINT('Ctrl Pts',(-19.684329226899,38.8226305447399,7.83777526298266));
#64341=CARTESIAN_POINT('Ctrl Pts',(-19.6843399030357,38.8249899154298,7.86942509116366));
#64342=CARTESIAN_POINT('',(-19.6843395759433,39.6187399153728,7.8687977216301));
#64343=CARTESIAN_POINT('Ctrl Pts',(-19.6843399030359,38.8249899154737,7.86942509175251));
#64344=CARTESIAN_POINT('Ctrl Pts',(-19.6843605266318,38.829547627553,7.93056461714531));
#64345=CARTESIAN_POINT('Ctrl Pts',(-19.68108701094,38.8341053396324,7.99183752883473));
#64346=CARTESIAN_POINT('Ctrl Pts',(-19.6745024781758,38.8386630517117,8.05285564540372));
#64347=CARTESIAN_POINT('Ctrl Pts',(-19.6679289612082,38.8432131388264,8.11377167983781));
#64348=CARTESIAN_POINT('Ctrl Pts',(-19.6580554746227,38.8477632259412,8.17443325378262));
#64349=CARTESIAN_POINT('Ctrl Pts',(-19.6449171408284,38.8523133130559,8.2344526715167));
#64350=CARTESIAN_POINT('Ctrl Pts',(-19.6317909666354,38.8568591890396,8.29441654094461));
#64351=CARTESIAN_POINT('Ctrl Pts',(-19.61540604119,38.8614050650233,8.35373892732559));
#64352=CARTESIAN_POINT('Ctrl Pts',(-19.5958490092529,38.865950941007,8.41203949569782));
#64353=CARTESIAN_POINT('Ctrl Pts',(-19.5763025908541,38.8704943499585,8.47030842453947));
#64354=CARTESIAN_POINT('Ctrl Pts',(-19.5535876426938,38.8750377589099,8.52755614371076));
#64355=CARTESIAN_POINT('Ctrl Pts',(-19.5278408334042,38.8795811678614,8.58341684171773));
#64356=CARTESIAN_POINT('Ctrl Pts',(-19.5020981414711,38.8841238502438,8.6392686066408));
#64357=CARTESIAN_POINT('Ctrl Pts',(-19.4733247686859,38.8886665326262,8.69373332027379));
#64358=CARTESIAN_POINT('Ctrl Pts',(-19.4417048915243,38.8932092150087,8.74646656849764));
#64359=CARTESIAN_POINT('Ctrl Pts',(-19.4100557842604,38.8977560967455,8.79924856448326));
#64360=CARTESIAN_POINT('Ctrl Pts',(-19.375555184547,38.9023029784823,8.85029545262463));
#64361=CARTESIAN_POINT('Ctrl Pts',(-19.3384317914997,38.9068498602192,8.89928999968087));
#64362=CARTESIAN_POINT('Ctrl Pts',(-19.3012908955347,38.9113988857174,8.94830764666006));
#64363=CARTESIAN_POINT('Ctrl Pts',(-19.2615250799658,38.9159479112156,8.99527062998618));
#64364=CARTESIAN_POINT('Ctrl Pts',(-19.2194026985627,38.9204969367138,9.0398956305566));
#64365=CARTESIAN_POINT('Ctrl Pts',(-19.1772031503065,38.925054295881,9.08460238269823));
#64366=CARTESIAN_POINT('Ctrl Pts',(-19.1326387927123,38.9296116550482,9.1269622424915));
#64367=CARTESIAN_POINT('Ctrl Pts',(-19.0860133208819,38.9341690142153,9.16673026093779));
#64368=CARTESIAN_POINT('Ctrl Pts',(-19.0526610813367,38.9374289948369,9.19517721118597));
#64369=CARTESIAN_POINT('Ctrl Pts',(-19.018254926862,38.9406889754584,9.22229878469583));
#64370=CARTESIAN_POINT('Ctrl Pts',(-18.982914803714,38.9439489560799,9.24801913342716));
#64371=CARTESIAN_POINT('Ctrl Pts',(-18.933079321978,38.9485460737539,9.28428912501935));
#64372=CARTESIAN_POINT('Ctrl Pts',(-18.8811714116231,38.9531431914279,9.3179267070985));
#64373=CARTESIAN_POINT('Ctrl Pts',(-18.8275004130645,38.9577403091019,9.34868789318622));
#64374=CARTESIAN_POINT('Ctrl Pts',(-18.7728978647845,38.9624172174226,9.37998299097858));
#64375=CARTESIAN_POINT('Ctrl Pts',(-18.7164708149572,38.9670941257434,9.40830050220937));
#64376=CARTESIAN_POINT('Ctrl Pts',(-18.6585787436045,38.9717710340641,9.43342755646948));
#64377=CARTESIAN_POINT('Ctrl Pts',(-18.6018309435631,38.9763555005031,9.45805795951889));
#64378=CARTESIAN_POINT('Ctrl Pts',(-18.5436759985838,38.980939966942,9.47962266770406));
#64379=CARTESIAN_POINT('Ctrl Pts',(-18.4844779382697,38.985524433381,9.49796708977768));
#64380=CARTESIAN_POINT('Ctrl Pts',(-18.425316077184,38.9901060964486,9.51630029435663));
#64381=CARTESIAN_POINT('Ctrl Pts',(-18.3651128507941,38.9946877595161,9.53141696704901));
#64382=CARTESIAN_POINT('Ctrl Pts',(-18.3042498995799,38.9992694225837,9.54321153421271));
#64383=CARTESIAN_POINT('Ctrl Pts',(-18.2434018079045,39.0038499670496,9.55500322176203));
#64384=CARTESIAN_POINT('Ctrl Pts',(-18.1818948107058,39.0084305115155,9.56347431709158));
#64385=CARTESIAN_POINT('Ctrl Pts',(-18.1201212469924,39.0130110559814,9.56857024339333));
#64386=CARTESIAN_POINT('Ctrl Pts',(-18.056090429958,39.0177589770496,9.57385237874434));
#64387=CARTESIAN_POINT('Ctrl Pts',(-17.9917737632777,39.0225068981178,9.575507795877));
#64388=CARTESIAN_POINT('Ctrl Pts',(-17.927611980059,39.027254819186,9.57353465798811));
#64389=CARTESIAN_POINT('Ctrl Pts',(-17.8656336372198,39.0318411673979,9.57162866643969));
#64390=CARTESIAN_POINT('Ctrl Pts',(-17.8038003251905,39.0364275156098,9.56633724512009));
#64391=CARTESIAN_POINT('Ctrl Pts',(-17.7425048162126,39.0410138638217,9.557711726948));
#64392=CARTESIAN_POINT('Ctrl Pts',(-17.6779702300848,39.0458425713181,9.5486304050917));
#64393=CARTESIAN_POINT('Ctrl Pts',(-17.6140324978053,39.0506712788145,9.53585295760223));
#64394=CARTESIAN_POINT('Ctrl Pts',(-17.5511354989815,39.0554999863108,9.51949994706461));
#64395=CARTESIAN_POINT('Ctrl Pts',(-17.4882385001577,39.0603286938072,9.503146936527));
#64396=CARTESIAN_POINT('Ctrl Pts',(-17.4263828296021,39.0651574013035,9.48321863613079));
#64397=CARTESIAN_POINT('Ctrl Pts',(-17.3659883835307,39.0699861087999,9.45989451550748));
#64398=CARTESIAN_POINT('Ctrl Pts',(-17.3084905167746,39.0745832265531,9.43768904353049));
#64399=CARTESIAN_POINT('Ctrl Pts',(-17.2520806849564,39.0791803443063,9.41231486187921));
#64400=CARTESIAN_POINT('Ctrl Pts',(-17.197131629014,39.0837774620595,9.38389958362823));
#64401=CARTESIAN_POINT('Ctrl Pts',(-17.1412288416141,39.0884543703704,9.35499111137642));
#64402=CARTESIAN_POINT('Ctrl Pts',(-17.0868385511607,39.0931312786812,9.32293507173071));
#64403=CARTESIAN_POINT('Ctrl Pts',(-17.0343345422624,39.0978081869921,9.28791807860746));
#64404=CARTESIAN_POINT('Ctrl Pts',(-16.9828683053979,39.1023926535113,9.25359321656022));
#64405=CARTESIAN_POINT('Ctrl Pts',(-16.9332149059744,39.1069771200305,9.21642368176465));
#64406=CARTESIAN_POINT('Ctrl Pts',(-16.8857016283261,39.1115615865497,9.17663151245937));
#64407=CARTESIAN_POINT('Ctrl Pts',(-16.8382174047356,39.1161432496977,9.13686367580475));
#64408=CARTESIAN_POINT('Ctrl Pts',(-16.7928710974951,39.1207249128458,9.09447671076512));
#64409=CARTESIAN_POINT('Ctrl Pts',(-16.7499583548246,39.1253065759938,9.04973403220139));
#64410=CARTESIAN_POINT('Ctrl Pts',(-16.7070560891935,39.1298871205401,9.0050022774514));
#64411=CARTESIAN_POINT('Ctrl Pts',(-16.6665865608835,39.1344676650864,8.95791631815617));
#64412=CARTESIAN_POINT('Ctrl Pts',(-16.6288083708181,39.1390482096328,8.90877621113923));
#64413=CARTESIAN_POINT('Ctrl Pts',(-16.5896497380871,39.1437961306234,8.85784048871027));
#64414=CARTESIAN_POINT('Ctrl Pts',(-16.5533833437414,39.148544051614,8.80469801499726));
#64415=CARTESIAN_POINT('Ctrl Pts',(-16.5202497170263,39.1532919726046,8.74971810653079));
#64416=CARTESIAN_POINT('Ctrl Pts',(-16.4882436342424,39.1578783208961,8.69660917532453));
#64417=CARTESIAN_POINT('Ctrl Pts',(-16.4591606981488,39.1624646691876,8.64178636464811));
#64418=CARTESIAN_POINT('Ctrl Pts',(-16.4331707571701,39.1670510174791,8.58560752450374));
#64419=CARTESIAN_POINT('Ctrl Pts',(-16.4058074147467,39.1718797248192,8.52645999350002));
#64420=CARTESIAN_POINT('Ctrl Pts',(-16.381873270837,39.1767084321594,8.46580973999901));
#64421=CARTESIAN_POINT('Ctrl Pts',(-16.3615077185165,39.1815371394995,8.40409509488335));
#64422=CARTESIAN_POINT('Ctrl Pts',(-16.3411421661961,39.1863658468396,8.3423804497677));
#64423=CARTESIAN_POINT('Ctrl Pts',(-16.3243452984608,39.1911945541798,8.27960206094635));
#64424=CARTESIAN_POINT('Ctrl Pts',(-16.3111940086415,39.1960232615199,8.21621005012255));
#64425=CARTESIAN_POINT('Ctrl Pts',(-16.2986734683704,39.20062037903,8.15585838611979));
#64426=CARTESIAN_POINT('Ctrl Pts',(-16.2894053224898,39.2052174965402,8.09470268886554));
#64427=CARTESIAN_POINT('Ctrl Pts',(-16.2834844654515,39.2098146140503,8.03312534026237));
#64428=CARTESIAN_POINT('Ctrl Pts',(-16.2774608418202,39.2144915223915,7.97047921153508));
#64429=CARTESIAN_POINT('Ctrl Pts',(-16.2749020118353,39.2191684307327,7.90739715505296));
#64430=CARTESIAN_POINT('Ctrl Pts',(-16.2758538622243,39.223845339074,7.84429442270082));
#64431=CARTESIAN_POINT('Ctrl Pts',(-16.2767868986858,39.2284298053507,7.78243895594146));
#64432=CARTESIAN_POINT('Ctrl Pts',(-16.2810930889719,39.2330142716274,7.72056415694667));
#64433=CARTESIAN_POINT('Ctrl Pts',(-16.2887633409867,39.2375987379042,7.65906541580508));
#64434=CARTESIAN_POINT('Ctrl Pts',(-16.2964289026938,39.2421804008105,7.59760428073067));
#64435=CARTESIAN_POINT('Ctrl Pts',(-16.3074543843327,39.2467620637169,7.53651925165197));
#64436=CARTESIAN_POINT('Ctrl Pts',(-16.3217787737923,39.2513437266233,7.47620157370288));
#64437=CARTESIAN_POINT('Ctrl Pts',(-16.3360996659915,39.2559242709293,7.4158986221489));
#64438=CARTESIAN_POINT('Ctrl Pts',(-16.3537177495671,39.2605048152353,7.35636314489289));
#64439=CARTESIAN_POINT('Ctrl Pts',(-16.3745211363523,39.2650853595413,7.29797512818008));
#64440=CARTESIAN_POINT('Ctrl Pts',(-16.3960846962851,39.2698332807662,7.23745356451644));
#64441=CARTESIAN_POINT('Ctrl Pts',(-16.4210707179747,39.2745812019911,7.17816551312208));
#64442=CARTESIAN_POINT('Ctrl Pts',(-16.4492993205381,39.279329123216,7.12051333200989));
#64443=CARTESIAN_POINT('Ctrl Pts',(-16.4765672953818,39.283915471273,7.0648230717245));
#64444=CARTESIAN_POINT('Ctrl Pts',(-16.5068603707055,39.28850181933,7.0106595512061));
#64445=CARTESIAN_POINT('Ctrl Pts',(-16.5399699736584,39.2930881673871,6.95835952325786));
#64446=CARTESIAN_POINT('Ctrl Pts',(-16.5748292116265,39.2979168751959,6.90329576660154));
#64447=CARTESIAN_POINT('Ctrl Pts',(-16.6128105375504,39.3027455830047,6.85029844399803));
#64448=CARTESIAN_POINT('Ctrl Pts',(-16.6536212425395,39.3075742908135,6.79972235968539));
#64449=CARTESIAN_POINT('Ctrl Pts',(-16.6944319475285,39.3124029986223,6.74914627537275));
#64450=CARTESIAN_POINT('Ctrl Pts',(-16.7380715376231,39.3172317064311,6.70099185881445));
#64451=CARTESIAN_POINT('Ctrl Pts',(-16.784203506772,39.3220604142399,6.65556779424143));
#64452=CARTESIAN_POINT('Ctrl Pts',(-16.8281229364164,39.326657531961,6.61232231729808));
#64453=CARTESIAN_POINT('Ctrl Pts',(-16.8744815298284,39.331254649682,6.5713735816584));
#64454=CARTESIAN_POINT('Ctrl Pts',(-16.9230094584221,39.3358517674031,6.53300866471959));
#64455=CARTESIAN_POINT('Ctrl Pts',(-16.9723796696096,39.340528675718,6.49397786109065));
#64456=CARTESIAN_POINT('Ctrl Pts',(-17.023994927625,39.3452055840328,6.457621864394));
#64457=CARTESIAN_POINT('Ctrl Pts',(-17.0775312116696,39.3498824923477,6.42420439837113));
#64458=CARTESIAN_POINT('Ctrl Pts',(-17.130009319699,39.35446695883,6.39144744813983));
#64459=CARTESIAN_POINT('Ctrl Pts',(-17.1843327517215,39.3590514253124,6.36151420496099));
#64460=CARTESIAN_POINT('Ctrl Pts',(-17.2401643630905,39.3636358917947,6.3346114283483));
#64461=CARTESIAN_POINT('Ctrl Pts',(-17.2959618337749,39.3682175549042,6.30772510261687));
#64462=CARTESIAN_POINT('Ctrl Pts',(-17.3532651974793,39.3727992180137,6.28386578953471));
#64463=CARTESIAN_POINT('Ctrl Pts',(-17.4117126387867,39.3773808811231,6.26319437681925));
#64464=CARTESIAN_POINT('Ctrl Pts',(-17.4701458102765,39.3819614256294,6.24252801098495));
#64465=CARTESIAN_POINT('Ctrl Pts',(-17.5297220251438,39.3865419701356,6.22504817011098));
#64466=CARTESIAN_POINT('Ctrl Pts',(-17.59006134055,39.3911225146419,6.21086688976854));
#64467=CARTESIAN_POINT('Ctrl Pts',(-17.6526054996454,39.3958704356684,6.19616741484173));
#64468=CARTESIAN_POINT('Ctrl Pts',(-17.7159690551745,39.4006183566949,6.18501242633746));
#64469=CARTESIAN_POINT('Ctrl Pts',(-17.7797163984031,39.4053662777214,6.17746896201831));
#64470=CARTESIAN_POINT('Ctrl Pts',(-17.8412944057669,39.4099526259694,6.17018220341996));
#64471=CARTESIAN_POINT('Ctrl Pts',(-17.9032299665162,39.4145389742174,6.16626506269091));
#64472=CARTESIAN_POINT('Ctrl Pts',(-17.9651270364674,39.4191253224654,6.16572489587046));
#64473=CARTESIAN_POINT('Ctrl Pts',(-18.0302949706326,39.4239540298812,6.1651561846888));
#64474=CARTESIAN_POINT('Ctrl Pts',(-18.0954195876102,39.4287827372969,6.16833122856295));
#64475=CARTESIAN_POINT('Ctrl Pts',(-18.1600440537407,39.4336114447127,6.17519647914202));
#64476=CARTESIAN_POINT('Ctrl Pts',(-18.2246685198713,39.4384401521284,6.18206172972109));
#64477=CARTESIAN_POINT('Ctrl Pts',(-18.2887922064639,39.4432688595442,6.19261700484584));
#64478=CARTESIAN_POINT('Ctrl Pts',(-18.3519732819213,39.4480975669599,6.20674694855633));
#64479=CARTESIAN_POINT('Ctrl Pts',(-18.4121241356718,39.4526946851866,6.22019920734551));
#64480=CARTESIAN_POINT('Ctrl Pts',(-18.4716678499828,39.4572918034133,6.23694629958069));
#64481=CARTESIAN_POINT('Ctrl Pts',(-18.5302169031767,39.46188892164,6.25691717662774));
#64482=CARTESIAN_POINT('Ctrl Pts',(-18.5897821648267,39.4665658298917,6.27723467882111));
#64483=CARTESIAN_POINT('Ctrl Pts',(-18.6483173698797,39.4712427381433,6.30088891746777));
#64484=CARTESIAN_POINT('Ctrl Pts',(-18.7054252334764,39.475919646395,6.32775064719233));
#64485=CARTESIAN_POINT('Ctrl Pts',(-18.7614043337383,39.4805041133921,6.35408144240603));
#64486=CARTESIAN_POINT('Ctrl Pts',(-18.8160115200929,39.4850885803892,6.38349386045697));
#64487=CARTESIAN_POINT('Ctrl Pts',(-18.8688902536374,39.4896730473864,6.41581674036991));
#64488=CARTESIAN_POINT('Ctrl Pts',(-18.9217366521901,39.4942547110126,6.44811985505796));
#64489=CARTESIAN_POINT('Ctrl Pts',(-18.9728562602278,39.4988363746388,6.48332963772018));
#64490=CARTESIAN_POINT('Ctrl Pts',(-19.0219177035941,39.503418038265,6.52122932470449));
#64491=CARTESIAN_POINT('Ctrl Pts',(-19.0709671687274,39.5079985832891,6.5591197585716));
#64492=CARTESIAN_POINT('Ctrl Pts',(-19.1179590640269,39.5125791283132,6.59969848197639));
#64493=CARTESIAN_POINT('Ctrl Pts',(-19.1625932323363,39.5171596733373,6.64270701035473));
#64494=CARTESIAN_POINT('Ctrl Pts',(-19.2088583564377,39.5219075938658,6.68728709279397));
#64495=CARTESIAN_POINT('Ctrl Pts',(-19.2525896491255,39.5266555143944,6.73447763243855));
#64496=CARTESIAN_POINT('Ctrl Pts',(-19.2934945768315,39.5314034349229,6.78394897346661));
#64497=CARTESIAN_POINT('Ctrl Pts',(-19.333007509586,39.5359897836855,6.83173680444298));
#64498=CARTESIAN_POINT('Ctrl Pts',(-19.3698831051157,39.5405761324481,6.88165222235139));
#64499=CARTESIAN_POINT('Ctrl Pts',(-19.4039004291453,39.5451624812107,6.93336645187149));
#64500=CARTESIAN_POINT('Ctrl Pts',(-19.439715339687,39.5499911876222,6.98781343019293));
#64501=CARTESIAN_POINT('Ctrl Pts',(-19.4723611869233,39.5548198940338,7.04425404942017));
#64502=CARTESIAN_POINT('Ctrl Pts',(-19.5016352469356,39.5596486004453,7.10227543292967));
#64503=CARTESIAN_POINT('Ctrl Pts',(-19.5309093069479,39.5644773068568,7.16029681643917));
#64504=CARTESIAN_POINT('Ctrl Pts',(-19.5568113918848,39.5693060132684,7.21989833721848));
#64505=CARTESIAN_POINT('Ctrl Pts',(-19.5791988445213,39.5741347196799,7.28064620873227));
#64506=CARTESIAN_POINT('Ctrl Pts',(-19.6037514026038,39.5794304135025,7.34726904733508));
#64507=CARTESIAN_POINT('Ctrl Pts',(-19.6241618666497,39.5847261073252,7.41549605425292));
#64508=CARTESIAN_POINT('Ctrl Pts',(-19.6402487498504,39.5900218011479,7.48483909307897));
#64509=CARTESIAN_POINT('Ctrl Pts',(-19.6561960370784,39.5952715409146,7.55358039887612));
#64510=CARTESIAN_POINT('Ctrl Pts',(-19.6678943533168,39.6005212806814,7.62341826524155));
#64511=CARTESIAN_POINT('Ctrl Pts',(-19.6752133150058,39.6057710204481,7.69385616040597));
#64512=CARTESIAN_POINT('Ctrl Pts',(-19.6812402070881,39.610093985423,7.7518591409785));
#64513=CARTESIAN_POINT('Ctrl Pts',(-19.6842982882008,39.6144169503979,7.81026856950894));
#64514=CARTESIAN_POINT('Ctrl Pts',(-19.6843395759433,39.6187399153728,7.86879772163009));
#64515=CARTESIAN_POINT('',(-19.6843395514373,40.4124899154864,7.8712365300618));
#64516=CARTESIAN_POINT('Ctrl Pts',(-19.6843395759439,39.6187399154298,7.86879772240173));
#64517=CARTESIAN_POINT('Ctrl Pts',(-19.6843834605849,39.623334787325,7.93100825561096));
#64518=CARTESIAN_POINT('Ctrl Pts',(-19.6810168737825,39.6279296592201,7.99324607275286));
#64519=CARTESIAN_POINT('Ctrl Pts',(-19.6742574015537,39.6325245311153,8.05511264916427));
#64520=CARTESIAN_POINT('Ctrl Pts',(-19.6674980385379,39.6371193287709,8.11697822599498));
#64521=CARTESIAN_POINT('Ctrl Pts',(-19.65734595536,39.6417141264265,8.17847207298165));
#64522=CARTESIAN_POINT('Ctrl Pts',(-19.6438705362152,39.6463089240822,8.23920140074895));
#64523=CARTESIAN_POINT('Ctrl Pts',(-19.6303798438661,39.6509089295375,8.29999955987628));
#64524=CARTESIAN_POINT('Ctrl Pts',(-19.6135584020532,39.6555089349927,8.36003097560791));
#64525=CARTESIAN_POINT('Ctrl Pts',(-19.5935264115865,39.660108940448,8.41891470622755));
#64526=CARTESIAN_POINT('Ctrl Pts',(-19.5734833716148,39.6647114832339,8.47783091669856));
#64527=CARTESIAN_POINT('Ctrl Pts',(-19.5502264444524,39.6693140260199,8.53559771268408));
#64528=CARTESIAN_POINT('Ctrl Pts',(-19.5239241603994,39.6739165688058,8.59185387893595));
#64529=CARTESIAN_POINT('Ctrl Pts',(-19.4975679111077,39.6785285547762,8.64822546776632));
#64530=CARTESIAN_POINT('Ctrl Pts',(-19.4681540596482,39.6831405407466,8.70307978841625));
#64531=CARTESIAN_POINT('Ctrl Pts',(-19.4358969845023,39.6877525267169,8.7560805866947));
#64532=CARTESIAN_POINT('Ctrl Pts',(-19.4069425912083,39.6918923086113,8.80365483052499));
#64533=CARTESIAN_POINT('Ctrl Pts',(-19.375698142922,39.6960320905056,8.84973584474876));
#64534=CARTESIAN_POINT('Ctrl Pts',(-19.3423463698601,39.7001718723999,8.8941031218237));
#64535=CARTESIAN_POINT('Ctrl Pts',(-19.3053101067791,39.7047689908515,8.94337181116394));
#64536=CARTESIAN_POINT('Ctrl Pts',(-19.2655216553048,39.709366109303,8.99073000183231));
#64537=CARTESIAN_POINT('Ctrl Pts',(-19.2232053905419,39.7139632277546,9.03585384698407));
#64538=CARTESIAN_POINT('Ctrl Pts',(-19.1801546645829,39.7186401359782,9.08176088303107));
#64539=CARTESIAN_POINT('Ctrl Pts',(-19.1344877834538,39.7233170442017,9.12535479199504));
#64540=CARTESIAN_POINT('Ctrl Pts',(-19.0864861736111,39.7279939524253,9.16632680416915));
#64541=CARTESIAN_POINT('Ctrl Pts',(-19.0394333355832,39.7325784196095,9.20648898745478));
#64542=CARTESIAN_POINT('Ctrl Pts',(-18.9901376285894,39.7371628867938,9.2441316298211));
#64543=CARTESIAN_POINT('Ctrl Pts',(-18.938901888341,39.741747353978,9.27900035632927));
#64544=CARTESIAN_POINT('Ctrl Pts',(-18.8876974785648,39.7463290177769,9.31384776073568));
#64545=CARTESIAN_POINT('Ctrl Pts',(-18.8345558078204,39.7509106815759,9.34592432684974));
#64546=CARTESIAN_POINT('Ctrl Pts',(-18.7798108992277,39.7554923453748,9.37501739560596));
#64547=CARTESIAN_POINT('Ctrl Pts',(-18.7250793566459,39.760072890557,9.40410336126743));
#64548=CARTESIAN_POINT('Ctrl Pts',(-18.6687458026009,39.7646534357393,9.43020703680343));
#64549=CARTESIAN_POINT('Ctrl Pts',(-18.6111694173609,39.7692339809215,9.45316139486417));
#64550=CARTESIAN_POINT('Ctrl Pts',(-18.5514891652782,39.7739819012714,9.47695451542484));
#64551=CARTESIAN_POINT('Ctrl Pts',(-18.4904740137347,39.7787298216212,9.49736343306464));
#64552=CARTESIAN_POINT('Ctrl Pts',(-18.4285448545843,39.7834777419711,9.51425738527334));
#64553=CARTESIAN_POINT('Ctrl Pts',(-18.3687231412914,39.7880640908543,9.53057643722366));
#64554=CARTESIAN_POINT('Ctrl Pts',(-18.3080491634902,39.7926504397375,9.54361588246976));
#64555=CARTESIAN_POINT('Ctrl Pts',(-18.2469135163627,39.7972367886208,9.55330983790355));
#64556=CARTESIAN_POINT('Ctrl Pts',(-18.1825472680243,39.8020654947039,9.56351605264325));
#64557=CARTESIAN_POINT('Ctrl Pts',(-18.1176698464845,39.8068942007871,9.57001332349494));
#64558=CARTESIAN_POINT('Ctrl Pts',(-18.0527409794033,39.8117229068703,9.57278700532846));
#64559=CARTESIAN_POINT('Ctrl Pts',(-17.9878121123222,39.8165516129535,9.57556068716197));
#64560=CARTESIAN_POINT('Ctrl Pts',(-17.9228324484238,39.8213803190367,9.57461086709453));
#64561=CARTESIAN_POINT('Ctrl Pts',(-17.8582560250215,39.8262090251199,9.5699862470492));
#64562=CARTESIAN_POINT('Ctrl Pts',(-17.7967766858213,39.8308061465389,9.56558342370503));
#64563=CARTESIAN_POINT('Ctrl Pts',(-17.7354102222827,39.8354032679579,9.55783219221645));
#64564=CARTESIAN_POINT('Ctrl Pts',(-17.6745504038976,39.840000389377,9.54674547258696));
#64565=CARTESIAN_POINT('Ctrl Pts',(-17.6126343184671,39.8446772972296,9.53546633475944));
#64566=CARTESIAN_POINT('Ctrl Pts',(-17.5512431682437,39.8493542050822,9.52073476806028));
#64567=CARTESIAN_POINT('Ctrl Pts',(-17.4907889895575,39.8540311129348,9.50261980352494));
#64568=CARTESIAN_POINT('Ctrl Pts',(-17.4315296688199,39.8586155831654,9.48486287560235));
#64569=CARTESIAN_POINT('Ctrl Pts',(-17.3731711301398,39.8632000533959,9.46385522942179));
#64570=CARTESIAN_POINT('Ctrl Pts',(-17.3160913162341,39.8677845236265,9.43971337995834));
#64571=CARTESIAN_POINT('Ctrl Pts',(-17.2590464061497,39.8723661904924,9.41558629303074));
#64572=CARTESIAN_POINT('Ctrl Pts',(-17.2032791382798,39.8769478573583,9.38832900092216));
#64573=CARTESIAN_POINT('Ctrl Pts',(-17.1491493160739,39.8815295242243,9.35810684314653));
#64574=CARTESIAN_POINT('Ctrl Pts',(-17.0950327095123,39.8861100724891,9.32789206402595));
#64575=CARTESIAN_POINT('Ctrl Pts',(-17.0425531992868,39.8906906207539,9.29471410426889));
#64576=CARTESIAN_POINT('Ctrl Pts',(-16.9920458895369,39.8952711690188,9.25878418453662));
#64577=CARTESIAN_POINT('Ctrl Pts',(-16.9396930878605,39.9000190864205,9.22154141767166));
#64578=CARTESIAN_POINT('Ctrl Pts',(-16.8894599130539,39.9047670038223,9.18134197493637));
#64579=CARTESIAN_POINT('Ctrl Pts',(-16.8416844604441,39.909514921224,9.13846859165122));
#64580=CARTESIAN_POINT('Ctrl Pts',(-16.7955347441432,39.9141012731923,9.09705413365267));
#64581=CARTESIAN_POINT('Ctrl Pts',(-16.7516784831589,39.9186876251606,9.05314522856172));
#64582=CARTESIAN_POINT('Ctrl Pts',(-16.7103828329202,39.9232739771288,9.00703433750092));
#64583=CARTESIAN_POINT('Ctrl Pts',(-16.6669050726911,39.9281026772473,8.95848689354746));
#64584=CARTESIAN_POINT('Ctrl Pts',(-16.6262664506392,39.9329313773658,8.90749879688026));
#64585=CARTESIAN_POINT('Ctrl Pts',(-16.5887285565003,39.9377600774844,8.85444837655531));
#64586=CARTESIAN_POINT('Ctrl Pts',(-16.5511906623615,39.9425887776029,8.80139795623036));
#64587=CARTESIAN_POINT('Ctrl Pts',(-16.5167537747039,39.9474174777214,8.74628580455052));
#64588=CARTESIAN_POINT('Ctrl Pts',(-16.4856231727145,39.9522461778399,8.68951981896229));
#64589=CARTESIAN_POINT('Ctrl Pts',(-16.45598565322,39.9568432843765,8.63547643730633));
#64590=CARTESIAN_POINT('Ctrl Pts',(-16.4292227170486,39.9614403909132,8.57971224002759));
#64591=CARTESIAN_POINT('Ctrl Pts',(-16.4055370287649,39.9660374974498,8.52256508319814));
#64592=CARTESIAN_POINT('Ctrl Pts',(-16.3814401702935,39.9707144071627,8.46442588396258));
#64593=CARTESIAN_POINT('Ctrl Pts',(-16.3605287557726,39.9753913168757,8.40485567186033));
#64594=CARTESIAN_POINT('Ctrl Pts',(-16.3429682111376,39.9800682265886,8.3442380814043));
#64595=CARTESIAN_POINT('Ctrl Pts',(-16.3257548079632,39.9846526819214,8.28481879540422));
#64596=CARTESIAN_POINT('Ctrl Pts',(-16.311761147436,39.9892371372542,8.22439367651532));
#64597=CARTESIAN_POINT('Ctrl Pts',(-16.3010942695617,39.993821592587,8.16334345723332));
#64598=CARTESIAN_POINT('Ctrl Pts',(-16.2904339143323,39.9984032445902,8.10233056929643));
#64599=CARTESIAN_POINT('Ctrl Pts',(-16.2830963955218,40.0029848965935,8.04069383933047));
#64600=CARTESIAN_POINT('Ctrl Pts',(-16.279137893869,40.0075665485967,7.97882523387381));
#64601=CARTESIAN_POINT('Ctrl Pts',(-16.2751803586257,40.0121470820576,7.91697173271963));
#64602=CARTESIAN_POINT('Ctrl Pts',(-16.2746002354141,40.0167276155185,7.85488697626326));
#64603=CARTESIAN_POINT('Ctrl Pts',(-16.2774017616269,40.0213081489793,7.7929670571187));
#64604=CARTESIAN_POINT('Ctrl Pts',(-16.2803056712924,40.0260560807777,7.72878423746007));
#64605=CARTESIAN_POINT('Ctrl Pts',(-16.2868432222247,40.0308040125761,7.66477912115993));
#64606=CARTESIAN_POINT('Ctrl Pts',(-16.2969601845755,40.0355519443745,7.60138910056386));
#64607=CARTESIAN_POINT('Ctrl Pts',(-16.3067328193948,40.0401382818543,7.54015653875443));
#64608=CARTESIAN_POINT('Ctrl Pts',(-16.3198449356221,40.0447246193342,7.47949837470028));
#64609=CARTESIAN_POINT('Ctrl Pts',(-16.336195665568,40.0493109568141,7.4197976613759));
#64610=CARTESIAN_POINT('Ctrl Pts',(-16.3534105442188,40.0541396857717,7.35694171924702));
#64611=CARTESIAN_POINT('Ctrl Pts',(-16.3742156630405,40.0589684147294,7.2951478547041));
#64612=CARTESIAN_POINT('Ctrl Pts',(-16.3984349834176,40.063797143687,7.23484101681334));
#64613=CARTESIAN_POINT('Ctrl Pts',(-16.4226543037948,40.0686258726446,7.17453417892257));
#64614=CARTESIAN_POINT('Ctrl Pts',(-16.4502874790932,40.0734546016022,7.115714922943));
#64615=CARTESIAN_POINT('Ctrl Pts',(-16.481103090757,40.0782833305598,7.0587769165872));
#64616=CARTESIAN_POINT('Ctrl Pts',(-16.5104406821505,40.082880457453,7.00456984831777));
#64617=CARTESIAN_POINT('Ctrl Pts',(-16.5427828906446,40.0874775843461,6.95184497186535));
#64618=CARTESIAN_POINT('Ctrl Pts',(-16.5779557347004,40.0920747112392,6.90095577307296));
#64619=CARTESIAN_POINT('Ctrl Pts',(-16.6137389815674,40.0967516184076,6.84918342391737));
#64620=CARTESIAN_POINT('Ctrl Pts',(-16.6524518797614,40.101428525576,6.79931158585618));
#64621=CARTESIAN_POINT('Ctrl Pts',(-16.6938617948253,40.1061054327443,6.75168727415355));
#64622=CARTESIAN_POINT('Ctrl Pts',(-16.7344533076658,40.1106899081552,6.70500418250723));
#64623=CARTESIAN_POINT('Ctrl Pts',(-16.7776358526656,40.1152743835661,6.66048099082597));
#64624=CARTESIAN_POINT('Ctrl Pts',(-16.8231475709803,40.119858858977,6.61841408881723));
#64625=CARTESIAN_POINT('Ctrl Pts',(-16.8686314580829,40.124440530901,6.57637291145511));
#64626=CARTESIAN_POINT('Ctrl Pts',(-16.9164413212043,40.129022202825,6.53678539022267));
#64627=CARTESIAN_POINT('Ctrl Pts',(-16.9662782841984,40.133603874749,6.49991127348911));
#64628=CARTESIAN_POINT('Ctrl Pts',(-17.0161030782439,40.1381844279424,6.46304616049905));
#64629=CARTESIAN_POINT('Ctrl Pts',(-17.0679535805295,40.1427649811359,6.42889343941496));
#64630=CARTESIAN_POINT('Ctrl Pts',(-17.1214992819713,40.1473455343294,6.39767145217373));
#64631=CARTESIAN_POINT('Ctrl Pts',(-17.1770013774115,40.152093446742,6.36530871027224));
#64632=CARTESIAN_POINT('Ctrl Pts',(-17.234324473639,40.1568413591545,6.33609535606809));
#64633=CARTESIAN_POINT('Ctrl Pts',(-17.2930716667694,40.161589271567,6.31022299651359));
#64634=CARTESIAN_POINT('Ctrl Pts',(-17.3498198855619,40.1661756280896,6.28523098851388));
#64635=CARTESIAN_POINT('Ctrl Pts',(-17.4078963179194,40.1707619846121,6.26335636640238));
#64636=CARTESIAN_POINT('Ctrl Pts',(-17.4669244179725,40.1753483411346,6.24472209061737));
#64637=CARTESIAN_POINT('Ctrl Pts',(-17.5290714438634,40.1801770314922,6.22510321725659));
#64638=CARTESIAN_POINT('Ctrl Pts',(-17.5922728715517,40.1850057218497,6.2090767825581));
#64639=CARTESIAN_POINT('Ctrl Pts',(-17.656076207819,40.1898344122073,6.1967253027494));
#64640=CARTESIAN_POINT('Ctrl Pts',(-17.7198795440864,40.1946631025648,6.18437382294069));
#64641=CARTESIAN_POINT('Ctrl Pts',(-17.7842841344778,40.1994917929224,6.17569730786789));
#64642=CARTESIAN_POINT('Ctrl Pts',(-17.8488337389117,40.2043204832799,6.17071478334209));
#64643=CARTESIAN_POINT('Ctrl Pts',(-17.9102880180637,40.2089176250869,6.16597118412448));
#64644=CARTESIAN_POINT('Ctrl Pts',(-17.9721261674394,40.213514766894,6.1645558626403));
#64645=CARTESIAN_POINT('Ctrl Pts',(-18.0339568376348,40.218111908701,6.16651431022375));
#64646=CARTESIAN_POINT('Ctrl Pts',(-18.0968603114741,40.2227888140051,6.16850673818777));
#64647=CARTESIAN_POINT('Ctrl Pts',(-18.1597555225077,40.2274657193092,6.17399126125987));
#64648=CARTESIAN_POINT('Ctrl Pts',(-18.2222247586303,40.2321426246133,6.18296058080836));
#64649=CARTESIAN_POINT('Ctrl Pts',(-18.2834596204156,40.2367271155989,6.19175266915376));
#64650=CARTESIAN_POINT('Ctrl Pts',(-18.3442846600452,40.2413116065845,6.20389301401672));
#64651=CARTESIAN_POINT('Ctrl Pts',(-18.4043088509711,40.2458960975701,6.21932231050772));
#64652=CARTESIAN_POINT('Ctrl Pts',(-18.4642963388076,40.2504777852695,6.23474217242174));
#64653=CARTESIAN_POINT('Ctrl Pts',(-18.523483456918,40.255059472969,6.25344687177774));
#64654=CARTESIAN_POINT('Ctrl Pts',(-18.581489893297,40.2596411606684,6.27532613244541));
#64655=CARTESIAN_POINT('Ctrl Pts',(-18.6394821681899,40.2642217298108,6.29720005158778));
#64656=CARTESIAN_POINT('Ctrl Pts',(-18.6962938574641,40.2688022989532,6.32224681392534));
#64657=CARTESIAN_POINT('Ctrl Pts',(-18.7515622869704,40.2733828680957,6.3503071123003));
#64658=CARTESIAN_POINT('Ctrl Pts',(-18.8088496721119,40.278130765421,6.37939245332686));
#64659=CARTESIAN_POINT('Ctrl Pts',(-18.8644783167017,40.2828786627463,6.41171555370701));
#64660=CARTESIAN_POINT('Ctrl Pts',(-18.9180720149298,40.2876265600717,6.44704682775378));
#64661=CARTESIAN_POINT('Ctrl Pts',(-18.9698424426039,40.2922129327836,6.48117612332669));
#64662=CARTESIAN_POINT('Ctrl Pts',(-19.0197137857215,40.2967993054956,6.51811181769598));
#64663=CARTESIAN_POINT('Ctrl Pts',(-19.0673785482589,40.3013856782075,6.5576042028464));
#64664=CARTESIAN_POINT('Ctrl Pts',(-19.1175613243197,40.3062143378396,6.5991828746914));
#64665=CARTESIAN_POINT('Ctrl Pts',(-19.1652974388243,40.3110429974716,6.64359542279421));
#64666=CARTESIAN_POINT('Ctrl Pts',(-19.2102722044345,40.3158716571037,6.69050640586911));
#64667=CARTESIAN_POINT('Ctrl Pts',(-19.2552469700448,40.3207003167357,6.73741738894401));
#64668=CARTESIAN_POINT('Ctrl Pts',(-19.2974600236317,40.3255289763678,6.78682626247607));
#64669=CARTESIAN_POINT('Ctrl Pts',(-19.336647989908,40.3303576359998,6.83836001091529));
#64670=CARTESIAN_POINT('Ctrl Pts',(-19.3740406321603,40.3349650795427,6.88753283620867));
#64671=CARTESIAN_POINT('Ctrl Pts',(-19.4088347701809,40.3395725230856,6.93884434070388));
#64672=CARTESIAN_POINT('Ctrl Pts',(-19.4407782109389,40.3441799666285,6.99198983260663));
#64673=CARTESIAN_POINT('Ctrl Pts',(-19.4726722376121,40.348780282805,7.04505311245642));
#64674=CARTESIAN_POINT('Ctrl Pts',(-19.5017240534172,40.3533805989816,7.09994432471515));
#64675=CARTESIAN_POINT('Ctrl Pts',(-19.527722958467,40.3579809151581,7.1563274704502));
#64676=CARTESIAN_POINT('Ctrl Pts',(-19.5536896928802,40.3625755389756,7.21264084856632));
#64677=CARTESIAN_POINT('Ctrl Pts',(-19.576610803041,40.3671701627932,7.27044203976666));
#64678=CARTESIAN_POINT('Ctrl Pts',(-19.5963210577965,40.3717647866107,7.32936974398072));
#64679=CARTESIAN_POINT('Ctrl Pts',(-19.6160164077617,40.376355935998,7.38825288737651));
#64680=CARTESIAN_POINT('Ctrl Pts',(-19.6325055595317,40.3809470853853,7.44826037554428));
#64681=CARTESIAN_POINT('Ctrl Pts',(-19.6456717694011,40.3855382347726,7.50901192232934));
#64682=CARTESIAN_POINT('Ctrl Pts',(-19.6588373065105,40.3901291495638,7.5697603648643));
#64683=CARTESIAN_POINT('Ctrl Pts',(-19.6686801137244,40.3947200643551,7.63125230042118));
#64684=CARTESIAN_POINT('Ctrl Pts',(-19.6751340377647,40.3993109791463,7.69309485702321));
#64685=CARTESIAN_POINT('Ctrl Pts',(-19.6813097026429,40.4037039579075,7.75227108878679));
#64686=CARTESIAN_POINT('Ctrl Pts',(-19.6843826970131,40.4080969366687,7.81176789347959));
#64687=CARTESIAN_POINT('Ctrl Pts',(-19.6843395514378,40.4124899154299,7.87123652929707));
#64688=CARTESIAN_POINT('Ctrl Pts',(-19.6843395514373,40.4124899154864,7.8712365300618));
#64689=CARTESIAN_POINT('Ctrl Pts',(-19.6842878411527,40.4177549291061,7.94251007690588));
#64690=CARTESIAN_POINT('Ctrl Pts',(-19.6797612505141,40.4230199427259,8.01360330873315));
#64691=CARTESIAN_POINT('Ctrl Pts',(-19.6708512413931,40.4282849563456,8.08400213802566));
#64692=CARTESIAN_POINT('Ctrl Pts',(-19.6618564270657,40.4336000822111,8.15507102131738));
#64693=CARTESIAN_POINT('Ctrl Pts',(-19.6483944695626,40.4389152080765,8.22543203500817));
#64694=CARTESIAN_POINT('Ctrl Pts',(-19.6306090111538,40.444230333942,8.29457593890581));
#64695=CARTESIAN_POINT('Ctrl Pts',(-19.6170407903194,40.4482851522013,8.34732463595239));
#64696=CARTESIAN_POINT('Ctrl Pts',(-19.6009573588429,40.4523399704605,8.3993653731387));
#64697=CARTESIAN_POINT('Ctrl Pts',(-19.5824409865512,40.4563947887198,8.45048059418118));
#64698=CARTESIAN_POINT('Ctrl Pts',(-19.5614477628561,40.4609920016846,8.50843326723516));
#64699=CARTESIAN_POINT('Ctrl Pts',(-19.5372635639648,40.4655892146493,8.5653646470191));
#64700=CARTESIAN_POINT('Ctrl Pts',(-19.5100081538699,40.4701864276141,8.62089938386691));
#64701=CARTESIAN_POINT('Ctrl Pts',(-19.4822803260345,40.4748633240235,8.67739670373251));
#64702=CARTESIAN_POINT('Ctrl Pts',(-19.4513738977614,40.4795402204329,8.73244797242256));
#64703=CARTESIAN_POINT('Ctrl Pts',(-19.417467586182,40.4842171168423,8.78567558353173));
#64704=CARTESIAN_POINT('Ctrl Pts',(-19.3842306907973,40.48880167675,8.83785231581559));
#64705=CARTESIAN_POINT('Ctrl Pts',(-19.3481115760661,40.4933862366577,8.88827629507691));
#64706=CARTESIAN_POINT('Ctrl Pts',(-19.3093253636047,40.4979707965654,8.93661563521128));
#64707=CARTESIAN_POINT('Ctrl Pts',(-19.2705628760136,40.5025525521753,8.98492540698873));
#64708=CARTESIAN_POINT('Ctrl Pts',(-19.2291368434709,40.5071343077852,9.03115267183257));
#64709=CARTESIAN_POINT('Ctrl Pts',(-19.18530441965,40.5117160633951,9.07499630355125));
#64710=CARTESIAN_POINT('Ctrl Pts',(-19.1414827074028,40.5162966993359,9.11882922095733));
#64711=CARTESIAN_POINT('Ctrl Pts',(-19.095256131015,40.5208773352767,9.16027930174823));
#64712=CARTESIAN_POINT('Ctrl Pts',(-19.0469192564903,40.5254579712174,9.1990816888853));
#64713=CARTESIAN_POINT('Ctrl Pts',(-18.9968180681141,40.5302058020693,9.23930037754727));
#64714=CARTESIAN_POINT('Ctrl Pts',(-18.9444499631566,40.5349536329212,9.27667393689923));
#64715=CARTESIAN_POINT('Ctrl Pts',(-18.8901790902337,40.5397014637731,9.310954148924));
#64716=CARTESIAN_POINT('Ctrl Pts',(-18.8377530679985,40.544287899782,9.34406906049716));
#64717=CARTESIAN_POINT('Ctrl Pts',(-18.7835520689903,40.5488743357909,9.37429737488332));
#64718=CARTESIAN_POINT('Ctrl Pts',(-18.727930304232,40.5534607717998,9.40146175127277));
#64719=CARTESIAN_POINT('Ctrl Pts',(-18.6693725780964,40.5582893000732,9.43005998292126));
#64720=CARTESIAN_POINT('Ctrl Pts',(-18.6092405334155,40.5631178283465,9.4552615992809));
#64721=CARTESIAN_POINT('Ctrl Pts',(-18.5479694136963,40.5679463566199,9.47691803795511));
#64722=CARTESIAN_POINT('Ctrl Pts',(-18.486698293977,40.5727748848932,9.49857447662932));
#64723=CARTESIAN_POINT('Ctrl Pts',(-18.4242887448175,40.5776034131666,9.51668563102563));
#64724=CARTESIAN_POINT('Ctrl Pts',(-18.361189111174,40.5824319414399,9.53116516250563));
#64725=CARTESIAN_POINT('Ctrl Pts',(-18.301111690253,40.587029203084,9.54495118402799));
#64726=CARTESIAN_POINT('Ctrl Pts',(-18.2401621044606,40.5916264647281,9.55550217781377));
#64727=CARTESIAN_POINT('Ctrl Pts',(-18.1787206854397,40.5962237263722,9.56271525212553));
#64728=CARTESIAN_POINT('Ctrl Pts',(-18.1162150461293,40.6009006166967,9.5700532633309));
#64729=CARTESIAN_POINT('Ctrl Pts',(-18.0532008692111,40.6055775070212,9.57393641178694));
#64730=CARTESIAN_POINT('Ctrl Pts',(-17.9900923324682,40.6102543973457,9.57431011861848));
#64731=CARTESIAN_POINT('Ctrl Pts',(-17.9282289445468,40.6148390113352,9.57467645211125));
#64732=CARTESIAN_POINT('Ctrl Pts',(-17.8662754201515,40.6194236253247,9.571670567226));
#64733=CARTESIAN_POINT('Ctrl Pts',(-17.8046272750187,40.6240082393142,9.56529326163134));
#64734=CARTESIAN_POINT('Ctrl Pts',(-17.7430168138054,40.6285900508475,9.55891985431895));
#64735=CARTESIAN_POINT('Ctrl Pts',(-17.6817118669993,40.6331718623809,9.5491791649594));
#64736=CARTESIAN_POINT('Ctrl Pts',(-17.6211048950814,40.6377536739142,9.53612398676252));
#64737=CARTESIAN_POINT('Ctrl Pts',(-17.5605127109042,40.6423343675128,9.52307199395149));
#64738=CARTESIAN_POINT('Ctrl Pts',(-17.5006186609421,40.6469150611114,9.50670722486737));
#64739=CARTESIAN_POINT('Ctrl Pts',(-17.4418050166596,40.6514957547099,9.48713357379878));
#64740=CARTESIAN_POINT('Ctrl Pts',(-17.3808460947574,40.6562435329974,9.46684595718556));
#64741=CARTESIAN_POINT('Ctrl Pts',(-17.3210484916843,40.6609913112849,9.44311096440126));
#64742=CARTESIAN_POINT('Ctrl Pts',(-17.2628181995382,40.6657390895724,9.4160999646486));
#64743=CARTESIAN_POINT('Ctrl Pts',(-17.2065659782525,40.6703255868232,9.39000652291512));
#64744=CARTESIAN_POINT('Ctrl Pts',(-17.1517767189282,40.6749120840741,9.36085640068078));
#64745=CARTESIAN_POINT('Ctrl Pts',(-17.0987915006898,40.6794985813249,9.3288510603703));
#64746=CARTESIAN_POINT('Ctrl Pts',(-17.0430114990502,40.6843270001307,9.29515755123035));
#64747=CARTESIAN_POINT('Ctrl Pts',(-16.9892316597327,40.6891554189365,9.25829963538069));
#64748=CARTESIAN_POINT('Ctrl Pts',(-16.9378127825556,40.6939838377423,9.21856243437058));
#64749=CARTESIAN_POINT('Ctrl Pts',(-16.8863939053786,40.6988122565482,9.17882523336047));
#64750=CARTESIAN_POINT('Ctrl Pts',(-16.8373364298726,40.703640675354,9.1362092317421));
#64751=CARTESIAN_POINT('Ctrl Pts',(-16.7909559844104,40.7084690941598,9.09104429264079));
#64752=CARTESIAN_POINT('Ctrl Pts',(-16.7468039473542,40.7130655253478,9.04804936137239));
#64753=CARTESIAN_POINT('Ctrl Pts',(-16.7048960713131,40.7176619565358,9.00256812221833));
#64754=CARTESIAN_POINT('Ctrl Pts',(-16.665525008342,40.7222583877239,8.95486419975304));
#64755=CARTESIAN_POINT('Ctrl Pts',(-16.6254638776663,40.7269353818554,8.90632415720873));
#64756=CARTESIAN_POINT('Ctrl Pts',(-16.5880297897841,40.7316123759869,8.85548306815653));
#64757=CARTESIAN_POINT('Ctrl Pts',(-16.5534933249741,40.7362893701184,8.80265939211831));
#64758=CARTESIAN_POINT('Ctrl Pts',(-16.5196451881018,40.7408731495638,8.75088851671246));
#64759=CARTESIAN_POINT('Ctrl Pts',(-16.4885805250383,40.7454569290092,8.69721380371065));
#64760=CARTESIAN_POINT('Ctrl Pts',(-16.4605131055109,40.7500407084546,8.64196788344839));
#64761=CARTESIAN_POINT('Ctrl Pts',(-16.4324628412779,40.7546216862144,8.58675573045232));
#64762=CARTESIAN_POINT('Ctrl Pts',(-16.4074064182867,40.7592026639742,8.529974727469));
#64763=CARTESIAN_POINT('Ctrl Pts',(-16.3855122645559,40.763783641734,8.47198313690539));
#64764=CARTESIAN_POINT('Ctrl Pts',(-16.3636234437673,40.7683635036668,8.41400567183841));
#64765=CARTESIAN_POINT('Ctrl Pts',(-16.344895542964,40.7729433655995,8.35481868075846));
#64766=CARTESIAN_POINT('Ctrl Pts',(-16.3294485300274,40.7775232275322,8.29479957694341));
#64767=CARTESIAN_POINT('Ctrl Pts',(-16.3134324461011,40.7822718124779,8.23256935755861));
#64768=CARTESIAN_POINT('Ctrl Pts',(-16.3009439111735,40.7870203974235,8.16944506758937));
#64769=CARTESIAN_POINT('Ctrl Pts',(-16.2920591288017,40.7917689823691,8.1058610839843));
#64770=CARTESIAN_POINT('Ctrl Pts',(-16.2834791470357,40.7963546627542,8.04445840723785));
#64771=CARTESIAN_POINT('Ctrl Pts',(-16.2782596213027,40.8009403431392,7.98262760078482));
#64772=CARTESIAN_POINT('Ctrl Pts',(-16.2764161851709,40.8055260235242,7.9207643718782));
#64773=CARTESIAN_POINT('Ctrl Pts',(-16.2744745179824,40.8103560607502,7.85560464127183));
#64774=CARTESIAN_POINT('Ctrl Pts',(-16.2762787961322,40.8151860979761,7.79040958364245));
#64775=CARTESIAN_POINT('Ctrl Pts',(-16.281784964333,40.820016135202,7.72563751098501));
#64776=CARTESIAN_POINT('Ctrl Pts',(-16.2872911325338,40.824846172428,7.66086543832757));
#64777=CARTESIAN_POINT('Ctrl Pts',(-16.2964990212439,40.8296762096539,7.59651698449358));
#64778=CARTESIAN_POINT('Ctrl Pts',(-16.3093023662471,40.8345062468799,7.53303671984536));
#64779=CARTESIAN_POINT('Ctrl Pts',(-16.3214907112066,40.8391042765246,7.47260568690377));
#64780=CARTESIAN_POINT('Ctrl Pts',(-16.3369870654642,40.8437023061694,7.412712884101));
#64781=CARTESIAN_POINT('Ctrl Pts',(-16.3557284589915,40.8483003358141,7.35374735190046));
#64782=CARTESIAN_POINT('Ctrl Pts',(-16.37479089435,40.8529771301385,7.29377173459539));
#64783=CARTESIAN_POINT('Ctrl Pts',(-16.3972105797347,40.8576539244629,7.23475599390204));
#64784=CARTESIAN_POINT('Ctrl Pts',(-16.4228666501253,40.8623307187874,7.17709988720741));
#64785=CARTESIAN_POINT('Ctrl Pts',(-16.4480211573433,40.8669160841531,7.12057092817619));
#64786=CARTESIAN_POINT('Ctrl Pts',(-16.4762864321406,40.8715014495189,7.06534940841457));
#64787=CARTESIAN_POINT('Ctrl Pts',(-16.5074987781142,40.8760868148846,7.01179548641081));
#64788=CARTESIAN_POINT('Ctrl Pts',(-16.5386919922201,40.8806693696124,6.95827439073013));
#64789=CARTESIAN_POINT('Ctrl Pts',(-16.5728284398669,40.8852519243403,6.90641930469754));
#64790=CARTESIAN_POINT('Ctrl Pts',(-16.6096983038783,40.8898344790681,6.85656618508852));
#64791=CARTESIAN_POINT('Ctrl Pts',(-16.6465590984013,40.8944159065493,6.80672532867346));
#64792=CARTESIAN_POINT('Ctrl Pts',(-16.6861516720603,40.8989973340306,6.75888587002064));
#64793=CARTESIAN_POINT('Ctrl Pts',(-16.728223839013,40.9035787615118,6.7133534341102));
#64794=CARTESIAN_POINT('Ctrl Pts',(-16.7718169799035,40.9083258146859,6.66617493018474));
#64795=CARTESIAN_POINT('Ctrl Pts',(-16.8180720839233,40.9130728678599,6.62147392010099));
#64796=CARTESIAN_POINT('Ctrl Pts',(-16.8666660075634,40.9178199210339,6.57954959146613));
#64797=CARTESIAN_POINT('Ctrl Pts',(-16.9136235679298,40.9224071208169,6.53903703258589));
#64798=CARTESIAN_POINT('Ctrl Pts',(-16.9627644637704,40.9269943206,6.50111737585054));
#64799=CARTESIAN_POINT('Ctrl Pts',(-17.0137645727833,40.9315815203831,6.46601854186343));
#64800=CARTESIAN_POINT('Ctrl Pts',(-17.0674305370288,40.9364085002526,6.42908503708725));
#64801=CARTESIAN_POINT('Ctrl Pts',(-17.1231548723184,40.941235480122,6.39527568975556));
#64802=CARTESIAN_POINT('Ctrl Pts',(-17.1805296351771,40.9460624599915,6.36480168370747));
#64803=CARTESIAN_POINT('Ctrl Pts',(-17.2379043980357,40.950889439861,6.33432767765938));
#64804=CARTESIAN_POINT('Ctrl Pts',(-17.2969289675865,40.9557164197304,6.30718921361192));
#64805=CARTESIAN_POINT('Ctrl Pts',(-17.3571732524428,40.9605433995999,6.28353799978463));
#64806=CARTESIAN_POINT('Ctrl Pts',(-17.4145580294188,40.9651412658363,6.26100939588588));
#64807=CARTESIAN_POINT('Ctrl Pts',(-17.4732841783451,40.9697391320727,6.24155223822962));
#64808=CARTESIAN_POINT('Ctrl Pts',(-17.5329906431261,40.9743369983091,6.2253245090696));
#64809=CARTESIAN_POINT('Ctrl Pts',(-17.5937223088222,40.9790138130595,6.20881813867956));
#64810=CARTESIAN_POINT('Ctrl Pts',(-17.6554678145706,40.98369062781,6.19565342837095));
#64811=CARTESIAN_POINT('Ctrl Pts',(-17.7178256722736,40.9883674425604,6.18594553013236));
#64812=CARTESIAN_POINT('Ctrl Pts',(-17.7789625958245,40.9929526877307,6.17642770745023));
#64813=CARTESIAN_POINT('Ctrl Pts',(-17.840687581427,40.9975379329009,6.17023263360172));
#64814=CARTESIAN_POINT('Ctrl Pts',(-17.9026092417226,41.0021231780712,6.16741798842662));
#64815=CARTESIAN_POINT('Ctrl Pts',(-17.9644931649934,41.0067056288476,6.16460505858562));
#64816=CARTESIAN_POINT('Ctrl Pts',(-18.0265730179909,41.0112880796239,6.16516849546682));
#64817=CARTESIAN_POINT('Ctrl Pts',(-18.0884527516576,41.0158705304003,6.16911410251661));
#64818=CARTESIAN_POINT('Ctrl Pts',(-18.1503174830268,41.0204518701943,6.17305875298227));
#64819=CARTESIAN_POINT('Ctrl Pts',(-18.2119816837657,41.0250332099883,6.18038391343445));
#64820=CARTESIAN_POINT('Ctrl Pts',(-18.2730518285094,41.0296145497823,6.19104334141489));
#64821=CARTESIAN_POINT('Ctrl Pts',(-18.3363324803282,41.0343617166605,6.20208860016527));
#64822=CARTESIAN_POINT('Ctrl Pts',(-18.3989746623878,41.0391088835386,6.21671409507796));
#64823=CARTESIAN_POINT('Ctrl Pts',(-18.4605517470838,41.0438560504167,6.23481045319672));
#64824=CARTESIAN_POINT('Ctrl Pts',(-18.520053238235,41.0484432034037,6.25229683303733));
#64825=CARTESIAN_POINT('Ctrl Pts',(-18.5785598237685,41.0530303563906,6.27302355336963));
#64826=CARTESIAN_POINT('Ctrl Pts',(-18.6357042839605,41.0576175093776,6.29684179829368));
#64827=CARTESIAN_POINT('Ctrl Pts',(-18.6958388038233,41.0624446832013,6.32190632279299));
#64828=CARTESIAN_POINT('Ctrl Pts',(-18.7544641529891,41.067271857025,6.35039451360709));
#64829=CARTESIAN_POINT('Ctrl Pts',(-18.8111816878708,41.0720990308487,6.38207801368881));
#64830=CARTESIAN_POINT('Ctrl Pts',(-18.8678992227526,41.0769262046724,6.41376151377053));
#64831=CARTESIAN_POINT('Ctrl Pts',(-18.9227084380972,41.0817533784961,6.44863990994636));
#64832=CARTESIAN_POINT('Ctrl Pts',(-18.9752486778418,41.0865805523198,6.48643398970117));
#64833=CARTESIAN_POINT('Ctrl Pts',(-19.0248466829921,41.0911374061395,6.52211161453584));
#64834=CARTESIAN_POINT('Ctrl Pts',(-19.0726347189551,41.0956942599593,6.56053956304578));
#64835=CARTESIAN_POINT('Ctrl Pts',(-19.1182874020377,41.100251113779,6.60150615848472));
#64836=CARTESIAN_POINT('Ctrl Pts',(-19.1638599640665,41.1047999702609,6.64240085701476));
#64837=CARTESIAN_POINT('Ctrl Pts',(-19.2073042273338,41.1093488267428,6.68582501751963));
#64838=CARTESIAN_POINT('Ctrl Pts',(-19.2483254139918,41.1138976832247,6.73152493227887));
#64839=CARTESIAN_POINT('Ctrl Pts',(-19.2893065428958,41.1184420976855,6.77718022044173));
#64840=CARTESIAN_POINT('Ctrl Pts',(-19.3278689372972,41.1229865121464,6.82510647678214));
#64841=CARTESIAN_POINT('Ctrl Pts',(-19.3637537214592,41.1275309266073,6.87501232472565));
#64842=CARTESIAN_POINT('Ctrl Pts',(-19.399617222011,41.1320726457323,6.92488857303136));
#64843=CARTESIAN_POINT('Ctrl Pts',(-19.4328059574439,41.1366143648573,6.97674166550847));
#64844=CARTESIAN_POINT('Ctrl Pts',(-19.4631019211595,41.1411560839822,7.03024793715464));
#64845=CARTESIAN_POINT('Ctrl Pts',(-19.4933915305055,41.145696850513,7.0837429862291));
#64846=CARTESIAN_POINT('Ctrl Pts',(-19.5207893171996,41.1502376170437,7.13889007462835));
#64847=CARTESIAN_POINT('Ctrl Pts',(-19.5451222840827,41.1547783835744,7.19533929159332));
#64848=CARTESIAN_POINT('Ctrl Pts',(-19.5694763472953,41.1593230868838,7.25183744921097));
#64849=CARTESIAN_POINT('Ctrl Pts',(-19.5907600761388,41.1638677901933,7.30963951323497));
#64850=CARTESIAN_POINT('Ctrl Pts',(-19.6088484657843,41.1684124935028,7.36837512909319));
#64851=CARTESIAN_POINT('Ctrl Pts',(-19.6269446131302,41.1729591459325,7.42713593532626));
#64852=CARTESIAN_POINT('Ctrl Pts',(-19.6418425658306,41.1775057983622,7.48683058660605));
#64853=CARTESIAN_POINT('Ctrl Pts',(-19.6534679622412,41.182052450792,7.54707614682026));
#64854=CARTESIAN_POINT('Ctrl Pts',(-19.6651144382153,41.1866073473663,7.60743094633072));
#64855=CARTESIAN_POINT('Ctrl Pts',(-19.6734764366779,41.1911622439407,7.66833813464));
#64856=CARTESIAN_POINT('Ctrl Pts',(-19.6785313660541,41.1957171405151,7.72940827147221));
#64857=CARTESIAN_POINT('Ctrl Pts',(-19.6824240182035,41.1992247321392,7.77643658417713));
#64858=CARTESIAN_POINT('Ctrl Pts',(-19.6843566180351,41.2027323237633,7.82356137122071));
#64859=CARTESIAN_POINT('Ctrl Pts',(-19.6843398922845,41.2062399153875,7.87060594373627));
#64860=CARTESIAN_POINT('Origin',(-17.98,42.93984859951,7.87));
#64861=CARTESIAN_POINT('',(-19.24999991436,34.6054735995751,7.87046639652064));
#64862=CARTESIAN_POINT('Ctrl Pts',(-18.810359785549,34.7139132859163,8.83093840933901));
#64863=CARTESIAN_POINT('Ctrl Pts',(-18.8480000770215,34.7089793142232,8.79841292794362));
#64864=CARTESIAN_POINT('Ctrl Pts',(-18.8837142939927,34.7040453425301,8.76368311649533));
#64865=CARTESIAN_POINT('Ctrl Pts',(-18.9172453719093,34.699111370837,8.72701290120657));
#64866=CARTESIAN_POINT('Ctrl Pts',(-18.9507928644184,34.6941749837985,8.69032473461191));
#64867=CARTESIAN_POINT('Ctrl Pts',(-18.9821547422459,34.68923859676,8.65169469762151));
#64868=CARTESIAN_POINT('Ctrl Pts',(-19.0111143192575,34.6843022097216,8.61141976006991));
#64869=CARTESIAN_POINT('Ctrl Pts',(-19.0401293155334,34.6793563760348,8.57106774931358));
#64870=CARTESIAN_POINT('Ctrl Pts',(-19.0667325374929,34.674410542348,8.52906501637736));
#64871=CARTESIAN_POINT('Ctrl Pts',(-19.0907515469335,34.6694647086613,8.48573614558909));
#64872=CARTESIAN_POINT('Ctrl Pts',(-19.1060831698011,34.6663077234809,8.4580788057703));
#64873=CARTESIAN_POINT('Ctrl Pts',(-19.1203628104226,34.6631507383005,8.4298816437122));
#64874=CARTESIAN_POINT('Ctrl Pts',(-19.1335559487169,34.6599937531201,8.40123316272596));
#64875=CARTESIAN_POINT('Ctrl Pts',(-19.1560538394946,34.65461023434,8.35237970710382));
#64876=CARTESIAN_POINT('Ctrl Pts',(-19.1754766558247,34.64922671556,8.30202519731203));
#64877=CARTESIAN_POINT('Ctrl Pts',(-19.1916417683459,34.6438431967799,8.25055778168331));
#64878=CARTESIAN_POINT('Ctrl Pts',(-19.2077585403069,34.6384757770101,8.19924427551205));
#64879=CARTESIAN_POINT('Ctrl Pts',(-19.22063686448,34.6331083572404,8.14682484893595));
#64880=CARTESIAN_POINT('Ctrl Pts',(-19.2301420171886,34.6277409374706,8.09370725705597));
#64881=CARTESIAN_POINT('Ctrl Pts',(-19.2396044484566,34.6223976418693,8.04082840516496));
#64882=CARTESIAN_POINT('Ctrl Pts',(-19.2457238109817,34.6170543462681,7.9872580131992));
#64883=CARTESIAN_POINT('Ctrl Pts',(-19.2484157084143,34.6117110506668,7.93341601255157));
#64884=CARTESIAN_POINT('Ctrl Pts',(-19.2494631630086,34.6096319003029,7.91246534397657));
#64885=CARTESIAN_POINT('Ctrl Pts',(-19.2499921996046,34.607552749939,7.89147371151049));
#64886=CARTESIAN_POINT('Ctrl Pts',(-19.24999991436,34.6054735995751,7.87046639652063));
#64887=CARTESIAN_POINT('',(-17.7961609204192,34.0285,9.12662372762052));
#64888=CARTESIAN_POINT('Ctrl Pts',(-19.2499999143602,34.60547359951,7.87046639586325));
#64889=CARTESIAN_POINT('Ctrl Pts',(-19.2500186228147,34.600431606206,7.81952311472636));
#64890=CARTESIAN_POINT('Ctrl Pts',(-19.246967776457,34.5953896129021,7.76860069349798));
#64891=CARTESIAN_POINT('Ctrl Pts',(-19.2408810348543,34.5903476195981,7.71808220662215));
#64892=CARTESIAN_POINT('Ctrl Pts',(-19.2347835878813,34.5852967584287,7.66747486775573));
#64893=CARTESIAN_POINT('Ctrl Pts',(-19.2256396491361,34.5802458972594,7.6172733915475));
#64894=CARTESIAN_POINT('Ctrl Pts',(-19.2135345173812,34.57519503609,7.56785335608491));
#64895=CARTESIAN_POINT('Ctrl Pts',(-19.2014184031309,34.5701395924791,7.51838848382752));
#64896=CARTESIAN_POINT('Ctrl Pts',(-19.1863358983142,34.5650841488681,7.4697069540304));
#64897=CARTESIAN_POINT('Ctrl Pts',(-19.168422001748,34.5600287052572,7.42216839575436));
#64898=CARTESIAN_POINT('Ctrl Pts',(-19.1504644036985,34.5549609287412,7.37451386575195));
#64899=CARTESIAN_POINT('Ctrl Pts',(-19.129661823782,34.5498931522253,7.32800834707118));
#64900=CARTESIAN_POINT('Ctrl Pts',(-19.1061968005565,34.5448253757093,7.28298997758443));
#64901=CARTESIAN_POINT('Ctrl Pts',(-19.0894217866189,34.5412024506063,7.25080659688501));
#64902=CARTESIAN_POINT('Ctrl Pts',(-19.0712870579479,34.5375795255032,7.21938276448517));
#64903=CARTESIAN_POINT('Ctrl Pts',(-19.051872661738,34.5339566004002,7.18883262187727));
#64904=CARTESIAN_POINT('Ctrl Pts',(-19.0253535487371,34.5290078624037,7.14710262547379));
#64905=CARTESIAN_POINT('Ctrl Pts',(-18.9963354076115,34.5240591244073,7.10683163003986));
#64906=CARTESIAN_POINT('Ctrl Pts',(-18.9650042712288,34.5191103864108,7.06833511636029));
#64907=CARTESIAN_POINT('Ctrl Pts',(-18.9337306655237,34.5141707353574,7.02990929052597));
#64908=CARTESIAN_POINT('Ctrl Pts',(-18.9001528311632,34.5092310843039,6.99325190543645));
#64909=CARTESIAN_POINT('Ctrl Pts',(-18.8644999814156,34.5042914332505,6.95864947310278));
#64910=CARTESIAN_POINT('Ctrl Pts',(-18.828883254654,34.4993567869848,6.92408209948645));
#64911=CARTESIAN_POINT('Ctrl Pts',(-18.7911960657585,34.4944221407191,6.89156593650389));
#64912=CARTESIAN_POINT('Ctrl Pts',(-18.7517063628538,34.4894874944534,6.86135274276335));
#64913=CARTESIAN_POINT('Ctrl Pts',(-18.7122398805274,34.4845557498389,6.83115731486508));
#64914=CARTESIAN_POINT('Ctrl Pts',(-18.6709734181886,34.4796240052243,6.8032625057152));
#64915=CARTESIAN_POINT('Ctrl Pts',(-18.6282081130353,34.4746922606097,6.77787993233562));
#64916=CARTESIAN_POINT('Ctrl Pts',(-18.5854497731739,34.4697613192407,6.75250149307909));
#64917=CARTESIAN_POINT('Ctrl Pts',(-18.5411935464605,34.4648303778717,6.72963475584668));
#64918=CARTESIAN_POINT('Ctrl Pts',(-18.4957674568792,34.4598994365027,6.70944671366438));
#64919=CARTESIAN_POINT('Ctrl Pts',(-18.4502969249553,34.4549636709767,6.68923892063199));
#64920=CARTESIAN_POINT('Ctrl Pts',(-18.4036547469488,34.4500279054508,6.67171527708261));
#64921=CARTESIAN_POINT('Ctrl Pts',(-18.3561896772165,34.4450921399248,6.65699491890769));
#64922=CARTESIAN_POINT('Ctrl Pts',(-18.3086990327265,34.4401537149483,6.64226662922451));
#64923=CARTESIAN_POINT('Ctrl Pts',(-18.2603851459658,34.4352152899717,6.6303447640693));
#64924=CARTESIAN_POINT('Ctrl Pts',(-18.2116092631565,34.4302768649952,6.62129781404046));
#64925=CARTESIAN_POINT('Ctrl Pts',(-18.1627422776133,34.4253292161156,6.61223396627789));
#64926=CARTESIAN_POINT('Ctrl Pts',(-18.1134121175931,34.4203815672359,6.60605581906447));
#64927=CARTESIAN_POINT('Ctrl Pts',(-18.0639858589226,34.4154339183563,6.60278006032851));
#64928=CARTESIAN_POINT('Ctrl Pts',(-18.0389630531116,34.4129290947976,6.60112165694256));
#64929=CARTESIAN_POINT('Ctrl Pts',(-18.013915625472,34.4104242712389,6.60020631664651));
#64930=CARTESIAN_POINT('Ctrl Pts',(-17.9888908928602,34.4079194476802,6.60003112163166));
#64931=CARTESIAN_POINT('Ctrl Pts',(-17.9395139360616,34.4029771145666,6.5996854397491));
#64932=CARTESIAN_POINT('Ctrl Pts',(-17.890006080321,34.398034781453,6.60222299368832));
#64933=CARTESIAN_POINT('Ctrl Pts',(-17.8407324357409,34.3930924483394,6.60765910089812));
#64934=CARTESIAN_POINT('Ctrl Pts',(-17.7915496724127,34.3881592309595,6.61308518164788));
#64935=CARTESIAN_POINT('Ctrl Pts',(-17.7426008050934,34.3832260135796,6.62139915367661));
#64936=CARTESIAN_POINT('Ctrl Pts',(-17.6942501103006,34.3782927961996,6.63256434489031));
#64937=CARTESIAN_POINT('Ctrl Pts',(-17.6459485910255,34.3733645961937,6.64371818044383));
#64938=CARTESIAN_POINT('Ctrl Pts',(-17.5982445727108,34.3684363961878,6.65771737207312));
#64939=CARTESIAN_POINT('Ctrl Pts',(-17.551494205748,34.3635081961818,6.67447384625325));
#64940=CARTESIAN_POINT('Ctrl Pts',(-17.5047713711017,34.358582898501,6.69122045217825));
#64941=CARTESIAN_POINT('Ctrl Pts',(-17.4590015915058,34.3536576008201,6.71072093911075));
#64942=CARTESIAN_POINT('Ctrl Pts',(-17.4145253338303,34.3487323031392,6.73283756572764));
#64943=CARTESIAN_POINT('Ctrl Pts',(-17.3700562283285,34.3438077974896,6.75495063579629));
#64944=CARTESIAN_POINT('Ctrl Pts',(-17.3268807230226,34.3388832918399,6.77967876502301));
#64945=CARTESIAN_POINT('Ctrl Pts',(-17.2853163954858,34.3339587861903,6.80683741148444));
#64946=CARTESIAN_POINT('Ctrl Pts',(-17.2437107803969,34.3290293888271,6.83402303574376));
#64947=CARTESIAN_POINT('Ctrl Pts',(-17.2037199986934,34.324099991464,6.86364369561324));
#64948=CARTESIAN_POINT('Ctrl Pts',(-17.1656326711676,34.3191705941008,6.89547147105363));
#64949=CARTESIAN_POINT('Ctrl Pts',(-17.1275245720404,34.3142385084031,6.92731660433739));
#64950=CARTESIAN_POINT('Ctrl Pts',(-17.0913223943485,34.3093064227055,6.9613708728251));
#64951=CARTESIAN_POINT('Ctrl Pts',(-17.0572789666622,34.3043743370078,6.99736840841281));
#64952=CARTESIAN_POINT('Ctrl Pts',(-17.02317104724,34.2994329079863,7.03343413759067));
#64953=CARTESIAN_POINT('Ctrl Pts',(-16.9912303931655,34.2944914789648,7.07145006012652));
#64954=CARTESIAN_POINT('Ctrl Pts',(-16.9616694537387,34.2895500499434,7.11111733545216));
#64955=CARTESIAN_POINT('Ctrl Pts',(-16.9463792721866,34.2869941316156,7.13163494596014));
#64956=CARTESIAN_POINT('Ctrl Pts',(-16.9317250454833,34.2844382132879,7.15259388680391));
#64957=CARTESIAN_POINT('Ctrl Pts',(-16.9177313970105,34.2818822949602,7.17395013461477));
#64958=CARTESIAN_POINT('Ctrl Pts',(-16.8905925241095,34.276925421649,7.21536781750925));
#64959=CARTESIAN_POINT('Ctrl Pts',(-16.8658205031715,34.2719685483378,7.25846521105024));
#64960=CARTESIAN_POINT('Ctrl Pts',(-16.8436263679747,34.2670116750265,7.30294182975858));
#64961=CARTESIAN_POINT('Ctrl Pts',(-16.8214733055949,34.2620639749833,7.34733613933392));
#64962=CARTESIAN_POINT('Ctrl Pts',(-16.8018889075183,34.2571162749401,7.39310412652142));
#64963=CARTESIAN_POINT('Ctrl Pts',(-16.7850399872838,34.252168574897,7.43991795200291));
#64964=CARTESIAN_POINT('Ctrl Pts',(-16.7682083159663,34.2472259400132,7.48668385228935));
#64965=CARTESIAN_POINT('Ctrl Pts',(-16.7541067617319,34.2422833051294,7.53449295983615));
#64966=CARTESIAN_POINT('Ctrl Pts',(-16.7428545015778,34.2373406702457,7.58299648829016));
#64967=CARTESIAN_POINT('Ctrl Pts',(-16.7316090177099,34.2324010118935,7.63147080716473));
#64968=CARTESIAN_POINT('Ctrl Pts',(-16.7232095513179,34.2274613535414,7.6806381876418));
#64969=CARTESIAN_POINT('Ctrl Pts',(-16.7177250290144,34.2225216951893,7.73013614611617));
#64970=CARTESIAN_POINT('Ctrl Pts',(-16.7122414978942,34.2175829295507,7.7796251591342));
#64971=CARTESIAN_POINT('Ctrl Pts',(-16.7096719242146,34.2126441639121,7.82944408920579));
#64972=CARTESIAN_POINT('Ctrl Pts',(-16.7100334996795,34.2077053982735,7.87922431913868));
#64973=CARTESIAN_POINT('Ctrl Pts',(-16.7103954139834,34.2027620044261,7.92905119904701));
#64974=CARTESIAN_POINT('Ctrl Pts',(-16.71369395739,34.1978186105788,7.97883875953236));
#64975=CARTESIAN_POINT('Ctrl Pts',(-16.7198941752857,34.1928752167315,8.02821918506006));
#64976=CARTESIAN_POINT('Ctrl Pts',(-16.7260976023264,34.1879292642535,8.07762516919673));
#64977=CARTESIAN_POINT('Ctrl Pts',(-16.7352055959661,34.1829833117755,8.12662306128246));
#64978=CARTESIAN_POINT('Ctrl Pts',(-16.7471318960423,34.1780373592975,8.174854454197));
#64979=CARTESIAN_POINT('Ctrl Pts',(-16.7590798518372,34.1730824259826,8.22317342544435));
#64980=CARTESIAN_POINT('Ctrl Pts',(-16.7738561668314,34.1681274926678,8.27072259772776));
#64981=CARTESIAN_POINT('Ctrl Pts',(-16.7913249557066,34.1631725593529,8.31715952307225));
#64982=CARTESIAN_POINT('Ctrl Pts',(-16.799935976576,34.160730086982,8.34005002430323));
#64983=CARTESIAN_POINT('Ctrl Pts',(-16.8092004992438,34.1582876146111,8.36267058670134));
#64984=CARTESIAN_POINT('Ctrl Pts',(-16.819098120925,34.1558451422402,8.38498235616398));
#64985=CARTESIAN_POINT('Ctrl Pts',(-16.8391628871209,34.1508936863611,8.43021346845593));
#64986=CARTESIAN_POINT('Ctrl Pts',(-16.8619184940994,34.1459422304821,8.47436813249849));
#64987=CARTESIAN_POINT('Ctrl Pts',(-16.8872269071449,34.140990774603,8.51710661218381));
#64988=CARTESIAN_POINT('Ctrl Pts',(-16.9124896153011,34.1360482606415,8.55976790972885));
#64989=CARTESIAN_POINT('Ctrl Pts',(-16.9402957091205,34.13110574668,8.60101762863171));
#64990=CARTESIAN_POINT('Ctrl Pts',(-16.9704601981101,34.1261632327185,8.64053837568294));
#64991=CARTESIAN_POINT('Ctrl Pts',(-17.0005946724359,34.1212256367218,8.6800197982843));
#64992=CARTESIAN_POINT('Ctrl Pts',(-17.0330825656132,34.1162880407251,8.71777522231424));
#64993=CARTESIAN_POINT('Ctrl Pts',(-17.0676954834215,34.1113504447284,8.75351596987858));
#64994=CARTESIAN_POINT('Ctrl Pts',(-17.1022886214296,34.1064156703563,8.78923629313631));
#64995=CARTESIAN_POINT('Ctrl Pts',(-17.1390039983283,34.1014808959843,8.82294382870522));
#64996=CARTESIAN_POINT('Ctrl Pts',(-17.1775745075821,34.0965461216122,8.85438474648779));
#64997=CARTESIAN_POINT('Ctrl Pts',(-17.2161393118952,34.0916120771396,8.8858210138633));
#64998=CARTESIAN_POINT('Ctrl Pts',(-17.2565582793194,34.0866780326671,8.91499098457647));
#64999=CARTESIAN_POINT('Ctrl Pts',(-17.2985311606618,34.0817439881945,8.94168102577725));
#65000=CARTESIAN_POINT('Ctrl Pts',(-17.3405457934919,34.076805035703,8.96839761623778));
#65001=CARTESIAN_POINT('Ctrl Pts',(-17.3841169632708,34.0718660832114,8.99262905895595));
#65002=CARTESIAN_POINT('Ctrl Pts',(-17.428916880813,34.0669271307199,9.01420601106057));
#65003=CARTESIAN_POINT('Ctrl Pts',(-17.473741395472,34.0619854665271,9.03579480985688));
#65004=CARTESIAN_POINT('Ctrl Pts',(-17.519795494874,34.0570438023344,9.0547260078026));
#65005=CARTESIAN_POINT('Ctrl Pts',(-17.5667315843423,34.0521021381416,9.07087851867697));
#65006=CARTESIAN_POINT('Ctrl Pts',(-17.6137556714152,34.0471512091248,9.08706131290645));
#65007=CARTESIAN_POINT('Ctrl Pts',(-17.6616645218855,34.0422002801079,9.1004548750603));
#65008=CARTESIAN_POINT('Ctrl Pts',(-17.7100971451986,34.0372493510911,9.11098849671142));
#65009=CARTESIAN_POINT('Ctrl Pts',(-17.7343622653189,34.0347688972341,9.11626592290024));
#65010=CARTESIAN_POINT('Ctrl Pts',(-17.7587587284728,34.0322884433771,9.12082628997828));
#65011=CARTESIAN_POINT('Ctrl Pts',(-17.7832407132708,34.0298079895202,9.12466560608227));
#65012=CARTESIAN_POINT('Ctrl Pts',(-17.787543982134,34.0293719930134,9.12534045371341));
#65013=CARTESIAN_POINT('Ctrl Pts',(-17.7918507662628,34.0289359965067,9.12599316912035));
#65014=CARTESIAN_POINT('Ctrl Pts',(-17.7961609204192,34.0285,9.12662372762052));
#65015=CARTESIAN_POINT('',(-16.7144063041452,34.0285,7.97570050620834));
#65016=CARTESIAN_POINT('Origin',(-17.98,34.0285,7.87));
#65017=CARTESIAN_POINT('',(-19.249999578241,34.4358804771951,7.86896498015955));
#65018=CARTESIAN_POINT('Ctrl Pts',(-19.2499995766417,34.4359014004106,7.86896301890149));
#65019=CARTESIAN_POINT('Ctrl Pts',(-19.2499454334291,34.429303487383,7.80265336563593));
#65020=CARTESIAN_POINT('Ctrl Pts',(-19.2446942465949,34.4227055743554,7.73656774318384));
#65021=CARTESIAN_POINT('Ctrl Pts',(-19.2343727205358,34.4161076613278,7.67138208042656));
#65022=CARTESIAN_POINT('Ctrl Pts',(-19.2294208866225,34.4129422602719,7.64010874219643));
#65023=CARTESIAN_POINT('Ctrl Pts',(-19.223302717142,34.409776859216,7.6090421404699));
#65024=CARTESIAN_POINT('Ctrl Pts',(-19.2160359553257,34.40661145816,7.57825504778653));
#65025=CARTESIAN_POINT('Ctrl Pts',(-19.2046689857615,34.4016600068298,7.53009660330325));
#65026=CARTESIAN_POINT('Ctrl Pts',(-19.1904586753062,34.3967085554996,7.48249918143714));
#65027=CARTESIAN_POINT('Ctrl Pts',(-19.1734779460725,34.3917571041694,7.43582216519208));
#65028=CARTESIAN_POINT('Ctrl Pts',(-19.1565278826982,34.3868145947703,7.3892294439613));
#65029=CARTESIAN_POINT('Ctrl Pts',(-19.1368175094606,34.3818720853711,7.34355434149111));
#65030=CARTESIAN_POINT('Ctrl Pts',(-19.1144700226763,34.376929575972,7.29914295340351));
#65031=CARTESIAN_POINT('Ctrl Pts',(-19.0921447724198,34.3719919845418,7.25477575619416));
#65032=CARTESIAN_POINT('Ctrl Pts',(-19.0671878484165,34.3670543931117,7.21167027018952));
#65033=CARTESIAN_POINT('Ctrl Pts',(-19.0397704070058,34.3621168016816,7.17015238484737));
#65034=CARTESIAN_POINT('Ctrl Pts',(-19.0123686334772,34.3571820318715,7.12865822518136));
#65035=CARTESIAN_POINT('Ctrl Pts',(-18.9825094291592,34.3522472620613,7.08875032432696));
#65036=CARTESIAN_POINT('Ctrl Pts',(-18.9504084321542,34.3473124922512,7.05072747220235));
#65037=CARTESIAN_POINT('Ctrl Pts',(-18.9183121831044,34.342378452327,7.01271024391541));
#65038=CARTESIAN_POINT('Ctrl Pts',(-18.8839751532307,34.3374444124028,6.97657792775663));
#65039=CARTESIAN_POINT('Ctrl Pts',(-18.8476529763935,34.3325103724785,6.94259592811145));
#65040=CARTESIAN_POINT('Ctrl Pts',(-18.8112946685128,34.3275714244781,6.90858012528547));
#65041=CARTESIAN_POINT('Ctrl Pts',(-18.7729476720726,34.3226324764777,6.87671928311416));
#65042=CARTESIAN_POINT('Ctrl Pts',(-18.7329028661743,34.3176935284773,6.84724036347416));
#65043=CARTESIAN_POINT('Ctrl Pts',(-18.6928360736914,34.3127518687495,6.81774525844512));
#65044=CARTESIAN_POINT('Ctrl Pts',(-18.6510700747914,34.3078102090216,6.79063497815227));
#65045=CARTESIAN_POINT('Ctrl Pts',(-18.6079241248343,34.3028685492938,6.76609271519248));
#65046=CARTESIAN_POINT('Ctrl Pts',(-18.5646972822835,34.2979176246483,6.74150443893814));
#65047=CARTESIAN_POINT('Ctrl Pts',(-18.5200858156786,34.2929667000029,6.71949403160375));
#65048=CARTESIAN_POINT('Ctrl Pts',(-18.4744314489635,34.2880157753574,6.70019764820042));
#65049=CARTESIAN_POINT('Ctrl Pts',(-18.4515579037279,34.2855352853849,6.69052986107689));
#65050=CARTESIAN_POINT('Ctrl Pts',(-18.4284228494437,34.2830547954125,6.68154256543674));
#65051=CARTESIAN_POINT('Ctrl Pts',(-18.4050705842528,34.28057430544,6.67324814668915));
#65052=CARTESIAN_POINT('Ctrl Pts',(-18.3589291304473,34.2756731357871,6.65685930661915));
#65053=CARTESIAN_POINT('Ctrl Pts',(-18.3117254131915,34.2707719661342,6.6431029058274));
#65054=CARTESIAN_POINT('Ctrl Pts',(-18.2637934055715,34.2658707964813,6.63211418016274));
#65055=CARTESIAN_POINT('Ctrl Pts',(-18.2159493949058,34.2609786247408,6.62114562837436));
#65056=CARTESIAN_POINT('Ctrl Pts',(-18.1673802837452,34.2560864530002,6.6129348061338));
#65057=CARTESIAN_POINT('Ctrl Pts',(-18.1184367778866,34.2511942812597,6.60756772121101));
#65058=CARTESIAN_POINT('Ctrl Pts',(-18.0695425146008,34.2463070315842,6.60220603616845));
#65059=CARTESIAN_POINT('Ctrl Pts',(-18.0202751547846,34.2414197819088,6.5996824902367));
#65060=CARTESIAN_POINT('Ctrl Pts',(-17.970994919409,34.2365325322333,6.60003192617942));
#65061=CARTESIAN_POINT('Ctrl Pts',(-17.921742325506,34.2316480238349,6.60038116612218));
#65062=CARTESIAN_POINT('Ctrl Pts',(-17.8724774286441,34.2267635154366,6.60360019434172));
#65063=CARTESIAN_POINT('Ctrl Pts',(-17.823562126101,34.2218790070382,6.60967179210733));
#65064=CARTESIAN_POINT('Ctrl Pts',(-17.7746524847437,34.2169950639457,6.61574268717988));
#65065=CARTESIAN_POINT('Ctrl Pts',(-17.7260929120851,34.2121111208532,6.62466542637155));
#65066=CARTESIAN_POINT('Ctrl Pts',(-17.6782390964949,34.2072271777607,6.63637106181974));
#65067=CARTESIAN_POINT('Ctrl Pts',(-17.6303309640999,34.2023376911148,6.64808998383049));
#65068=CARTESIAN_POINT('Ctrl Pts',(-17.5831307319228,34.1974482044689,6.66259797245389));
#65069=CARTESIAN_POINT('Ctrl Pts',(-17.536980961493,34.192558717823,6.6797755961499));
#65070=CARTESIAN_POINT('Ctrl Pts',(-17.4908030027674,34.187666244677,6.69696371194442));
#65071=CARTESIAN_POINT('Ctrl Pts',(-17.4456772933211,34.1827737715309,6.71682447850852));
#65072=CARTESIAN_POINT('Ctrl Pts',(-17.40192482136,34.1778812983849,6.73919095872013));
#65073=CARTESIAN_POINT('Ctrl Pts',(-17.3580803849902,34.1729785416279,6.76160445159256));
#65074=CARTESIAN_POINT('Ctrl Pts',(-17.3156154268354,34.1680757848709,6.78653388232076));
#65075=CARTESIAN_POINT('Ctrl Pts',(-17.274823394364,34.1631730281139,6.81376803927184));
#65076=CARTESIAN_POINT('Ctrl Pts',(-17.2508725896127,34.1602944029826,6.82975841622004));
#65077=CARTESIAN_POINT('Ctrl Pts',(-17.2274979119499,34.1574157778513,6.84654252814164));
#65078=CARTESIAN_POINT('Ctrl Pts',(-17.2047531057044,34.15453715272,6.86407144742532));
#65079=CARTESIAN_POINT('Ctrl Pts',(-17.1632591851753,34.14928560469,6.89604989454266));
#65080=CARTESIAN_POINT('Ctrl Pts',(-17.1236685159173,34.14403405666,6.93066006210468));
#65081=CARTESIAN_POINT('Ctrl Pts',(-17.0863201058028,34.13878250863,6.96764959871027));
#65082=CARTESIAN_POINT('Ctrl Pts',(-17.0502648631405,34.1337127924629,7.00335839365478));
#65083=CARTESIAN_POINT('Ctrl Pts',(-17.0162995457397,34.1286430762957,7.04128408624179));
#65084=CARTESIAN_POINT('Ctrl Pts',(-16.9846970405727,34.1235733601286,7.08115779844429));
#65085=CARTESIAN_POINT('Ctrl Pts',(-16.9531357999906,34.1185102636814,7.12097944603434));
#65086=CARTESIAN_POINT('Ctrl Pts',(-16.9239315670765,34.1134471672341,7.16274366761761));
#65087=CARTESIAN_POINT('Ctrl Pts',(-16.897318768203,34.1083840707869,7.20614658973942));
#65088=CARTESIAN_POINT('Ctrl Pts',(-16.8707316582046,34.1033258616593,7.24950761577028));
#65089=CARTESIAN_POINT('Ctrl Pts',(-16.8467312842112,34.0982676525316,7.29450376745023));
#65090=CARTESIAN_POINT('Ctrl Pts',(-16.8255090619546,34.0932094434039,7.34080185755137));
#65091=CARTESIAN_POINT('Ctrl Pts',(-16.8043001092413,34.0881543970046,7.3870709990106));
#65092=CARTESIAN_POINT('Ctrl Pts',(-16.785866071209,34.0830993506054,7.43463999713855));
#65093=CARTESIAN_POINT('Ctrl Pts',(-16.7703516593605,34.0780443042061,7.48315262442644));
#65094=CARTESIAN_POINT('Ctrl Pts',(-16.7548369971137,34.0729891762198,7.53166603469493));
#65095=CARTESIAN_POINT('Ctrl Pts',(-16.7422422219879,34.0679340482334,7.58112262009095));
#65096=CARTESIAN_POINT('Ctrl Pts',(-16.7326626587095,34.0628789202471,7.63114950905991));
#65097=CARTESIAN_POINT('Ctrl Pts',(-16.7230831325064,34.0578238118254,7.68117620441224));
#65098=CARTESIAN_POINT('Ctrl Pts',(-16.7165188826359,34.0527687034036,7.73177269408068));
#65099=CARTESIAN_POINT('Ctrl Pts',(-16.7130139277447,34.0477135949819,7.78255691730597));
#65100=CARTESIAN_POINT('Ctrl Pts',(-16.7095063931632,34.0426547659376,7.83337851835005));
#65101=CARTESIAN_POINT('Ctrl Pts',(-16.7090626718887,34.0375959368933,7.88438761672372));
#65102=CARTESIAN_POINT('Ctrl Pts',(-16.7116747290644,34.032537107849,7.93519974774569));
#65103=CARTESIAN_POINT('Ctrl Pts',(-16.712369564202,34.0311914052327,7.94871631789656));
#65104=CARTESIAN_POINT('Ctrl Pts',(-16.713280345878,34.0298457026163,7.96221896542966));
#65105=CARTESIAN_POINT('Ctrl Pts',(-16.7144063041452,34.0285,7.97570050620834));
#65106=CARTESIAN_POINT('Ctrl Pts',(-19.2499995788896,34.435871992073,7.86896577552077));
#65107=CARTESIAN_POINT('Ctrl Pts',(-19.2500561832405,34.4423874535631,7.93847438149077));
#65108=CARTESIAN_POINT('Ctrl Pts',(-19.2444064699017,34.448898524241,8.00786438420913));
#65109=CARTESIAN_POINT('Ctrl Pts',(-19.2297862522652,34.4575354975776,8.09661020094649));
#65110=CARTESIAN_POINT('Ctrl Pts',(-19.2259771711595,34.4595105479342,8.1166954469874));
#65111=CARTESIAN_POINT('Ctrl Pts',(-19.218134183589,34.4631464043062,8.15321324412816));
#65112=CARTESIAN_POINT('Ctrl Pts',(-19.214253362788,34.4648022192572,8.16967410323797));
#65113=CARTESIAN_POINT('Ctrl Pts',(-19.2055381018845,34.4682533448045,8.20359313464447));
#65114=CARTESIAN_POINT('Ctrl Pts',(-19.2006565261306,34.4700498023201,8.22103500930035));
#65115=CARTESIAN_POINT('Ctrl Pts',(-19.1885295438783,34.474225864029,8.26104740325841));
#65116=CARTESIAN_POINT('Ctrl Pts',(-19.1810221144874,34.4766134614314,8.28353043061039));
#65117=CARTESIAN_POINT('Ctrl Pts',(-19.1396848304862,34.48885402516,8.39668365613964));
#65118=CARTESIAN_POINT('Ctrl Pts',(-19.0962061968643,34.4990205318921,8.48346514625448));
#65119=CARTESIAN_POINT('Ctrl Pts',(-19.0218803611092,34.5133528401569,8.59727026210805));
#65120=CARTESIAN_POINT('Ctrl Pts',(-18.9989352040304,34.5174792966232,8.62908378191094));
#65121=CARTESIAN_POINT('Ctrl Pts',(-18.9587636195176,34.5242007179762,8.67967059086213));
#65122=CARTESIAN_POINT('Ctrl Pts',(-18.9423791036808,34.5268214051788,8.69907866701827));
#65123=CARTESIAN_POINT('Ctrl Pts',(-18.917345419193,34.5306399845124,8.72698884109266));
#65124=CARTESIAN_POINT('Ctrl Pts',(-18.9091401754607,34.5318640272109,8.73587810070143));
#65125=CARTESIAN_POINT('Ctrl Pts',(-18.8936886793601,34.5341166862003,8.75214504195841));
#65126=CARTESIAN_POINT('Ctrl Pts',(-18.8864778356671,34.5351473863616,8.7595531618484));
#65127=CARTESIAN_POINT('Ctrl Pts',(-18.86772814022,34.5377773886837,8.77835100657601));
#65128=CARTESIAN_POINT('Ctrl Pts',(-18.8560600923456,34.5393669515313,8.78960948747787));
#65129=CARTESIAN_POINT('Ctrl Pts',(-18.8330834518678,34.5424159449781,8.81094520262985));
#65130=CARTESIAN_POINT('Ctrl Pts',(-18.8218085718806,34.5438761809861,8.82104536020224));
#65131=CARTESIAN_POINT('Ctrl Pts',(-18.8103597424409,34.5453270911211,8.83093844658933));
#65132=CARTESIAN_POINT('Origin',(-17.98,34.0285,7.87));
#65133=CARTESIAN_POINT('',(-18.5116348366204,34.0285,6.25069791697424));
#65134=CARTESIAN_POINT('',(-19.68434,34.0285,7.87));
#65135=CARTESIAN_POINT('Origin',(-17.98,34.0285,7.87));
#65136=CARTESIAN_POINT('Ctrl Pts',(-18.5116348366204,34.0285,6.25069791697424));
#65137=CARTESIAN_POINT('Ctrl Pts',(-18.4477983675585,34.0285,6.23870611066214));
#65138=CARTESIAN_POINT('Ctrl Pts',(-18.3832442000431,34.0285,6.23070689758999));
#65139=CARTESIAN_POINT('Ctrl Pts',(-18.3183243142307,34.0285,6.22660131571174));
#65140=CARTESIAN_POINT('Ctrl Pts',(-18.2609661061129,34.0285,6.22297393995667));
#65141=CARTESIAN_POINT('Ctrl Pts',(-18.2033219294552,34.0285,6.22238700818959));
#65142=CARTESIAN_POINT('Ctrl Pts',(-18.1456465741428,34.0285,6.22480389998478));
#65143=CARTESIAN_POINT('Ctrl Pts',(-18.1314043910992,34.0285,6.22540072015445));
#65144=CARTESIAN_POINT('Ctrl Pts',(-18.1171699644767,34.0285,6.22618044836808));
#65145=CARTESIAN_POINT('Ctrl Pts',(-18.1029488004271,34.0285,6.2271419028461));
#65146=CARTESIAN_POINT('Ctrl Pts',(-18.039457939995,34.0285,6.23143434837749));
#65147=CARTESIAN_POINT('Ctrl Pts',(-17.9762179002088,34.0285,6.23934585586296));
#65148=CARTESIAN_POINT('Ctrl Pts',(-17.9135732010023,34.0285,6.25080658082955));
#65149=CARTESIAN_POINT('Ctrl Pts',(-17.8717765066452,34.0285,6.2584532041609));
#65150=CARTESIAN_POINT('Ctrl Pts',(-17.8302452091138,34.0285,6.26768078671085));
#65151=CARTESIAN_POINT('Ctrl Pts',(-17.7890894280646,34.0285,6.27847894017026));
#65152=CARTESIAN_POINT('Ctrl Pts',(-17.7738772006603,34.0285,6.28247021337135));
#65153=CARTESIAN_POINT('Ctrl Pts',(-17.7587122268377,34.0285,6.28667749313672));
#65154=CARTESIAN_POINT('Ctrl Pts',(-17.7436272591778,34.0285,6.29109218874144));
#65155=CARTESIAN_POINT('Ctrl Pts',(-17.684577575458,34.0285,6.30837339113148));
#65156=CARTESIAN_POINT('Ctrl Pts',(-17.6266753461434,34.0285,6.32884750660487));
#65157=CARTESIAN_POINT('Ctrl Pts',(-17.5702302830355,34.0285,6.35244256448365));
#65158=CARTESIAN_POINT('Ctrl Pts',(-17.5152199185782,34.0285,6.37543789236239));
#65159=CARTESIAN_POINT('Ctrl Pts',(-17.4615928472096,34.0285,6.40139816138878));
#65160=CARTESIAN_POINT('Ctrl Pts',(-17.4096690783012,34.0285,6.4302922821505));
#65161=CARTESIAN_POINT('Ctrl Pts',(-17.3782632796365,34.0285,6.44776872806942));
#65162=CARTESIAN_POINT('Ctrl Pts',(-17.3474813084972,34.0285,6.46631913073517));
#65163=CARTESIAN_POINT('Ctrl Pts',(-17.3174017826758,34.0285,6.48594174657202));
#65164=CARTESIAN_POINT('Ctrl Pts',(-17.2924442615412,34.0285,6.50222298226608));
#65165=CARTESIAN_POINT('Ctrl Pts',(-17.267970417772,34.0285,6.51924244114969));
#65166=CARTESIAN_POINT('Ctrl Pts',(-17.2440288126058,34.0285,6.53700081495576));
#65167=CARTESIAN_POINT('Ctrl Pts',(-17.2333815441399,34.0285,6.5448982876657));
#65168=CARTESIAN_POINT('Ctrl Pts',(-17.2228371138846,34.0285,6.55294403764358));
#65169=CARTESIAN_POINT('Ctrl Pts',(-17.2124195643277,34.0285,6.56112233024434));
#65170=CARTESIAN_POINT('Ctrl Pts',(-17.1676647316062,34.0285,6.59625709157124));
#65171=CARTESIAN_POINT('Ctrl Pts',(-17.1251724160825,34.0285,6.63388991678137));
#65172=CARTESIAN_POINT('Ctrl Pts',(-17.0852264667732,34.0285,6.67398593907778));
#65173=CARTESIAN_POINT('Ctrl Pts',(-17.080151930788,34.0285,6.6790795395936));
#65174=CARTESIAN_POINT('Ctrl Pts',(-17.0751185456676,34.0285,6.68421292889612));
#65175=CARTESIAN_POINT('Ctrl Pts',(-17.0701269456468,34.0285,6.68938606742345));
#65176=CARTESIAN_POINT('Ctrl Pts',(-17.029744147875,34.0285,6.73123753912078));
#65177=CARTESIAN_POINT('Ctrl Pts',(-16.9920920490028,34.0285,6.77568953714568));
#65178=CARTESIAN_POINT('Ctrl Pts',(-16.9572880675087,34.0285,6.82243210278544));
#65179=CARTESIAN_POINT('Ctrl Pts',(-16.9270997258523,34.0285,6.86297575557615));
#65180=CARTESIAN_POINT('Ctrl Pts',(-16.8990548859259,34.0285,6.90524353527338));
#65181=CARTESIAN_POINT('Ctrl Pts',(-16.8732618745741,34.0285,6.94903484153182));
#65182=CARTESIAN_POINT('Ctrl Pts',(-16.8681371425678,34.0285,6.95773559793896));
#65183=CARTESIAN_POINT('Ctrl Pts',(-16.8631002530348,34.0285,6.96649853884193));
#65184=CARTESIAN_POINT('Ctrl Pts',(-16.858155953323,34.0285,6.97531533866574));
#65185=CARTESIAN_POINT('Ctrl Pts',(-16.8306640666196,34.0285,7.02433956372781));
#65186=CARTESIAN_POINT('Ctrl Pts',(-16.8061063757587,34.0285,7.07488941615454));
#65187=CARTESIAN_POINT('Ctrl Pts',(-16.7845650810918,34.0285,7.12667245441139));
#65188=CARTESIAN_POINT('Ctrl Pts',(-16.763360070835,34.0285,7.17764709982381));
#65189=CARTESIAN_POINT('Ctrl Pts',(-16.7450780721175,34.0285,7.22981788604346));
#65190=CARTESIAN_POINT('Ctrl Pts',(-16.7298468231901,34.0285,7.28290675957567));
#65191=CARTESIAN_POINT('Ctrl Pts',(-16.7147402924653,34.0285,7.33556092490247));
#65192=CARTESIAN_POINT('Ctrl Pts',(-16.7026347861426,34.0285,7.38911923149214));
#65193=CARTESIAN_POINT('Ctrl Pts',(-16.6937032695783,34.0285,7.44329516703774));
#65194=CARTESIAN_POINT('Ctrl Pts',(-16.6920623691379,34.0285,7.45324838336542));
#65195=CARTESIAN_POINT('Ctrl Pts',(-16.6905287322653,34.0285,7.46322238082028));
#65196=CARTESIAN_POINT('Ctrl Pts',(-16.6891036091325,34.0285,7.47321528432834));
#65197=CARTESIAN_POINT('Ctrl Pts',(-16.6875741705604,34.0285,7.48393964331189));
#65198=CARTESIAN_POINT('Ctrl Pts',(-16.686170862869,34.0285,7.49467810037056));
#65199=CARTESIAN_POINT('Ctrl Pts',(-16.6848954111995,34.0285,7.50542132298178));
#65200=CARTESIAN_POINT('Ctrl Pts',(-16.6786799335084,34.0285,7.55777474574567));
#65201=CARTESIAN_POINT('Ctrl Pts',(-16.6754890773626,34.0285,7.61029605110518));
#65202=CARTESIAN_POINT('Ctrl Pts',(-16.6754319365421,34.0285,7.66273374271887));
#65203=CARTESIAN_POINT('Ctrl Pts',(-16.6753745061326,34.0285,7.71543718793836));
#65204=CARTESIAN_POINT('Ctrl Pts',(-16.6784826472741,34.0285,7.7680571926682));
#65205=CARTESIAN_POINT('Ctrl Pts',(-16.6849167607292,34.0285,7.82031641789131));
#65206=CARTESIAN_POINT('Ctrl Pts',(-16.6910111090541,34.0285,7.86981599913381));
#65207=CARTESIAN_POINT('Ctrl Pts',(-16.7000898992755,34.0285,7.91899240774701));
#65208=CARTESIAN_POINT('Ctrl Pts',(-16.712329638489,34.0285,7.96757972342322));
#65209=CARTESIAN_POINT('Ctrl Pts',(-16.7130120144162,34.0285,7.97028850781839));
#65210=CARTESIAN_POINT('Ctrl Pts',(-16.7137042249467,34.0285,7.97299545191025));
#65211=CARTESIAN_POINT('Ctrl Pts',(-16.7144063041452,34.0285,7.97570050620834));
#65212=CARTESIAN_POINT('Ctrl Pts',(-17.7958274652882,34.0285,9.12890304511207));
#65213=CARTESIAN_POINT('Ctrl Pts',(-17.8438421718885,34.0285,9.14456709927581));
#65214=CARTESIAN_POINT('Ctrl Pts',(-17.89277854746,34.0285,9.15703166260375));
#65215=CARTESIAN_POINT('Ctrl Pts',(-17.9423455702771,34.0285,9.16645118943153));
#65216=CARTESIAN_POINT('Ctrl Pts',(-17.9788483505988,34.0285,9.1733880377429));
#65217=CARTESIAN_POINT('Ctrl Pts',(-18.0156941104094,34.0285,9.17867267409858));
#65218=CARTESIAN_POINT('Ctrl Pts',(-18.0527778734286,34.0285,9.18235277161469));
#65219=CARTESIAN_POINT('Ctrl Pts',(-18.0659311497185,34.0285,9.1836580690134));
#65220=CARTESIAN_POINT('Ctrl Pts',(-18.079116397763,34.0285,9.18476152516703));
#65221=CARTESIAN_POINT('Ctrl Pts',(-18.0923229261104,34.0285,9.18566448225191));
#65222=CARTESIAN_POINT('Ctrl Pts',(-18.1454432003452,34.0285,9.18929642296404));
#65223=CARTESIAN_POINT('Ctrl Pts',(-18.1987891581145,34.0285,9.18968112794214));
#65224=CARTESIAN_POINT('Ctrl Pts',(-18.2520569989133,34.0285,9.18697003409754));
#65225=CARTESIAN_POINT('Ctrl Pts',(-18.2901479978194,34.0285,9.18503137333863));
#65226=CARTESIAN_POINT('Ctrl Pts',(-18.3281998805904,34.0285,9.18150876304076));
#65227=CARTESIAN_POINT('Ctrl Pts',(-18.3661092456966,34.0285,9.17644326610694));
#65228=CARTESIAN_POINT('Ctrl Pts',(-18.3781547717082,34.0285,9.17483372780664));
#65229=CARTESIAN_POINT('Ctrl Pts',(-18.3901878310136,34.0285,9.17306802072464));
#65230=CARTESIAN_POINT('Ctrl Pts',(-18.4021992137758,34.0285,9.17114816946817));
#65231=CARTESIAN_POINT('Ctrl Pts',(-18.4576095783033,34.0285,9.16229159899116));
#65232=CARTESIAN_POINT('Ctrl Pts',(-18.5123949314096,34.0285,9.15018542975578));
#65233=CARTESIAN_POINT('Ctrl Pts',(-18.5662341053607,34.0285,9.13499667932461));
#65234=CARTESIAN_POINT('Ctrl Pts',(-18.6200732793119,34.0285,9.11980792889344));
#65235=CARTESIAN_POINT('Ctrl Pts',(-18.6729674045624,34.0285,9.10153660156417));
#65236=CARTESIAN_POINT('Ctrl Pts',(-18.7246136905742,34.0285,9.08030056607039));
#65237=CARTESIAN_POINT('Ctrl Pts',(-18.7576957896348,34.0285,9.06669779452361));
#65238=CARTESIAN_POINT('Ctrl Pts',(-18.7902662184505,34.0285,9.0518775916147));
#65239=CARTESIAN_POINT('Ctrl Pts',(-18.8222460418491,34.0285,9.03586036752327));
#65240=CARTESIAN_POINT('Ctrl Pts',(-18.8502323779702,34.0285,9.02184329771136));
#65241=CARTESIAN_POINT('Ctrl Pts',(-18.8777664606405,34.0285,9.0069093719839));
#65242=CARTESIAN_POINT('Ctrl Pts',(-18.9047943322193,34.0285,8.99106711939537));
#65243=CARTESIAN_POINT('Ctrl Pts',(-18.913064824246,34.0285,8.98621941160102));
#65244=CARTESIAN_POINT('Ctrl Pts',(-18.9212849235068,34.0285,8.9812882991084));
#65245=CARTESIAN_POINT('Ctrl Pts',(-18.9294459656864,34.0285,8.97627873609161));
#65246=CARTESIAN_POINT('Ctrl Pts',(-18.9797430547245,34.0285,8.94540443945738));
#65247=CARTESIAN_POINT('Ctrl Pts',(-19.0278778119151,34.0285,8.91150716656161));
#65248=CARTESIAN_POINT('Ctrl Pts',(-19.0735206728694,34.0285,8.87472873332212));
#65249=CARTESIAN_POINT('Ctrl Pts',(-19.0792370626728,34.0285,8.87012253957442));
#65250=CARTESIAN_POINT('Ctrl Pts',(-19.0849143688835,34.0285,8.86547108651176));
#65251=CARTESIAN_POINT('Ctrl Pts',(-19.0905519435273,34.0285,8.86077459547289));
#65252=CARTESIAN_POINT('Ctrl Pts',(-19.1339677064135,34.0285,8.82460625106497));
#65253=CARTESIAN_POINT('Ctrl Pts',(-19.1750287637336,34.0285,8.78577085039626));
#65254=CARTESIAN_POINT('Ctrl Pts',(-19.2137029428852,34.0285,8.74456929570144));
#65255=CARTESIAN_POINT('Ctrl Pts',(-19.234699233103,34.0285,8.72220088818067));
#65256=CARTESIAN_POINT('Ctrl Pts',(-19.2549916655178,34.0285,8.69913421137922));
#65257=CARTESIAN_POINT('Ctrl Pts',(-19.2745721746555,34.0285,8.67541188309048));
#65258=CARTESIAN_POINT('Ctrl Pts',(-19.2887649969517,34.0285,8.65821688639835));
#65259=CARTESIAN_POINT('Ctrl Pts',(-19.3025837319496,34.0285,8.64067733049516));
#65260=CARTESIAN_POINT('Ctrl Pts',(-19.3160244998568,34.0285,8.62280834510891));
#65261=CARTESIAN_POINT('Ctrl Pts',(-19.3251656884946,34.0285,8.61065548544268));
#65262=CARTESIAN_POINT('Ctrl Pts',(-19.3341353501016,34.0285,8.59834525568747));
#65263=CARTESIAN_POINT('Ctrl Pts',(-19.3429129178832,34.0285,8.58591015550462));
#65264=CARTESIAN_POINT('Ctrl Pts',(-19.3772396241466,34.0285,8.53727982396515));
#65265=CARTESIAN_POINT('Ctrl Pts',(-19.4086800748933,34.0285,8.48668186632755));
#65266=CARTESIAN_POINT('Ctrl Pts',(-19.4372102427494,34.0285,8.43446034078614));
#65267=CARTESIAN_POINT('Ctrl Pts',(-19.4666484450477,34.0285,8.38057675198429));
#65268=CARTESIAN_POINT('Ctrl Pts',(-19.4929888584362,34.0285,8.32496401828332));
#65269=CARTESIAN_POINT('Ctrl Pts',(-19.5161757455008,34.0285,8.26795179493227));
#65270=CARTESIAN_POINT('Ctrl Pts',(-19.5393626325653,34.0285,8.21093957158123));
#65271=CARTESIAN_POINT('Ctrl Pts',(-19.5593965687678,34.0285,8.15252693850102));
#65272=CARTESIAN_POINT('Ctrl Pts',(-19.5761835248491,34.0285,8.09300780438079));
#65273=CARTESIAN_POINT('Ctrl Pts',(-19.5793637812432,34.0285,8.08173201942358));
#65274=CARTESIAN_POINT('Ctrl Pts',(-19.5824273766733,34.0285,8.07041644188063));
#65275=CARTESIAN_POINT('Ctrl Pts',(-19.5853734902581,34.0285,8.05906296865037));
#65276=CARTESIAN_POINT('Ctrl Pts',(-19.5884200416724,34.0285,8.0473224369528));
#65277=CARTESIAN_POINT('Ctrl Pts',(-19.5913389660892,34.0285,8.03554884052617));
#65278=CARTESIAN_POINT('Ctrl Pts',(-19.5941280042834,34.0285,8.02375265392161));
#65279=CARTESIAN_POINT('Ctrl Pts',(-19.6089012698,34.0285,7.9612693945833));
#65280=CARTESIAN_POINT('Ctrl Pts',(-19.6200513196573,34.0285,7.89808613178614));
#65281=CARTESIAN_POINT('Ctrl Pts',(-19.6275294811123,34.0285,7.83455530273799));
#65282=CARTESIAN_POINT('Ctrl Pts',(-19.6350208727503,34.0285,7.77091207647897));
#65283=CARTESIAN_POINT('Ctrl Pts',(-19.6388279358374,34.0285,7.70691905863735));
#65284=CARTESIAN_POINT('Ctrl Pts',(-19.6388604237698,34.0285,7.64289952645537));
#65285=CARTESIAN_POINT('Ctrl Pts',(-19.6388926236947,34.0285,7.57944753110339));
#65286=CARTESIAN_POINT('Ctrl Pts',(-19.6352173525578,34.0285,7.51596845155174));
#65287=CARTESIAN_POINT('Ctrl Pts',(-19.6276985634618,34.0285,7.45276180285684));
#65288=CARTESIAN_POINT('Ctrl Pts',(-19.626277169771,34.0285,7.44081286659565));
#65289=CARTESIAN_POINT('Ctrl Pts',(-19.6247182640679,34.0285,7.42887364845075));
#65290=CARTESIAN_POINT('Ctrl Pts',(-19.6230207093981,34.0285,7.41694615762716));
#65291=CARTESIAN_POINT('Origin',(-17.98,34.0285,7.87));
#65292=CARTESIAN_POINT('Ctrl Pts',(-18.5714796494485,41.7180970761119,8.99125045312017));
#65293=CARTESIAN_POINT('Ctrl Pts',(-18.9443656600646,41.6760846918719,8.79454641948545));
#65294=CARTESIAN_POINT('Ctrl Pts',(-19.4718969281881,41.5920599233919,8.00298830736167));
#65295=CARTESIAN_POINT('Ctrl Pts',(-18.9000484458028,41.4660227706719,6.68614628737439));
#65296=CARTESIAN_POINT('Ctrl Pts',(-17.4844919540699,41.3399856179519,6.45621531221888));
#65297=CARTESIAN_POINT('Ctrl Pts',(-16.5232775015748,41.213948465232,7.51911552834859));
#65298=CARTESIAN_POINT('Ctrl Pts',(-16.8953504400754,41.0879113125119,8.90400264567513));
#65299=CARTESIAN_POINT('Ctrl Pts',(-18.2606051857913,40.961874159792,9.34187611889218));
#65300=CARTESIAN_POINT('Ctrl Pts',(-19.368874647327,40.8358370070719,8.43242596995452));
#65301=CARTESIAN_POINT('Ctrl Pts',(-19.2056642802028,40.709799854352,7.00797545227637));
#65302=CARTESIAN_POINT('Ctrl Pts',(-17.9203268783257,40.5837627016319,6.37276257178433));
#65303=CARTESIAN_POINT('Ctrl Pts',(-16.6896320092116,40.457725548912,7.10825717650556));
#65304=CARTESIAN_POINT('Ctrl Pts',(-16.6402725882592,40.3316883961919,8.54114494966668));
#65305=CARTESIAN_POINT('Ctrl Pts',(-17.8174461113438,40.205651243472,9.3595885920492));
#65306=CARTESIAN_POINT('Ctrl Pts',(-19.143437440358,40.079614090752,8.81430625229477));
#65307=CARTESIAN_POINT('Ctrl Pts',(-19.404294163858,39.953576938032,7.40450320966821));
#65308=CARTESIAN_POINT('Ctrl Pts',(-18.3611989837821,39.827539785312,6.42086660001849));
#65309=CARTESIAN_POINT('Ctrl Pts',(-16.9691135802101,39.701502632592,6.76392163550818));
#65310=CARTESIAN_POINT('Ctrl Pts',(-16.5025018622442,39.575465479872,8.11959955528859));
#65311=CARTESIAN_POINT('Ctrl Pts',(-17.3885503485607,39.449428327152,9.24676719033193));
#65312=CARTESIAN_POINT('Ctrl Pts',(-18.8160752155619,39.323391174432,9.11349462344888));
#65313=CARTESIAN_POINT('Ctrl Pts',(-19.4781672291768,39.197354021712,7.84179377198361));
#65314=CARTESIAN_POINT('Ctrl Pts',(-18.7686763775428,39.071316868992,6.59591593747959));
#65315=CARTESIAN_POINT('Ctrl Pts',(-17.3371466403695,38.945279716272,6.51647120732814));
#65316=CARTESIAN_POINT('Ctrl Pts',(-16.494153769907,38.819242563552,7.67619181215477));
#65317=CARTESIAN_POINT('Ctrl Pts',(-17.0114637963517,38.693205410832,9.0133452034285));
#65318=CARTESIAN_POINT('Ctrl Pts',(-18.415475673635,38.567168258112,9.30375784937852));
#65319=CARTESIAN_POINT('Ctrl Pts',(-19.4208064439724,38.441131105392,8.28155488545429));
#65320=CARTESIAN_POINT('Ctrl Pts',(-19.1070685657665,38.315093952672,6.88257046799409));
#65321=CARTESIAN_POINT('Ctrl Pts',(-17.761491320168,38.189056799952,6.38758487946864));
#65322=CARTESIAN_POINT('Ctrl Pts',(-16.6159603404313,38.063019647232,7.24976098169606));
#65323=CARTESIAN_POINT('Ctrl Pts',(-16.7192174666317,37.936982494512,8.67977036019592));
#65324=CARTESIAN_POINT('Ctrl Pts',(-17.9767300580474,37.810945341792,9.36842915754399));
#65325=CARTESIAN_POINT('Ctrl Pts',(-19.2372363048034,37.6849081890721,8.68526529828479));
#65326=CARTESIAN_POINT('Ctrl Pts',(-19.3467336840785,37.558871036352,7.25572020255653));
#65327=CARTESIAN_POINT('Ctrl Pts',(-18.2049765586077,37.4328338836321,6.38855267366891));
#65328=CARTESIAN_POINT('Ctrl Pts',(-16.8572517778355,37.306796730912,6.87766081284674));
#65329=CARTESIAN_POINT('Ctrl Pts',(-16.537411058784,37.1807595781921,8.27526260580466));
#65330=CARTESIAN_POINT('Ctrl Pts',(-17.5382708774487,37.054722425472,9.30184357185776));
#65331=CARTESIAN_POINT('Ctrl Pts',(-18.9435368801747,36.928685272752,9.01756146401863));
#65332=CARTESIAN_POINT('Ctrl Pts',(-19.466677949177,36.8026481200321,7.68267859169109));
#65333=CARTESIAN_POINT('Ctrl Pts',(-18.628754675352,36.676610967312,6.5192898171438));
#65334=CARTESIAN_POINT('Ctrl Pts',(-17.1968918401205,36.5505738145921,6.59248591091588));
#65335=CARTESIAN_POINT('Ctrl Pts',(-16.4819701427196,36.424536661872,7.83525534113844));
#65336=CARTESIAN_POINT('Ctrl Pts',(-17.1385055544403,36.2984995091521,9.10983373266509));
#65337=CARTESIAN_POINT('Ctrl Pts',(-18.5654351459831,36.172462356432,9.24933548309321));
#65338=CARTESIAN_POINT('Ctrl Pts',(-19.4563947146754,36.0464252037121,8.12604559865597));
#65339=CARTESIAN_POINT('Ctrl Pts',(-18.9957042014948,35.9203880509921,6.7683443136604));
#65340=CARTESIAN_POINT('Ctrl Pts',(-17.6051294267902,35.7943508982721,6.41921635646431));
#65341=CARTESIAN_POINT('Ctrl Pts',(-16.5577508962692,35.6683137455521,7.39829197305275));
#65342=CARTESIAN_POINT('Ctrl Pts',(-16.8124525466696,35.5422765928321,8.80921823049927));
#65343=CARTESIAN_POINT('Ctrl Pts',(-18.1360504665275,35.4162394401121,9.3602863258882));
#65344=CARTESIAN_POINT('Ctrl Pts',(-19.3167866617019,35.2902022873921,8.54698087261944));
#65345=CARTESIAN_POINT('Ctrl Pts',(-19.2736779139766,35.1641651346721,7.11390592332082));
#65346=CARTESIAN_POINT('Ctrl Pts',(-18.0462119602502,35.0381279819521,6.37301796104198));
#65347=CARTESIAN_POINT('Ctrl Pts',(-16.7581002235375,34.9120908292321,7.00267267196968));
#65348=CARTESIAN_POINT('Ctrl Pts',(-16.5887026766086,34.7860536765121,8.42628260585971));
#65349=CARTESIAN_POINT('Ctrl Pts',(-17.6929361751755,34.6600165237921,9.34078907379165));
#65350=CARTESIAN_POINT('Ctrl Pts',(-19.0602006334414,34.5339793710721,8.90842522185144));
#65351=CARTESIAN_POINT('Ctrl Pts',(-19.4380918746699,34.4079422183521,7.52607638637724));
#65352=CARTESIAN_POINT('Ctrl Pts',(-18.4819749584899,34.2819050656321,6.45719431747657));
#65353=CARTESIAN_POINT('Ctrl Pts',(-17.0643238211113,34.1558567053176,6.68460455611039));
#65354=CARTESIAN_POINT('Ctrl Pts',(-16.6815128915769,34.071820729243,7.55561568178109));
#65355=CARTESIAN_POINT('Ctrl Pts',(-16.7167313810425,34.0297971374084,7.97584489432982));
#65356=CARTESIAN_POINT('Ctrl Pts',(-18.6397356458259,41.6336362795415,9.12064132385885));
#65357=CARTESIAN_POINT('Ctrl Pts',(-19.0556522259867,41.5916238953015,8.90123789588367));
#65358=CARTESIAN_POINT('Ctrl Pts',(-19.6440599289284,41.5075991268215,8.01833498823901));
#65359=CARTESIAN_POINT('Ctrl Pts',(-19.0062208617807,41.3815619741013,6.54953108041721));
#65360=CARTESIAN_POINT('Ctrl Pts',(-17.4273109582073,41.2555248213815,6.29306636429208));
#65361=CARTESIAN_POINT('Ctrl Pts',(-16.3551735851203,41.1294876686615,7.47862390831015));
#65362=CARTESIAN_POINT('Ctrl Pts',(-16.7701832656815,41.0034505159415,9.02332523082788));
#65363=CARTESIAN_POINT('Ctrl Pts',(-18.2929866659701,40.8774133632215,9.51172874380123));
#65364=CARTESIAN_POINT('Ctrl Pts',(-19.5291490083893,40.7513762105015,8.49732920881249));
#65365=CARTESIAN_POINT('Ctrl Pts',(-19.3471043732769,40.6253390577815,6.90849892005496));
#65366=CARTESIAN_POINT('Ctrl Pts',(-17.9134406762718,40.4993019050615,6.19998328415929));
#65367=CARTESIAN_POINT('Ctrl Pts',(-16.540725190546,40.3732647523415,7.02035302722595));
#65368=CARTESIAN_POINT('Ctrl Pts',(-16.4856697554351,40.2472275996215,8.61859421997696));
#65369=CARTESIAN_POINT('Ctrl Pts',(-17.7986876001328,40.1211904469015,9.53148521374625));
#65370=CARTESIAN_POINT('Ctrl Pts',(-19.2776966355619,39.9951532941815,8.9232779881709));
#65371=CARTESIAN_POINT('Ctrl Pts',(-19.5686558919062,39.8691161414615,7.35078547438482));
#65372=CARTESIAN_POINT('Ctrl Pts',(-18.4051888598166,39.7430789887415,6.25363845583508));
#65373=CARTESIAN_POINT('Ctrl Pts',(-16.852458578011,39.6170418360215,6.63628160442634));
#65374=CARTESIAN_POINT('Ctrl Pts',(-16.3320004635361,39.4910046833015,8.14840302529378));
#65375=CARTESIAN_POINT('Ctrl Pts',(-17.3202978139153,39.3649675305815,9.40564436631503));
#65376=CARTESIAN_POINT('Ctrl Pts',(-18.9125572279824,39.2389303778615,9.2569923153688));
#65377=CARTESIAN_POINT('Ctrl Pts',(-19.6510538146457,39.1128932251415,7.83853880928271));
#65378=CARTESIAN_POINT('Ctrl Pts',(-18.8596886245723,38.9868560724214,6.44888826334574));
#65379=CARTESIAN_POINT('Ctrl Pts',(-17.2629621834282,38.8608189197014,6.36027571276549));
#65380=CARTESIAN_POINT('Ctrl Pts',(-16.3226890120016,38.7347817669814,7.65382659472116));
#65381=CARTESIAN_POINT('Ctrl Pts',(-16.8996959550249,38.6087446142615,9.14528578014338));
#65382=CARTESIAN_POINT('Ctrl Pts',(-18.465729010381,38.4827074615415,9.46921167465304));
#65383=CARTESIAN_POINT('Ctrl Pts',(-19.5870736680637,38.3566703088215,8.3290477937849));
#65384=CARTESIAN_POINT('Ctrl Pts',(-19.2371308392764,38.2306331561015,6.76862236069675));
#65385=CARTESIAN_POINT('Ctrl Pts',(-17.7362756974954,38.1045960033815,6.21651606722604));
#65386=CARTESIAN_POINT('Ctrl Pts',(-16.4585519052485,37.9785588506615,7.1781861908711));
#65387=CARTESIAN_POINT('Ctrl Pts',(-16.5737247719793,37.8525216979416,8.77321682589191));
#65388=CARTESIAN_POINT('Ctrl Pts',(-17.976352710921,37.7264845452215,9.541345969212));
#65389=CARTESIAN_POINT('Ctrl Pts',(-19.382319769207,37.6004473925016,8.77934587282061));
#65390=CARTESIAN_POINT('Ctrl Pts',(-19.5044530062501,37.4744102397814,7.1848330982105));
#65391=CARTESIAN_POINT('Ctrl Pts',(-18.2309385662332,37.3483730870616,6.21759554364139));
#65392=CARTESIAN_POINT('Ctrl Pts',(-16.7276880664614,37.2223359343414,6.76314613761378));
#65393=CARTESIAN_POINT('Ctrl Pts',(-16.3709381367864,37.0962987816215,8.32202939309731));
#65394=CARTESIAN_POINT('Ctrl Pts',(-17.4872959006819,36.9702616289015,9.46707649195042));
#65395=CARTESIAN_POINT('Ctrl Pts',(-19.0547278059556,36.8442244761816,9.14998859182253));
#65396=CARTESIAN_POINT('Ctrl Pts',(-19.6382386864027,36.7181873234616,7.66106194033403));
#65397=CARTESIAN_POINT('Ctrl Pts',(-18.7036201365931,36.5921501707416,6.36341958655524));
#65398=CARTESIAN_POINT('Ctrl Pts',(-17.1065221583002,36.4661130180216,6.44506241609585));
#65399=CARTESIAN_POINT('Ctrl Pts',(-16.3090994097922,36.3400758653015,7.83124585186588));
#65400=CARTESIAN_POINT('Ctrl Pts',(-17.0413981697968,36.2140387125816,9.2529089624626));
#65401=CARTESIAN_POINT('Ctrl Pts',(-18.6329936143779,36.0880015598614,9.40850903678189));
#65402=CARTESIAN_POINT('Ctrl Pts',(-19.6267687797688,35.9619644071416,8.15559293383585));
#65403=CARTESIAN_POINT('Ctrl Pts',(-19.1129151695516,35.8359272544215,6.64121465399068));
#65404=CARTESIAN_POINT('Ctrl Pts',(-17.5618698412561,35.7098901017015,6.25179777628167));
#65405=CARTESIAN_POINT('Ctrl Pts',(-16.3936251655486,35.5838529489816,7.34385746899409));
#65406=CARTESIAN_POINT('Ctrl Pts',(-16.6777190612162,35.4578157962616,8.9176028151563));
#65407=CARTESIAN_POINT('Ctrl Pts',(-18.1540584911281,35.3317786435416,9.53226346517944));
#65408=CARTESIAN_POINT('Ctrl Pts',(-19.471050135726,35.2057414908216,8.6251036009875));
#65409=CARTESIAN_POINT('Ctrl Pts',(-19.4229666935522,35.0797043381016,7.02665363221171));
#65410=CARTESIAN_POINT('Ctrl Pts',(-18.0538527359272,34.9536671853816,6.2002681450112));
#65411=CARTESIAN_POINT('Ctrl Pts',(-16.6170945493887,34.8276300326616,6.90258420567117));
#65412=CARTESIAN_POINT('Ctrl Pts',(-16.4281487418217,34.7015928799416,8.49047690834462));
#65413=CARTESIAN_POINT('Ctrl Pts',(-17.6598093762981,34.5755557272216,9.51051625508399));
#65414=CARTESIAN_POINT('Ctrl Pts',(-19.1848544073993,34.4495185745016,9.02825816664846));
#65415=CARTESIAN_POINT('Ctrl Pts',(-19.6063538153946,34.3234814217816,7.48638804046807));
#65416=CARTESIAN_POINT('Ctrl Pts',(-18.5399022278055,34.1974442690615,6.29415834550658));
#65417=CARTESIAN_POINT('Ctrl Pts',(-16.9586559591529,34.071395908747,6.54781143533374));
#65418=CARTESIAN_POINT('Ctrl Pts',(-16.5316691371024,33.9873599326724,7.51933613284737));
#65419=CARTESIAN_POINT('Ctrl Pts',(-16.5709517952873,33.9453363408379,7.98805925999848));
#65420=CARTESIAN_POINT('Ctrl Pts',(-18.7079916422033,41.5491754829709,9.25003219459753));
#65421=CARTESIAN_POINT('Ctrl Pts',(-19.1669387919087,41.5071630987309,9.00792937228188));
#65422=CARTESIAN_POINT('Ctrl Pts',(-19.8162229296688,41.4231383302509,8.03368166911634));
#65423=CARTESIAN_POINT('Ctrl Pts',(-19.1123932777587,41.2971011775309,6.41291587346004));
#65424=CARTESIAN_POINT('Ctrl Pts',(-17.3701299623446,41.1710640248109,6.12991741636527));
#65425=CARTESIAN_POINT('Ctrl Pts',(-16.1870696686658,41.0450268720909,7.4381322882717));
#65426=CARTESIAN_POINT('Ctrl Pts',(-16.6450160912875,40.9189897193709,9.14264781598064));
#65427=CARTESIAN_POINT('Ctrl Pts',(-18.325368146149,40.7929525666509,9.68158136871029));
#65428=CARTESIAN_POINT('Ctrl Pts',(-19.6894233694515,40.6669154139309,8.56223244767046));
#65429=CARTESIAN_POINT('Ctrl Pts',(-19.488544466351,40.5408782612109,6.80902238783358));
#65430=CARTESIAN_POINT('Ctrl Pts',(-17.906554474218,40.4148411084909,6.02720399653423));
#65431=CARTESIAN_POINT('Ctrl Pts',(-16.3918183718805,40.2888039557709,6.93244887794637));
#65432=CARTESIAN_POINT('Ctrl Pts',(-16.3310669226111,40.1627668030509,8.69604349028723));
#65433=CARTESIAN_POINT('Ctrl Pts',(-17.7799290889218,40.0367296503309,9.7033818354433));
#65434=CARTESIAN_POINT('Ctrl Pts',(-19.4119558307657,39.9106924976109,9.03224972404705));
#65435=CARTESIAN_POINT('Ctrl Pts',(-19.7330176199543,39.784655344891,7.29706773910144));
#65436=CARTESIAN_POINT('Ctrl Pts',(-18.449178735851,39.6586181921709,6.08641031165167));
#65437=CARTESIAN_POINT('Ctrl Pts',(-16.7358035758118,39.5325810394509,6.50864157334445));
#65438=CARTESIAN_POINT('Ctrl Pts',(-16.1614990648281,39.4065438867309,8.177206495299));
#65439=CARTESIAN_POINT('Ctrl Pts',(-17.2520452792698,39.2805067340109,9.56452154229811));
#65440=CARTESIAN_POINT('Ctrl Pts',(-19.009039240403,39.1544695812909,9.40049000728872));
#65441=CARTESIAN_POINT('Ctrl Pts',(-19.8239404001145,39.028432428571,7.8352838465818));
#65442=CARTESIAN_POINT('Ctrl Pts',(-18.9507008716018,38.9023952758509,6.3018605892119));
#65443=CARTESIAN_POINT('Ctrl Pts',(-17.1887777264871,38.776358123131,6.20408021820285));
#65444=CARTESIAN_POINT('Ctrl Pts',(-16.1512242540963,38.6503209704109,7.63146137728754));
#65445=CARTESIAN_POINT('Ctrl Pts',(-16.7879281136981,38.524283817691,9.27722635685827));
#65446=CARTESIAN_POINT('Ctrl Pts',(-18.5159823471268,38.3982466649709,9.63466549992755));
#65447=CARTESIAN_POINT('Ctrl Pts',(-19.7533408921551,38.272209512251,8.37654070211551));
#65448=CARTESIAN_POINT('Ctrl Pts',(-19.3671931127862,38.146172359531,6.65467425339943));
#65449=CARTESIAN_POINT('Ctrl Pts',(-17.7110600748227,38.0201352068109,6.04544725498344));
#65450=CARTESIAN_POINT('Ctrl Pts',(-16.3011434700655,37.894098054091,7.10661140004615));
#65451=CARTESIAN_POINT('Ctrl Pts',(-16.4282320773269,37.768060901371,8.86666329158789));
#65452=CARTESIAN_POINT('Ctrl Pts',(-17.9759753637945,37.642023748651,9.71426278088));
#65453=CARTESIAN_POINT('Ctrl Pts',(-19.5274032336106,37.515986595931,8.87342644735645));
#65454=CARTESIAN_POINT('Ctrl Pts',(-19.6621723284219,37.389949443211,7.11394599386444));
#65455=CARTESIAN_POINT('Ctrl Pts',(-18.2569005738588,37.263912290491,6.0466384136139));
#65456=CARTESIAN_POINT('Ctrl Pts',(-16.5981243550872,37.137875137771,6.6486314623808));
#65457=CARTESIAN_POINT('Ctrl Pts',(-16.2044652147889,37.011837985051,8.36879618038998));
#65458=CARTESIAN_POINT('Ctrl Pts',(-17.4363209239151,36.885800832331,9.63230941204306));
#65459=CARTESIAN_POINT('Ctrl Pts',(-19.1659187317365,36.759763679611,9.28241571962643));
#65460=CARTESIAN_POINT('Ctrl Pts',(-19.8097994236285,36.633726526891,7.63944528897695));
#65461=CARTESIAN_POINT('Ctrl Pts',(-18.7784855978342,36.507689374171,6.20754935596669));
#65462=CARTESIAN_POINT('Ctrl Pts',(-17.0161524764798,36.381652221451,6.29763892127583));
#65463=CARTESIAN_POINT('Ctrl Pts',(-16.1362286768648,36.255615068731,7.82723636259333));
#65464=CARTESIAN_POINT('Ctrl Pts',(-16.9442907851535,36.129577916011,9.39598419226011));
#65465=CARTESIAN_POINT('Ctrl Pts',(-18.7005520827727,36.003540763291,9.56768259047058));
#65466=CARTESIAN_POINT('Ctrl Pts',(-19.797142844862,35.877503610571,8.18514026901571));
#65467=CARTESIAN_POINT('Ctrl Pts',(-19.2301261376084,35.751466457851,6.51408499432096));
#65468=CARTESIAN_POINT('Ctrl Pts',(-17.518610255722,35.625429305131,6.08437919609904));
#65469=CARTESIAN_POINT('Ctrl Pts',(-16.2294994348282,35.499392152411,7.28942296493543));
#65470=CARTESIAN_POINT('Ctrl Pts',(-16.5429855757627,35.373354999691,9.02598739981334));
#65471=CARTESIAN_POINT('Ctrl Pts',(-18.1720665157287,35.247317846971,9.70424060447069));
#65472=CARTESIAN_POINT('Ctrl Pts',(-19.6253136097501,35.121280694251,8.70322632935556));
#65473=CARTESIAN_POINT('Ctrl Pts',(-19.5722554731277,34.995243541531,6.93940134110259));
#65474=CARTESIAN_POINT('Ctrl Pts',(-18.0614935116043,34.869206388811,6.02751832898042));
#65475=CARTESIAN_POINT('Ctrl Pts',(-16.4760888752399,34.7431692360911,6.80249573937267));
#65476=CARTESIAN_POINT('Ctrl Pts',(-16.2675948070349,34.617132083371,8.55467121082956));
#65477=CARTESIAN_POINT('Ctrl Pts',(-17.6266825774209,34.491094930651,9.68024343637631));
#65478=CARTESIAN_POINT('Ctrl Pts',(-19.3095081813571,34.3650577779311,9.14809111144546));
#65479=CARTESIAN_POINT('Ctrl Pts',(-19.7746157561195,34.239020625211,7.44669969455893));
#65480=CARTESIAN_POINT('Ctrl Pts',(-18.597829497121,34.1129834724911,6.13112237353658));
#65481=CARTESIAN_POINT('Ctrl Pts',(-16.8529880971946,33.9869351121764,6.41101831455709));
#65482=CARTESIAN_POINT('Ctrl Pts',(-16.3818253826279,33.902899136102,7.48305658391363));
#65483=CARTESIAN_POINT('Ctrl Pts',(-16.4251722095321,33.8608755442674,8.00027362566716));
#65484=CARTESIAN_POINT('Ctrl Pts',(-18.7762476385807,41.4647146864003,9.37942306533622));
#65485=CARTESIAN_POINT('Ctrl Pts',(-19.2782253578306,41.4227023021603,9.11462084868009));
#65486=CARTESIAN_POINT('Ctrl Pts',(-19.9883859304091,41.3386775336803,8.04902834999368));
#65487=CARTESIAN_POINT('Ctrl Pts',(-19.2185656937367,41.2126403809603,6.27630066650286));
#65488=CARTESIAN_POINT('Ctrl Pts',(-17.3129489664818,41.0866032282403,5.96676846843845));
#65489=CARTESIAN_POINT('Ctrl Pts',(-16.0189657522113,40.9605660755203,7.39764066823327));
#65490=CARTESIAN_POINT('Ctrl Pts',(-16.5198489168936,40.8345289228003,9.26197040113339));
#65491=CARTESIAN_POINT('Ctrl Pts',(-18.357749626328,40.7084917700804,9.85143399361934));
#65492=CARTESIAN_POINT('Ctrl Pts',(-19.8496977305136,40.5824546173603,8.62713568652844));
#65493=CARTESIAN_POINT('Ctrl Pts',(-19.6299845594252,40.4564174646403,6.70954585561218));
#65494=CARTESIAN_POINT('Ctrl Pts',(-17.8996682721641,40.3303803119205,5.85442470890919));
#65495=CARTESIAN_POINT('Ctrl Pts',(-16.2429115532149,40.2043431592003,6.84454472866676));
#65496=CARTESIAN_POINT('Ctrl Pts',(-16.176464089787,40.0783060064804,8.7734927605975));
#65497=CARTESIAN_POINT('Ctrl Pts',(-17.7611705777108,39.9522688537603,9.87527845714036));
#65498=CARTESIAN_POINT('Ctrl Pts',(-19.5462150259696,39.8262317010404,9.14122145992317));
#65499=CARTESIAN_POINT('Ctrl Pts',(-19.8973793480026,39.7001945483203,7.24335000381806));
#65500=CARTESIAN_POINT('Ctrl Pts',(-18.4931686118854,39.5741573956004,5.91918216746824));
#65501=CARTESIAN_POINT('Ctrl Pts',(-16.6191485736127,39.4481202428803,6.3810015422626));
#65502=CARTESIAN_POINT('Ctrl Pts',(-15.99099766612,39.3220830901604,8.20600996530419));
#65503=CARTESIAN_POINT('Ctrl Pts',(-17.1837927446244,39.1960459374403,9.7233987182812));
#65504=CARTESIAN_POINT('Ctrl Pts',(-19.1055212528237,39.0700087847204,9.54398769920866));
#65505=CARTESIAN_POINT('Ctrl Pts',(-19.9968269855834,38.9439716320003,7.8320288838809));
#65506=CARTESIAN_POINT('Ctrl Pts',(-19.0417131186312,38.8179344792804,6.15483291507804));
#65507=CARTESIAN_POINT('Ctrl Pts',(-17.1145932695458,38.6918973265603,6.04788472364022));
#65508=CARTESIAN_POINT('Ctrl Pts',(-15.979759496191,38.5658601738404,7.60909615985389));
#65509=CARTESIAN_POINT('Ctrl Pts',(-16.6761602723712,38.4398230211204,9.40916693357315));
#65510=CARTESIAN_POINT('Ctrl Pts',(-18.5662356838727,38.3137858684004,9.80011932520205));
#65511=CARTESIAN_POINT('Ctrl Pts',(-19.9196081162464,38.1877487156804,8.42403361044614));
#65512=CARTESIAN_POINT('Ctrl Pts',(-19.4972553862961,38.0617115629604,6.54072614610208));
#65513=CARTESIAN_POINT('Ctrl Pts',(-17.6858444521501,37.9356744102404,5.87437844274086));
#65514=CARTESIAN_POINT('Ctrl Pts',(-16.1437350348827,37.8096372575204,7.03503660922119));
#65515=CARTESIAN_POINT('Ctrl Pts',(-16.2827393826746,37.6836001048004,8.96010975728389));
#65516=CARTESIAN_POINT('Ctrl Pts',(-17.9755980166681,37.5575629520803,9.88717959254801));
#65517=CARTESIAN_POINT('Ctrl Pts',(-19.6724866980142,37.4315257993604,8.96750702189228));
#65518=CARTESIAN_POINT('Ctrl Pts',(-19.8198916505935,37.3054886466404,7.0430588895184));
#65519=CARTESIAN_POINT('Ctrl Pts',(-18.2828625814843,37.1794514939204,5.87568128358639));
#65520=CARTESIAN_POINT('Ctrl Pts',(-16.4685606437131,37.0534143412004,6.53411678714783));
#65521=CARTESIAN_POINT('Ctrl Pts',(-16.0379922927914,36.9273771884804,8.41556296768266));
#65522=CARTESIAN_POINT('Ctrl Pts',(-17.3853459471484,36.8013400357604,9.79754233213571));
#65523=CARTESIAN_POINT('Ctrl Pts',(-19.2771096575173,36.6753028830404,9.41484284743033));
#65524=CARTESIAN_POINT('Ctrl Pts',(-19.9813601608543,36.5492657303204,7.61782863761985));
#65525=CARTESIAN_POINT('Ctrl Pts',(-18.8533510590753,36.4232285776004,6.05167912537815));
#65526=CARTESIAN_POINT('Ctrl Pts',(-16.9257827946596,36.2971914248804,6.15021542645577));
#65527=CARTESIAN_POINT('Ctrl Pts',(-15.9633579439374,36.1711542721604,7.82322687332076));
#65528=CARTESIAN_POINT('Ctrl Pts',(-16.84718340051,36.0451171194404,9.53905942205762));
#65529=CARTESIAN_POINT('Ctrl Pts',(-18.7681105511675,35.9190799667204,9.72685614415925));
#65530=CARTESIAN_POINT('Ctrl Pts',(-19.9675169099553,35.7930428140004,8.21468760419558));
#65531=CARTESIAN_POINT('Ctrl Pts',(-19.3473371056652,35.6670056612804,6.38695533465123));
#65532=CARTESIAN_POINT('Ctrl Pts',(-17.4753506701879,35.5409685085604,5.91696061591641));
#65533=CARTESIAN_POINT('Ctrl Pts',(-16.0653737041077,35.4149313558404,7.23498846087677));
#65534=CARTESIAN_POINT('Ctrl Pts',(-16.4082520903093,35.2888942031204,9.13437198447035));
#65535=CARTESIAN_POINT('Ctrl Pts',(-18.1900745403292,35.1628570504005,9.87621774376195));
#65536=CARTESIAN_POINT('Ctrl Pts',(-19.7795770837743,35.0368198976804,8.78134905772361));
#65537=CARTESIAN_POINT('Ctrl Pts',(-19.7215442527032,34.9107827449605,6.8521490499935));
#65538=CARTESIAN_POINT('Ctrl Pts',(-18.0691342872814,34.7847455922404,5.85476851294963));
#65539=CARTESIAN_POINT('Ctrl Pts',(-16.335083201091,34.6587084395204,6.70240727307417));
#65540=CARTESIAN_POINT('Ctrl Pts',(-16.1070408722481,34.5326712868005,8.61886551331448));
#65541=CARTESIAN_POINT('Ctrl Pts',(-17.5935557785435,34.4066341340805,9.84997061766864));
#65542=CARTESIAN_POINT('Ctrl Pts',(-19.4341619553151,34.2805969813605,9.26792405624247));
#65543=CARTESIAN_POINT('Ctrl Pts',(-19.9428776968442,34.1545598286405,7.40701134864978));
#65544=CARTESIAN_POINT('Ctrl Pts',(-18.6557567664365,34.0285226759205,5.96808640156658));
#65545=CARTESIAN_POINT('Ctrl Pts',(-16.7473202352362,33.902474315606,6.27422519378043));
#65546=CARTESIAN_POINT('Ctrl Pts',(-16.2319816281533,33.8184383395314,7.44677703497991));
#65547=CARTESIAN_POINT('Ctrl Pts',(-16.2793926237768,33.7764147476968,8.01248799133582));
#65548=CARTESIAN_POINT('Ctrl Pts',(-18.5338892852531,34.0285,6.25817448361128));
#65549=CARTESIAN_POINT('Ctrl Pts',(-18.5264711357089,34.0285,6.25568229473227));
#65550=CARTESIAN_POINT('Ctrl Pts',(-18.5190529861647,34.0285,6.25319010585325));
#65551=CARTESIAN_POINT('Ctrl Pts',(-18.5116348366204,34.0285,6.25069791697424));
#65552=CARTESIAN_POINT('Ctrl Pts',(-18.7711332099614,41.4659999999999,6.8735740585268));
#65553=CARTESIAN_POINT('Ctrl Pts',(-18.8150325114478,41.466,6.89761174551022));
#65554=CARTESIAN_POINT('Ctrl Pts',(-18.8572623534118,41.466,6.92446099914179));
#65555=CARTESIAN_POINT('Ctrl Pts',(-18.8977382984637,41.466,6.95381227460289));
#65556=CARTESIAN_POINT('Ctrl Pts',(-18.9281859213735,41.466,6.97589147660826));
#65557=CARTESIAN_POINT('Ctrl Pts',(-18.9576411714496,41.466,6.99938767928607));
#65558=CARTESIAN_POINT('Ctrl Pts',(-18.9860655235891,41.466,7.02418759153614));
#65559=CARTESIAN_POINT('Ctrl Pts',(-18.9960253921561,41.466,7.03287745948003));
#65560=CARTESIAN_POINT('Ctrl Pts',(-19.0058600905433,41.466,7.04172886589521));
#65561=CARTESIAN_POINT('Ctrl Pts',(-19.0155632740424,41.466,7.05073310140044));
#65562=CARTESIAN_POINT('Ctrl Pts',(-19.0545719021686,41.466,7.08693182673792));
#65563=CARTESIAN_POINT('Ctrl Pts',(-19.0913713554988,41.466,7.12551658131604));
#65564=CARTESIAN_POINT('Ctrl Pts',(-19.1258640554372,41.466,7.16616277809746));
#65565=CARTESIAN_POINT('Ctrl Pts',(-19.1505598681049,41.466,7.19526432315358));
#65566=CARTESIAN_POINT('Ctrl Pts',(-19.1740730954751,41.466,7.22542383308934));
#65567=CARTESIAN_POINT('Ctrl Pts',(-19.1963627498986,41.466,7.25653761332732));
#65568=CARTESIAN_POINT('Ctrl Pts',(-19.2034400634619,41.466,7.26641672471689));
#65569=CARTESIAN_POINT('Ctrl Pts',(-19.2103950492517,41.466,7.27639371368076));
#65570=CARTESIAN_POINT('Ctrl Pts',(-19.2172228745623,41.466,7.28646048298054));
#65571=CARTESIAN_POINT('Ctrl Pts',(-19.2487206908539,41.466,7.33290004984561));
#65572=CARTESIAN_POINT('Ctrl Pts',(-19.2774226769727,41.466,7.38110989018601));
#65573=CARTESIAN_POINT('Ctrl Pts',(-19.3032305569381,41.466,7.43074160061262));
#65574=CARTESIAN_POINT('Ctrl Pts',(-19.3290384369034,41.466,7.48037331103924));
#65575=CARTESIAN_POINT('Ctrl Pts',(-19.351952988103,41.466,7.53142771228986));
#65576=CARTESIAN_POINT('Ctrl Pts',(-19.3718527099145,41.466,7.58360345354479));
#65577=CARTESIAN_POINT('Ctrl Pts',(-19.3845995020632,41.466,7.61702469105144));
#65578=CARTESIAN_POINT('Ctrl Pts',(-19.3961087909219,41.466,7.65090693892874));
#65579=CARTESIAN_POINT('Ctrl Pts',(-19.4063413847352,41.466,7.68517870375625));
#65580=CARTESIAN_POINT('Ctrl Pts',(-19.4152961833237,41.466,7.71517078170846));
#65581=CARTESIAN_POINT('Ctrl Pts',(-19.4232731813879,41.466,7.74546129662054));
#65582=CARTESIAN_POINT('Ctrl Pts',(-19.4302416374854,41.466,7.77600509182718));
#65583=CARTESIAN_POINT('Ctrl Pts',(-19.4323739776039,41.466,7.78535146051786));
#65584=CARTESIAN_POINT('Ctrl Pts',(-19.4344110319851,41.466,7.7947182361204));
#65585=CARTESIAN_POINT('Ctrl Pts',(-19.4363504761414,41.466,7.80409571244044));
#65586=CARTESIAN_POINT('Ctrl Pts',(-19.4483033966471,41.466,7.86188970905142));
#65587=CARTESIAN_POINT('Ctrl Pts',(-19.4565726897916,41.466,7.92017862831491));
#65588=CARTESIAN_POINT('Ctrl Pts',(-19.4610359660074,41.466,7.97862520969174));
#65589=CARTESIAN_POINT('Ctrl Pts',(-19.4615949525186,41.466,7.98594513546783));
#65590=CARTESIAN_POINT('Ctrl Pts',(-19.4620941934996,41.466,7.99326758225861));
#65591=CARTESIAN_POINT('Ctrl Pts',(-19.4625334064251,41.466,8.0005919263415));
#65592=CARTESIAN_POINT('Ctrl Pts',(-19.4659158586079,41.466,8.05699792486926));
#65593=CARTESIAN_POINT('Ctrl Pts',(-19.4657422592885,41.466,8.11351490517321));
#65594=CARTESIAN_POINT('Ctrl Pts',(-19.4622098192675,41.466,8.1699133343397));
#65595=CARTESIAN_POINT('Ctrl Pts',(-19.4602920504131,41.466,8.20053215596072));
#65596=CARTESIAN_POINT('Ctrl Pts',(-19.4573834243698,41.466,8.23111637650103));
#65597=CARTESIAN_POINT('Ctrl Pts',(-19.4535094695855,41.466,8.26163092984805));
#65598=CARTESIAN_POINT('Ctrl Pts',(-19.4507014550128,41.466,8.28374923407363));
#65599=CARTESIAN_POINT('Ctrl Pts',(-19.4473861691094,41.466,8.30583095869765));
#65600=CARTESIAN_POINT('Ctrl Pts',(-19.4435719785325,41.466,8.32786291427628));
#65601=CARTESIAN_POINT('Ctrl Pts',(-19.4409779138594,41.466,8.34284704170591));
#65602=CARTESIAN_POINT('Ctrl Pts',(-19.4381517046733,41.466,8.3578139735458));
#65603=CARTESIAN_POINT('Ctrl Pts',(-19.4351029448282,41.466,8.37272646495416));
#65604=CARTESIAN_POINT('Ctrl Pts',(-19.423146378304,41.466,8.43120998107918));
#65605=CARTESIAN_POINT('Ctrl Pts',(-19.407760050003,41.466,8.48893384781506));
#65606=CARTESIAN_POINT('Ctrl Pts',(-19.3891801125346,41.466,8.54564278007359));
#65607=CARTESIAN_POINT('Ctrl Pts',(-19.3701830601375,41.466,8.60362481361556));
#65608=CARTESIAN_POINT('Ctrl Pts',(-19.3478473647113,41.466,8.66054673865175));
#65609=CARTESIAN_POINT('Ctrl Pts',(-19.322371280564,41.466,8.7161471563606));
#65610=CARTESIAN_POINT('Ctrl Pts',(-19.2966429325138,41.466,8.77229812878943));
#65611=CARTESIAN_POINT('Ctrl Pts',(-19.2677115047853,41.466,8.82710235142388));
#65612=CARTESIAN_POINT('Ctrl Pts',(-19.2357284380611,41.466,8.88028714355455));
#65613=CARTESIAN_POINT('Ctrl Pts',(-19.2296907577689,41.466,8.8903272305188));
#65614=CARTESIAN_POINT('Ctrl Pts',(-19.2235441817892,41.466,8.90030956924581));
#65615=CARTESIAN_POINT('Ctrl Pts',(-19.2172895300246,41.466,8.91023226242081));
#65616=CARTESIAN_POINT('Ctrl Pts',(-19.2108216298987,41.466,8.92049326348867));
#65617=CARTESIAN_POINT('Ctrl Pts',(-19.2042422248717,41.466,8.93068391788601));
#65618=CARTESIAN_POINT('Ctrl Pts',(-19.1975573996987,41.466,8.94079540529106));
#65619=CARTESIAN_POINT('Ctrl Pts',(-19.1621485581562,41.466,8.99435492944009));
#65620=CARTESIAN_POINT('Ctrl Pts',(-19.1237481043056,41.466,9.04575390697403));
#65621=CARTESIAN_POINT('Ctrl Pts',(-19.0825794977659,41.466,9.09471548562896));
#65622=CARTESIAN_POINT('Ctrl Pts',(-19.0413380622158,41.466,9.14376367939251));
#65623=CARTESIAN_POINT('Ctrl Pts',(-18.9973183329169,41.466,9.19036693480611));
#65624=CARTESIAN_POINT('Ctrl Pts',(-18.9506940483373,41.466,9.23423807965469));
#65625=CARTESIAN_POINT('Ctrl Pts',(-18.904483092379,41.466,9.27772030272191));
#65626=CARTESIAN_POINT('Ctrl Pts',(-18.8557131262279,41.466,9.31851969980534));
#65627=CARTESIAN_POINT('Ctrl Pts',(-18.8045092055452,41.466,9.35633200217432));
#65628=CARTESIAN_POINT('Ctrl Pts',(-18.7948293201577,41.466,9.36348025856348));
#65629=CARTESIAN_POINT('Ctrl Pts',(-18.7850623324094,41.466,9.37052166322747));
#65630=CARTESIAN_POINT('Ctrl Pts',(-18.7752089275578,41.466,9.3774540116144));
#65631=CARTESIAN_POINT('Origin',(-17.98,41.466,7.87));
#65632=CARTESIAN_POINT('',(-17.1642490230617,41.466,9.36643749592967));
#65633=CARTESIAN_POINT('',(-17.98,41.466,6.16566));
#65634=CARTESIAN_POINT('Origin',(-17.98,41.466,7.87));
#65635=CARTESIAN_POINT('Ctrl Pts',(-17.1642490230617,41.466,9.36643749592966));
#65636=CARTESIAN_POINT('Ctrl Pts',(-17.111789340126,41.466,9.32813761290297));
#65637=CARTESIAN_POINT('Ctrl Pts',(-17.0617472209979,41.466,9.28658023314859));
#65638=CARTESIAN_POINT('Ctrl Pts',(-17.0142916333355,41.466,9.24208960048121));
#65639=CARTESIAN_POINT('Ctrl Pts',(-16.9723635246812,41.466,9.20278109810107));
#65640=CARTESIAN_POINT('Ctrl Pts',(-16.9324549121243,41.466,9.16118180478115));
#65641=CARTESIAN_POINT('Ctrl Pts',(-16.8947136208791,41.466,9.11750245025616));
#65642=CARTESIAN_POINT('Ctrl Pts',(-16.8853938943848,41.466,9.10671639540251));
#65643=CARTESIAN_POINT('Ctrl Pts',(-16.8762127526669,41.466,9.09581071679169));
#65644=CARTESIAN_POINT('Ctrl Pts',(-16.8671731058919,41.466,9.0847902358313));
#65645=CARTESIAN_POINT('Ctrl Pts',(-16.8267762849462,41.466,9.03554136503217));
#65646=CARTESIAN_POINT('Ctrl Pts',(-16.7891936371374,41.466,8.98399208345677));
#65647=CARTESIAN_POINT('Ctrl Pts',(-16.754610798532,41.466,8.93044211916827));
#65648=CARTESIAN_POINT('Ctrl Pts',(-16.7315927675667,41.466,8.89479973740068));
#65649=CARTESIAN_POINT('Ctrl Pts',(-16.7099046708807,41.466,8.85827062428873));
#65650=CARTESIAN_POINT('Ctrl Pts',(-16.6896140741525,41.466,8.82094175216212));
#65651=CARTESIAN_POINT('Ctrl Pts',(-16.6821032533031,41.466,8.80712399831256));
#65652=CARTESIAN_POINT('Ctrl Pts',(-16.6747821860011,41.466,8.79319273006064));
#65653=CARTESIAN_POINT('Ctrl Pts',(-16.6676670453304,41.466,8.7791776958499));
#65654=CARTESIAN_POINT('Ctrl Pts',(-16.6397849483158,41.466,8.72425699060802));
#65655=CARTESIAN_POINT('Ctrl Pts',(-16.6150219263874,41.466,8.66798258419846));
#65656=CARTESIAN_POINT('Ctrl Pts',(-16.5935382103396,41.466,8.61063032490477));
#65657=CARTESIAN_POINT('Ctrl Pts',(-16.5726544678895,41.466,8.55487973644248));
#65658=CARTESIAN_POINT('Ctrl Pts',(-16.5548694058506,41.466,8.49810968578338));
#65659=CARTESIAN_POINT('Ctrl Pts',(-16.5403786854517,41.466,8.44057349599969));
#65660=CARTESIAN_POINT('Ctrl Pts',(-16.5315952966197,41.466,8.40569857516278));
#65661=CARTESIAN_POINT('Ctrl Pts',(-16.5240232072093,41.466,8.37054223600281));
#65662=CARTESIAN_POINT('Ctrl Pts',(-16.5177150916484,41.466,8.33516306780605));
#65663=CARTESIAN_POINT('Ctrl Pts',(-16.5124844857984,41.466,8.3058271302586));
#65664=CARTESIAN_POINT('Ctrl Pts',(-16.5081230458163,41.466,8.27633800030858));
#65665=CARTESIAN_POINT('Ctrl Pts',(-16.5046645357234,41.466,8.24673058741785));
#65666=CARTESIAN_POINT('Ctrl Pts',(-16.5031264715678,41.466,8.23356361687713));
#65667=CARTESIAN_POINT('Ctrl Pts',(-16.5017668817373,41.466,8.22037002113934));
#65668=CARTESIAN_POINT('Ctrl Pts',(-16.500590768404,41.466,8.20717809512951));
#65669=CARTESIAN_POINT('Ctrl Pts',(-16.4955380736504,41.466,8.15050432615207));
#65670=CARTESIAN_POINT('Ctrl Pts',(-16.4938551585946,41.466,8.09376815400606));
#65671=CARTESIAN_POINT('Ctrl Pts',(-16.4957110288904,41.466,8.03720028052094));
#65672=CARTESIAN_POINT('Ctrl Pts',(-16.4959467899537,41.466,8.03001416302452));
#65673=CARTESIAN_POINT('Ctrl Pts',(-16.4962397270978,41.466,8.02283077768763));
#65674=CARTESIAN_POINT('Ctrl Pts',(-16.4965902458921,41.466,8.01565061373279));
#65675=CARTESIAN_POINT('Ctrl Pts',(-16.499426906949,41.466,7.95754334016558));
#65676=CARTESIAN_POINT('Ctrl Pts',(-16.5060310991316,41.466,7.8996447512003));
#65677=CARTESIAN_POINT('Ctrl Pts',(-16.5162572633791,41.466,7.84225298758334));
#65678=CARTESIAN_POINT('Ctrl Pts',(-16.5251210845501,41.466,7.79250703034307));
#65679=CARTESIAN_POINT('Ctrl Pts',(-16.5367071997515,41.466,7.74314182037325));
#65680=CARTESIAN_POINT('Ctrl Pts',(-16.5509437230047,41.466,7.69437344281404));
#65681=CARTESIAN_POINT('Ctrl Pts',(-16.5537733871242,41.466,7.68468019638797));
#65682=CARTESIAN_POINT('Ctrl Pts',(-16.5567085247615,41.466,7.67500836402618));
#65683=CARTESIAN_POINT('Ctrl Pts',(-16.5597463211422,41.466,7.66536710704331));
#65684=CARTESIAN_POINT('Ctrl Pts',(-16.5766386373201,41.466,7.6117548365366));
#65685=CARTESIAN_POINT('Ctrl Pts',(-16.5966526679052,41.466,7.55923575103508));
#65686=CARTESIAN_POINT('Ctrl Pts',(-16.6196315985352,41.466,7.50807009544535));
#65687=CARTESIAN_POINT('Ctrl Pts',(-16.6424239719694,41.466,7.45731983434818));
#65688=CARTESIAN_POINT('Ctrl Pts',(-16.6681341614876,41.466,7.40790030018259));
#65689=CARTESIAN_POINT('Ctrl Pts',(-16.6966444927864,41.466,7.36010176185949));
#65690=CARTESIAN_POINT('Ctrl Pts',(-16.7244863815382,41.466,7.3134238901594));
#65691=CARTESIAN_POINT('Ctrl Pts',(-16.7549994631107,41.466,7.26829134122073));
#65692=CARTESIAN_POINT('Ctrl Pts',(-16.7880956091478,41.466,7.22501906714602));
#65693=CARTESIAN_POINT('Ctrl Pts',(-16.7942239191475,41.466,7.2170064752985));
#65694=CARTESIAN_POINT('Ctrl Pts',(-16.800440835444,41.466,7.20905780493933));
#65695=CARTESIAN_POINT('Ctrl Pts',(-16.8067458480612,41.466,7.201175251189));
#65696=CARTESIAN_POINT('Ctrl Pts',(-16.8135124330135,41.466,7.19271563773047));
#65697=CARTESIAN_POINT('Ctrl Pts',(-16.8203756788944,41.466,7.18433827145502));
#65698=CARTESIAN_POINT('Ctrl Pts',(-16.8273299671494,41.466,7.17605080146591));
#65699=CARTESIAN_POINT('Ctrl Pts',(-16.8612192200063,41.466,7.1356647611257));
#65700=CARTESIAN_POINT('Ctrl Pts',(-16.8973023839425,41.466,7.09736756612636));
#65701=CARTESIAN_POINT('Ctrl Pts',(-16.9354709299001,41.466,7.06141095674866));
#65702=CARTESIAN_POINT('Ctrl Pts',(-16.9728200232057,41.466,7.02622631125308));
#65703=CARTESIAN_POINT('Ctrl Pts',(-17.0121666768651,41.466,6.99328240785907));
#65704=CARTESIAN_POINT('Ctrl Pts',(-17.053425649955,41.466,6.96286170831185));
#65705=CARTESIAN_POINT('Ctrl Pts',(-17.0946846230449,41.466,6.93244100876463));
#65706=CARTESIAN_POINT('Ctrl Pts',(-17.1378565889557,41.466,6.90454300915782));
#65707=CARTESIAN_POINT('Ctrl Pts',(-17.1828623892565,41.466,6.87950438873575));
#65708=CARTESIAN_POINT('Ctrl Pts',(-17.1853034404496,41.466,6.87814632924464));
#65709=CARTESIAN_POINT('Ctrl Pts',(-17.187749886468,41.466,6.87679669586823));
#65710=CARTESIAN_POINT('Ctrl Pts',(-17.1902017145828,41.466,6.87545554732224));
#65711=CARTESIAN_POINT('Origin',(-17.98,41.466,7.87));
#65712=CARTESIAN_POINT('Ctrl Pts',(-16.919120712612,41.7180306875295,6.53336958898414));
#65713=CARTESIAN_POINT('Ctrl Pts',(-16.4744792903503,41.6760070959761,6.88626475233909));
#65714=CARTESIAN_POINT('Ctrl Pts',(-15.9731097926503,41.5919711201828,8.0647797895269));
#65715=CARTESIAN_POINT('Ctrl Pts',(-17.0570912447157,41.4659227601494,9.66491258748614));
#65716=CARTESIAN_POINT('Ctrl Pts',(-18.9869867646696,41.3398856074294,9.61721882671002));
#65717=CARTESIAN_POINT('Ctrl Pts',(-19.9944243161724,41.2138484547095,7.97209135863573));
#65718=CARTESIAN_POINT('Ctrl Pts',(-19.1579218343253,41.0878113019894,6.23241881161424));
#65719=CARTESIAN_POINT('Ctrl Pts',(-17.2428825517742,40.9617741492695,5.9925063653308));
#65720=CARTESIAN_POINT('Ctrl Pts',(-16.002750484554,40.8357369965494,7.47117978806733));
#65721=CARTESIAN_POINT('Ctrl Pts',(-16.5727688803051,40.7096998438294,9.31511334944695));
#65722=CARTESIAN_POINT('Ctrl Pts',(-18.4311354207765,40.5836626911095,9.83596614536317));
#65723=CARTESIAN_POINT('Ctrl Pts',(-19.8764752136172,40.4576255383895,8.55699758717004));
#65724=CARTESIAN_POINT('Ctrl Pts',(-19.5855828694099,40.3315883856694,6.64906030815352));
#65725=CARTESIAN_POINT('Ctrl Pts',(-17.8247655900277,40.2055512329495,5.85891088905231));
#65726=CARTESIAN_POINT('Ctrl Pts',(-16.2060676779772,40.0795140802294,6.90992356756758));
#65727=CARTESIAN_POINT('Ctrl Pts',(-16.2114169699092,39.9534769275095,8.83989534416103));
#65728=CARTESIAN_POINT('Ctrl Pts',(-17.8359170203282,39.8274397747895,9.88191984558327));
#65729=CARTESIAN_POINT('Ctrl Pts',(-19.5923259270914,39.7014026220695,9.08201784123309));
#65730=CARTESIAN_POINT('Ctrl Pts',(-19.8726389403143,39.5753654693495,7.17250451380341));
#65731=CARTESIAN_POINT('Ctrl Pts',(-18.4202273722028,39.4493283166295,5.90155345671652));
#65732=CARTESIAN_POINT('Ctrl Pts',(-16.564784501438,39.3232911639095,6.43272927708271));
#65733=CARTESIAN_POINT('Ctrl Pts',(-16.0049815753982,39.1972540111895,8.27973680401534));
#65734=CARTESIAN_POINT('Ctrl Pts',(-17.2533222079187,39.0712168584695,9.75162732564038));
#65735=CARTESIAN_POINT('Ctrl Pts',(-19.1669415762779,38.9451797057495,9.50087452448219));
#65736=CARTESIAN_POINT('Ctrl Pts',(-19.9939074072142,38.8191425530295,7.75704437735073));
#65737=CARTESIAN_POINT('Ctrl Pts',(-18.977126540798,38.6931054003095,6.11662591640547));
#65738=CARTESIAN_POINT('Ctrl Pts',(-17.047469164447,38.5670682475894,6.08143402191977));
#65739=CARTESIAN_POINT('Ctrl Pts',(-15.971550466053,38.4410310948696,7.68368712782179));
#65740=CARTESIAN_POINT('Ctrl Pts',(-16.7343817423075,38.3149939421494,9.45651100615227));
#65741=CARTESIAN_POINT('Ctrl Pts',(-18.6375854804388,38.1889567894296,9.77687266294394));
#65742=CARTESIAN_POINT('Ctrl Pts',(-19.9387649879574,38.0629196367095,8.35147870009828));
#65743=CARTESIAN_POINT('Ctrl Pts',(-19.4466810796223,37.9368824839895,6.48528752899183));
#65744=CARTESIAN_POINT('Ctrl Pts',(-17.6118401080523,37.8108453312696,5.88681057116351));
#65745=CARTESIAN_POINT('Ctrl Pts',(-16.1140521619751,37.6848081785495,7.10395778023238));
#65746=CARTESIAN_POINT('Ctrl Pts',(-16.3245528642827,37.5587710258296,9.0224221438397));
#65747=CARTESIAN_POINT('Ctrl Pts',(-18.0506273100736,37.4327338731095,9.885835757102));
#65748=CARTESIAN_POINT('Ctrl Pts',(-19.7120419461359,37.3066967203895,8.90373725558146));
#65749=CARTESIAN_POINT('Ctrl Pts',(-19.7877597397529,37.1806595676696,6.97524487118986));
#65750=CARTESIAN_POINT('Ctrl Pts',(-18.2084605066696,37.0546224149495,5.86590723461282));
#65751=CARTESIAN_POINT('Ctrl Pts',(-16.4200040391922,36.9285852622296,6.59133091857842));
#65752=CARTESIAN_POINT('Ctrl Pts',(-16.0597350780566,36.8025481095095,8.48738533320445));
#65753=CARTESIAN_POINT('Ctrl Pts',(-17.4574824475422,36.6765109567896,9.81821903631862));
#65754=CARTESIAN_POINT('Ctrl Pts',(-19.3335983859541,36.5504738040695,9.36544422685155));
#65755=CARTESIAN_POINT('Ctrl Pts',(-19.9704852863384,36.4244366513495,7.54357946878979));
#65756=CARTESIAN_POINT('Ctrl Pts',(-18.7850685961396,36.2983994986295,6.02055508638104));
#65757=CARTESIAN_POINT('Ctrl Pts',(-16.8626058508363,36.1723623459096,6.19071073752218));
#65758=CARTESIAN_POINT('Ctrl Pts',(-15.9631254208457,36.0463251931896,7.89826790759811));
#65759=CARTESIAN_POINT('Ctrl Pts',(-16.9101082626336,35.9202880404696,9.57994533257586));
#65760=CARTESIAN_POINT('Ctrl Pts',(-18.8365844605054,35.7942508877495,9.69615606533807));
#65761=CARTESIAN_POINT('Ctrl Pts',(-19.9788518580036,35.6682137350296,8.14050672632103));
#65762=CARTESIAN_POINT('Ctrl Pts',(-19.2911551757379,35.5421765823096,6.33720867716853));
#65763=CARTESIAN_POINT('Ctrl Pts',(-17.4030881947443,35.4161394295896,5.9371878387631));
#65764=CARTESIAN_POINT('Ctrl Pts',(-16.0431847714053,35.2901022768696,7.30667887406427));
#65765=CARTESIAN_POINT('Ctrl Pts',(-16.456456247779,35.1640651241495,9.19187763717425));
#65766=CARTESIAN_POINT('Ctrl Pts',(-18.2645297627139,35.0380279714296,9.86692133823987));
#65767=CARTESIAN_POINT('Ctrl Pts',(-19.8121404918094,34.9119908187095,8.71370280670959));
#65768=CARTESIAN_POINT('Ctrl Pts',(-19.6823612553971,34.7859536659897,6.78820027878308));
#65769=CARTESIAN_POINT('Ctrl Pts',(-17.9941617887159,34.6599165132695,5.85283083503748));
#65770=CARTESIAN_POINT('Ctrl Pts',(-16.2927908841274,34.5338793605497,6.76471570606888));
#65771=CARTESIAN_POINT('Ctrl Pts',(-16.1364825910008,34.4078422078296,8.68745919491244));
#65772=CARTESIAN_POINT('Ctrl Pts',(-17.6671032609381,34.2818050551096,9.86388249352386));
#65773=CARTESIAN_POINT('Ctrl Pts',(-19.4859215301242,34.1557679023896,9.2106775978793));
#65774=CARTESIAN_POINT('Ctrl Pts',(-19.7759329669726,34.0717431339096,7.96347022487569));
#65775=CARTESIAN_POINT('Ctrl Pts',(-19.6250757346175,34.0297307496696,7.41637949582761));
#65776=CARTESIAN_POINT('Ctrl Pts',(-17.0100469219083,41.6335880900653,6.64792997106398));
#65777=CARTESIAN_POINT('Ctrl Pts',(-16.6035149806241,41.5915644985119,6.97057907356705));
#65778=CARTESIAN_POINT('Ctrl Pts',(-16.1451170334339,41.5075285227186,8.04808553588302));
#65779=CARTESIAN_POINT('Ctrl Pts',(-17.1361922278737,41.3814801626852,9.51107359794373));
#65780=CARTESIAN_POINT('Ctrl Pts',(-18.9006795943709,41.2554430099652,9.46746759053033));
#65781=CARTESIAN_POINT('Ctrl Pts',(-19.8217713393811,41.1294058572452,7.96334127712032));
#65782=CARTESIAN_POINT('Ctrl Pts',(-19.0569641018898,41.0033687045251,6.37277318712605));
#65783=CARTESIAN_POINT('Ctrl Pts',(-17.306059669256,40.8773315518052,6.15342323985913));
#65784=CARTESIAN_POINT('Ctrl Pts',(-16.1722172706527,40.7512943990851,7.50536200888441));
#65785=CARTESIAN_POINT('Ctrl Pts',(-16.69338033237,40.6252572463652,9.1912550741175));
#65786=CARTESIAN_POINT('Ctrl Pts',(-18.3924693499255,40.4992200936452,9.6674664382544));
#65787=CARTESIAN_POINT('Ctrl Pts',(-19.7139314593479,40.3731829409252,8.49811616009379));
#65788=CARTESIAN_POINT('Ctrl Pts',(-19.4479710169003,40.2471457882052,6.75370503001651));
#65789=CARTESIAN_POINT('Ctrl Pts',(-17.8380704745879,40.1211086354852,6.03127801091937));
#65790=CARTESIAN_POINT('Ctrl Pts',(-16.3581084836628,39.9950714827652,6.992210130868));
#65791=CARTESIAN_POINT('Ctrl Pts',(-16.3629992966297,39.8690343300452,8.75676721817435));
#65792=CARTESIAN_POINT('Ctrl Pts',(-17.8482661342392,39.7429971773252,9.70948152282443));
#65793=CARTESIAN_POINT('Ctrl Pts',(-19.4541361382593,39.6169600246052,8.97813779643167));
#65794=CARTESIAN_POINT('Ctrl Pts',(-19.7104239866857,39.4909228718852,7.23228569844436));
#65795=CARTESIAN_POINT('Ctrl Pts',(-18.3824962121559,39.3648857191652,6.07026575462908));
#65796=CARTESIAN_POINT('Ctrl Pts',(-16.6860802814116,39.2388485664453,6.55591537386204));
#65797=CARTESIAN_POINT('Ctrl Pts',(-16.1742571383903,39.1128114137252,8.24461894014414));
#65798=CARTESIAN_POINT('Ctrl Pts',(-17.3156045597369,38.9867742610053,9.59035615929501));
#65799=CARTESIAN_POINT('Ctrl Pts',(-19.065210776676,38.8607371082852,9.3610949660424));
#65800=CARTESIAN_POINT('Ctrl Pts',(-19.8212987338348,38.7346999555652,7.766725616968));
#65801=CARTESIAN_POINT('Ctrl Pts',(-18.8916644739812,38.6086628028452,6.26690470947348));
#65802=CARTESIAN_POINT('Ctrl Pts',(-17.1273948401923,38.4826256501252,6.23472905406568));
#65803=CARTESIAN_POINT('Ctrl Pts',(-16.1436913541404,38.3565884974052,7.69965569598187));
#65804=CARTESIAN_POINT('Ctrl Pts',(-16.8411416232371,38.2305513446852,9.32053377150254));
#65805=CARTESIAN_POINT('Ctrl Pts',(-18.5812249163903,38.1045141919653,9.61343776048767));
#65806=CARTESIAN_POINT('Ctrl Pts',(-19.770882480141,37.9784770392452,8.31021195695673));
#65807=CARTESIAN_POINT('Ctrl Pts',(-19.3209742698072,37.8524398865252,6.60396894491806));
#65808=CARTESIAN_POINT('Ctrl Pts',(-17.6433944835478,37.7264027338052,6.05678645741582));
#65809=CARTESIAN_POINT('Ctrl Pts',(-16.2739794653669,37.6003655810852,7.16961399204876));
#65810=CARTESIAN_POINT('Ctrl Pts',(-16.4664385005945,37.4743284283653,8.9236499477057));
#65811=CARTESIAN_POINT('Ctrl Pts',(-18.0445739601269,37.3482912756453,9.71306180804281));
#65812=CARTESIAN_POINT('Ctrl Pts',(-19.5635914952915,37.2222541229252,8.81513734494529));
#65813=CARTESIAN_POINT('Ctrl Pts',(-19.6328196420356,37.0962169702053,7.05193285358171));
#65814=CARTESIAN_POINT('Ctrl Pts',(-18.1888795344588,36.9701798174852,6.03767471127206));
#65815=CARTESIAN_POINT('Ctrl Pts',(-16.5537087131546,36.8441426647653,6.70092353095212));
#65816=CARTESIAN_POINT('Ctrl Pts',(-16.2243178088843,36.7181055120452,8.43447025729455));
#65817=CARTESIAN_POINT('Ctrl Pts',(-17.5022665628516,36.5920683593253,9.65124040457685));
#65818=CARTESIAN_POINT('Ctrl Pts',(-19.217583706803,36.4660312066053,9.23727217525425));
#65819=CARTESIAN_POINT('Ctrl Pts',(-19.7998840842051,36.3399940538853,7.57155643270289));
#65820=CARTESIAN_POINT('Ctrl Pts',(-18.7160674981441,36.2139569011653,6.17906795141363));
#65821=CARTESIAN_POINT('Ctrl Pts',(-16.9583758554741,36.0879197484453,6.33463984308984));
#65822=CARTESIAN_POINT('Ctrl Pts',(-16.1359884056251,35.9618825957253,7.89584511198585));
#65823=CARTESIAN_POINT('Ctrl Pts',(-17.0018069141132,35.8358454430053,9.43338874593749));
#65824=CARTESIAN_POINT('Ctrl Pts',(-18.7631680229694,35.7098082902853,9.53963924897777));
#65825=CARTESIAN_POINT('Ctrl Pts',(-19.807533570849,35.5837711375653,8.11732204215769));
#65826=CARTESIAN_POINT('Ctrl Pts',(-19.1787782339442,35.4577339848453,6.4685816865996));
#65827=CARTESIAN_POINT('Ctrl Pts',(-17.4525343515067,35.3316968321253,6.10284597272071));
#65828=CARTESIAN_POINT('Ctrl Pts',(-16.209186001646,35.2056596794053,7.3549601961777));
#65829=CARTESIAN_POINT('Ctrl Pts',(-16.5870366632261,35.0796225266853,9.07858169094301));
#65830=CARTESIAN_POINT('Ctrl Pts',(-18.2401431872918,34.9535853739653,9.69576851274171));
#65831=CARTESIAN_POINT('Ctrl Pts',(-19.655110760153,34.8275482212453,8.64139043441735));
#65832=CARTESIAN_POINT('Ctrl Pts',(-19.5364546874716,34.7015110685253,6.88091954386572));
#65833=CARTESIAN_POINT('Ctrl Pts',(-17.9929480052251,34.5754739158053,6.02571906827927));
#65834=CARTESIAN_POINT('Ctrl Pts',(-16.437398787232,34.4494367630853,6.8594477950413));
#65835=CARTESIAN_POINT('Ctrl Pts',(-16.2944874194151,34.3233996103653,8.61739611918706));
#65836=CARTESIAN_POINT('Ctrl Pts',(-17.6939211229911,34.1973624576453,9.69299012238081));
#65837=CARTESIAN_POINT('Ctrl Pts',(-19.3568514861902,34.0713253049253,9.0957703381064));
#65838=CARTESIAN_POINT('Ctrl Pts',(-19.6220065223918,33.9873005364453,7.95545904647767));
#65839=CARTESIAN_POINT('Ctrl Pts',(-19.4840790139423,33.9452881522053,7.45525855906674));
#65840=CARTESIAN_POINT('Ctrl Pts',(-17.1009731312045,41.549145492601,6.76249035314384));
#65841=CARTESIAN_POINT('Ctrl Pts',(-16.7325506708981,41.5071219010477,7.05489339479501));
#65842=CARTESIAN_POINT('Ctrl Pts',(-16.3171242742175,41.4230859252543,8.03139128223913));
#65843=CARTESIAN_POINT('Ctrl Pts',(-17.2152932110317,41.2970375652208,9.35723460840133));
#65844=CARTESIAN_POINT('Ctrl Pts',(-18.8143724240723,41.1710004125009,9.31771635435063));
#65845=CARTESIAN_POINT('Ctrl Pts',(-19.6491183625899,41.0449632597809,7.95459119560491));
#65846=CARTESIAN_POINT('Ctrl Pts',(-18.9560063694543,40.9189261070609,6.51312756263786));
#65847=CARTESIAN_POINT('Ctrl Pts',(-17.3692367867377,40.7928889543409,6.31434011438746));
#65848=CARTESIAN_POINT('Ctrl Pts',(-16.3416840567515,40.6668518016209,7.53954422970151));
#65849=CARTESIAN_POINT('Ctrl Pts',(-16.813991784435,40.5408146489009,9.06739679878805));
#65850=CARTESIAN_POINT('Ctrl Pts',(-18.3538032790746,40.4147774961809,9.49896673114564));
#65851=CARTESIAN_POINT('Ctrl Pts',(-19.5513877050788,40.2887403434609,8.43923473301753));
#65852=CARTESIAN_POINT('Ctrl Pts',(-19.3103591643909,40.1627031907409,6.8583497518795));
#65853=CARTESIAN_POINT('Ctrl Pts',(-17.8513753591482,40.0366660380209,6.20364513278643));
#65854=CARTESIAN_POINT('Ctrl Pts',(-16.5101492893484,39.9106288853009,7.07449669416841));
#65855=CARTESIAN_POINT('Ctrl Pts',(-16.5145816233501,39.7845917325809,8.6736390921877));
#65856=CARTESIAN_POINT('Ctrl Pts',(-17.8606152481501,39.6585545798609,9.53704320006559));
#65857=CARTESIAN_POINT('Ctrl Pts',(-19.3159463494272,39.5325174271409,8.87425775163027));
#65858=CARTESIAN_POINT('Ctrl Pts',(-19.548209033057,39.406480274421,7.2920668830853));
#65859=CARTESIAN_POINT('Ctrl Pts',(-18.344765052109,39.2804431217009,6.23897805254165));
#65860=CARTESIAN_POINT('Ctrl Pts',(-16.8073760613852,39.154405968981,6.67910147064134));
#65861=CARTESIAN_POINT('Ctrl Pts',(-16.3435327013825,39.0283688162609,8.20950107627294));
#65862=CARTESIAN_POINT('Ctrl Pts',(-17.377886911555,38.902331663541,9.42908499294963));
#65863=CARTESIAN_POINT('Ctrl Pts',(-18.9634799770742,38.7762945108209,9.22131540760264));
#65864=CARTESIAN_POINT('Ctrl Pts',(-19.6486900604556,38.6502573581009,7.77640685658525));
#65865=CARTESIAN_POINT('Ctrl Pts',(-18.8062024071642,38.524220205381,6.4171835025415));
#65866=CARTESIAN_POINT('Ctrl Pts',(-17.2073205159376,38.3981830526609,6.38802408621161));
#65867=CARTESIAN_POINT('Ctrl Pts',(-16.3158322422279,38.272145899941,7.71562426414195));
#65868=CARTESIAN_POINT('Ctrl Pts',(-16.9479015041667,38.1461087472209,9.1845565368528));
#65869=CARTESIAN_POINT('Ctrl Pts',(-18.5248643523418,38.020071594501,9.45000285803138));
#65870=CARTESIAN_POINT('Ctrl Pts',(-19.6029999723246,37.894034441781,8.26894521381518));
#65871=CARTESIAN_POINT('Ctrl Pts',(-19.1952674599919,37.7679972890609,6.72265036084428));
#65872=CARTESIAN_POINT('Ctrl Pts',(-17.6749488590434,37.641960136341,6.22676234366814));
#65873=CARTESIAN_POINT('Ctrl Pts',(-16.4339067687587,37.5159229836209,7.23527020386514));
#65874=CARTESIAN_POINT('Ctrl Pts',(-16.6083241369064,37.389885830901,8.82487775157168));
#65875=CARTESIAN_POINT('Ctrl Pts',(-18.0385206101803,37.2638486781809,9.54028785898363));
#65876=CARTESIAN_POINT('Ctrl Pts',(-19.4151410444472,37.137811525461,8.72653743430914));
#65877=CARTESIAN_POINT('Ctrl Pts',(-19.4778795443183,37.011774372741,7.12862083597354));
#65878=CARTESIAN_POINT('Ctrl Pts',(-18.169298562248,36.885737220021,6.20944218793131));
#65879=CARTESIAN_POINT('Ctrl Pts',(-16.687413387117,36.7597000673009,6.81051614332581));
#65880=CARTESIAN_POINT('Ctrl Pts',(-16.388900539712,36.633662914581,8.38155518138464));
#65881=CARTESIAN_POINT('Ctrl Pts',(-17.547050678161,36.507625761861,9.48426177283507));
#65882=CARTESIAN_POINT('Ctrl Pts',(-19.101569027652,36.381588609141,9.10910012365699));
#65883=CARTESIAN_POINT('Ctrl Pts',(-19.6292828820718,36.255551456421,7.59953339661598));
#65884=CARTESIAN_POINT('Ctrl Pts',(-18.6470664001486,36.129514303701,6.33758081644621));
#65885=CARTESIAN_POINT('Ctrl Pts',(-17.0541458601119,36.003477150981,6.47856894865749));
#65886=CARTESIAN_POINT('Ctrl Pts',(-16.3088513904044,35.877439998261,7.89342231637359));
#65887=CARTESIAN_POINT('Ctrl Pts',(-17.0935055655928,35.751402845541,9.28683215929911));
#65888=CARTESIAN_POINT('Ctrl Pts',(-18.6897515854333,35.625365692821,9.38312243261748));
#65889=CARTESIAN_POINT('Ctrl Pts',(-19.6362152836945,35.499328540101,8.09413735799435));
#65890=CARTESIAN_POINT('Ctrl Pts',(-19.0664012921504,35.373291387381,6.59995469603067));
#65891=CARTESIAN_POINT('Ctrl Pts',(-17.5019805082691,35.247254234661,6.2685041066783));
#65892=CARTESIAN_POINT('Ctrl Pts',(-16.3751872318868,35.121217081941,7.40324151829113));
#65893=CARTESIAN_POINT('Ctrl Pts',(-16.7176170786733,34.995179929221,8.96528574471179));
#65894=CARTESIAN_POINT('Ctrl Pts',(-18.2157566118698,34.869142776501,9.52461568724354));
#65895=CARTESIAN_POINT('Ctrl Pts',(-19.4980810284966,34.7431056237811,8.56907806212513));
#65896=CARTESIAN_POINT('Ctrl Pts',(-19.390548119546,34.617068471061,6.97363880894833));
#65897=CARTESIAN_POINT('Ctrl Pts',(-17.9917342217342,34.4910313183411,6.19860730152107));
#65898=CARTESIAN_POINT('Ctrl Pts',(-16.5820066903367,34.3649941656211,6.95417988401373));
#65899=CARTESIAN_POINT('Ctrl Pts',(-16.4524922478294,34.238957012901,8.5473330434617));
#65900=CARTESIAN_POINT('Ctrl Pts',(-17.7207389850441,34.112919860181,9.52209775123777));
#65901=CARTESIAN_POINT('Ctrl Pts',(-19.2277814422563,33.9868827074611,8.98086307833352));
#65902=CARTESIAN_POINT('Ctrl Pts',(-19.4680800778111,33.9028579389811,7.94744786807967));
#65903=CARTESIAN_POINT('Ctrl Pts',(-19.3430822932671,33.8608455547411,7.49413762230587));
#65904=CARTESIAN_POINT('Ctrl Pts',(-17.1918993405008,41.4647028951367,6.87705073522368));
#65905=CARTESIAN_POINT('Ctrl Pts',(-16.8615863611721,41.4226793035834,7.13920771602296));
#65906=CARTESIAN_POINT('Ctrl Pts',(-16.4891315150011,41.33864332779,8.01469702859525));
#65907=CARTESIAN_POINT('Ctrl Pts',(-17.2943941941897,41.2125949677566,9.20339561885893));
#65908=CARTESIAN_POINT('Ctrl Pts',(-18.7280652537737,41.0865578150366,9.16796511817092));
#65909=CARTESIAN_POINT('Ctrl Pts',(-19.4764653857986,40.9605206623167,7.9458411140895));
#65910=CARTESIAN_POINT('Ctrl Pts',(-18.8550486370188,40.8344835095965,6.65348193814967));
#65911=CARTESIAN_POINT('Ctrl Pts',(-17.4324139042195,40.7084463568767,6.47525698891578));
#65912=CARTESIAN_POINT('Ctrl Pts',(-16.5111508428501,40.5824092041566,7.57372645051859));
#65913=CARTESIAN_POINT('Ctrl Pts',(-16.9346032365001,40.4563720514366,8.94353852345861));
#65914=CARTESIAN_POINT('Ctrl Pts',(-18.3151372082236,40.3303348987166,9.33046702403687));
#65915=CARTESIAN_POINT('Ctrl Pts',(-19.3888439508095,40.2042977459966,8.38035330594127));
#65916=CARTESIAN_POINT('Ctrl Pts',(-19.1727473118813,40.0782605932766,6.96299447374249));
#65917=CARTESIAN_POINT('Ctrl Pts',(-17.8646802437086,39.9522234405567,6.37601225465347));
#65918=CARTESIAN_POINT('Ctrl Pts',(-16.6621900950339,39.8261862878366,7.15678325746883));
#65919=CARTESIAN_POINT('Ctrl Pts',(-16.6661639500706,39.7001491351166,8.59051096620103));
#65920=CARTESIAN_POINT('Ctrl Pts',(-17.872964362061,39.5741119823967,9.36460487730674));
#65921=CARTESIAN_POINT('Ctrl Pts',(-19.1777565605952,39.4480748296766,8.77037770682886));
#65922=CARTESIAN_POINT('Ctrl Pts',(-19.3859940794283,39.3220376769567,7.35184806772624));
#65923=CARTESIAN_POINT('Ctrl Pts',(-18.3070338920621,39.1960005242366,6.40769035045421));
#65924=CARTESIAN_POINT('Ctrl Pts',(-16.9286718413587,39.0699633715167,6.80228756742067));
#65925=CARTESIAN_POINT('Ctrl Pts',(-16.5128082643746,38.9439262187966,8.17438321240174));
#65926=CARTESIAN_POINT('Ctrl Pts',(-17.4401692633733,38.8178890660767,9.26781382660424));
#65927=CARTESIAN_POINT('Ctrl Pts',(-18.8617491774723,38.6918519133567,9.08153584916288));
#65928=CARTESIAN_POINT('Ctrl Pts',(-19.4760813870762,38.5658147606367,7.78608809620251));
#65929=CARTESIAN_POINT('Ctrl Pts',(-18.7207403403473,38.4397776079167,6.56746229560953));
#65930=CARTESIAN_POINT('Ctrl Pts',(-17.2872461916829,38.3137404551967,6.54131911835751));
#65931=CARTESIAN_POINT('Ctrl Pts',(-16.4879731303155,38.1877033024767,7.73159283230202));
#65932=CARTESIAN_POINT('Ctrl Pts',(-17.0546613850961,38.0616661497567,9.04857930220307));
#65933=CARTESIAN_POINT('Ctrl Pts',(-18.4685037882934,37.9356289970366,9.28656795557511));
#65934=CARTESIAN_POINT('Ctrl Pts',(-19.4351174645082,37.8095918443167,8.22767847067363));
#65935=CARTESIAN_POINT('Ctrl Pts',(-19.0695606501767,37.6835546915967,6.8413317767705));
#65936=CARTESIAN_POINT('Ctrl Pts',(-17.706503234539,37.5575175388767,6.39673822992046));
#65937=CARTESIAN_POINT('Ctrl Pts',(-16.5938340721504,37.4314803861567,7.30092641568153));
#65938=CARTESIAN_POINT('Ctrl Pts',(-16.7502097732182,37.3054432334367,8.72610555543768));
#65939=CARTESIAN_POINT('Ctrl Pts',(-18.0324672602335,37.1794060807167,9.36751390992444));
#65940=CARTESIAN_POINT('Ctrl Pts',(-19.2666905936027,37.0533689279967,8.63793752367297));
#65941=CARTESIAN_POINT('Ctrl Pts',(-19.3229394466011,36.9273317752767,7.20530881836537));
#65942=CARTESIAN_POINT('Ctrl Pts',(-18.1497175900372,36.8012946225567,6.38120966459056));
#65943=CARTESIAN_POINT('Ctrl Pts',(-16.8211180610794,36.6752574698367,6.9201087556995));
#65944=CARTESIAN_POINT('Ctrl Pts',(-16.5534832705398,36.5492203171167,8.32864010547475));
#65945=CARTESIAN_POINT('Ctrl Pts',(-17.5918347934705,36.4231831643967,9.31728314109329));
#65946=CARTESIAN_POINT('Ctrl Pts',(-18.9855543485009,36.2971460116767,8.98092807205971));
#65947=CARTESIAN_POINT('Ctrl Pts',(-19.4586816799386,36.1711088589567,7.62751036052907));
#65948=CARTESIAN_POINT('Ctrl Pts',(-18.5780653021531,36.0450717062367,6.49609368147881));
#65949=CARTESIAN_POINT('Ctrl Pts',(-17.1499158647496,35.9190345535167,6.62249805422515));
#65950=CARTESIAN_POINT('Ctrl Pts',(-16.4817143751837,35.7929974007967,7.89099952076132));
#65951=CARTESIAN_POINT('Ctrl Pts',(-17.1852042170723,35.6669602480767,9.14027557266074));
#65952=CARTESIAN_POINT('Ctrl Pts',(-18.6163351478973,35.5409230953567,9.22660561625718));
#65953=CARTESIAN_POINT('Ctrl Pts',(-19.46489699654,35.4148859426367,8.07095267383102));
#65954=CARTESIAN_POINT('Ctrl Pts',(-18.9540243503566,35.2888487899167,6.73132770546173));
#65955=CARTESIAN_POINT('Ctrl Pts',(-17.5514266650314,35.1628116371968,6.43416224063591));
#65956=CARTESIAN_POINT('Ctrl Pts',(-16.5411884621276,35.0367744844767,7.45152284040454));
#65957=CARTESIAN_POINT('Ctrl Pts',(-16.8481974941205,34.9107373317568,8.85198979848058));
#65958=CARTESIAN_POINT('Ctrl Pts',(-18.1913700364478,34.7847001790368,9.35346286174535));
#65959=CARTESIAN_POINT('Ctrl Pts',(-19.3410512968401,34.6586630263167,8.49676568983289));
#65960=CARTESIAN_POINT('Ctrl Pts',(-19.2446415516205,34.5326258735968,7.06635807403095));
#65961=CARTESIAN_POINT('Ctrl Pts',(-17.9905204382435,34.4065887208768,6.37149553476286));
#65962=CARTESIAN_POINT('Ctrl Pts',(-16.7266145934414,34.2805515681568,7.04891197298617));
#65963=CARTESIAN_POINT('Ctrl Pts',(-16.6104970762435,34.1545144154369,8.47726996773631));
#65964=CARTESIAN_POINT('Ctrl Pts',(-17.7475568470971,34.0284772627168,9.35120538009473));
#65965=CARTESIAN_POINT('Ctrl Pts',(-19.0987113983223,33.9024401099968,8.86595581856062));
#65966=CARTESIAN_POINT('Ctrl Pts',(-19.3141536332304,33.8184153415168,7.93943668968165));
#65967=CARTESIAN_POINT('Ctrl Pts',(-19.2020855725918,33.7764029572768,7.533016685545));
#65968=CARTESIAN_POINT('Ctrl Pts',(-17.1849388579978,41.466,9.37753196187617));
#65969=CARTESIAN_POINT('Ctrl Pts',(-17.1780422463525,41.466,9.37383380656067));
#65970=CARTESIAN_POINT('Ctrl Pts',(-17.1711456347071,41.466,9.37013565124517));
#65971=CARTESIAN_POINT('Ctrl Pts',(-17.1642490230617,41.466,9.36643749592967));
#65972=CARTESIAN_POINT('Origin',(-17.98,41.466,7.87));
#65973=CARTESIAN_POINT('',(-17.98,41.616,6.01566));
#65974=CARTESIAN_POINT('Origin',(-17.98,41.616,7.87));
#65975=CARTESIAN_POINT('Origin',(-17.98,41.466,6.01566));
#65976=CARTESIAN_POINT('Origin',(-17.98,41.616,7.87));
#65977=CARTESIAN_POINT('',(-20.8502,41.616,7.87));
#65978=CARTESIAN_POINT('Origin',(-17.98,41.616,7.87));
#65979=CARTESIAN_POINT('Origin',(-17.98,33.8535,7.87));
#65980=CARTESIAN_POINT('',(-19.33434,33.6785,7.87));
#65981=CARTESIAN_POINT('',(-19.50934,33.8535,7.87));
#65982=CARTESIAN_POINT('Origin',(-17.98,33.6785,7.87));
#65983=CARTESIAN_POINT('Origin',(-17.98,33.6785,7.87));
#65984=CARTESIAN_POINT('Origin',(-14.830178752974,45.1212,7.47706978764225));
#65985=CARTESIAN_POINT('',(-15.1458469071313,42.216,7.41654185840086));
#65986=CARTESIAN_POINT('',(-15.1458469071313,44.8212,7.41654185840086));
#65987=CARTESIAN_POINT('',(-15.1458469071313,41.616,7.41654185840086));
#65988=CARTESIAN_POINT('',(-15.2715817176658,42.216,7.39243278178041));
#65989=CARTESIAN_POINT('',(-14.830178752974,42.216,7.47706978764225));
#65990=CARTESIAN_POINT('',(-15.2715817176658,44.9412,7.39243278178041));
#65991=CARTESIAN_POINT('',(-15.2715817176658,45.1212,7.39243278178041));
#65992=CARTESIAN_POINT('Ctrl Pts',(-15.1458469071312,44.8212,7.41654185840086));
#65993=CARTESIAN_POINT('Ctrl Pts',(-15.2100565813885,44.8826581248803,7.404229946132));
#65994=CARTESIAN_POINT('Ctrl Pts',(-15.2715817176658,44.9412,7.39243278178041));
#65995=CARTESIAN_POINT('Origin',(-15.2715817176658,45.1212,7.39243278178041));
#65996=CARTESIAN_POINT('',(-15.1616754338717,44.8212,7.32677382246615));
#65997=CARTESIAN_POINT('',(-15.1616754338717,42.216,7.32677382246615));
#65998=CARTESIAN_POINT('',(-15.1616754338717,41.616,7.32677382246615));
#65999=CARTESIAN_POINT('Ctrl Pts',(-15.2715817176658,44.9412,7.39243278178041));
#66000=CARTESIAN_POINT('Ctrl Pts',(-15.2178018689555,44.8826581248802,7.36030423756528));
#66001=CARTESIAN_POINT('Ctrl Pts',(-15.1616754338717,44.8212,7.32677382246614));
#66002=CARTESIAN_POINT('',(-15.2715817176658,42.216,7.39243278178041));
#66003=CARTESIAN_POINT('Origin',(-15.0647720895333,42.216,7.35596666447035));
#66004=CARTESIAN_POINT('Origin',(-17.98,42.216,7.87));
#66005=CARTESIAN_POINT('Origin',(-17.98,44.9712,7.87));
#66006=CARTESIAN_POINT('',(-20.7302,44.9412,7.87));
#66007=CARTESIAN_POINT('',(-20.8498381190176,44.8212,7.91557642629242));
#66008=CARTESIAN_POINT('Ctrl Pts',(-20.7302,44.9412,7.87));
#66009=CARTESIAN_POINT('Ctrl Pts',(-20.7887418751198,44.8826581248802,7.8923016667123));
#66010=CARTESIAN_POINT('Ctrl Pts',(-20.8498381190176,44.8212,7.91557642629242));
#66011=CARTESIAN_POINT('',(-20.8141530928687,44.8212,8.32345814159914));
#66012=CARTESIAN_POINT('Origin',(-17.98,44.8212,7.87));
#66013=CARTESIAN_POINT('',(-20.6884182823342,44.9412,8.34756721821959));
#66014=CARTESIAN_POINT('Ctrl Pts',(-20.8141530928687,44.8212,8.32345814159914));
#66015=CARTESIAN_POINT('Ctrl Pts',(-20.7499434186116,44.8826581248802,8.33577005386797));
#66016=CARTESIAN_POINT('Ctrl Pts',(-20.6884182823342,44.9412,8.34756721821959));
#66017=CARTESIAN_POINT('',(-20.7983245661282,44.8212,8.41322617753386));
#66018=CARTESIAN_POINT('Ctrl Pts',(-20.6884182823342,44.9412,8.34756721821959));
#66019=CARTESIAN_POINT('Ctrl Pts',(-20.7421981310449,44.8826581248798,8.37969576243495));
#66020=CARTESIAN_POINT('Ctrl Pts',(-20.7983245661282,44.8212,8.41322617753386));
#66021=CARTESIAN_POINT('',(-20.6923537591437,44.8212,8.80871461331909));
#66022=CARTESIAN_POINT('Origin',(-17.98,44.8212,7.87));
#66023=CARTESIAN_POINT('',(-20.5643426456854,44.9412,8.81062379817425));
#66024=CARTESIAN_POINT('Ctrl Pts',(-20.6923537591437,44.8212,8.80871461331909));
#66025=CARTESIAN_POINT('Ctrl Pts',(-20.6269816329882,44.8826581248798,8.80968958705249));
#66026=CARTESIAN_POINT('Ctrl Pts',(-20.5643426456854,44.9412,8.81062379817425));
#66027=CARTESIAN_POINT('',(-20.6611776474381,44.8212,8.89437027625664));
#66028=CARTESIAN_POINT('Ctrl Pts',(-20.5643426456854,44.9412,8.81062379817425));
#66029=CARTESIAN_POINT('Ctrl Pts',(-20.6117263944973,44.8826581248799,8.85160301033426));
#66030=CARTESIAN_POINT('Ctrl Pts',(-20.6611776474381,44.8212,8.89437027625664));
#66031=CARTESIAN_POINT('',(-20.4881409289644,44.8212,9.26544871652585));
#66032=CARTESIAN_POINT('Origin',(-17.98,44.8212,7.87));
#66033=CARTESIAN_POINT('',(-20.361743065488,44.9412,9.2451));
#66034=CARTESIAN_POINT('Ctrl Pts',(-20.4881409289644,44.8212,9.26544871652586));
#66035=CARTESIAN_POINT('Ctrl Pts',(-20.423592649883,44.8826581248802,9.25505712764031));
#66036=CARTESIAN_POINT('Ctrl Pts',(-20.361743065488,44.9412,9.2451));
#66037=CARTESIAN_POINT('',(-20.442564502672,44.8212,9.34438940249174));
#66038=CARTESIAN_POINT('Ctrl Pts',(-20.361743065488,44.9412,9.2451));
#66039=CARTESIAN_POINT('Ctrl Pts',(-20.4012909831707,44.8826581248803,9.29368474747942));
#66040=CARTESIAN_POINT('Ctrl Pts',(-20.442564502672,44.8212,9.34438940249174));
#66041=CARTESIAN_POINT('',(-20.207719505839,44.8212,9.67978281661211));
#66042=CARTESIAN_POINT('Origin',(-17.98,44.8212,7.87));
#66043=CARTESIAN_POINT('',(-20.0867754274658,44.9412,9.63779448415992));
#66044=CARTESIAN_POINT('Ctrl Pts',(-20.207719505839,44.8212,9.67978281661211));
#66045=CARTESIAN_POINT('Ctrl Pts',(-20.1459563406293,44.8826581248801,9.65834040827754));
#66046=CARTESIAN_POINT('Ctrl Pts',(-20.0867754274658,44.9412,9.63779448415992));
#66047=CARTESIAN_POINT('',(-20.1491275816099,44.8212,9.74960995280916));
#66048=CARTESIAN_POINT('Ctrl Pts',(-20.0867754274658,44.9412,9.63779448415992));
#66049=CARTESIAN_POINT('Ctrl Pts',(-20.1172858705533,44.8826581248798,9.69250854399236));
#66050=CARTESIAN_POINT('Ctrl Pts',(-20.1491275816099,44.8212,9.74960995280916));
#66051=CARTESIAN_POINT('',(-19.8596099528092,44.8212,10.0391275816099));
#66052=CARTESIAN_POINT('Origin',(-17.98,44.8212,7.87));
#66053=CARTESIAN_POINT('',(-19.7477944841599,44.9412,9.97677542746581));
#66054=CARTESIAN_POINT('Ctrl Pts',(-19.8596099528092,44.8212,10.0391275816099));
#66055=CARTESIAN_POINT('Ctrl Pts',(-19.8025085439922,44.88265812488,10.0072858705532));
#66056=CARTESIAN_POINT('Ctrl Pts',(-19.7477944841599,44.9412,9.97677542746581));
#66057=CARTESIAN_POINT('',(-19.7897828166121,44.8212,10.097719505839));
#66058=CARTESIAN_POINT('Ctrl Pts',(-19.7477944841599,44.9412,9.97677542746581));
#66059=CARTESIAN_POINT('Ctrl Pts',(-19.7683404082775,44.88265812488,10.0359563406293));
#66060=CARTESIAN_POINT('Ctrl Pts',(-19.7897828166121,44.8212,10.097719505839));
#66061=CARTESIAN_POINT('',(-19.4543894024917,44.8212,10.332564502672));
#66062=CARTESIAN_POINT('Origin',(-17.98,44.8212,7.87));
#66063=CARTESIAN_POINT('',(-19.3551,44.9412,10.251743065488));
#66064=CARTESIAN_POINT('Ctrl Pts',(-19.4543894024917,44.8212,10.332564502672));
#66065=CARTESIAN_POINT('Ctrl Pts',(-19.4036847474795,44.8826581248802,10.2912909831707));
#66066=CARTESIAN_POINT('Ctrl Pts',(-19.3551,44.9412,10.251743065488));
#66067=CARTESIAN_POINT('',(-19.3754487165258,44.8212,10.3781409289644));
#66068=CARTESIAN_POINT('Ctrl Pts',(-19.3551,44.9412,10.251743065488));
#66069=CARTESIAN_POINT('Ctrl Pts',(-19.3650571276404,44.8826581248798,10.3135926498835));
#66070=CARTESIAN_POINT('Ctrl Pts',(-19.3754487165258,44.8212,10.3781409289644));
#66071=CARTESIAN_POINT('',(-19.0043702762566,44.8212,10.5511776474381));
#66072=CARTESIAN_POINT('Origin',(-17.98,44.8212,7.87));
#66073=CARTESIAN_POINT('',(-18.9206237981742,44.9412,10.4543426456854));
#66074=CARTESIAN_POINT('Ctrl Pts',(-19.0043702762566,44.8212,10.5511776474381));
#66075=CARTESIAN_POINT('Ctrl Pts',(-18.9616030103341,44.8826581248802,10.5017263944971));
#66076=CARTESIAN_POINT('Ctrl Pts',(-18.9206237981742,44.9412,10.4543426456854));
#66077=CARTESIAN_POINT('',(-18.9187146133191,44.8212,10.5823537591437));
#66078=CARTESIAN_POINT('Ctrl Pts',(-18.9206237981743,44.9412,10.4543426456854));
#66079=CARTESIAN_POINT('Ctrl Pts',(-18.9196895870525,44.8826581248799,10.5169816329881));
#66080=CARTESIAN_POINT('Ctrl Pts',(-18.9187146133191,44.8212,10.5823537591437));
#66081=CARTESIAN_POINT('',(-18.5232261775339,44.8212,10.6883245661282));
#66082=CARTESIAN_POINT('Origin',(-17.98,44.8212,7.87));
#66083=CARTESIAN_POINT('',(-18.4575672182196,44.9412,10.5784182823342));
#66084=CARTESIAN_POINT('Ctrl Pts',(-18.5232261775339,44.8212,10.6883245661282));
#66085=CARTESIAN_POINT('Ctrl Pts',(-18.4896957624347,44.8826581248802,10.6321981310445));
#66086=CARTESIAN_POINT('Ctrl Pts',(-18.4575672182196,44.9412,10.5784182823342));
#66087=CARTESIAN_POINT('',(-18.4334581415991,44.8212,10.7041530928687));
#66088=CARTESIAN_POINT('Ctrl Pts',(-18.4575672182196,44.9412,10.5784182823342));
#66089=CARTESIAN_POINT('Ctrl Pts',(-18.4457700538679,44.8826581248799,10.6399434186118));
#66090=CARTESIAN_POINT('Ctrl Pts',(-18.4334581415991,44.8212,10.7041530928687));
#66091=CARTESIAN_POINT('',(-18.0255764262924,44.8212,10.7398381190176));
#66092=CARTESIAN_POINT('Origin',(-17.98,44.8212,7.87));
#66093=CARTESIAN_POINT('',(-17.98,44.9412,10.6202));
#66094=CARTESIAN_POINT('Ctrl Pts',(-18.0255764262924,44.8212,10.7398381190176));
#66095=CARTESIAN_POINT('Ctrl Pts',(-18.0023016667124,44.88265812488,10.67874187512));
#66096=CARTESIAN_POINT('Ctrl Pts',(-17.98,44.9412,10.6202));
#66097=CARTESIAN_POINT('',(-17.9344235737076,44.8212,10.7398381190176));
#66098=CARTESIAN_POINT('Ctrl Pts',(-17.98,44.9412,10.6202));
#66099=CARTESIAN_POINT('Ctrl Pts',(-17.9576983332875,44.8826581248798,10.6787418751202));
#66100=CARTESIAN_POINT('Ctrl Pts',(-17.9344235737076,44.8212,10.7398381190176));
#66101=CARTESIAN_POINT('',(-17.5265418584009,44.8212,10.7041530928687));
#66102=CARTESIAN_POINT('Origin',(-17.98,44.8212,7.87));
#66103=CARTESIAN_POINT('',(-17.5024327817804,44.9412,10.5784182823342));
#66104=CARTESIAN_POINT('Ctrl Pts',(-17.5265418584009,44.8212,10.7041530928687));
#66105=CARTESIAN_POINT('Ctrl Pts',(-17.5142299461321,44.88265812488,10.6399434186118));
#66106=CARTESIAN_POINT('Ctrl Pts',(-17.5024327817804,44.9412,10.5784182823342));
#66107=CARTESIAN_POINT('',(-17.4367738224661,44.8212,10.6883245661282));
#66108=CARTESIAN_POINT('Ctrl Pts',(-17.5024327817804,44.9412,10.5784182823342));
#66109=CARTESIAN_POINT('Ctrl Pts',(-17.4703042375651,44.8826581248799,10.6321981310448));
#66110=CARTESIAN_POINT('Ctrl Pts',(-17.4367738224661,44.8212,10.6883245661282));
#66111=CARTESIAN_POINT('',(-17.0412853866809,44.8212,10.5823537591437));
#66112=CARTESIAN_POINT('Origin',(-17.98,44.8212,7.87));
#66113=CARTESIAN_POINT('',(-17.0393762018257,44.9412,10.4543426456854));
#66114=CARTESIAN_POINT('Ctrl Pts',(-17.0412853866809,44.8212,10.5823537591437));
#66115=CARTESIAN_POINT('Ctrl Pts',(-17.0403104129475,44.8826581248804,10.5169816329876));
#66116=CARTESIAN_POINT('Ctrl Pts',(-17.0393762018257,44.9412,10.4543426456854));
#66117=CARTESIAN_POINT('',(-16.9556297237434,44.8212,10.5511776474381));
#66118=CARTESIAN_POINT('Ctrl Pts',(-17.0393762018257,44.9412,10.4543426456854));
#66119=CARTESIAN_POINT('Ctrl Pts',(-16.9983969896657,44.8826581248799,10.5017263944974));
#66120=CARTESIAN_POINT('Ctrl Pts',(-16.9556297237434,44.8212,10.5511776474381));
#66121=CARTESIAN_POINT('',(-16.5845512834741,44.8212,10.3781409289644));
#66122=CARTESIAN_POINT('Origin',(-17.98,44.8212,7.87));
#66123=CARTESIAN_POINT('',(-16.6049,44.9412,10.251743065488));
#66124=CARTESIAN_POINT('Ctrl Pts',(-16.5845512834741,44.8212,10.3781409289644));
#66125=CARTESIAN_POINT('Ctrl Pts',(-16.5949428723596,44.8826581248797,10.3135926498836));
#66126=CARTESIAN_POINT('Ctrl Pts',(-16.6049,44.9412,10.251743065488));
#66127=CARTESIAN_POINT('',(-16.5056105975083,44.8212,10.332564502672));
#66128=CARTESIAN_POINT('Ctrl Pts',(-16.6049,44.9412,10.251743065488));
#66129=CARTESIAN_POINT('Ctrl Pts',(-16.5563152525203,44.88265812488,10.2912909831709));
#66130=CARTESIAN_POINT('Ctrl Pts',(-16.5056105975083,44.8212,10.332564502672));
#66131=CARTESIAN_POINT('',(-16.1702171833879,44.8212,10.097719505839));
#66132=CARTESIAN_POINT('Origin',(-17.98,44.8212,7.87));
#66133=CARTESIAN_POINT('',(-16.2122055158401,44.9412,9.97677542746581));
#66134=CARTESIAN_POINT('Ctrl Pts',(-16.1702171833879,44.8212,10.097719505839));
#66135=CARTESIAN_POINT('Ctrl Pts',(-16.1916595917225,44.8826581248802,10.0359563406291));
#66136=CARTESIAN_POINT('Ctrl Pts',(-16.2122055158401,44.9412,9.97677542746581));
#66137=CARTESIAN_POINT('',(-16.1003900471908,44.8212,10.0391275816099));
#66138=CARTESIAN_POINT('Ctrl Pts',(-16.2122055158401,44.9412,9.97677542746581));
#66139=CARTESIAN_POINT('Ctrl Pts',(-16.1574914560079,44.8826581248801,10.0072858705531));
#66140=CARTESIAN_POINT('Ctrl Pts',(-16.1003900471908,44.8212,10.0391275816099));
#66141=CARTESIAN_POINT('',(-15.8108724183901,44.8212,9.74960995280916));
#66142=CARTESIAN_POINT('Origin',(-17.98,44.8212,7.87));
#66143=CARTESIAN_POINT('',(-15.8732245725342,44.9412,9.63779448415992));
#66144=CARTESIAN_POINT('Ctrl Pts',(-15.8108724183901,44.8212,9.74960995280916));
#66145=CARTESIAN_POINT('Ctrl Pts',(-15.8427141294468,44.88265812488,9.69250854399223));
#66146=CARTESIAN_POINT('Ctrl Pts',(-15.8732245725342,44.9412,9.63779448415992));
#66147=CARTESIAN_POINT('',(-15.752280494161,44.8212,9.67978281661211));
#66148=CARTESIAN_POINT('Ctrl Pts',(-15.8732245725342,44.9412,9.63779448415992));
#66149=CARTESIAN_POINT('Ctrl Pts',(-15.8140436593705,44.8826581248799,9.65834040827761));
#66150=CARTESIAN_POINT('Ctrl Pts',(-15.752280494161,44.8212,9.67978281661211));
#66151=CARTESIAN_POINT('',(-15.517435497328,44.8212,9.34438940249174));
#66152=CARTESIAN_POINT('Origin',(-17.98,44.8212,7.87));
#66153=CARTESIAN_POINT('',(-15.598256934512,44.9412,9.2451));
#66154=CARTESIAN_POINT('Ctrl Pts',(-15.517435497328,44.8212,9.34438940249174));
#66155=CARTESIAN_POINT('Ctrl Pts',(-15.5587090168291,44.88265812488,9.29368474747968));
#66156=CARTESIAN_POINT('Ctrl Pts',(-15.598256934512,44.9412,9.2451));
#66157=CARTESIAN_POINT('',(-15.4718590710356,44.8212,9.26544871652585));
#66158=CARTESIAN_POINT('Ctrl Pts',(-15.598256934512,44.9412,9.2451));
#66159=CARTESIAN_POINT('Ctrl Pts',(-15.5364073501168,44.8826581248801,9.25505712764034));
#66160=CARTESIAN_POINT('Ctrl Pts',(-15.4718590710356,44.8212,9.26544871652585));
#66161=CARTESIAN_POINT('',(-15.2988223525619,44.8212,8.89437027625664));
#66162=CARTESIAN_POINT('Origin',(-17.98,44.8212,7.87));
#66163=CARTESIAN_POINT('',(-15.3956573543146,44.9412,8.81062379817425));
#66164=CARTESIAN_POINT('Ctrl Pts',(-15.2988223525619,44.8212,8.89437027625664));
#66165=CARTESIAN_POINT('Ctrl Pts',(-15.3482736055027,44.88265812488,8.85160301033418));
#66166=CARTESIAN_POINT('Ctrl Pts',(-15.3956573543146,44.9412,8.81062379817426));
#66167=CARTESIAN_POINT('',(-15.2676462408563,44.8212,8.80871461331909));
#66168=CARTESIAN_POINT('Ctrl Pts',(-15.3956573543146,44.9412,8.81062379817425));
#66169=CARTESIAN_POINT('Ctrl Pts',(-15.3330183670121,44.8826581248801,8.8096895870525));
#66170=CARTESIAN_POINT('Ctrl Pts',(-15.2676462408562,44.8212,8.80871461331909));
#66171=CARTESIAN_POINT('',(-15.1616754338717,44.8212,8.41322617753385));
#66172=CARTESIAN_POINT('Origin',(-17.98,44.8212,7.87));
#66173=CARTESIAN_POINT('',(-15.2715817176658,44.9412,8.34756721821959));
#66174=CARTESIAN_POINT('Ctrl Pts',(-15.1616754338717,44.8212,8.41322617753386));
#66175=CARTESIAN_POINT('Ctrl Pts',(-15.2178018689556,44.8826581248803,8.37969576243469));
#66176=CARTESIAN_POINT('Ctrl Pts',(-15.2715817176658,44.9412,8.34756721821959));
#66177=CARTESIAN_POINT('',(-15.1458469071313,44.8212,8.32345814159913));
#66178=CARTESIAN_POINT('Ctrl Pts',(-15.2715817176658,44.9412,8.34756721821959));
#66179=CARTESIAN_POINT('Ctrl Pts',(-15.2100565813884,44.8826581248802,8.33577005386797));
#66180=CARTESIAN_POINT('Ctrl Pts',(-15.1458469071312,44.8212,8.32345814159913));
#66181=CARTESIAN_POINT('',(-15.1101618809824,44.8212,7.91557642629241));
#66182=CARTESIAN_POINT('Origin',(-17.98,44.8212,7.87));
#66183=CARTESIAN_POINT('',(-15.2298,44.9412,7.87));
#66184=CARTESIAN_POINT('Ctrl Pts',(-15.1101618809824,44.8212,7.91557642629241));
#66185=CARTESIAN_POINT('Ctrl Pts',(-15.1712581248802,44.8826581248802,7.89230166671231));
#66186=CARTESIAN_POINT('Ctrl Pts',(-15.2298,44.9412,7.87));
#66187=CARTESIAN_POINT('',(-15.1101618809824,44.8212,7.82442357370758));
#66188=CARTESIAN_POINT('Ctrl Pts',(-15.2298,44.9412,7.87));
#66189=CARTESIAN_POINT('Ctrl Pts',(-15.1712581248802,44.8826581248802,7.8476983332877));
#66190=CARTESIAN_POINT('Ctrl Pts',(-15.1101618809824,44.8212,7.82442357370758));
#66191=CARTESIAN_POINT('Origin',(-17.98,44.8212,7.87));
#66192=CARTESIAN_POINT('',(-15.2676462408563,44.8212,6.93128538668091));
#66193=CARTESIAN_POINT('Origin',(-17.98,44.8212,7.87));
#66194=CARTESIAN_POINT('',(-15.3956573543146,44.9412,6.92937620182574));
#66195=CARTESIAN_POINT('Ctrl Pts',(-15.2676462408562,44.8212,6.93128538668091));
#66196=CARTESIAN_POINT('Ctrl Pts',(-15.3330183670122,44.8826581248802,6.93031041294749));
#66197=CARTESIAN_POINT('Ctrl Pts',(-15.3956573543146,44.9412,6.92937620182574));
#66198=CARTESIAN_POINT('',(-15.2988223525619,44.8212,6.84562972374336));
#66199=CARTESIAN_POINT('Ctrl Pts',(-15.3956573543146,44.9412,6.92937620182574));
#66200=CARTESIAN_POINT('Ctrl Pts',(-15.3482736055027,44.8826581248799,6.88839698966574));
#66201=CARTESIAN_POINT('Ctrl Pts',(-15.2988223525619,44.8212,6.84562972374336));
#66202=CARTESIAN_POINT('',(-15.4718590710356,44.8212,6.47455128347414));
#66203=CARTESIAN_POINT('Origin',(-17.98,44.8212,7.87));
#66204=CARTESIAN_POINT('',(-15.598256934512,44.9412,6.4949));
#66205=CARTESIAN_POINT('Ctrl Pts',(-15.4718590710356,44.8212,6.47455128347414));
#66206=CARTESIAN_POINT('Ctrl Pts',(-15.5364073501167,44.88265812488,6.48494287235965));
#66207=CARTESIAN_POINT('Ctrl Pts',(-15.598256934512,44.9412,6.4949));
#66208=CARTESIAN_POINT('',(-15.517435497328,44.8212,6.39561059750826));
#66209=CARTESIAN_POINT('Ctrl Pts',(-15.598256934512,44.9412,6.4949));
#66210=CARTESIAN_POINT('Ctrl Pts',(-15.5587090168292,44.8826581248801,6.44631525252043));
#66211=CARTESIAN_POINT('Ctrl Pts',(-15.517435497328,44.8212,6.39561059750826));
#66212=CARTESIAN_POINT('',(-15.752280494161,44.8212,6.0602171833879));
#66213=CARTESIAN_POINT('Origin',(-17.98,44.8212,7.87));
#66214=CARTESIAN_POINT('',(-15.8732245725342,44.9412,6.10220551584008));
#66215=CARTESIAN_POINT('Ctrl Pts',(-15.752280494161,44.8212,6.06021718338789));
#66216=CARTESIAN_POINT('Ctrl Pts',(-15.8140436593704,44.8826581248798,6.08165959172236));
#66217=CARTESIAN_POINT('Ctrl Pts',(-15.8732245725342,44.9412,6.10220551584008));
#66218=CARTESIAN_POINT('',(-15.8108724183901,44.8212,5.99039004719084));
#66219=CARTESIAN_POINT('Ctrl Pts',(-15.8732245725342,44.9412,6.10220551584008));
#66220=CARTESIAN_POINT('Ctrl Pts',(-15.8427141294467,44.8826581248798,6.04749145600765));
#66221=CARTESIAN_POINT('Ctrl Pts',(-15.8108724183901,44.8212,5.99039004719084));
#66222=CARTESIAN_POINT('',(-16.1003900471908,44.8212,5.70087241839011));
#66223=CARTESIAN_POINT('Origin',(-17.98,44.8212,7.87));
#66224=CARTESIAN_POINT('',(-16.2122055158401,44.9412,5.76322457253418));
#66225=CARTESIAN_POINT('Ctrl Pts',(-16.1003900471908,44.8212,5.70087241839011));
#66226=CARTESIAN_POINT('Ctrl Pts',(-16.1574914560079,44.8826581248801,5.73271412944688));
#66227=CARTESIAN_POINT('Ctrl Pts',(-16.2122055158401,44.9412,5.76322457253418));
#66228=CARTESIAN_POINT('',(-16.1702171833879,44.8212,5.642280494161));
#66229=CARTESIAN_POINT('Ctrl Pts',(-16.2122055158401,44.9412,5.76322457253418));
#66230=CARTESIAN_POINT('Ctrl Pts',(-16.1916595917224,44.88265812488,5.70404365937061));
#66231=CARTESIAN_POINT('Ctrl Pts',(-16.1702171833879,44.8212,5.64228049416099));
#66232=CARTESIAN_POINT('',(-16.5056105975083,44.8212,5.40743549732803));
#66233=CARTESIAN_POINT('Origin',(-17.98,44.8212,7.87));
#66234=CARTESIAN_POINT('',(-16.6049,44.9412,5.48825693451204));
#66235=CARTESIAN_POINT('Ctrl Pts',(-16.5056105975083,44.8212,5.40743549732802));
#66236=CARTESIAN_POINT('Ctrl Pts',(-16.5563152525204,44.8826581248801,5.44870901682921));
#66237=CARTESIAN_POINT('Ctrl Pts',(-16.6049,44.9412,5.48825693451204));
#66238=CARTESIAN_POINT('',(-16.5845512834741,44.8212,5.36185907103561));
#66239=CARTESIAN_POINT('Ctrl Pts',(-16.6049,44.9412,5.48825693451204));
#66240=CARTESIAN_POINT('Ctrl Pts',(-16.5949428723597,44.8826581248804,5.42640735011712));
#66241=CARTESIAN_POINT('Ctrl Pts',(-16.5845512834741,44.8212,5.36185907103561));
#66242=CARTESIAN_POINT('',(-16.9556297237434,44.8212,5.18882235256186));
#66243=CARTESIAN_POINT('Origin',(-17.98,44.8212,7.87));
#66244=CARTESIAN_POINT('',(-17.0393762018257,44.9412,5.28565735431459));
#66245=CARTESIAN_POINT('Ctrl Pts',(-16.9556297237434,44.8212,5.18882235256186));
#66246=CARTESIAN_POINT('Ctrl Pts',(-16.998396989666,44.8826581248802,5.23827360550292));
#66247=CARTESIAN_POINT('Ctrl Pts',(-17.0393762018257,44.9412,5.28565735431459));
#66248=CARTESIAN_POINT('',(-17.0412853866809,44.8212,5.15764624085626));
#66249=CARTESIAN_POINT('Ctrl Pts',(-17.0393762018257,44.9412,5.28565735431459));
#66250=CARTESIAN_POINT('Ctrl Pts',(-17.0403104129475,44.8826581248803,5.22301836701232));
#66251=CARTESIAN_POINT('Ctrl Pts',(-17.0412853866809,44.8212,5.15764624085625));
#66252=CARTESIAN_POINT('',(-17.4367738224661,44.8212,5.05167543387175));
#66253=CARTESIAN_POINT('Origin',(-17.98,44.8212,7.87));
#66254=CARTESIAN_POINT('',(-17.5024327817804,44.9412,5.16158171766583));
#66255=CARTESIAN_POINT('Ctrl Pts',(-17.4367738224661,44.8212,5.05167543387175));
#66256=CARTESIAN_POINT('Ctrl Pts',(-17.4703042375652,44.8826581248801,5.10780186895543));
#66257=CARTESIAN_POINT('Ctrl Pts',(-17.5024327817804,44.9412,5.16158171766583));
#66258=CARTESIAN_POINT('',(-17.5265418584009,44.8212,5.03584690713126));
#66259=CARTESIAN_POINT('Ctrl Pts',(-17.5024327817804,44.9412,5.16158171766583));
#66260=CARTESIAN_POINT('Ctrl Pts',(-17.514229946132,44.8826581248803,5.10005658138852));
#66261=CARTESIAN_POINT('Ctrl Pts',(-17.5265418584009,44.8212,5.03584690713125));
#66262=CARTESIAN_POINT('',(-17.9344235737076,44.8212,5.00016188098241));
#66263=CARTESIAN_POINT('Origin',(-17.98,44.8212,7.87));
#66264=CARTESIAN_POINT('',(-17.98,44.9412,5.1198));
#66265=CARTESIAN_POINT('Ctrl Pts',(-17.9344235737076,44.8212,5.00016188098241));
#66266=CARTESIAN_POINT('Ctrl Pts',(-17.9576983332877,44.8826581248802,5.06125812488014));
#66267=CARTESIAN_POINT('Ctrl Pts',(-17.98,44.9412,5.1198));
#66268=CARTESIAN_POINT('',(-18.0255764262924,44.8212,5.00016188098241));
#66269=CARTESIAN_POINT('Ctrl Pts',(-17.98,44.9412,5.1198));
#66270=CARTESIAN_POINT('Ctrl Pts',(-18.0023016667124,44.8826581248799,5.06125812487993));
#66271=CARTESIAN_POINT('Ctrl Pts',(-18.0255764262924,44.8212,5.00016188098241));
#66272=CARTESIAN_POINT('',(-18.4334581415991,44.8212,5.03584690713126));
#66273=CARTESIAN_POINT('Origin',(-17.98,44.8212,7.87));
#66274=CARTESIAN_POINT('',(-18.4575672182196,44.9412,5.16158171766583));
#66275=CARTESIAN_POINT('Ctrl Pts',(-18.4334581415991,44.8212,5.03584690713125));
#66276=CARTESIAN_POINT('Ctrl Pts',(-18.4457700538679,44.8826581248799,5.10005658138809));
#66277=CARTESIAN_POINT('Ctrl Pts',(-18.4575672182196,44.9412,5.16158171766583));
#66278=CARTESIAN_POINT('',(-18.5232261775339,44.8212,5.05167543387175));
#66279=CARTESIAN_POINT('Ctrl Pts',(-18.4575672182196,44.9412,5.16158171766583));
#66280=CARTESIAN_POINT('Ctrl Pts',(-18.4896957624347,44.8826581248803,5.10780186895555));
#66281=CARTESIAN_POINT('Ctrl Pts',(-18.5232261775339,44.8212,5.05167543387175));
#66282=CARTESIAN_POINT('',(-18.9187146133191,44.8212,5.15764624085626));
#66283=CARTESIAN_POINT('Origin',(-17.98,44.8212,7.87));
#66284=CARTESIAN_POINT('',(-18.9206237981743,44.9412,5.28565735431459));
#66285=CARTESIAN_POINT('Ctrl Pts',(-18.9187146133191,44.8212,5.15764624085625));
#66286=CARTESIAN_POINT('Ctrl Pts',(-18.9196895870525,44.8826581248801,5.22301836701204));
#66287=CARTESIAN_POINT('Ctrl Pts',(-18.9206237981743,44.9412,5.28565735431459));
#66288=CARTESIAN_POINT('',(-19.0043702762566,44.8212,5.18882235256187));
#66289=CARTESIAN_POINT('Ctrl Pts',(-18.9206237981743,44.9412,5.28565735431459));
#66290=CARTESIAN_POINT('Ctrl Pts',(-18.9616030103343,44.8826581248799,5.23827360550266));
#66291=CARTESIAN_POINT('Ctrl Pts',(-19.0043702762566,44.8212,5.18882235256186));
#66292=CARTESIAN_POINT('',(-19.3754487165259,44.8212,5.36185907103561));
#66293=CARTESIAN_POINT('Origin',(-17.98,44.8212,7.87));
#66294=CARTESIAN_POINT('',(-19.3551,44.9412,5.48825693451204));
#66295=CARTESIAN_POINT('Ctrl Pts',(-19.3754487165259,44.8212,5.36185907103561));
#66296=CARTESIAN_POINT('Ctrl Pts',(-19.3650571276403,44.8826581248801,5.4264073501168));
#66297=CARTESIAN_POINT('Ctrl Pts',(-19.3551,44.9412,5.48825693451204));
#66298=CARTESIAN_POINT('',(-19.4543894024917,44.8212,5.40743549732803));
#66299=CARTESIAN_POINT('Ctrl Pts',(-19.3551,44.9412,5.48825693451204));
#66300=CARTESIAN_POINT('Ctrl Pts',(-19.4036847474797,44.88265812488,5.44870901682913));
#66301=CARTESIAN_POINT('Ctrl Pts',(-19.4543894024917,44.8212,5.40743549732802));
#66302=CARTESIAN_POINT('',(-19.7897828166121,44.8212,5.642280494161));
#66303=CARTESIAN_POINT('Origin',(-17.98,44.8212,7.87));
#66304=CARTESIAN_POINT('',(-19.7477944841599,44.9412,5.76322457253419));
#66305=CARTESIAN_POINT('Ctrl Pts',(-19.7897828166121,44.8212,5.642280494161));
#66306=CARTESIAN_POINT('Ctrl Pts',(-19.7683404082776,44.88265812488,5.70404365937065));
#66307=CARTESIAN_POINT('Ctrl Pts',(-19.7477944841599,44.9412,5.76322457253419));
#66308=CARTESIAN_POINT('',(-19.8596099528092,44.8212,5.70087241839011));
#66309=CARTESIAN_POINT('Ctrl Pts',(-19.7477944841599,44.9412,5.76322457253419));
#66310=CARTESIAN_POINT('Ctrl Pts',(-19.8025085439923,44.8826581248798,5.73271412944674));
#66311=CARTESIAN_POINT('Ctrl Pts',(-19.8596099528092,44.8212,5.70087241839011));
#66312=CARTESIAN_POINT('',(-20.1491275816099,44.8212,5.99039004719085));
#66313=CARTESIAN_POINT('Origin',(-17.98,44.8212,7.87));
#66314=CARTESIAN_POINT('',(-20.0867754274658,44.9412,6.10220551584008));
#66315=CARTESIAN_POINT('Ctrl Pts',(-20.1491275816099,44.8212,5.99039004719084));
#66316=CARTESIAN_POINT('Ctrl Pts',(-20.1172858705531,44.8826581248802,6.04749145600798));
#66317=CARTESIAN_POINT('Ctrl Pts',(-20.0867754274658,44.9412,6.10220551584008));
#66318=CARTESIAN_POINT('',(-20.207719505839,44.8212,6.0602171833879));
#66319=CARTESIAN_POINT('Ctrl Pts',(-20.0867754274658,44.9412,6.10220551584008));
#66320=CARTESIAN_POINT('Ctrl Pts',(-20.1459563406292,44.8826581248801,6.08165959172247));
#66321=CARTESIAN_POINT('Ctrl Pts',(-20.207719505839,44.8212,6.0602171833879));
#66322=CARTESIAN_POINT('',(-20.442564502672,44.8212,6.39561059750827));
#66323=CARTESIAN_POINT('Origin',(-17.98,44.8212,7.87));
#66324=CARTESIAN_POINT('',(-20.361743065488,44.9412,6.4949));
#66325=CARTESIAN_POINT('Ctrl Pts',(-20.442564502672,44.8212,6.39561059750826));
#66326=CARTESIAN_POINT('Ctrl Pts',(-20.401290983171,44.8826581248798,6.44631525252014));
#66327=CARTESIAN_POINT('Ctrl Pts',(-20.361743065488,44.9412,6.4949));
#66328=CARTESIAN_POINT('',(-20.4881409289644,44.8212,6.47455128347415));
#66329=CARTESIAN_POINT('Ctrl Pts',(-20.361743065488,44.9412,6.4949));
#66330=CARTESIAN_POINT('Ctrl Pts',(-20.4235926498833,44.8826581248799,6.48494287235964));
#66331=CARTESIAN_POINT('Ctrl Pts',(-20.4881409289644,44.8212,6.47455128347414));
#66332=CARTESIAN_POINT('',(-20.6611776474381,44.8212,6.84562972374336));
#66333=CARTESIAN_POINT('Origin',(-17.98,44.8212,7.87));
#66334=CARTESIAN_POINT('',(-20.5643426456854,44.9412,6.92937620182574));
#66335=CARTESIAN_POINT('Ctrl Pts',(-20.6611776474381,44.8212,6.84562972374336));
#66336=CARTESIAN_POINT('Ctrl Pts',(-20.6117263944974,44.8826581248799,6.88839698966571));
#66337=CARTESIAN_POINT('Ctrl Pts',(-20.5643426456854,44.9412,6.92937620182574));
#66338=CARTESIAN_POINT('',(-20.6923537591437,44.8212,6.93128538668091));
#66339=CARTESIAN_POINT('Ctrl Pts',(-20.5643426456854,44.9412,6.92937620182574));
#66340=CARTESIAN_POINT('Ctrl Pts',(-20.6269816329882,44.8826581248799,6.9303104129475));
#66341=CARTESIAN_POINT('Ctrl Pts',(-20.6923537591437,44.8212,6.93128538668091));
#66342=CARTESIAN_POINT('',(-20.7983245661282,44.8212,7.32677382246615));
#66343=CARTESIAN_POINT('Origin',(-17.98,44.8212,7.87));
#66344=CARTESIAN_POINT('',(-20.6884182823342,44.9412,7.39243278178041));
#66345=CARTESIAN_POINT('Ctrl Pts',(-20.7983245661282,44.8212,7.32677382246615));
#66346=CARTESIAN_POINT('Ctrl Pts',(-20.7421981310449,44.8826581248798,7.36030423756504));
#66347=CARTESIAN_POINT('Ctrl Pts',(-20.6884182823342,44.9412,7.39243278178041));
#66348=CARTESIAN_POINT('',(-20.8141530928687,44.8212,7.41654185840086));
#66349=CARTESIAN_POINT('Ctrl Pts',(-20.6884182823342,44.9412,7.39243278178041));
#66350=CARTESIAN_POINT('Ctrl Pts',(-20.7499434186121,44.8826581248797,7.40422994613214));
#66351=CARTESIAN_POINT('Ctrl Pts',(-20.8141530928687,44.8212,7.41654185840087));
#66352=CARTESIAN_POINT('',(-20.8498381190176,44.8212,7.82442357370758));
#66353=CARTESIAN_POINT('Origin',(-17.98,44.8212,7.87));
#66354=CARTESIAN_POINT('Ctrl Pts',(-20.8498381190176,44.8212,7.82442357370758));
#66355=CARTESIAN_POINT('Ctrl Pts',(-20.7887418751198,44.8826581248802,7.8476983332877));
#66356=CARTESIAN_POINT('Ctrl Pts',(-20.7302,44.9412,7.87));
#66357=CARTESIAN_POINT('',(-20.5502,45.1212,7.87));
#66358=CARTESIAN_POINT('',(-20.7002,44.9712,7.87));
#66359=CARTESIAN_POINT('Origin',(-17.98,45.1212,7.87));
#66360=CARTESIAN_POINT('Origin',(-14.9462632306524,45.1212,6.93607856095471));
#66361=CARTESIAN_POINT('',(-15.2676462408563,42.216,6.93128538668091));
#66362=CARTESIAN_POINT('',(-15.2676462408563,41.616,6.93128538668091));
#66363=CARTESIAN_POINT('',(-15.3956573543146,42.216,6.92937620182574));
#66364=CARTESIAN_POINT('',(-14.9462632306524,42.216,6.93607856095471));
#66365=CARTESIAN_POINT('',(-15.3956573543146,45.1212,6.92937620182574));
#66366=CARTESIAN_POINT('Origin',(-15.3956573543146,45.1212,6.92937620182574));
#66367=CARTESIAN_POINT('',(-15.2988223525619,42.216,6.84562972374336));
#66368=CARTESIAN_POINT('',(-15.2988223525619,41.616,6.84562972374336));
#66369=CARTESIAN_POINT('',(-15.3956573543146,42.216,6.92937620182574));
#66370=CARTESIAN_POINT('Origin',(-15.1983219039495,42.216,6.85755197172735));
#66371=CARTESIAN_POINT('Origin',(-17.98,42.216,7.87));
#66372=CARTESIAN_POINT('Origin',(-15.1545262649226,45.1212,6.42346406460551));
#66373=CARTESIAN_POINT('',(-15.4718590710356,42.216,6.47455128347414));
#66374=CARTESIAN_POINT('',(-15.4718590710356,41.616,6.47455128347414));
#66375=CARTESIAN_POINT('',(-15.598256934512,42.216,6.4949));
#66376=CARTESIAN_POINT('',(-15.1545262649226,42.216,6.42346406460551));
#66377=CARTESIAN_POINT('',(-15.598256934512,45.1212,6.4949));
#66378=CARTESIAN_POINT('Origin',(-15.598256934512,45.1212,6.4949));
#66379=CARTESIAN_POINT('',(-15.517435497328,42.216,6.39561059750826));
#66380=CARTESIAN_POINT('',(-15.517435497328,41.616,6.39561059750826));
#66381=CARTESIAN_POINT('',(-15.598256934512,42.216,6.4949));
#66382=CARTESIAN_POINT('Origin',(-15.4163915997173,42.216,6.3899));
#66383=CARTESIAN_POINT('Origin',(-17.98,42.216,7.87));
#66384=CARTESIAN_POINT('Origin',(-15.4486398888744,45.1212,5.95480183067077));
#66385=CARTESIAN_POINT('',(-15.752280494161,42.216,6.0602171833879));
#66386=CARTESIAN_POINT('',(-15.752280494161,41.616,6.0602171833879));
#66387=CARTESIAN_POINT('',(-15.8732245725342,42.216,6.10220551584008));
#66388=CARTESIAN_POINT('',(-15.4486398888744,42.216,5.95480183067077));
#66389=CARTESIAN_POINT('',(-15.8732245725342,45.1212,6.10220551584008));
#66390=CARTESIAN_POINT('Origin',(-15.8732245725342,45.1212,6.10220551584008));
#66391=CARTESIAN_POINT('',(-15.8108724183901,42.216,5.99039004719084));
#66392=CARTESIAN_POINT('',(-15.8108724183901,41.616,5.99039004719084));
#66393=CARTESIAN_POINT('',(-15.8732245725342,42.216,6.10220551584008));
#66394=CARTESIAN_POINT('Origin',(-15.7123552394792,42.216,5.96722011780591));
#66395=CARTESIAN_POINT('Origin',(-17.98,42.216,7.87));
#66396=CARTESIAN_POINT('Origin',(-15.8196676088727,45.1212,5.54433192397406));
#66397=CARTESIAN_POINT('',(-16.1003900471908,42.216,5.70087241839011));
#66398=CARTESIAN_POINT('',(-16.1003900471908,41.616,5.70087241839011));
#66399=CARTESIAN_POINT('',(-16.2122055158401,42.216,5.76322457253418));
#66400=CARTESIAN_POINT('',(-15.8196676088727,42.216,5.54433192397406));
#66401=CARTESIAN_POINT('',(-16.2122055158401,45.1212,5.76322457253418));
#66402=CARTESIAN_POINT('Origin',(-16.2122055158401,45.1212,5.76322457253418));
#66403=CARTESIAN_POINT('',(-16.1702171833879,42.216,5.642280494161));
#66404=CARTESIAN_POINT('',(-16.1702171833879,41.616,5.642280494161));
#66405=CARTESIAN_POINT('',(-16.2122055158401,42.216,5.76322457253418));
#66406=CARTESIAN_POINT('Origin',(-16.0772201178059,42.216,5.6023552394792));
#66407=CARTESIAN_POINT('Origin',(-17.98,42.216,7.87));
#66408=CARTESIAN_POINT('Origin',(-16.2563359353945,45.1212,5.20452626492257));
#66409=CARTESIAN_POINT('',(-16.5056105975083,42.216,5.40743549732803));
#66410=CARTESIAN_POINT('',(-16.5056105975083,41.616,5.40743549732803));
#66411=CARTESIAN_POINT('',(-16.6049,42.216,5.48825693451204));
#66412=CARTESIAN_POINT('',(-16.2563359353945,42.216,5.20452626492257));
#66413=CARTESIAN_POINT('',(-16.6049,45.1212,5.48825693451204));
#66414=CARTESIAN_POINT('Origin',(-16.6049,45.1212,5.48825693451204));
#66415=CARTESIAN_POINT('',(-16.5845512834741,42.216,5.36185907103561));
#66416=CARTESIAN_POINT('',(-16.5845512834741,41.616,5.36185907103561));
#66417=CARTESIAN_POINT('',(-16.6049,42.216,5.48825693451204));
#66418=CARTESIAN_POINT('Origin',(-16.4999,42.216,5.30639159971731));
#66419=CARTESIAN_POINT('Origin',(-17.98,42.216,7.87));
#66420=CARTESIAN_POINT('Origin',(-16.7453769223032,45.1212,4.94570967651662));
#66421=CARTESIAN_POINT('',(-16.9556297237434,42.216,5.18882235256186));
#66422=CARTESIAN_POINT('',(-16.9556297237434,41.616,5.18882235256186));
#66423=CARTESIAN_POINT('',(-17.0393762018257,42.216,5.28565735431459));
#66424=CARTESIAN_POINT('',(-16.7453769223032,42.216,4.94570967651662));
#66425=CARTESIAN_POINT('',(-17.0393762018257,45.1212,5.28565735431459));
#66426=CARTESIAN_POINT('Origin',(-17.0393762018257,45.1212,5.28565735431459));
#66427=CARTESIAN_POINT('',(-17.0412853866809,42.216,5.15764624085626));
#66428=CARTESIAN_POINT('',(-17.0412853866809,41.616,5.15764624085626));
#66429=CARTESIAN_POINT('',(-17.0393762018257,42.216,5.28565735431459));
#66430=CARTESIAN_POINT('Origin',(-16.9675519717274,42.216,5.08832190394955));
#66431=CARTESIAN_POINT('Origin',(-17.98,42.216,7.87));
#66432=CARTESIAN_POINT('Origin',(-17.2719313066783,45.1212,4.77574616982741));
#66433=CARTESIAN_POINT('',(-17.4367738224661,42.216,5.05167543387175));
#66434=CARTESIAN_POINT('',(-17.4367738224661,41.616,5.05167543387175));
#66435=CARTESIAN_POINT('',(-17.5024327817804,42.216,5.16158171766583));
#66436=CARTESIAN_POINT('',(-17.2719313066783,42.216,4.77574616982741));
#66437=CARTESIAN_POINT('',(-17.5024327817804,45.1212,5.16158171766583));
#66438=CARTESIAN_POINT('Origin',(-17.5024327817804,45.1212,5.16158171766583));
#66439=CARTESIAN_POINT('',(-17.5265418584009,42.216,5.03584690713126));
#66440=CARTESIAN_POINT('',(-17.5265418584009,41.616,5.03584690713126));
#66441=CARTESIAN_POINT('',(-17.5024327817804,42.216,5.16158171766583));
#66442=CARTESIAN_POINT('Origin',(-17.4659666644704,42.216,4.95477208953326));
#66443=CARTESIAN_POINT('Origin',(-17.98,42.216,7.87));
#66444=CARTESIAN_POINT('Origin',(-17.82,45.1212,4.6998));
#66445=CARTESIAN_POINT('',(-17.9344235737076,42.216,5.00016188098241));
#66446=CARTESIAN_POINT('',(-17.9344235737076,41.616,5.00016188098241));
#66447=CARTESIAN_POINT('',(-17.98,42.216,5.1198));
#66448=CARTESIAN_POINT('',(-17.82,42.216,4.6998));
#66449=CARTESIAN_POINT('',(-17.98,45.1212,5.1198));
#66450=CARTESIAN_POINT('Origin',(-17.98,45.1212,5.1198));
#66451=CARTESIAN_POINT('',(-18.0255764262924,42.216,5.00016188098241));
#66452=CARTESIAN_POINT('',(-18.0255764262924,41.616,5.00016188098241));
#66453=CARTESIAN_POINT('',(-17.98,42.216,5.1198));
#66454=CARTESIAN_POINT('Origin',(-17.98,42.216,4.9098));
#66455=CARTESIAN_POINT('Origin',(-17.98,42.216,7.87));
#66456=CARTESIAN_POINT('Origin',(-18.3729302123577,45.1212,4.72017875297399));
#66457=CARTESIAN_POINT('',(-18.4334581415991,42.216,5.03584690713126));
#66458=CARTESIAN_POINT('',(-18.4334581415991,41.616,5.03584690713126));
#66459=CARTESIAN_POINT('',(-18.4575672182196,42.216,5.16158171766583));
#66460=CARTESIAN_POINT('',(-18.3729302123577,42.216,4.72017875297399));
#66461=CARTESIAN_POINT('',(-18.4575672182196,45.1212,5.16158171766583));
#66462=CARTESIAN_POINT('Origin',(-18.4575672182196,45.1212,5.16158171766583));
#66463=CARTESIAN_POINT('',(-18.5232261775339,42.216,5.05167543387175));
#66464=CARTESIAN_POINT('',(-18.5232261775339,41.616,5.05167543387175));
#66465=CARTESIAN_POINT('',(-18.4575672182196,42.216,5.16158171766583));
#66466=CARTESIAN_POINT('Origin',(-18.4940333355296,42.216,4.95477208953326));
#66467=CARTESIAN_POINT('Origin',(-17.98,42.216,7.87));
#66468=CARTESIAN_POINT('Origin',(-18.9139214390453,45.1212,4.83626323065241));
#66469=CARTESIAN_POINT('',(-18.9187146133191,42.216,5.15764624085626));
#66470=CARTESIAN_POINT('',(-18.9187146133191,41.616,5.15764624085626));
#66471=CARTESIAN_POINT('',(-18.9206237981743,42.216,5.28565735431459));
#66472=CARTESIAN_POINT('',(-18.9139214390453,42.216,4.83626323065241));
#66473=CARTESIAN_POINT('',(-18.9206237981743,45.1212,5.28565735431459));
#66474=CARTESIAN_POINT('Origin',(-18.9206237981743,45.1212,5.28565735431459));
#66475=CARTESIAN_POINT('',(-19.0043702762566,42.216,5.18882235256187));
#66476=CARTESIAN_POINT('',(-19.0043702762566,41.616,5.18882235256187));
#66477=CARTESIAN_POINT('',(-18.9206237981743,42.216,5.28565735431459));
#66478=CARTESIAN_POINT('Origin',(-18.9924480282726,42.216,5.08832190394955));
#66479=CARTESIAN_POINT('Origin',(-17.98,42.216,7.87));
#66480=CARTESIAN_POINT('Origin',(-19.4265359353945,45.1212,5.04452626492258));
#66481=CARTESIAN_POINT('',(-19.3754487165259,42.216,5.36185907103561));
#66482=CARTESIAN_POINT('',(-19.3754487165259,41.616,5.36185907103561));
#66483=CARTESIAN_POINT('',(-19.3551,42.216,5.48825693451204));
#66484=CARTESIAN_POINT('',(-19.4265359353945,42.216,5.04452626492258));
#66485=CARTESIAN_POINT('',(-19.3551,45.1212,5.48825693451204));
#66486=CARTESIAN_POINT('Origin',(-19.3551,45.1212,5.48825693451204));
#66487=CARTESIAN_POINT('',(-19.4543894024917,42.216,5.40743549732803));
#66488=CARTESIAN_POINT('',(-19.4543894024917,41.616,5.40743549732803));
#66489=CARTESIAN_POINT('',(-19.3551,42.216,5.48825693451204));
#66490=CARTESIAN_POINT('Origin',(-19.4601,42.216,5.30639159971731));
#66491=CARTESIAN_POINT('Origin',(-17.98,42.216,7.87));
#66492=CARTESIAN_POINT('Origin',(-19.8951981693292,45.1212,5.33863988887437));
#66493=CARTESIAN_POINT('',(-19.7897828166121,42.216,5.642280494161));
#66494=CARTESIAN_POINT('',(-19.7897828166121,41.616,5.642280494161));
#66495=CARTESIAN_POINT('',(-19.7477944841599,42.216,5.76322457253419));
#66496=CARTESIAN_POINT('',(-19.8951981693292,42.216,5.33863988887437));
#66497=CARTESIAN_POINT('',(-19.7477944841599,45.1212,5.76322457253419));
#66498=CARTESIAN_POINT('Origin',(-19.7477944841599,45.1212,5.76322457253419));
#66499=CARTESIAN_POINT('',(-19.8596099528092,42.216,5.70087241839011));
#66500=CARTESIAN_POINT('',(-19.8596099528092,41.616,5.70087241839011));
#66501=CARTESIAN_POINT('',(-19.7477944841599,42.216,5.76322457253419));
#66502=CARTESIAN_POINT('Origin',(-19.8827798821941,42.216,5.6023552394792));
#66503=CARTESIAN_POINT('Origin',(-17.98,42.216,7.87));
#66504=CARTESIAN_POINT('Origin',(-20.3056680760259,45.1212,5.7096676088727));
#66505=CARTESIAN_POINT('',(-20.1491275816099,42.216,5.99039004719085));
#66506=CARTESIAN_POINT('',(-20.1491275816099,41.616,5.99039004719085));
#66507=CARTESIAN_POINT('',(-20.0867754274658,42.216,6.10220551584008));
#66508=CARTESIAN_POINT('',(-20.3056680760259,42.216,5.7096676088727));
#66509=CARTESIAN_POINT('',(-20.0867754274658,45.1212,6.10220551584008));
#66510=CARTESIAN_POINT('Origin',(-20.0867754274658,45.1212,6.10220551584008));
#66511=CARTESIAN_POINT('',(-20.207719505839,42.216,6.0602171833879));
#66512=CARTESIAN_POINT('',(-20.207719505839,41.616,6.0602171833879));
#66513=CARTESIAN_POINT('',(-20.0867754274658,42.216,6.10220551584008));
#66514=CARTESIAN_POINT('Origin',(-20.2476447605208,42.216,5.96722011780591));
#66515=CARTESIAN_POINT('Origin',(-17.98,42.216,7.87));
#66516=CARTESIAN_POINT('Origin',(-20.6454737350774,45.1212,6.14633593539449));
#66517=CARTESIAN_POINT('',(-20.442564502672,42.216,6.39561059750827));
#66518=CARTESIAN_POINT('',(-20.442564502672,41.616,6.39561059750827));
#66519=CARTESIAN_POINT('',(-20.361743065488,42.216,6.4949));
#66520=CARTESIAN_POINT('',(-20.6454737350774,42.216,6.14633593539449));
#66521=CARTESIAN_POINT('',(-20.361743065488,45.1212,6.4949));
#66522=CARTESIAN_POINT('Origin',(-20.361743065488,45.1212,6.4949));
#66523=CARTESIAN_POINT('',(-20.4881409289644,42.216,6.47455128347415));
#66524=CARTESIAN_POINT('',(-20.4881409289644,41.616,6.47455128347415));
#66525=CARTESIAN_POINT('',(-20.361743065488,42.216,6.4949));
#66526=CARTESIAN_POINT('Origin',(-20.5436084002827,42.216,6.3899));
#66527=CARTESIAN_POINT('Origin',(-17.98,42.216,7.87));
#66528=CARTESIAN_POINT('Origin',(-20.9042903234834,45.1212,6.63537692230322));
#66529=CARTESIAN_POINT('',(-20.6611776474381,42.216,6.84562972374336));
#66530=CARTESIAN_POINT('',(-20.6611776474381,41.616,6.84562972374336));
#66531=CARTESIAN_POINT('',(-20.5643426456854,42.216,6.92937620182575));
#66532=CARTESIAN_POINT('',(-20.9042903234834,42.216,6.63537692230322));
#66533=CARTESIAN_POINT('',(-20.5643426456854,45.1212,6.92937620182575));
#66534=CARTESIAN_POINT('Origin',(-20.5643426456854,45.1212,6.92937620182575));
#66535=CARTESIAN_POINT('',(-20.6923537591437,42.216,6.93128538668091));
#66536=CARTESIAN_POINT('',(-20.6923537591437,41.616,6.93128538668091));
#66537=CARTESIAN_POINT('',(-20.5643426456854,42.216,6.92937620182575));
#66538=CARTESIAN_POINT('Origin',(-20.7616780960504,42.216,6.85755197172736));
#66539=CARTESIAN_POINT('Origin',(-17.98,42.216,7.87));
#66540=CARTESIAN_POINT('Origin',(-21.0742538301726,45.1212,7.16193130667835));
#66541=CARTESIAN_POINT('',(-20.7983245661282,42.216,7.32677382246615));
#66542=CARTESIAN_POINT('',(-20.7983245661282,41.616,7.32677382246615));
#66543=CARTESIAN_POINT('',(-20.6884182823342,42.216,7.39243278178041));
#66544=CARTESIAN_POINT('',(-21.0742538301726,42.216,7.16193130667835));
#66545=CARTESIAN_POINT('',(-20.6884182823342,45.1212,7.39243278178041));
#66546=CARTESIAN_POINT('Origin',(-20.6884182823342,45.1212,7.39243278178041));
#66547=CARTESIAN_POINT('',(-20.8141530928687,42.216,7.41654185840086));
#66548=CARTESIAN_POINT('',(-20.8141530928687,41.616,7.41654185840086));
#66549=CARTESIAN_POINT('',(-20.6884182823342,42.216,7.39243278178041));
#66550=CARTESIAN_POINT('Origin',(-20.8952279104667,42.216,7.35596666447035));
#66551=CARTESIAN_POINT('Origin',(-17.98,42.216,7.87));
#66552=CARTESIAN_POINT('Origin',(-21.1502,45.1212,7.71));
#66553=CARTESIAN_POINT('',(-20.8498381190176,42.216,7.82442357370758));
#66554=CARTESIAN_POINT('',(-20.8498381190176,41.616,7.82442357370758));
#66555=CARTESIAN_POINT('',(-20.7302,42.216,7.87));
#66556=CARTESIAN_POINT('',(-21.1502,42.216,7.71));
#66557=CARTESIAN_POINT('',(-20.7302,45.1212,7.87));
#66558=CARTESIAN_POINT('Origin',(-20.7302,45.1212,7.87));
#66559=CARTESIAN_POINT('',(-20.8498381190176,42.216,7.91557642629242));
#66560=CARTESIAN_POINT('',(-20.8498381190176,41.616,7.91557642629242));
#66561=CARTESIAN_POINT('',(-20.7302,42.216,7.87));
#66562=CARTESIAN_POINT('Origin',(-20.9402,42.216,7.87));
#66563=CARTESIAN_POINT('',(-20.8502,42.216,7.87));
#66564=CARTESIAN_POINT('Origin',(-17.98,42.216,7.87));
#66565=CARTESIAN_POINT('Origin',(-17.98,42.216,7.87));
#66566=CARTESIAN_POINT('Origin',(-21.129821247026,45.1212,8.26293021235775));
#66567=CARTESIAN_POINT('',(-20.8141530928687,42.216,8.32345814159914));
#66568=CARTESIAN_POINT('',(-20.8141530928687,41.616,8.32345814159914));
#66569=CARTESIAN_POINT('',(-20.6884182823342,42.216,8.34756721821959));
#66570=CARTESIAN_POINT('',(-21.129821247026,42.216,8.26293021235775));
#66571=CARTESIAN_POINT('',(-20.6884182823342,45.1212,8.34756721821959));
#66572=CARTESIAN_POINT('Origin',(-20.6884182823342,45.1212,8.34756721821959));
#66573=CARTESIAN_POINT('',(-20.7983245661282,42.216,8.41322617753386));
#66574=CARTESIAN_POINT('',(-20.7983245661282,41.616,8.41322617753386));
#66575=CARTESIAN_POINT('',(-20.6884182823342,42.216,8.34756721821959));
#66576=CARTESIAN_POINT('Origin',(-20.8952279104667,42.216,8.38403333552965));
#66577=CARTESIAN_POINT('Origin',(-17.98,42.216,7.87));
#66578=CARTESIAN_POINT('Origin',(-21.0137367693476,45.1212,8.80392143904529));
#66579=CARTESIAN_POINT('',(-20.6923537591437,42.216,8.80871461331909));
#66580=CARTESIAN_POINT('',(-20.6923537591437,41.616,8.80871461331909));
#66581=CARTESIAN_POINT('',(-20.5643426456854,42.216,8.81062379817425));
#66582=CARTESIAN_POINT('',(-21.0137367693476,42.216,8.80392143904529));
#66583=CARTESIAN_POINT('',(-20.5643426456854,45.1212,8.81062379817425));
#66584=CARTESIAN_POINT('Origin',(-20.5643426456854,45.1212,8.81062379817425));
#66585=CARTESIAN_POINT('',(-20.6611776474381,42.216,8.89437027625664));
#66586=CARTESIAN_POINT('',(-20.6611776474381,41.616,8.89437027625664));
#66587=CARTESIAN_POINT('',(-20.5643426456854,42.216,8.81062379817425));
#66588=CARTESIAN_POINT('Origin',(-20.7616780960504,42.216,8.88244802827264));
#66589=CARTESIAN_POINT('Origin',(-17.98,42.216,7.87));
#66590=CARTESIAN_POINT('Origin',(-20.8054737350774,45.1212,9.31653593539449));
#66591=CARTESIAN_POINT('',(-20.4881409289644,42.216,9.26544871652585));
#66592=CARTESIAN_POINT('',(-20.4881409289644,41.616,9.26544871652585));
#66593=CARTESIAN_POINT('',(-20.361743065488,42.216,9.2451));
#66594=CARTESIAN_POINT('',(-20.8054737350774,42.216,9.31653593539449));
#66595=CARTESIAN_POINT('',(-20.361743065488,45.1212,9.2451));
#66596=CARTESIAN_POINT('Origin',(-20.361743065488,45.1212,9.2451));
#66597=CARTESIAN_POINT('',(-20.442564502672,42.216,9.34438940249174));
#66598=CARTESIAN_POINT('',(-20.442564502672,41.616,9.34438940249174));
#66599=CARTESIAN_POINT('',(-20.361743065488,42.216,9.2451));
#66600=CARTESIAN_POINT('Origin',(-20.5436084002827,42.216,9.3501));
#66601=CARTESIAN_POINT('Origin',(-17.98,42.216,7.87));
#66602=CARTESIAN_POINT('Origin',(-20.5113601111256,45.1212,9.78519816932923));
#66603=CARTESIAN_POINT('',(-20.207719505839,42.216,9.67978281661211));
#66604=CARTESIAN_POINT('',(-20.207719505839,41.616,9.67978281661211));
#66605=CARTESIAN_POINT('',(-20.0867754274658,42.216,9.63779448415992));
#66606=CARTESIAN_POINT('',(-20.5113601111256,42.216,9.78519816932923));
#66607=CARTESIAN_POINT('',(-20.0867754274658,45.1212,9.63779448415992));
#66608=CARTESIAN_POINT('Origin',(-20.0867754274658,45.1212,9.63779448415992));
#66609=CARTESIAN_POINT('',(-20.1491275816099,42.216,9.74960995280916));
#66610=CARTESIAN_POINT('',(-20.1491275816099,41.616,9.74960995280916));
#66611=CARTESIAN_POINT('',(-20.0867754274658,42.216,9.63779448415992));
#66612=CARTESIAN_POINT('Origin',(-20.2476447605208,42.216,9.77277988219409));
#66613=CARTESIAN_POINT('Origin',(-17.98,42.216,7.87));
#66614=CARTESIAN_POINT('Origin',(-20.1403323911273,45.1212,10.1956680760259));
#66615=CARTESIAN_POINT('',(-19.8596099528092,42.216,10.0391275816099));
#66616=CARTESIAN_POINT('',(-19.8596099528092,41.616,10.0391275816099));
#66617=CARTESIAN_POINT('',(-19.7477944841599,42.216,9.97677542746581));
#66618=CARTESIAN_POINT('',(-20.1403323911273,42.216,10.1956680760259));
#66619=CARTESIAN_POINT('',(-19.7477944841599,45.1212,9.97677542746581));
#66620=CARTESIAN_POINT('Origin',(-19.7477944841599,45.1212,9.97677542746581));
#66621=CARTESIAN_POINT('',(-19.7897828166121,42.216,10.097719505839));
#66622=CARTESIAN_POINT('',(-19.7897828166121,41.616,10.097719505839));
#66623=CARTESIAN_POINT('',(-19.7477944841599,42.216,9.97677542746581));
#66624=CARTESIAN_POINT('Origin',(-19.8827798821941,42.216,10.1376447605208));
#66625=CARTESIAN_POINT('Origin',(-17.98,42.216,7.87));
#66626=CARTESIAN_POINT('Origin',(-19.7036640646055,45.1212,10.5354737350774));
#66627=CARTESIAN_POINT('',(-19.4543894024917,42.216,10.332564502672));
#66628=CARTESIAN_POINT('',(-19.4543894024917,41.616,10.332564502672));
#66629=CARTESIAN_POINT('',(-19.3551,42.216,10.251743065488));
#66630=CARTESIAN_POINT('',(-19.7036640646055,42.216,10.5354737350774));
#66631=CARTESIAN_POINT('',(-19.3551,45.1212,10.251743065488));
#66632=CARTESIAN_POINT('Origin',(-19.3551,45.1212,10.251743065488));
#66633=CARTESIAN_POINT('',(-19.3754487165258,42.216,10.3781409289644));
#66634=CARTESIAN_POINT('',(-19.3754487165258,41.616,10.3781409289644));
#66635=CARTESIAN_POINT('',(-19.3551,42.216,10.251743065488));
#66636=CARTESIAN_POINT('Origin',(-19.4601,42.216,10.4336084002827));
#66637=CARTESIAN_POINT('Origin',(-17.98,42.216,7.87));
#66638=CARTESIAN_POINT('Origin',(-19.2146230776968,45.1212,10.7942903234834));
#66639=CARTESIAN_POINT('',(-19.0043702762566,42.216,10.5511776474381));
#66640=CARTESIAN_POINT('',(-19.0043702762566,41.616,10.5511776474381));
#66641=CARTESIAN_POINT('',(-18.9206237981742,42.216,10.4543426456854));
#66642=CARTESIAN_POINT('',(-19.2146230776968,42.216,10.7942903234834));
#66643=CARTESIAN_POINT('',(-18.9206237981742,45.1212,10.4543426456854));
#66644=CARTESIAN_POINT('Origin',(-18.9206237981742,45.1212,10.4543426456854));
#66645=CARTESIAN_POINT('',(-18.9187146133191,42.216,10.5823537591437));
#66646=CARTESIAN_POINT('',(-18.9187146133191,41.616,10.5823537591437));
#66647=CARTESIAN_POINT('',(-18.9206237981742,42.216,10.4543426456854));
#66648=CARTESIAN_POINT('Origin',(-18.9924480282726,42.216,10.6516780960504));
#66649=CARTESIAN_POINT('Origin',(-17.98,42.216,7.87));
#66650=CARTESIAN_POINT('Origin',(-18.6880686933217,45.1212,10.9642538301726));
#66651=CARTESIAN_POINT('',(-18.5232261775339,42.216,10.6883245661282));
#66652=CARTESIAN_POINT('',(-18.5232261775339,41.616,10.6883245661282));
#66653=CARTESIAN_POINT('',(-18.4575672182196,42.216,10.5784182823342));
#66654=CARTESIAN_POINT('',(-18.6880686933217,42.216,10.9642538301726));
#66655=CARTESIAN_POINT('',(-18.4575672182196,45.1212,10.5784182823342));
#66656=CARTESIAN_POINT('Origin',(-18.4575672182196,45.1212,10.5784182823342));
#66657=CARTESIAN_POINT('',(-18.4334581415991,42.216,10.7041530928687));
#66658=CARTESIAN_POINT('',(-18.4334581415991,41.616,10.7041530928687));
#66659=CARTESIAN_POINT('',(-18.4575672182196,42.216,10.5784182823342));
#66660=CARTESIAN_POINT('Origin',(-18.4940333355296,42.216,10.7852279104667));
#66661=CARTESIAN_POINT('Origin',(-17.98,42.216,7.87));
#66662=CARTESIAN_POINT('Origin',(-18.14,45.1212,11.0402));
#66663=CARTESIAN_POINT('',(-18.0255764262924,42.216,10.7398381190176));
#66664=CARTESIAN_POINT('',(-18.0255764262924,41.616,10.7398381190176));
#66665=CARTESIAN_POINT('',(-17.98,42.216,10.6202));
#66666=CARTESIAN_POINT('',(-18.14,42.216,11.0402));
#66667=CARTESIAN_POINT('',(-17.98,45.1212,10.6202));
#66668=CARTESIAN_POINT('Origin',(-17.98,45.1212,10.6202));
#66669=CARTESIAN_POINT('',(-17.9344235737076,42.216,10.7398381190176));
#66670=CARTESIAN_POINT('',(-17.9344235737076,41.616,10.7398381190176));
#66671=CARTESIAN_POINT('',(-17.98,42.216,10.6202));
#66672=CARTESIAN_POINT('Origin',(-17.98,42.216,10.8302));
#66673=CARTESIAN_POINT('Origin',(-17.98,42.216,7.87));
#66674=CARTESIAN_POINT('Origin',(-17.5870697876422,45.1212,11.019821247026));
#66675=CARTESIAN_POINT('',(-17.5265418584009,42.216,10.7041530928687));
#66676=CARTESIAN_POINT('',(-17.5265418584009,41.616,10.7041530928687));
#66677=CARTESIAN_POINT('',(-17.5024327817804,42.216,10.5784182823342));
#66678=CARTESIAN_POINT('',(-17.5870697876422,42.216,11.019821247026));
#66679=CARTESIAN_POINT('',(-17.5024327817804,45.1212,10.5784182823342));
#66680=CARTESIAN_POINT('Origin',(-17.5024327817804,45.1212,10.5784182823342));
#66681=CARTESIAN_POINT('',(-17.4367738224661,42.216,10.6883245661282));
#66682=CARTESIAN_POINT('',(-17.4367738224661,41.616,10.6883245661282));
#66683=CARTESIAN_POINT('',(-17.5024327817804,42.216,10.5784182823342));
#66684=CARTESIAN_POINT('Origin',(-17.4659666644703,42.216,10.7852279104667));
#66685=CARTESIAN_POINT('Origin',(-17.98,42.216,7.87));
#66686=CARTESIAN_POINT('Origin',(-17.0460785609547,45.1212,10.9037367693476));
#66687=CARTESIAN_POINT('',(-17.0412853866809,42.216,10.5823537591437));
#66688=CARTESIAN_POINT('',(-17.0412853866809,41.616,10.5823537591437));
#66689=CARTESIAN_POINT('',(-17.0393762018257,42.216,10.4543426456854));
#66690=CARTESIAN_POINT('',(-17.0460785609547,42.216,10.9037367693476));
#66691=CARTESIAN_POINT('',(-17.0393762018257,45.1212,10.4543426456854));
#66692=CARTESIAN_POINT('Origin',(-17.0393762018257,45.1212,10.4543426456854));
#66693=CARTESIAN_POINT('',(-16.9556297237434,42.216,10.5511776474381));
#66694=CARTESIAN_POINT('',(-16.9556297237434,41.616,10.5511776474381));
#66695=CARTESIAN_POINT('',(-17.0393762018257,42.216,10.4543426456854));
#66696=CARTESIAN_POINT('Origin',(-16.9675519717273,42.216,10.6516780960504));
#66697=CARTESIAN_POINT('Origin',(-17.98,42.216,7.87));
#66698=CARTESIAN_POINT('Origin',(-16.5334640646055,45.1212,10.6954737350774));
#66699=CARTESIAN_POINT('',(-16.5845512834741,42.216,10.3781409289644));
#66700=CARTESIAN_POINT('',(-16.5845512834741,41.616,10.3781409289644));
#66701=CARTESIAN_POINT('',(-16.6049,42.216,10.251743065488));
#66702=CARTESIAN_POINT('',(-16.5334640646055,42.216,10.6954737350774));
#66703=CARTESIAN_POINT('',(-16.6049,45.1212,10.251743065488));
#66704=CARTESIAN_POINT('Origin',(-16.6049,45.1212,10.251743065488));
#66705=CARTESIAN_POINT('',(-16.5056105975083,42.216,10.332564502672));
#66706=CARTESIAN_POINT('',(-16.5056105975083,41.616,10.332564502672));
#66707=CARTESIAN_POINT('',(-16.6049,42.216,10.251743065488));
#66708=CARTESIAN_POINT('Origin',(-16.4999,42.216,10.4336084002827));
#66709=CARTESIAN_POINT('Origin',(-17.98,42.216,7.87));
#66710=CARTESIAN_POINT('Origin',(-16.0648018306708,45.1212,10.4013601111256));
#66711=CARTESIAN_POINT('',(-16.1702171833879,42.216,10.097719505839));
#66712=CARTESIAN_POINT('',(-16.1702171833879,41.616,10.097719505839));
#66713=CARTESIAN_POINT('',(-16.2122055158401,42.216,9.97677542746581));
#66714=CARTESIAN_POINT('',(-16.0648018306708,42.216,10.4013601111256));
#66715=CARTESIAN_POINT('',(-16.2122055158401,45.1212,9.97677542746581));
#66716=CARTESIAN_POINT('Origin',(-16.2122055158401,45.1212,9.97677542746581));
#66717=CARTESIAN_POINT('',(-16.1003900471908,42.216,10.0391275816099));
#66718=CARTESIAN_POINT('',(-16.1003900471908,41.616,10.0391275816099));
#66719=CARTESIAN_POINT('',(-16.2122055158401,42.216,9.97677542746581));
#66720=CARTESIAN_POINT('Origin',(-16.0772201178059,42.216,10.1376447605208));
#66721=CARTESIAN_POINT('Origin',(-17.98,42.216,7.87));
#66722=CARTESIAN_POINT('Origin',(-15.6543319239741,45.1212,10.0303323911273));
#66723=CARTESIAN_POINT('',(-15.8108724183901,42.216,9.74960995280916));
#66724=CARTESIAN_POINT('',(-15.8108724183901,41.616,9.74960995280916));
#66725=CARTESIAN_POINT('',(-15.8732245725342,42.216,9.63779448415992));
#66726=CARTESIAN_POINT('',(-15.6543319239741,42.216,10.0303323911273));
#66727=CARTESIAN_POINT('',(-15.8732245725342,45.1212,9.63779448415992));
#66728=CARTESIAN_POINT('Origin',(-15.8732245725342,45.1212,9.63779448415992));
#66729=CARTESIAN_POINT('',(-15.752280494161,42.216,9.67978281661211));
#66730=CARTESIAN_POINT('',(-15.752280494161,41.616,9.67978281661211));
#66731=CARTESIAN_POINT('',(-15.8732245725342,42.216,9.63779448415992));
#66732=CARTESIAN_POINT('Origin',(-15.7123552394792,42.216,9.77277988219409));
#66733=CARTESIAN_POINT('Origin',(-17.98,42.216,7.87));
#66734=CARTESIAN_POINT('Origin',(-15.3145262649226,45.1212,9.59366406460551));
#66735=CARTESIAN_POINT('',(-15.517435497328,42.216,9.34438940249174));
#66736=CARTESIAN_POINT('',(-15.517435497328,41.616,9.34438940249174));
#66737=CARTESIAN_POINT('',(-15.598256934512,42.216,9.2451));
#66738=CARTESIAN_POINT('',(-15.3145262649226,42.216,9.59366406460551));
#66739=CARTESIAN_POINT('',(-15.598256934512,45.1212,9.2451));
#66740=CARTESIAN_POINT('Origin',(-15.598256934512,45.1212,9.2451));
#66741=CARTESIAN_POINT('',(-15.4718590710356,42.216,9.26544871652585));
#66742=CARTESIAN_POINT('',(-15.4718590710356,41.616,9.26544871652585));
#66743=CARTESIAN_POINT('',(-15.598256934512,42.216,9.2451));
#66744=CARTESIAN_POINT('Origin',(-15.4163915997173,42.216,9.3501));
#66745=CARTESIAN_POINT('Origin',(-17.98,42.216,7.87));
#66746=CARTESIAN_POINT('Origin',(-15.0557096765166,45.1212,9.10462307769678));
#66747=CARTESIAN_POINT('',(-15.2988223525619,42.216,8.89437027625664));
#66748=CARTESIAN_POINT('',(-15.2988223525619,41.616,8.89437027625664));
#66749=CARTESIAN_POINT('',(-15.3956573543146,42.216,8.81062379817425));
#66750=CARTESIAN_POINT('',(-15.0557096765166,42.216,9.10462307769678));
#66751=CARTESIAN_POINT('',(-15.3956573543146,45.1212,8.81062379817425));
#66752=CARTESIAN_POINT('Origin',(-15.3956573543146,45.1212,8.81062379817425));
#66753=CARTESIAN_POINT('',(-15.2676462408563,42.216,8.80871461331909));
#66754=CARTESIAN_POINT('',(-15.2676462408563,41.616,8.80871461331909));
#66755=CARTESIAN_POINT('',(-15.3956573543146,42.216,8.81062379817425));
#66756=CARTESIAN_POINT('Origin',(-15.1983219039496,42.216,8.88244802827264));
#66757=CARTESIAN_POINT('Origin',(-17.98,42.216,7.87));
#66758=CARTESIAN_POINT('Origin',(-14.8857461698274,45.1212,8.57806869332165));
#66759=CARTESIAN_POINT('',(-15.1616754338717,42.216,8.41322617753385));
#66760=CARTESIAN_POINT('',(-15.1616754338717,41.616,8.41322617753385));
#66761=CARTESIAN_POINT('',(-15.2715817176658,42.216,8.34756721821959));
#66762=CARTESIAN_POINT('',(-14.8857461698274,42.216,8.57806869332165));
#66763=CARTESIAN_POINT('',(-15.2715817176658,45.1212,8.34756721821959));
#66764=CARTESIAN_POINT('Origin',(-15.2715817176658,45.1212,8.34756721821959));
#66765=CARTESIAN_POINT('',(-15.1458469071313,42.216,8.32345814159914));
#66766=CARTESIAN_POINT('',(-15.1458469071313,41.616,8.32345814159913));
#66767=CARTESIAN_POINT('',(-15.2715817176658,42.216,8.34756721821959));
#66768=CARTESIAN_POINT('Origin',(-15.0647720895333,42.216,8.38403333552965));
#66769=CARTESIAN_POINT('Origin',(-17.98,42.216,7.87));
#66770=CARTESIAN_POINT('Origin',(-14.8098,45.1212,8.03));
#66771=CARTESIAN_POINT('',(-15.1101618809824,42.216,7.91557642629241));
#66772=CARTESIAN_POINT('',(-15.1101618809824,41.616,7.91557642629241));
#66773=CARTESIAN_POINT('',(-15.2298,42.216,7.87));
#66774=CARTESIAN_POINT('',(-14.8098,42.216,8.03));
#66775=CARTESIAN_POINT('',(-15.2298,45.1212,7.87));
#66776=CARTESIAN_POINT('Origin',(-15.2298,45.1212,7.87));
#66777=CARTESIAN_POINT('',(-15.1101618809824,42.216,7.82442357370758));
#66778=CARTESIAN_POINT('',(-15.1101618809824,41.616,7.82442357370758));
#66779=CARTESIAN_POINT('',(-15.2298,42.216,7.87));
#66780=CARTESIAN_POINT('Origin',(-15.0198,42.216,7.87));
#66781=CARTESIAN_POINT('Origin',(-17.98,42.216,7.87));
#66782=CARTESIAN_POINT('Origin',(-17.98,41.616,7.87));
#66783=CARTESIAN_POINT('',(-20.8502,41.616,7.87));
#66784=CARTESIAN_POINT('Origin',(-17.98,45.1212,7.87));
#66785=CARTESIAN_POINT('',(-19.5839512165924,45.1212,7.87));
#66786=CARTESIAN_POINT('',(-18.7819756082962,45.1212,6.4809375));
#66787=CARTESIAN_POINT('',(-19.3834573145184,45.1212,7.522734375));
#66788=CARTESIAN_POINT('',(-17.1780243917038,45.1212,6.4809375));
#66789=CARTESIAN_POINT('',(-18.3809878041481,45.1212,6.4809375));
#66790=CARTESIAN_POINT('',(-16.3760487834076,45.1212,7.87));
#66791=CARTESIAN_POINT('',(-16.9775304896297,45.1212,6.828203125));
#66792=CARTESIAN_POINT('',(-17.1780243917038,45.1212,9.2590625));
#66793=CARTESIAN_POINT('',(-16.5765426854816,45.1212,8.217265625));
#66794=CARTESIAN_POINT('',(-18.7819756082962,45.1212,9.2590625));
#66795=CARTESIAN_POINT('',(-17.5790121958519,45.1212,9.2590625));
#66796=CARTESIAN_POINT('',(-18.9824695103703,45.1212,8.911796875));
#66797=CARTESIAN_POINT('Origin',(-16.3760487834076,43.3212,7.87));
#66798=CARTESIAN_POINT('',(-19.5839512165924,43.3212,7.87));
#66799=CARTESIAN_POINT('',(-18.7819756082962,43.3212,6.4809375));
#66800=CARTESIAN_POINT('',(-19.5839512165924,43.3212,7.87));
#66801=CARTESIAN_POINT('Origin',(-17.98,43.3212,7.87));
#66802=CARTESIAN_POINT('Origin',(-16.3760487834076,43.3212,7.87));
#66803=CARTESIAN_POINT('',(-17.1780243917038,43.3212,6.4809375));
#66804=CARTESIAN_POINT('',(-18.7819756082962,43.3212,6.4809375));
#66805=CARTESIAN_POINT('Origin',(-17.98,43.3212,7.87));
#66806=CARTESIAN_POINT('Origin',(-16.3760487834076,43.3212,7.87));
#66807=CARTESIAN_POINT('',(-16.3760487834076,43.3212,7.87));
#66808=CARTESIAN_POINT('',(-17.1780243917038,43.3212,6.4809375));
#66809=CARTESIAN_POINT('Origin',(-17.98,43.3212,7.87));
#66810=CARTESIAN_POINT('Origin',(-16.3760487834076,43.3212,7.87));
#66811=CARTESIAN_POINT('',(-17.1780243917038,43.3212,9.2590625));
#66812=CARTESIAN_POINT('',(-16.3760487834076,43.3212,7.87));
#66813=CARTESIAN_POINT('Origin',(-17.98,43.3212,7.87));
#66814=CARTESIAN_POINT('Origin',(-16.3760487834076,43.3212,7.87));
#66815=CARTESIAN_POINT('',(-18.7819756082962,43.3212,9.2590625));
#66816=CARTESIAN_POINT('',(-17.1780243917038,43.3212,9.2590625));
#66817=CARTESIAN_POINT('Origin',(-17.98,43.3212,7.87));
#66818=CARTESIAN_POINT('Origin',(-16.3760487834076,43.3212,7.87));
#66819=CARTESIAN_POINT('',(-18.7819756082962,43.3212,9.2590625));
#66820=CARTESIAN_POINT('Origin',(-17.98,43.3212,7.87));
#66821=CARTESIAN_POINT('Origin',(-17.98,43.3212,7.87));
#66822=CARTESIAN_POINT('',(-17.98,42.3574488791083,7.87));
#66823=CARTESIAN_POINT('',(-19.5839512165924,43.3212,7.87));
#66824=CARTESIAN_POINT('Origin',(-19.5839512165924,45.1212,7.87));
#66825=CARTESIAN_POINT('',(-19.5839512165924,45.1212,7.87));
#66826=CARTESIAN_POINT('',(-18.7819756082962,45.1212,6.4809375));
#66827=CARTESIAN_POINT('Origin',(-18.7819756082962,45.1212,9.2590625));
#66828=CARTESIAN_POINT('',(-18.7819756082962,45.1212,9.2590625));
#66829=CARTESIAN_POINT('Origin',(-17.1780243917038,45.1212,9.2590625));
#66830=CARTESIAN_POINT('',(-17.1780243917038,45.1212,9.2590625));
#66831=CARTESIAN_POINT('Origin',(-16.3760487834076,45.1212,7.87));
#66832=CARTESIAN_POINT('',(-16.3760487834076,45.1212,7.87));
#66833=CARTESIAN_POINT('Origin',(-17.1780243917038,45.1212,6.4809375));
#66834=CARTESIAN_POINT('',(-17.1780243917038,45.1212,6.4809375));
#66835=CARTESIAN_POINT('Origin',(-18.7819756082962,45.1212,6.4809375));
#66836=CARTESIAN_POINT('',(0.,0.,0.));
#66837=CARTESIAN_POINT('Origin',(88.011,66.41344859951,12.066));
#66838=CARTESIAN_POINT('',(87.1806428355035,64.3667534988952,13.0269406742195));
#66839=CARTESIAN_POINT('',(87.1806426736235,64.5371153383989,13.0269405343375));
#66840=CARTESIAN_POINT('',(87.1806428354228,66.41344859951,13.0269406741497));
#66841=CARTESIAN_POINT('',(87.2317863635668,64.9396,11.0631410324494));
#66842=CARTESIAN_POINT('Ctrl Pts',(87.1806428355035,64.3667534988952,13.0269406742195));
#66843=CARTESIAN_POINT('Ctrl Pts',(87.1852854866371,64.3673553924107,13.0309524292991));
#66844=CARTESIAN_POINT('Ctrl Pts',(87.1899570974136,64.3679586289739,13.0349304406614));
#66845=CARTESIAN_POINT('Ctrl Pts',(87.2014060533446,64.3694313833721,13.0445373041855));
#66846=CARTESIAN_POINT('Ctrl Pts',(87.2082133282221,64.3703023144596,13.0501296478996));
#66847=CARTESIAN_POINT('Ctrl Pts',(87.2230030283886,64.3721849081683,13.0620241974872));
#66848=CARTESIAN_POINT('Ctrl Pts',(87.2310040091184,64.3731974606554,13.0683021839868));
#66849=CARTESIAN_POINT('Ctrl Pts',(87.2535051205216,64.3760296076747,13.0855251537965));
#66850=CARTESIAN_POINT('Ctrl Pts',(87.2681652799829,64.3778573401527,13.0962555618629));
#66851=CARTESIAN_POINT('Ctrl Pts',(87.3514985479614,64.3881574257102,13.1545474817563));
#66852=CARTESIAN_POINT('Ctrl Pts',(87.4244878535983,64.3968669982924,13.195546313156));
#66853=CARTESIAN_POINT('Ctrl Pts',(87.569344206767,64.4135313761296,13.2590704050229));
#66854=CARTESIAN_POINT('Ctrl Pts',(87.6402549801509,64.421433039703,13.2829747600588));
#66855=CARTESIAN_POINT('Ctrl Pts',(87.7250878854589,64.4303806930004,13.3034620886454));
#66856=CARTESIAN_POINT('Ctrl Pts',(87.7373565607569,64.4316624541041,13.3062328287028));
#66857=CARTESIAN_POINT('Ctrl Pts',(87.7557049422675,64.4335593748953,13.3100910436916));
#66858=CARTESIAN_POINT('Ctrl Pts',(87.761754101863,64.4341815353569,13.3113170598695));
#66859=CARTESIAN_POINT('Ctrl Pts',(87.7726933367175,64.4353005652632,13.3134512682679));
#66860=CARTESIAN_POINT('Ctrl Pts',(87.7775799980215,64.4357982376748,13.3143748788322));
#66861=CARTESIAN_POINT('Ctrl Pts',(87.7886766903221,64.4369234303532,13.3164047859502));
#66862=CARTESIAN_POINT('Ctrl Pts',(87.7948897037884,64.4375499693954,13.3174935592502));
#66863=CARTESIAN_POINT('Ctrl Pts',(87.8141792544465,64.4394852644231,13.3207259357762));
#66864=CARTESIAN_POINT('Ctrl Pts',(87.8272821105822,64.4407857551994,13.3227113302234));
#66865=CARTESIAN_POINT('Ctrl Pts',(87.8585697877915,64.4438631434926,13.3269522980635));
#66866=CARTESIAN_POINT('Ctrl Pts',(87.8767775526825,64.4456316233368,13.3290202322757));
#66867=CARTESIAN_POINT('Ctrl Pts',(87.9482150465085,64.4525065353792,13.3355711924903));
#66868=CARTESIAN_POINT('Ctrl Pts',(88.0016654145285,64.4575140393961,13.3370889092384));
#66869=CARTESIAN_POINT('Ctrl Pts',(88.138142665675,64.4703121658286,13.3323515329334));
#66870=CARTESIAN_POINT('Ctrl Pts',(88.2207313937079,64.4780807532932,13.3213171577363));
#66871=CARTESIAN_POINT('Ctrl Pts',(88.318488572518,64.4877786842529,13.2983352841671));
#66872=CARTESIAN_POINT('Ctrl Pts',(88.3352509548554,64.4894592769705,13.2940312397134));
#66873=CARTESIAN_POINT('Ctrl Pts',(88.36249774422,64.492223952646,13.2864384172987));
#66874=CARTESIAN_POINT('Ctrl Pts',(88.3730371411727,64.4933015117071,13.2833535577206));
#66875=CARTESIAN_POINT('Ctrl Pts',(88.3919711725778,64.495253014305,13.2775439894654));
#66876=CARTESIAN_POINT('Ctrl Pts',(88.4003800499037,64.4961253358192,13.2748676683435));
#66877=CARTESIAN_POINT('Ctrl Pts',(88.4184027938903,64.4980076240898,13.2689239618665));
#66878=CARTESIAN_POINT('Ctrl Pts',(88.4280066465741,64.4990184575209,13.2656284991102));
#66879=CARTESIAN_POINT('Ctrl Pts',(88.4545673556663,64.5018366555625,13.2561569916632));
#66880=CARTESIAN_POINT('Ctrl Pts',(88.4714328152699,64.503652005156,13.2497344299144));
#66881=CARTESIAN_POINT('Ctrl Pts',(88.5418197392397,64.511343116927,13.2211985531459));
#66882=CARTESIAN_POINT('Ctrl Pts',(88.5939235281691,64.5173244337867,13.1958013353278));
#66883=CARTESIAN_POINT('Ctrl Pts',(88.7136434776234,64.5317787459712,13.1269556319073));
#66884=CARTESIAN_POINT('Ctrl Pts',(88.7792349925987,64.540299077164,13.0804700611733));
#66885=CARTESIAN_POINT('Ctrl Pts',(88.8608747796471,64.5515234701443,13.0101249335553));
#66886=CARTESIAN_POINT('Ctrl Pts',(88.8811579420215,64.5543691432288,12.9914645033955));
#66887=CARTESIAN_POINT('Ctrl Pts',(88.906899172118,64.5580419360455,12.9661873482062));
#66888=CARTESIAN_POINT('Ctrl Pts',(88.9129182727707,64.5589053581524,12.9601566038432));
#66889=CARTESIAN_POINT('Ctrl Pts',(88.9225985753985,64.5603009134007,12.9502603517882));
#66890=CARTESIAN_POINT('Ctrl Pts',(88.9262968019798,64.5608357509062,12.9464317694061));
#66891=CARTESIAN_POINT('Ctrl Pts',(88.9335423951454,64.5618867649839,12.9388357822443));
#66892=CARTESIAN_POINT('Ctrl Pts',(88.9370908974795,64.5624029988859,12.9350698623594));
#66893=CARTESIAN_POINT('Ctrl Pts',(88.9460186071812,64.5637059630603,12.9254783718742));
#66894=CARTESIAN_POINT('Ctrl Pts',(88.9513665502599,64.5644903675441,12.9196238226746));
#66895=CARTESIAN_POINT('Ctrl Pts',(88.9731797724281,64.5677080677679,12.8952904349869));
#66896=CARTESIAN_POINT('Ctrl Pts',(88.9891597101199,64.5701089328065,12.8763804110166));
#66897=CARTESIAN_POINT('Ctrl Pts',(89.0331340280854,64.5768876028051,12.8211450009424));
#66898=CARTESIAN_POINT('Ctrl Pts',(89.0597295593094,64.5812022014698,12.7837528607944));
#66899=CARTESIAN_POINT('Ctrl Pts',(89.1356278363609,64.5945113116869,12.6637859247197));
#66900=CARTESIAN_POINT('Ctrl Pts',(89.177617514863,64.6034321586965,12.57701446151));
#66901=CARTESIAN_POINT('Ctrl Pts',(89.2149210778998,64.6143217509405,12.4706607475849));
#66902=CARTESIAN_POINT('Ctrl Pts',(89.2201137877058,64.6159365806313,12.4548702484375));
#66903=CARTESIAN_POINT('Ctrl Pts',(89.2281487666283,64.6186112724524,12.4287178052946));
#66904=CARTESIAN_POINT('Ctrl Pts',(89.2311722262133,64.6196651987894,12.4184131768855));
#66905=CARTESIAN_POINT('Ctrl Pts',(89.2364203523027,64.621585300348,12.3996487061065));
#66906=CARTESIAN_POINT('Ctrl Pts',(89.2386890144655,64.6224499850216,12.3912017419092));
#66907=CARTESIAN_POINT('Ctrl Pts',(89.2434119023822,64.6243284828954,12.3728627872661));
#66908=CARTESIAN_POINT('Ctrl Pts',(89.2458346333304,64.6253432506614,12.362963432144));
#66909=CARTESIAN_POINT('Ctrl Pts',(89.252311789645,64.6282079154989,12.3350466364236));
#66910=CARTESIAN_POINT('Ctrl Pts',(89.2560925171016,64.6300663908075,12.3169692867603));
#66911=CARTESIAN_POINT('Ctrl Pts',(89.2708742965482,64.6382363565111,12.2377022700086));
#66912=CARTESIAN_POINT('Ctrl Pts',(89.2777659347643,64.6446716250192,12.175845641126));
#66913=CARTESIAN_POINT('Ctrl Pts',(89.2837002742137,64.6612263211449,12.0181045687151));
#66914=CARTESIAN_POINT('Ctrl Pts',(89.2764761922883,64.6714249825564,11.9223609554739));
#66915=CARTESIAN_POINT('Ctrl Pts',(89.2562308114717,64.6825175433449,11.8160888547564));
#66916=CARTESIAN_POINT('Ctrl Pts',(89.2537179987655,64.6837880113829,11.8038790886222));
#66917=CARTESIAN_POINT('Ctrl Pts',(89.249701790301,64.6856695553526,11.7857225540153));
#66918=CARTESIAN_POINT('Ctrl Pts',(89.2483345662003,64.6862875366826,11.7797470540538));
#66919=CARTESIAN_POINT('Ctrl Pts',(89.2457828826171,64.6874011236585,11.768954832619));
#66920=CARTESIAN_POINT('Ctrl Pts',(89.2446134402925,64.6878975073301,11.7641349950594));
#66921=CARTESIAN_POINT('Ctrl Pts',(89.2418926014574,64.6890215212784,11.753201043222));
#66922=CARTESIAN_POINT('Ctrl Pts',(89.24032385375,64.6896481597839,11.7470914668708));
#66923=CARTESIAN_POINT('Ctrl Pts',(89.2353181202467,64.6915839388708,11.728182341041));
#66924=CARTESIAN_POINT('Ctrl Pts',(89.2317260841949,64.6928848140655,11.7154240335023));
#66925=CARTESIAN_POINT('Ctrl Pts',(89.222695434177,64.695962359248,11.6851723985457));
#66926=CARTESIAN_POINT('Ctrl Pts',(89.2170766641268,64.697730617066,11.6677354239861));
#66927=CARTESIAN_POINT('Ctrl Pts',(89.1936494975032,64.7045926066705,11.6000833509232));
#66928=CARTESIAN_POINT('Ctrl Pts',(89.1730645993851,64.7095876745403,11.5508833007178));
#66929=CARTESIAN_POINT('Ctrl Pts',(89.1120723102569,64.7224834710716,11.4275245023046));
#66930=CARTESIAN_POINT('Ctrl Pts',(89.067266964979,64.730360227484,11.3558534227431));
#66931=CARTESIAN_POINT('Ctrl Pts',(89.0050631185615,64.7401820398604,11.2754048581576));
#66932=CARTESIAN_POINT('Ctrl Pts',(88.9941496821539,64.7418704040926,11.2618738928168));
#66933=CARTESIAN_POINT('Ctrl Pts',(88.9758654161854,64.7446474986935,11.2401329926345));
#66934=CARTESIAN_POINT('Ctrl Pts',(88.9686589069861,64.7457296563503,11.2317872067827));
#66935=CARTESIAN_POINT('Ctrl Pts',(88.9554689062131,64.7476892246248,11.2169081620566));
#66936=CARTESIAN_POINT('Ctrl Pts',(88.9495238973119,64.7485650029243,11.2103415703415));
#66937=CARTESIAN_POINT('Ctrl Pts',(88.9365933639396,64.7504545244626,11.1963559601061));
#66938=CARTESIAN_POINT('Ctrl Pts',(88.9295863220642,64.751469135291,11.188957820299));
#66939=CARTESIAN_POINT('Ctrl Pts',(88.9098812166861,64.7542976910521,11.1686480657552));
#66940=CARTESIAN_POINT('Ctrl Pts',(88.8969954767106,64.7561196327396,11.1559231545613));
#66941=CARTESIAN_POINT('Ctrl Pts',(88.8410142582401,64.7639246987715,11.10295655043));
#66942=CARTESIAN_POINT('Ctrl Pts',(88.7954240824389,64.770016804994,11.0654737760627));
#66943=CARTESIAN_POINT('Ctrl Pts',(88.6777175811957,64.7851394260122,10.9817012552498));
#66944=CARTESIAN_POINT('Ctrl Pts',(88.6031993351915,64.7942286054061,10.9392718022762));
#66945=CARTESIAN_POINT('Ctrl Pts',(88.5050363255195,64.8053521666606,10.8958274437958));
#66946=CARTESIAN_POINT('Ctrl Pts',(88.484865580124,64.8075947035554,10.8875148254209));
#66947=CARTESIAN_POINT('Ctrl Pts',(88.4572636547063,64.8105975405033,10.8769631709453));
#66948=CARTESIAN_POINT('Ctrl Pts',(88.4500131648125,64.8113802684468,10.8742671094635));
#66949=CARTESIAN_POINT('Ctrl Pts',(88.4380428888494,64.8126621184818,10.8699400945722));
#66950=CARTESIAN_POINT('Ctrl Pts',(88.4333374545993,64.813163377797,10.8682704791849));
#66951=CARTESIAN_POINT('Ctrl Pts',(88.4236492171154,64.8141899110996,10.8648970272056));
#66952=CARTESIAN_POINT('Ctrl Pts',(88.4186654683518,64.8147150036664,10.8631963596466));
#66953=CARTESIAN_POINT('Ctrl Pts',(88.4057209130096,64.8160715520812,10.8588688261711));
#66954=CARTESIAN_POINT('Ctrl Pts',(88.3977442002758,64.8169003621621,10.8562896184672));
#66955=CARTESIAN_POINT('Ctrl Pts',(88.3631872209157,64.8204628278205,10.8454926618706));
#66956=CARTESIAN_POINT('Ctrl Pts',(88.3363635255105,64.8231565930429,10.8380696441756));
#66957=CARTESIAN_POINT('Ctrl Pts',(88.2545472012226,64.8312232903121,10.8182983677254));
#66958=CARTESIAN_POINT('Ctrl Pts',(88.1989545792285,64.8365051180142,10.8087216265665));
#66959=CARTESIAN_POINT('Ctrl Pts',(88.0677429999102,64.8488929218288,10.7950196148503));
#66960=CARTESIAN_POINT('Ctrl Pts',(87.992041432188,64.8559874194276,10.7938958494005));
#66961=CARTESIAN_POINT('Ctrl Pts',(87.8994704204392,64.8649562475728,10.8007887443804));
#66962=CARTESIAN_POINT('Ctrl Pts',(87.8822737119054,64.866634320773,10.802422600144));
#66963=CARTESIAN_POINT('Ctrl Pts',(87.8541600005214,64.8694012170085,10.8056735078812));
#66964=CARTESIAN_POINT('Ctrl Pts',(87.8432208019436,64.8704836923715,10.8070830947309));
#66965=CARTESIAN_POINT('Ctrl Pts',(87.8234756450992,64.8724491168913,10.8098893002345));
#66966=CARTESIAN_POINT('Ctrl Pts',(87.8146632701996,64.8733304823305,10.8112365353676));
#66967=CARTESIAN_POINT('Ctrl Pts',(87.7956818226743,64.875238468276,10.8143432658307));
#66968=CARTESIAN_POINT('Ctrl Pts',(87.78551864641,64.8762660082169,10.8161341508317));
#66969=CARTESIAN_POINT('Ctrl Pts',(87.7571709613859,64.8791496491295,10.8214863750839));
#66970=CARTESIAN_POINT('Ctrl Pts',(87.7390418183201,64.8810141666138,10.8253219601202));
#66971=CARTESIAN_POINT('Ctrl Pts',(87.657840884435,64.8894635397951,10.8443667844751));
#66972=CARTESIAN_POINT('Ctrl Pts',(87.5959188389235,64.8961827836235,10.8639960705532));
#66973=CARTESIAN_POINT('Ctrl Pts',(87.4758157700362,64.9097733715291,10.9124581914677));
#66974=CARTESIAN_POINT('Ctrl Pts',(87.4177898419301,64.9166247214548,10.9411966759536));
#66975=CARTESIAN_POINT('Ctrl Pts',(87.361856214396,64.9234340157367,10.9744357508572));
#66976=CARTESIAN_POINT('Ctrl Pts',(87.3615077575042,64.9234764445663,10.9746430504489));
#66977=CARTESIAN_POINT('Ctrl Pts',(87.3608474851119,64.9235568559819,10.9750362796211));
#66978=CARTESIAN_POINT('Ctrl Pts',(87.360535650008,64.9235948393556,10.9752221760651));
#66979=CARTESIAN_POINT('Ctrl Pts',(87.3599449971576,64.9236667966063,10.9755746294431));
#66980=CARTESIAN_POINT('Ctrl Pts',(87.359666163549,64.923700771128,10.9757411596439));
#66981=CARTESIAN_POINT('Ctrl Pts',(87.3436980245512,64.9256467060782,10.9852862610969));
#66982=CARTESIAN_POINT('Ctrl Pts',(87.3282119847719,64.9275502272988,10.9950029322982));
#66983=CARTESIAN_POINT('Ctrl Pts',(87.2968854250589,64.9314282561891,11.0156144920826));
#66984=CARTESIAN_POINT('Ctrl Pts',(87.2810709406688,64.9334009634589,11.0265419450587));
#66985=CARTESIAN_POINT('Ctrl Pts',(87.259586424246,64.9360962148432,11.042119558274));
#66986=CARTESIAN_POINT('Ctrl Pts',(87.2537006150598,64.9368362177496,11.0464652179827));
#66987=CARTESIAN_POINT('Ctrl Pts',(87.2438435312091,64.9380778590066,11.053875449143));
#66988=CARTESIAN_POINT('Ctrl Pts',(87.2398523847873,64.9385812585839,11.0569130300643));
#66989=CARTESIAN_POINT('Ctrl Pts',(87.2345127837759,64.9392555174034,11.0610270757134));
#66990=CARTESIAN_POINT('Ctrl Pts',(87.2331485041146,64.9394278609354,11.0620826598129));
#66991=CARTESIAN_POINT('Ctrl Pts',(87.2317863635668,64.9396,11.0631410324494));
#66992=CARTESIAN_POINT('',(88.8007982854172,64.9396,11.0714555473222));
#66993=CARTESIAN_POINT('Origin',(88.011,64.9396,12.066));
#66994=CARTESIAN_POINT('Ctrl Pts',(88.8007982854172,64.9395999999999,11.0714555473223));
#66995=CARTESIAN_POINT('Ctrl Pts',(88.8039625986033,64.9391980619403,11.0739684255774));
#66996=CARTESIAN_POINT('Ctrl Pts',(88.807114965516,64.9387969694434,11.0764964424272));
#66997=CARTESIAN_POINT('Ctrl Pts',(88.8140395431263,64.9379143035852,11.0821040683382));
#66998=CARTESIAN_POINT('Ctrl Pts',(88.8178062392383,64.9374331007555,11.0851904330235));
#66999=CARTESIAN_POINT('Ctrl Pts',(88.8300347641081,64.9358670524407,11.0953283879135));
#67000=CARTESIAN_POINT('Ctrl Pts',(88.8384229311932,64.9347867845429,11.1024686622547));
#67001=CARTESIAN_POINT('Ctrl Pts',(88.888433394735,64.9283022879217,11.1461739696863));
#67002=CARTESIAN_POINT('Ctrl Pts',(88.9277244303466,64.9230205582054,11.1853257428775));
#67003=CARTESIAN_POINT('Ctrl Pts',(88.9966091156371,64.9131116344935,11.2635907108737));
#67004=CARTESIAN_POINT('Ctrl Pts',(89.0267385508018,64.9084894206371,11.3020883485947));
#67005=CARTESIAN_POINT('Ctrl Pts',(89.0788693959558,64.899751525597,11.3772532037377));
#67006=CARTESIAN_POINT('Ctrl Pts',(89.1013819878381,64.8956521897241,11.4134790096461));
#67007=CARTESIAN_POINT('Ctrl Pts',(89.1275212597907,64.8903904022928,11.460682883441));
#67008=CARTESIAN_POINT('Ctrl Pts',(89.1328802420769,64.8892811253686,11.4706738370152));
#67009=CARTESIAN_POINT('Ctrl Pts',(89.1431190956893,64.8870991070607,11.4903918383416));
#67010=CARTESIAN_POINT('Ctrl Pts',(89.1480091230171,64.8860267819946,11.5001125196342));
#67011=CARTESIAN_POINT('Ctrl Pts',(89.1571032641745,64.8839724046135,11.5187842450845));
#67012=CARTESIAN_POINT('Ctrl Pts',(89.1613289357173,64.8829911132916,11.5277239542659));
#67013=CARTESIAN_POINT('Ctrl Pts',(89.1707618003447,64.8807371473299,11.5482983169384));
#67014=CARTESIAN_POINT('Ctrl Pts',(89.1758989774433,64.8794623851442,11.5599636275386));
#67015=CARTESIAN_POINT('Ctrl Pts',(89.1920641457929,64.8752897819886,11.5982220136997));
#67016=CARTESIAN_POINT('Ctrl Pts',(89.2023627202778,64.8723697190078,11.6251107815787));
#67017=CARTESIAN_POINT('Ctrl Pts',(89.2438264385035,64.8593312699377,11.745463462886));
#67018=CARTESIAN_POINT('Ctrl Pts',(89.2649621009981,64.8489203306577,11.8420015420369));
#67019=CARTESIAN_POINT('Ctrl Pts',(89.2791066873026,64.8338201746025,11.9838497602535));
#67020=CARTESIAN_POINT('Ctrl Pts',(89.2811942927401,64.8291623636649,12.0279162525263));
#67021=CARTESIAN_POINT('Ctrl Pts',(89.2809071201598,64.8228380985561,12.0886438597775));
#67022=CARTESIAN_POINT('Ctrl Pts',(89.2805014705874,64.8211154897322,12.1052802182264));
#67023=CARTESIAN_POINT('Ctrl Pts',(89.2792396040871,64.8181713908366,12.133918399802));
#67024=CARTESIAN_POINT('Ctrl Pts',(89.2785396304068,64.8169435713111,12.1459245040709));
#67025=CARTESIAN_POINT('Ctrl Pts',(89.2773022474209,64.8152103426091,12.1629758640275));
#67026=CARTESIAN_POINT('Ctrl Pts',(89.2769050443221,64.8146979220926,12.1680300055463));
#67027=CARTESIAN_POINT('Ctrl Pts',(89.2760520860028,64.8136787199122,12.178110147181));
#67028=CARTESIAN_POINT('Ctrl Pts',(89.2755966175181,64.8131719310478,12.1831360907898));
#67029=CARTESIAN_POINT('Ctrl Pts',(89.2745854028635,64.8121198285345,12.1936001913951));
#67030=CARTESIAN_POINT('Ctrl Pts',(89.2740244867495,64.81157485627,12.199037693705));
#67031=CARTESIAN_POINT('Ctrl Pts',(89.2723699609018,64.8100674305017,12.214121806448));
#67032=CARTESIAN_POINT('Ctrl Pts',(89.2712007769097,64.8091091899186,12.2237601718485));
#67033=CARTESIAN_POINT('Ctrl Pts',(89.2625600995788,64.8026753318308,12.288747761552));
#67034=CARTESIAN_POINT('Ctrl Pts',(89.2515535359822,64.797379371364,12.3435764336325));
#67035=CARTESIAN_POINT('Ctrl Pts',(89.2173790373507,64.7850756757847,12.4699576146926));
#67036=CARTESIAN_POINT('Ctrl Pts',(89.1914071549365,64.778123376064,12.5405215551405));
#67037=CARTESIAN_POINT('Ctrl Pts',(89.1479534032458,64.7684804319102,12.6325245258898));
#67038=CARTESIAN_POINT('Ctrl Pts',(89.1357912896725,64.7659331657174,12.6563028289485));
#67039=CARTESIAN_POINT('Ctrl Pts',(89.1130760809626,64.7614061004957,12.6974592401371));
#67040=CARTESIAN_POINT('Ctrl Pts',(89.10283809079,64.7594371464347,12.7150007176854));
#67041=CARTESIAN_POINT('Ctrl Pts',(89.0867791158788,64.7564459019296,12.7410595924762));
#67042=CARTESIAN_POINT('Ctrl Pts',(89.0812672557742,64.7554351946831,12.7497646852751));
#67043=CARTESIAN_POINT('Ctrl Pts',(89.0710750047924,64.7535938658215,12.7654364943452));
#67044=CARTESIAN_POINT('Ctrl Pts',(89.0664302414056,64.7527646555366,12.7724258078832));
#67045=CARTESIAN_POINT('Ctrl Pts',(89.0562308865529,64.7509644846309,12.7874483867613));
#67046=CARTESIAN_POINT('Ctrl Pts',(89.0506522631417,64.7499926196978,12.7954645559896));
#67047=CARTESIAN_POINT('Ctrl Pts',(89.0350375505561,64.7473061063133,12.8173590448606));
#67048=CARTESIAN_POINT('Ctrl Pts',(89.0248127905045,64.7455840077606,12.8310992535981));
#67049=CARTESIAN_POINT('Ctrl Pts',(88.947793396566,64.7328681192317,12.9303439136694));
#67050=CARTESIAN_POINT('Ctrl Pts',(88.8705809318035,64.7214245208296,13.007158332812));
#67051=CARTESIAN_POINT('Ctrl Pts',(88.7508671219386,64.7054423492614,13.0991040290845));
#67052=CARTESIAN_POINT('Ctrl Pts',(88.7158695065866,64.7009527455055,13.123292259264));
#67053=CARTESIAN_POINT('Ctrl Pts',(88.6597216871977,64.6940815401407,13.1580685007915));
#67054=CARTESIAN_POINT('Ctrl Pts',(88.6393791246303,64.6916556127317,13.1698991679731));
#67055=CARTESIAN_POINT('Ctrl Pts',(88.6120799267297,64.6884931444257,13.1847761435283));
#67056=CARTESIAN_POINT('Ctrl Pts',(88.605410101818,64.6877276437395,13.1883340765922));
#67057=CARTESIAN_POINT('Ctrl Pts',(88.5942810453438,64.6864626619759,13.1941436820083));
#67058=CARTESIAN_POINT('Ctrl Pts',(88.5898399292759,64.6859611099252,13.1964288056608));
#67059=CARTESIAN_POINT('Ctrl Pts',(88.5812408133145,64.6849961785841,13.2007894108011));
#67060=CARTESIAN_POINT('Ctrl Pts',(88.5770848653467,64.6845325773918,13.2028682948642));
#67061=CARTESIAN_POINT('Ctrl Pts',(88.567090758041,64.6834240593559,13.2077991433247));
#67062=CARTESIAN_POINT('Ctrl Pts',(88.5612418369229,64.6827804651764,13.2106292598123));
#67063=CARTESIAN_POINT('Ctrl Pts',(88.5394775038795,64.6804036119533,13.2209549763501));
#67064=CARTESIAN_POINT('Ctrl Pts',(88.5234273868804,64.6786862845017,13.2281651149287));
#67065=CARTESIAN_POINT('Ctrl Pts',(88.4042655311097,64.6661549432488,13.278746641844));
#67066=CARTESIAN_POINT('Ctrl Pts',(88.2959622948081,64.6559211468479,13.3086651245138));
#67067=CARTESIAN_POINT('Ctrl Pts',(88.1383241793907,64.6408773546819,13.3304844380366));
#67068=CARTESIAN_POINT('Ctrl Pts',(88.0912041650722,64.6363679741724,13.3343448052624));
#67069=CARTESIAN_POINT('Ctrl Pts',(88.0296166877627,64.6303811616122,13.3359448715109));
#67070=CARTESIAN_POINT('Ctrl Pts',(88.0152448407508,64.6289776846651,13.3360742099973));
#67071=CARTESIAN_POINT('Ctrl Pts',(87.9914222153296,64.6266386624352,13.3358842715739));
#67072=CARTESIAN_POINT('Ctrl Pts',(87.9819713117008,64.6257074331782,13.3357033811669));
#67073=CARTESIAN_POINT('Ctrl Pts',(87.9634625971441,64.6238766820813,13.3351423769161));
#67074=CARTESIAN_POINT('Ctrl Pts',(87.9544050775975,64.6229774769138,13.3347707364097));
#67075=CARTESIAN_POINT('Ctrl Pts',(87.9325271369293,64.6207969824826,13.3336383329156));
#67076=CARTESIAN_POINT('Ctrl Pts',(87.9197130917095,64.6195127721846,13.3327800136501));
#67077=CARTESIAN_POINT('Ctrl Pts',(87.8757942410094,64.6150852001708,13.3291684148847));
#67078=CARTESIAN_POINT('Ctrl Pts',(87.8447821908518,64.6119134679753,13.3254626873137));
#67079=CARTESIAN_POINT('Ctrl Pts',(87.711696870125,64.5980897811447,13.304559434578));
#67080=CARTESIAN_POINT('Ctrl Pts',(87.6118094170502,64.5871259828709,13.2760627817375));
#67081=CARTESIAN_POINT('Ctrl Pts',(87.4832054966514,64.5725363818701,13.2216990499138));
#67082=CARTESIAN_POINT('Ctrl Pts',(87.4505136322956,64.5687878865604,13.2062030772724));
#67083=CARTESIAN_POINT('Ctrl Pts',(87.4105048195553,64.564181695724,13.1851013047375));
#67084=CARTESIAN_POINT('Ctrl Pts',(87.4025309523575,64.5632627367182,13.1807859107637));
#67085=CARTESIAN_POINT('Ctrl Pts',(87.3897790350741,64.5617923480321,13.1737070739876));
#67086=CARTESIAN_POINT('Ctrl Pts',(87.3849718258394,64.5612378623138,13.1709973657771));
#67087=CARTESIAN_POINT('Ctrl Pts',(87.3757019500532,64.5601684873268,13.165692245785));
#67088=CARTESIAN_POINT('Ctrl Pts',(87.3712373837137,64.5596534163888,13.1631009272378));
#67089=CARTESIAN_POINT('Ctrl Pts',(87.3600673889788,64.5583643680578,13.1565262763514));
#67090=CARTESIAN_POINT('Ctrl Pts',(87.3533825560524,64.5575925569061,13.1525082292144));
#67091=CARTESIAN_POINT('Ctrl Pts',(87.3286813955454,64.5547375332339,13.1373496137561));
#67092=CARTESIAN_POINT('Ctrl Pts',(87.3109060796185,64.5526768222063,13.1258194935782));
#67093=CARTESIAN_POINT('Ctrl Pts',(87.2542136235734,64.5460535434991,13.0869961045621));
#67094=CARTESIAN_POINT('Ctrl Pts',(87.2165618611432,64.5415736954848,13.0579786261327));
#67095=CARTESIAN_POINT('Ctrl Pts',(87.1806426736235,64.5371153383989,13.0269405343375));
#67096=CARTESIAN_POINT('Origin',(88.011,66.41344859951,12.066));
#67097=CARTESIAN_POINT('',(87.1806430603713,63.5747053956106,13.0269408685296));
#67098=CARTESIAN_POINT('',(87.1806428353965,63.7449175370261,13.026940674127));
#67099=CARTESIAN_POINT('',(87.1806428354228,66.41344859951,13.0269406741497));
#67100=CARTESIAN_POINT('Ctrl Pts',(87.1806430603713,63.5747053956106,13.0269408685296));
#67101=CARTESIAN_POINT('Ctrl Pts',(87.2131406687874,63.5787450234789,13.0550223203165));
#67102=CARTESIAN_POINT('Ctrl Pts',(87.2470702450564,63.5827579522435,13.0814617222632));
#67103=CARTESIAN_POINT('Ctrl Pts',(87.3191685061318,63.5910193312261,13.1319712231246));
#67104=CARTESIAN_POINT('Ctrl Pts',(87.3573716279986,63.5952604067966,13.1558141030443));
#67105=CARTESIAN_POINT('Ctrl Pts',(87.4145618027948,63.6015073096007,13.1874166523558));
#67106=CARTESIAN_POINT('Ctrl Pts',(87.4325997569936,63.6034634380922,13.196825756598));
#67107=CARTESIAN_POINT('Ctrl Pts',(87.4617680786992,63.606611329425,13.2111603204942));
#67108=CARTESIAN_POINT('Ctrl Pts',(87.472757328571,63.6077939158658,13.2163663181297));
#67109=CARTESIAN_POINT('Ctrl Pts',(87.4938073175145,63.6100542870305,13.2259708015726));
#67110=CARTESIAN_POINT('Ctrl Pts',(87.5038537162376,63.6111310013651,13.2303981963543));
#67111=CARTESIAN_POINT('Ctrl Pts',(87.5142063701444,63.6122389457791,13.2348011650559));
#67112=CARTESIAN_POINT('Ctrl Pts',(87.5144569053705,63.612265757187,13.2349076222169));
#67113=CARTESIAN_POINT('Ctrl Pts',(87.5149878586663,63.6123225759548,13.2351330328213));
#67114=CARTESIAN_POINT('Ctrl Pts',(87.515268285302,63.6123525839926,13.235251965928));
#67115=CARTESIAN_POINT('Ctrl Pts',(87.5158627988254,63.6124161995113,13.2355038556333));
#67116=CARTESIAN_POINT('Ctrl Pts',(87.5161768965165,63.61244980785,13.235636786608));
#67117=CARTESIAN_POINT('Ctrl Pts',(87.5168430341345,63.6125210812403,13.2359183899411));
#67118=CARTESIAN_POINT('Ctrl Pts',(87.5171950875685,63.6125587473646,13.2360670299148));
#67119=CARTESIAN_POINT('Ctrl Pts',(87.5177264607698,63.6126155961416,13.2362910976934));
#67120=CARTESIAN_POINT('Ctrl Pts',(87.5179057312002,63.6126347748571,13.2363666433736));
#67121=CARTESIAN_POINT('Ctrl Pts',(87.5184222444489,63.6126900311517,13.2365841655457));
#67122=CARTESIAN_POINT('Ctrl Pts',(87.5187595310051,63.6127261122261,13.2367260373687));
#67123=CARTESIAN_POINT('Ctrl Pts',(87.5197258433452,63.6128294783682,13.237132002988));
#67124=CARTESIAN_POINT('Ctrl Pts',(87.5203550195716,63.6128967754866,13.2373957352643));
#67125=CARTESIAN_POINT('Ctrl Pts',(87.5261534965033,63.6135169332949,13.2398207959798));
#67126=CARTESIAN_POINT('Ctrl Pts',(87.5313367300346,63.614070915077,13.2419483568284));
#67127=CARTESIAN_POINT('Ctrl Pts',(87.5455210975899,63.6155860740318,13.2476612314488));
#67128=CARTESIAN_POINT('Ctrl Pts',(87.5545492293514,63.6165495119586,13.2511778580204));
#67129=CARTESIAN_POINT('Ctrl Pts',(87.5784760483602,63.6191011038844,13.2601838735489));
#67130=CARTESIAN_POINT('Ctrl Pts',(87.5934383831394,63.6206949429883,13.2654975322845));
#67131=CARTESIAN_POINT('Ctrl Pts',(87.6760588885035,63.6294912798135,13.2931059347143));
#67132=CARTESIAN_POINT('Ctrl Pts',(87.7453860665709,63.6368661139339,13.3099531291621));
#67133=CARTESIAN_POINT('Ctrl Pts',(87.8727567295861,63.650400179432,13.3297712955638));
#67134=CARTESIAN_POINT('Ctrl Pts',(87.9303064327199,63.6565068025264,13.3347464607807));
#67135=CARTESIAN_POINT('Ctrl Pts',(88.0145442374373,63.6653388672667,13.3362726264008));
#67136=CARTESIAN_POINT('Ctrl Pts',(88.0411046007869,63.6681074788489,13.3359208867717));
#67137=CARTESIAN_POINT('Ctrl Pts',(88.0849473249219,63.67263481569,13.3339637432382));
#67138=CARTESIAN_POINT('Ctrl Pts',(88.1022420391561,63.6744096520455,13.3328367125123));
#67139=CARTESIAN_POINT('Ctrl Pts',(88.1264742161432,63.6768765519549,13.3307586987851));
#67140=CARTESIAN_POINT('Ctrl Pts',(88.1334339497509,63.677582760264,13.3301039502309));
#67141=CARTESIAN_POINT('Ctrl Pts',(88.1453886095671,63.6787914641302,13.3288796331493));
#67142=CARTESIAN_POINT('Ctrl Pts',(88.1503860853758,63.6792954282006,13.3283378272539));
#67143=CARTESIAN_POINT('Ctrl Pts',(88.1610247368387,63.6803653614817,13.3271204751063));
#67144=CARTESIAN_POINT('Ctrl Pts',(88.1666647672518,63.6809308743539,13.3264367335511));
#67145=CARTESIAN_POINT('Ctrl Pts',(88.1821320602516,63.6824775553295,13.3244562240559));
#67146=CARTESIAN_POINT('Ctrl Pts',(88.1919493816631,63.6834546075764,13.3230821745321));
#67147=CARTESIAN_POINT('Ctrl Pts',(88.2637504602322,63.6905734878149,13.3121741296016));
#67148=CARTESIAN_POINT('Ctrl Pts',(88.3249808159283,63.6964983989757,13.2981736686667));
#67149=CARTESIAN_POINT('Ctrl Pts',(88.4319229477739,63.7070055514274,13.2652252342958));
#67150=CARTESIAN_POINT('Ctrl Pts',(88.4780285434595,63.7115915937569,13.2480328108368));
#67151=CARTESIAN_POINT('Ctrl Pts',(88.5575036850467,63.7197682114682,13.2130194248616));
#67152=CARTESIAN_POINT('Ctrl Pts',(88.5912901466401,63.7233364198879,13.1963020546574));
#67153=CARTESIAN_POINT('Ctrl Pts',(88.6473480786777,63.7294743352627,13.1653884758522));
#67154=CARTESIAN_POINT('Ctrl Pts',(88.6700117397826,63.7320197742271,13.1519545101977));
#67155=CARTESIAN_POINT('Ctrl Pts',(88.7021055914414,63.7357311203229,13.1315560617776));
#67156=CARTESIAN_POINT('Ctrl Pts',(88.7118841132616,63.7368767353092,13.1251497046399));
#67157=CARTESIAN_POINT('Ctrl Pts',(88.7289375286381,63.7389020713695,13.1136376612935));
#67158=CARTESIAN_POINT('Ctrl Pts',(88.7362500123025,63.7397796181008,13.1085887846743));
#67159=CARTESIAN_POINT('Ctrl Pts',(88.7514421101462,63.7416224181797,13.0978622956034));
#67160=CARTESIAN_POINT('Ctrl Pts',(88.759310737603,63.7425881794204,13.0921702305799));
#67161=CARTESIAN_POINT('Ctrl Pts',(88.7799557338921,63.7451528968482,13.0768721867402));
#67162=CARTESIAN_POINT('Ctrl Pts',(88.7926168405301,63.746757644709,13.067114655407));
#67163=CARTESIAN_POINT('Ctrl Pts',(88.8614207666623,63.7556615716778,13.0119887216614));
#67164=CARTESIAN_POINT('Ctrl Pts',(88.9137883536432,63.7631378547537,12.9621466423837));
#67165=CARTESIAN_POINT('Ctrl Pts',(88.9967866777995,63.7762839455562,12.8684558517146));
#67166=CARTESIAN_POINT('Ctrl Pts',(89.0294222183898,63.7818916109602,12.8266095438839));
#67167=CARTESIAN_POINT('Ctrl Pts',(89.0833411475737,63.7919186993168,12.747756198595));
#67168=CARTESIAN_POINT('Ctrl Pts',(89.1055621633078,63.7963467421912,12.7114779573518));
#67169=CARTESIAN_POINT('Ctrl Pts',(89.1303948830462,63.8016349441104,12.6659518835218));
#67170=CARTESIAN_POINT('Ctrl Pts',(89.1347753651175,63.8025823922271,12.6577061046064));
#67171=CARTESIAN_POINT('Ctrl Pts',(89.141591311496,63.8040795125435,12.6445270399634));
#67172=CARTESIAN_POINT('Ctrl Pts',(89.1440862110694,63.8046326243585,12.6396252192228));
#67173=CARTESIAN_POINT('Ctrl Pts',(89.148804906487,63.8056884558851,12.6302033033459));
#67174=CARTESIAN_POINT('Ctrl Pts',(89.1510336968047,63.8061914410068,12.6256861128039));
#67175=CARTESIAN_POINT('Ctrl Pts',(89.1564553745613,63.8074259352643,12.6145309802248));
#67176=CARTESIAN_POINT('Ctrl Pts',(89.1596175336583,63.8081555802353,12.6078782357836));
#67177=CARTESIAN_POINT('Ctrl Pts',(89.1705303452844,63.8107095262049,12.5843943637716));
#67178=CARTESIAN_POINT('Ctrl Pts',(89.1779709683628,63.8125166856189,12.5674202086316));
#67179=CARTESIAN_POINT('Ctrl Pts',(89.2149290597154,63.8218875464834,12.4778242807444));
#67180=CARTESIAN_POINT('Ctrl Pts',(89.2380517197679,63.8291784619634,12.4027377156281));
#67181=CARTESIAN_POINT('Ctrl Pts',(89.2687239892374,63.8432210895852,12.2560815713231));
#67182=CARTESIAN_POINT('Ctrl Pts',(89.2774195744954,63.8499382387509,12.1850778192762));
#67183=CARTESIAN_POINT('Ctrl Pts',(89.280773403647,63.858569533237,12.095897521019));
#67184=CARTESIAN_POINT('Ctrl Pts',(89.2810680787087,63.8603053854848,12.0780564740048));
#67185=CARTESIAN_POINT('Ctrl Pts',(89.2809408342881,63.8630419787497,12.0501167382223));
#67186=CARTESIAN_POINT('Ctrl Pts',(89.2807743705657,63.8640347674062,12.0400185860298));
#67187=CARTESIAN_POINT('Ctrl Pts',(89.2802372105144,63.8659007814367,12.0211164042517));
#67188=CARTESIAN_POINT('Ctrl Pts',(89.2798952802257,63.8667730560387,12.0123120906722));
#67189=CARTESIAN_POINT('Ctrl Pts',(89.2789201780326,63.8687416255734,11.992518109279));
#67190=CARTESIAN_POINT('Ctrl Pts',(89.2782356841114,63.8698394569732,11.981531855538));
#67191=CARTESIAN_POINT('Ctrl Pts',(89.2760985109865,63.8726875656997,11.9531744583774));
#67192=CARTESIAN_POINT('Ctrl Pts',(89.274430884886,63.8744443594351,11.9358225549148));
#67193=CARTESIAN_POINT('Ctrl Pts',(89.2642929771692,63.883298432387,11.8491172907055));
#67194=CARTESIAN_POINT('Ctrl Pts',(89.2504684527016,63.8905557788021,11.7805259593325));
#67195=CARTESIAN_POINT('Ctrl Pts',(89.2133710063105,63.9046046375526,11.6521482022126));
#67196=CARTESIAN_POINT('Ctrl Pts',(89.1910692512142,63.9113611225054,11.5922845371013));
#67197=CARTESIAN_POINT('Ctrl Pts',(89.1580831977303,63.9195780806291,11.5207246663503));
#67198=CARTESIAN_POINT('Ctrl Pts',(89.1515618710104,63.9211358260342,11.5072122768603));
#67199=CARTESIAN_POINT('Ctrl Pts',(89.1367915154864,63.9245195491915,11.4779442115678));
#67200=CARTESIAN_POINT('Ctrl Pts',(89.1284475334855,63.9263414857828,11.4622390629724));
#67201=CARTESIAN_POINT('Ctrl Pts',(89.1163336786624,63.9288617477336,11.4405503338875));
#67202=CARTESIAN_POINT('Ctrl Pts',(89.1128401677556,63.9295750147433,11.4344162135768));
#67203=CARTESIAN_POINT('Ctrl Pts',(89.1067666915956,63.9307917735312,11.4239558249729));
#67204=CARTESIAN_POINT('Ctrl Pts',(89.1042118665007,63.9312967883145,11.419615296589));
#67205=CARTESIAN_POINT('Ctrl Pts',(89.0987379192445,63.9323644014166,11.4104406170507));
#67206=CARTESIAN_POINT('Ctrl Pts',(89.0958122914753,63.9329265752029,11.4056105827813));
#67207=CARTESIAN_POINT('Ctrl Pts',(89.087606889162,63.9344806576538,11.3922656465326));
#67208=CARTESIAN_POINT('Ctrl Pts',(89.0822582334137,63.9354682880542,11.3837931448105));
#67209=CARTESIAN_POINT('Ctrl Pts',(89.0428437867525,63.9425731688896,11.3229658324481));
#67210=CARTESIAN_POINT('Ctrl Pts',(89.005050149669,63.9484753419939,11.273113632677));
#67211=CARTESIAN_POINT('Ctrl Pts',(88.9314862158845,63.95892212194,11.1896533973522));
#67212=CARTESIAN_POINT('Ctrl Pts',(88.8971597717507,63.9634710757743,11.1549571645173));
#67213=CARTESIAN_POINT('Ctrl Pts',(88.8326231080811,63.9716464978133,11.0968322885665));
#67214=CARTESIAN_POINT('Ctrl Pts',(88.8031929807521,63.9752520849876,11.0726317874674));
#67215=CARTESIAN_POINT('Ctrl Pts',(88.7514854356052,63.9814468660623,11.033873201625));
#67216=CARTESIAN_POINT('Ctrl Pts',(88.729756612073,63.9840111564482,11.0186256116557));
#67217=CARTESIAN_POINT('Ctrl Pts',(88.6977655029417,63.9877448704223,10.9976411777459));
#67218=CARTESIAN_POINT('Ctrl Pts',(88.6878749852476,63.9888936480539,10.9913476557364));
#67219=CARTESIAN_POINT('Ctrl Pts',(88.6703329490658,63.9909225798765,10.98052355803));
#67220=CARTESIAN_POINT('Ctrl Pts',(88.6627181664685,63.991800534376,10.9759346509671));
#67221=CARTESIAN_POINT('Ctrl Pts',(88.6466989888236,63.993642208575,10.9665088372009));
#67222=CARTESIAN_POINT('Ctrl Pts',(88.6382861651878,63.9946064225003,10.9616875102278));
#67223=CARTESIAN_POINT('Ctrl Pts',(88.6159236146856,63.9971623295577,10.9492096769612));
#67224=CARTESIAN_POINT('Ctrl Pts',(88.6018843224834,63.9987597422808,10.9417185123187));
#67225=CARTESIAN_POINT('Ctrl Pts',(88.5239249681155,64.007595907638,10.9019840113731));
#67226=CARTESIAN_POINT('Ctrl Pts',(88.4575215763254,64.015008778335,10.874933546742));
#67227=CARTESIAN_POINT('Ctrl Pts',(88.3353996434419,64.0284418570183,10.8368368536491));
#67228=CARTESIAN_POINT('Ctrl Pts',(88.2805336713743,64.0344064140802,10.8236519364154));
#67229=CARTESIAN_POINT('Ctrl Pts',(88.1854269851198,64.0445245098215,10.8073956730959));
#67230=CARTESIAN_POINT('Ctrl Pts',(88.1455763343356,64.0486982698697,10.8025128534222));
#67231=CARTESIAN_POINT('Ctrl Pts',(88.0963745849009,64.0537282366461,10.7988394152524));
#67232=CARTESIAN_POINT('Ctrl Pts',(88.087185548408,64.0546623572592,10.7982537527102));
#67233=CARTESIAN_POINT('Ctrl Pts',(88.0725258385121,64.0561434130099,10.7974793983722));
#67234=CARTESIAN_POINT('Ctrl Pts',(88.067059202746,64.0566936664489,10.7972260581442));
#67235=CARTESIAN_POINT('Ctrl Pts',(88.0565415215797,64.0577482282593,10.7968067496772));
#67236=CARTESIAN_POINT('Ctrl Pts',(88.0514910246063,64.0582527749808,10.7966355858726));
#67237=CARTESIAN_POINT('Ctrl Pts',(88.0389941399391,64.0594969468888,10.796286724085));
#67238=CARTESIAN_POINT('Ctrl Pts',(88.031546874037,64.0602346430776,10.7961443740158));
#67239=CARTESIAN_POINT('Ctrl Pts',(88.0050686975203,64.062845624223,10.7958712703927));
#67240=CARTESIAN_POINT('Ctrl Pts',(87.9860351083321,64.0647007693153,10.7961027353957));
#67241=CARTESIAN_POINT('Ctrl Pts',(87.8891426289245,64.074068813907,10.7994607298161));
#67242=CARTESIAN_POINT('Ctrl Pts',(87.8116747596349,64.0813162683423,10.8093202252663));
#67243=CARTESIAN_POINT('Ctrl Pts',(87.6661522397116,64.0952888852786,10.8416473049455));
#67244=CARTESIAN_POINT('Ctrl Pts',(87.59814434867,64.1019799919406,10.8628760819618));
#67245=CARTESIAN_POINT('Ctrl Pts',(87.515752326902,64.1105834245303,10.8964068828306));
#67246=CARTESIAN_POINT('Ctrl Pts',(87.4993715215902,64.1123191892338,10.9034792292961));
#67247=CARTESIAN_POINT('Ctrl Pts',(87.4739584275012,64.1150558899876,10.9150923627463));
#67248=CARTESIAN_POINT('Ctrl Pts',(87.4648215510081,64.116048880045,10.9194001886641));
#67249=CARTESIAN_POINT('Ctrl Pts',(87.4478100985854,64.1179154340813,10.9276701585964));
#67250=CARTESIAN_POINT('Ctrl Pts',(87.4399234375693,64.1187880483147,10.9316062223438));
#67251=CARTESIAN_POINT('Ctrl Pts',(87.4222754515723,64.1207576157007,10.940644626871));
#67252=CARTESIAN_POINT('Ctrl Pts',(87.4125384038292,64.1218561077368,10.945792426369));
#67253=CARTESIAN_POINT('Ctrl Pts',(87.3875535185791,64.1247064478936,10.9594201928604));
#67254=CARTESIAN_POINT('Ctrl Pts',(87.3724118997576,64.1264648241931,10.9680885529502));
#67255=CARTESIAN_POINT('Ctrl Pts',(87.2923526703218,64.1359352558347,11.0161376721976));
#67256=CARTESIAN_POINT('Ctrl Pts',(87.2309004700675,64.1438392951705,11.0609603375917));
#67257=CARTESIAN_POINT('Ctrl Pts',(87.1195558350058,64.159426540112,11.1585659985002));
#67258=CARTESIAN_POINT('Ctrl Pts',(87.0694328550914,64.1670722357002,11.2106859659522));
#67259=CARTESIAN_POINT('Ctrl Pts',(87.0125524887848,64.1764055149449,11.2809306849819));
#67260=CARTESIAN_POINT('Ctrl Pts',(87.0014031373127,64.1782711863826,11.2953213660597));
#67261=CARTESIAN_POINT('Ctrl Pts',(86.9863260827417,64.1808409420637,11.3156706794672));
#67262=CARTESIAN_POINT('Ctrl Pts',(86.9821341402639,64.1815607220895,11.3214291320676));
#67263=CARTESIAN_POINT('Ctrl Pts',(86.9750555275098,64.1827849341244,11.3313269372816));
#67264=CARTESIAN_POINT('Ctrl Pts',(86.9721447422379,64.1832909401244,11.335448689416));
#67265=CARTESIAN_POINT('Ctrl Pts',(86.9660479020776,64.1843562240845,11.3441921175065));
#67266=CARTESIAN_POINT('Ctrl Pts',(86.9628678130022,64.1849151079535,11.3488177154556));
#67267=CARTESIAN_POINT('Ctrl Pts',(86.9541786192119,64.1864516885805,11.3616378325616));
#67268=CARTESIAN_POINT('Ctrl Pts',(86.9487340464657,64.1874252545805,11.3698760455567));
#67269=CARTESIAN_POINT('Ctrl Pts',(86.9154367951051,64.1934534272418,11.4215588742874));
#67270=CARTESIAN_POINT('Ctrl Pts',(86.89015264914,64.1983627543781,11.4666117561619));
#67271=CARTESIAN_POINT('Ctrl Pts',(86.8197882194496,64.2135934603464,11.612112384576));
#67272=CARTESIAN_POINT('Ctrl Pts',(86.7849715252741,64.2237299871624,11.7169283300702));
#67273=CARTESIAN_POINT('Ctrl Pts',(86.7608576378158,64.2359998639838,11.8416464581302));
#67274=CARTESIAN_POINT('Ctrl Pts',(86.7579598015079,64.2376551876887,11.8584412525019));
#67275=CARTESIAN_POINT('Ctrl Pts',(86.7537654420734,64.2403855686736,11.8860558945803));
#67276=CARTESIAN_POINT('Ctrl Pts',(86.7522686104747,64.2414543339038,11.8968436060929));
#67277=CARTESIAN_POINT('Ctrl Pts',(86.7498137999967,64.2433943952547,11.9163779122075));
#67278=CARTESIAN_POINT('Ctrl Pts',(86.7488076146665,64.2442641204557,11.9251178762813));
#67279=CARTESIAN_POINT('Ctrl Pts',(86.7468339819988,64.2461457436484,11.9439845973359));
#67280=CARTESIAN_POINT('Ctrl Pts',(86.7458972562207,64.2471585426138,11.9541138445864));
#67281=CARTESIAN_POINT('Ctrl Pts',(86.7436229538902,64.2499958695721,11.9824102664751));
#67282=CARTESIAN_POINT('Ctrl Pts',(86.7425544914341,64.2518286100351,12.0005956892039));
#67283=CARTESIAN_POINT('Ctrl Pts',(86.741416161925,64.254930706385,12.0312011137534));
#67284=CARTESIAN_POINT('Ctrl Pts',(86.7411367015634,64.2561934210007,12.0436111484597));
#67285=CARTESIAN_POINT('Ctrl Pts',(86.7407470209236,64.261260659823,12.0932119099433));
#67286=CARTESIAN_POINT('Ctrl Pts',(86.7420885633283,64.2651054950066,12.1303914859789));
#67287=CARTESIAN_POINT('Ctrl Pts',(86.7490159633792,64.2741522994197,12.2168309390463));
#67288=CARTESIAN_POINT('Ctrl Pts',(86.7558582180125,64.2793744861255,12.2659303845996));
#67289=CARTESIAN_POINT('Ctrl Pts',(86.7770006061972,64.2907660866966,12.371892813843));
#67290=CARTESIAN_POINT('Ctrl Pts',(86.7924066335504,64.2969235381556,12.4284319860954));
#67291=CARTESIAN_POINT('Ctrl Pts',(86.8158911199343,64.3042476902289,12.495860700432));
#67292=CARTESIAN_POINT('Ctrl Pts',(86.8203064715159,64.3055592229958,12.5079439152556));
#67293=CARTESIAN_POINT('Ctrl Pts',(86.8271285147874,64.3074905933901,12.5257684228813));
#67294=CARTESIAN_POINT('Ctrl Pts',(86.8293948049736,64.3081178129633,12.5315618812203));
#67295=CARTESIAN_POINT('Ctrl Pts',(86.8335444677901,64.3092406340744,12.5419443989946));
#67296=CARTESIAN_POINT('Ctrl Pts',(86.8354122331139,64.3097370899307,12.5465392874675));
#67297=CARTESIAN_POINT('Ctrl Pts',(86.8396839252235,64.3108527292287,12.5568740906869));
#67298=CARTESIAN_POINT('Ctrl Pts',(86.8421031763912,64.3114709899404,12.562607432181));
#67299=CARTESIAN_POINT('Ctrl Pts',(86.8496508074487,64.3133596780019,12.5801336546242));
#67300=CARTESIAN_POINT('Ctrl Pts',(86.8549164975763,64.3146223560553,12.5918672303559));
#67301=CARTESIAN_POINT('Ctrl Pts',(86.8678122273157,64.3175938133118,12.6194724442524));
#67302=CARTESIAN_POINT('Ctrl Pts',(86.8755960979228,64.319294897505,12.6352697992552));
#67303=CARTESIAN_POINT('Ctrl Pts',(86.9066028202,64.3257530716487,12.6950297471398));
#67304=CARTESIAN_POINT('Ctrl Pts',(86.9320729482213,64.3304228446853,12.7377804872196));
#67305=CARTESIAN_POINT('Ctrl Pts',(87.0100279385388,64.3434392160269,12.8527027482771));
#67306=CARTESIAN_POINT('Ctrl Pts',(87.0676889060196,64.3517446021911,12.920989561554));
#67307=CARTESIAN_POINT('Ctrl Pts',(87.1443847984837,64.3620077360665,12.9945320065046));
#67308=CARTESIAN_POINT('Ctrl Pts',(87.1569903905394,64.3636719752522,13.0061388811433));
#67309=CARTESIAN_POINT('Ctrl Pts',(87.1734140123514,64.3658148539388,13.0206583922605));
#67310=CARTESIAN_POINT('Ctrl Pts',(87.1770196048446,64.3662837674904,13.0238098092067));
#67311=CARTESIAN_POINT('Ctrl Pts',(87.1806428355035,64.3667534988952,13.0269406742195));
#67312=CARTESIAN_POINT('Ctrl Pts',(87.1806426736235,64.5371153383989,13.0269405343375));
#67313=CARTESIAN_POINT('Ctrl Pts',(87.1514263005812,64.5334889472477,13.0016944045938));
#67314=CARTESIAN_POINT('Ctrl Pts',(87.1233561873418,64.5298768299862,12.9751114426022));
#67315=CARTESIAN_POINT('Ctrl Pts',(87.0555201547087,64.520689310057,12.9047193089426));
#67316=CARTESIAN_POINT('Ctrl Pts',(87.0175412458783,64.5150997030018,12.8593661369084));
#67317=CARTESIAN_POINT('Ctrl Pts',(86.9722199431844,64.5076327208031,12.7968656124822));
#67318=CARTESIAN_POINT('Ctrl Pts',(86.9618953341684,64.5058692079263,12.7819663901448));
#67319=CARTESIAN_POINT('Ctrl Pts',(86.9462692331873,64.5030954847935,12.7583527064121));
#67320=CARTESIAN_POINT('Ctrl Pts',(86.940747507997,64.5020934835451,12.7497861247048));
#67321=CARTESIAN_POINT('Ctrl Pts',(86.9306218333549,64.500213673722,12.7336536829499));
#67322=CARTESIAN_POINT('Ctrl Pts',(86.9259927259231,64.4993368519204,12.7261042557688));
#67323=CARTESIAN_POINT('Ctrl Pts',(86.9157821177259,64.4973625108793,12.7090545781324));
#67324=CARTESIAN_POINT('Ctrl Pts',(86.9102446307748,64.4962634838933,12.699529003006));
#67325=CARTESIAN_POINT('Ctrl Pts',(86.8963042190765,64.4934213174479,12.6748141086086));
#67326=CARTESIAN_POINT('Ctrl Pts',(86.8880878587672,64.4916717900589,12.6595229986332));
#67327=CARTESIAN_POINT('Ctrl Pts',(86.8414170612262,64.4812720287656,12.5682261513557));
#67328=CARTESIAN_POINT('Ctrl Pts',(86.8103837221789,64.4723754689405,12.4886929163256));
#67329=CARTESIAN_POINT('Ctrl Pts',(86.7734118987346,64.4578459449939,12.3559167338631));
#67330=CARTESIAN_POINT('Ctrl Pts',(86.7624499871806,64.4522803861895,12.3043265477575));
#67331=CARTESIAN_POINT('Ctrl Pts',(86.750783559761,64.4439984807312,12.2256148972025));
#67332=CARTESIAN_POINT('Ctrl Pts',(86.7476874389326,64.4412245571559,12.198906378796));
#67333=CARTESIAN_POINT('Ctrl Pts',(86.7447559369753,64.437655009817,12.1639449816109));
#67334=CARTESIAN_POINT('Ctrl Pts',(86.7441498706048,64.4368243646672,12.1557664147302));
#67335=CARTESIAN_POINT('Ctrl Pts',(86.7432849708381,64.4354674845392,12.1423302170906));
#67336=CARTESIAN_POINT('Ctrl Pts',(86.742979536059,64.4349388244294,12.1370760437235));
#67337=CARTESIAN_POINT('Ctrl Pts',(86.7424668449186,64.4339486386881,12.1271969304457));
#67338=CARTESIAN_POINT('Ctrl Pts',(86.7422521997091,64.4334867148656,12.1225725299884));
#67339=CARTESIAN_POINT('Ctrl Pts',(86.7417993822429,64.432385373132,12.1115113038061));
#67340=CARTESIAN_POINT('Ctrl Pts',(86.7415848767882,64.4317472441949,12.1050734993737));
#67341=CARTESIAN_POINT('Ctrl Pts',(86.7409779219114,64.4294162429925,12.081460824189));
#67342=CARTESIAN_POINT('Ctrl Pts',(86.7408849428629,64.4277385608864,12.06427883881));
#67343=CARTESIAN_POINT('Ctrl Pts',(86.7423247799866,64.4183688303657,11.9675449801144));
#67344=CARTESIAN_POINT('Ctrl Pts',(86.7509822654883,64.4109701511084,11.8882651688358));
#67345=CARTESIAN_POINT('Ctrl Pts',(86.7772020010118,64.3987688622362,11.7607016800924));
#67346=CARTESIAN_POINT('Ctrl Pts',(86.7903547609049,64.3940139219809,11.711755732834));
#67347=CARTESIAN_POINT('Ctrl Pts',(86.8133028262411,64.3871017878831,11.6430373958035));
#67348=CARTESIAN_POINT('Ctrl Pts',(86.8207441553494,64.3850079878521,11.6225287045076));
#67349=CARTESIAN_POINT('Ctrl Pts',(86.8351245368275,64.3811989508431,11.5858692952538));
#67350=CARTESIAN_POINT('Ctrl Pts',(86.841877851755,64.3794897971484,11.5696514040103));
#67351=CARTESIAN_POINT('Ctrl Pts',(86.8530016746293,64.3767894878367,11.544425486218));
#67352=CARTESIAN_POINT('Ctrl Pts',(86.8571462798581,64.3758060336757,11.5353196128981));
#67353=CARTESIAN_POINT('Ctrl Pts',(86.8651212212295,64.3739543670005,11.5183335140868));
#67354=CARTESIAN_POINT('Ctrl Pts',(86.868926397684,64.3730870707836,11.510442052974));
#67355=CARTESIAN_POINT('Ctrl Pts',(86.8776864510072,64.3711256887929,11.4927451794826));
#67356=CARTESIAN_POINT('Ctrl Pts',(86.8826874526101,64.3700300422996,11.4829635814334));
#67357=CARTESIAN_POINT('Ctrl Pts',(86.8959700102513,64.3671798752017,11.4577948970307));
#67358=CARTESIAN_POINT('Ctrl Pts',(86.9044430240218,64.365418727724,11.4425123048997));
#67359=CARTESIAN_POINT('Ctrl Pts',(86.9482963189253,64.3565721187751,11.3671260004022));
#67360=CARTESIAN_POINT('Ctrl Pts',(86.9882629789643,64.3493262275239,11.3098458963732));
#67361=CARTESIAN_POINT('Ctrl Pts',(87.0737872774044,64.3352207541863,11.2065349647267));
#67362=CARTESIAN_POINT('Ctrl Pts',(87.1185710934398,64.3283950668457,11.1601198158045));
#67363=CARTESIAN_POINT('Ctrl Pts',(87.1779501565983,64.3201025460595,11.107274056901));
#67364=CARTESIAN_POINT('Ctrl Pts',(87.1893950954753,64.3185358901248,11.0974480361107));
#67365=CARTESIAN_POINT('Ctrl Pts',(87.2147417733791,64.3151383816756,11.0764594226154));
#67366=CARTESIAN_POINT('Ctrl Pts',(87.228709638359,64.3133115679607,11.0653803809104));
#67367=CARTESIAN_POINT('Ctrl Pts',(87.2485109415623,64.3107888646646,11.0503426042845));
#67368=CARTESIAN_POINT('Ctrl Pts',(87.2541500286295,64.3100778106454,11.046133519007));
#67369=CARTESIAN_POINT('Ctrl Pts',(87.2638668210019,64.3088655030661,11.0390057685277));
#67370=CARTESIAN_POINT('Ctrl Pts',(87.2679272365382,64.3083627275558,11.0360640741105));
#67371=CARTESIAN_POINT('Ctrl Pts',(87.2765830441093,64.307299088083,11.0298709445926));
#67372=CARTESIAN_POINT('Ctrl Pts',(87.2811827549543,64.3067386508385,11.0266259201193));
#67373=CARTESIAN_POINT('Ctrl Pts',(87.2939613869813,64.3051943522894,11.0177374546552));
#67374=CARTESIAN_POINT('Ctrl Pts',(87.3021854954923,64.3042146820836,11.0121590455435));
#67375=CARTESIAN_POINT('Ctrl Pts',(87.3577438948443,64.2976844325905,10.9754185235902));
#67376=CARTESIAN_POINT('Ctrl Pts',(87.4070617320362,64.2923099975984,10.947352367846));
#67377=CARTESIAN_POINT('Ctrl Pts',(87.5449283615138,64.2779050190931,10.8806816027452));
#67378=CARTESIAN_POINT('Ctrl Pts',(87.6362494195677,64.2689811858377,10.8487233620262));
#67379=CARTESIAN_POINT('Ctrl Pts',(87.7538994904113,64.2573918041214,10.8220608064475));
#67380=CARTESIAN_POINT('Ctrl Pts',(87.7776420349127,64.2550501793617,10.8173890634394));
#67381=CARTESIAN_POINT('Ctrl Pts',(87.8126797724498,64.2515805649232,10.8115289837774));
#67382=CARTESIAN_POINT('Ctrl Pts',(87.8238818593748,64.2504692202658,10.8098092404708));
#67383=CARTESIAN_POINT('Ctrl Pts',(87.8438741424197,64.2484811519999,10.8070133642217));
#67384=CARTESIAN_POINT('Ctrl Pts',(87.852655559775,64.24760631994,10.8058788036133));
#67385=CARTESIAN_POINT('Ctrl Pts',(87.8713008731174,64.2457449509016,10.803667792833));
#67386=CARTESIAN_POINT('Ctrl Pts',(87.8811668882946,64.2447577357528,10.8026149454319));
#67387=CARTESIAN_POINT('Ctrl Pts',(87.9079082817935,64.24207499275,10.8000777803914));
#67388=CARTESIAN_POINT('Ctrl Pts',(87.9248019299921,64.2403727035484,10.7988154080409));
#67389=CARTESIAN_POINT('Ctrl Pts',(87.9624560215783,64.2365595105638,10.7967581133915));
#67390=CARTESIAN_POINT('Ctrl Pts',(87.9832204017704,64.2344438891176,10.7961340017414));
#67391=CARTESIAN_POINT('Ctrl Pts',(88.0505643823638,64.2275374953974,10.7957622405441));
#67392=CARTESIAN_POINT('Ctrl Pts',(88.0971121437529,64.2226925271662,10.7980674618984));
#67393=CARTESIAN_POINT('Ctrl Pts',(88.212385563456,64.2105326762894,10.810152861959));
#67394=CARTESIAN_POINT('Ctrl Pts',(88.2806403414343,64.203183458623,10.8230187250191));
#67395=CARTESIAN_POINT('Ctrl Pts',(88.3762349272313,64.192843860975,10.8492867123143));
#67396=CARTESIAN_POINT('Ctrl Pts',(88.4046824910195,64.1897621955934,10.8581911115611));
#67397=CARTESIAN_POINT('Ctrl Pts',(88.4410479720605,64.1858357329378,10.870995681333));
#67398=CARTESIAN_POINT('Ctrl Pts',(88.4492723947148,64.1849486128141,10.8739874566524));
#67399=CARTESIAN_POINT('Ctrl Pts',(88.4625046643305,64.1835234340543,10.8789563991309));
#67400=CARTESIAN_POINT('Ctrl Pts',(88.4675317771834,64.1829824859203,10.8808807179496));
#67401=CARTESIAN_POINT('Ctrl Pts',(88.4773747750737,64.1819244884297,10.8847204280945));
#67402=CARTESIAN_POINT('Ctrl Pts',(88.4821914062006,64.1814073319472,10.8866334246328));
#67403=CARTESIAN_POINT('Ctrl Pts',(88.4942658639066,64.1801120120324,10.8915147561668));
#67404=CARTESIAN_POINT('Ctrl Pts',(88.5015083794349,64.1793360539418,10.8945210098232));
#67405=CARTESIAN_POINT('Ctrl Pts',(88.5304822005445,64.1762339300989,10.9068634135562));
#67406=CARTESIAN_POINT('Ctrl Pts',(88.5519807807032,64.1739369425836,10.9167396158973));
#67407=CARTESIAN_POINT('Ctrl Pts',(88.639162269327,64.164588055302,10.9597790894026));
#67408=CARTESIAN_POINT('Ctrl Pts',(88.7021849870034,64.1577428061385,10.9980212617296));
#67409=CARTESIAN_POINT('Ctrl Pts',(88.8209621084332,64.1439391681884,11.0850381822837));
#67410=CARTESIAN_POINT('Ctrl Pts',(88.8764673917627,64.137005077584,11.1336438677674));
#67411=CARTESIAN_POINT('Ctrl Pts',(88.9384203134823,64.1283279890282,11.1982195158716));
#67412=CARTESIAN_POINT('Ctrl Pts',(88.9491814588237,64.1267823269317,11.2098651372503));
#67413=CARTESIAN_POINT('Ctrl Pts',(88.9661605086323,64.1242776274631,11.2289443127793));
#67414=CARTESIAN_POINT('Ctrl Pts',(88.9725165843419,64.1233244051715,11.2362532519637));
#67415=CARTESIAN_POINT('Ctrl Pts',(88.9845492098895,64.1214889329676,11.250413652914));
#67416=CARTESIAN_POINT('Ctrl Pts',(88.9902386054785,64.1206072768338,11.2572535026833));
#67417=CARTESIAN_POINT('Ctrl Pts',(89.0032769455921,64.1185538724829,11.2732676179831));
#67418=CARTESIAN_POINT('Ctrl Pts',(89.0105711658079,64.1173800261024,11.2824850819217));
#67419=CARTESIAN_POINT('Ctrl Pts',(89.034024988014,64.113520732952,11.3129834961945));
#67420=CARTESIAN_POINT('Ctrl Pts',(89.0496396985808,64.110814688494,11.3346715622391));
#67421=CARTESIAN_POINT('Ctrl Pts',(89.086027981821,64.104153523494,11.3887310349992));
#67422=CARTESIAN_POINT('Ctrl Pts',(89.106036224985,64.1001747616221,11.4215828975474));
#67423=CARTESIAN_POINT('Ctrl Pts',(89.1478112650182,64.0911031729747,11.4977520270928));
#67424=CARTESIAN_POINT('Ctrl Pts',(89.1686513517111,64.0859957755468,11.5415112865018));
#67425=CARTESIAN_POINT('Ctrl Pts',(89.2104674788678,64.0743234168536,11.6440305099637));
#67426=CARTESIAN_POINT('Ctrl Pts',(89.2297223071949,64.0677728430725,11.7033723539282));
#67427=CARTESIAN_POINT('Ctrl Pts',(89.2469263903564,64.0603882417334,11.7736198134119));
#67428=CARTESIAN_POINT('Ctrl Pts',(89.2491928113738,64.0593712872739,11.7833716211018));
#67429=CARTESIAN_POINT('Ctrl Pts',(89.2525565287029,64.057790402386,11.7986626682724));
#67430=CARTESIAN_POINT('Ctrl Pts',(89.2537325319229,64.057222374955,11.8041838019497));
#67431=CARTESIAN_POINT('Ctrl Pts',(89.2558875652958,64.0561517678565,11.8146431029454));
#67432=CARTESIAN_POINT('Ctrl Pts',(89.2568740644978,64.0556488265479,11.8195793083298));
#67433=CARTESIAN_POINT('Ctrl Pts',(89.2591727792289,64.0544448631296,11.831448314691));
#67434=CARTESIAN_POINT('Ctrl Pts',(89.2604566248935,64.0537454275362,11.8383864438066));
#67435=CARTESIAN_POINT('Ctrl Pts',(89.26477182315,64.0512939027927,11.8628440998175));
#67436=CARTESIAN_POINT('Ctrl Pts',(89.2674932823561,64.0495577445784,11.8804175352169));
#67437=CARTESIAN_POINT('Ctrl Pts',(89.2718292319115,64.0463832981692,11.9129158422528));
#67438=CARTESIAN_POINT('Ctrl Pts',(89.2735498741069,64.04494113111,11.9278226503319));
#67439=CARTESIAN_POINT('Ctrl Pts',(89.2811985731855,64.0374073224708,12.0062695105088));
#67440=CARTESIAN_POINT('Ctrl Pts',(89.2825959978206,64.0314586250321,12.0701642807362));
#67441=CARTESIAN_POINT('Ctrl Pts',(89.2754483935195,64.0189303066367,12.2036642181091));
#67442=CARTESIAN_POINT('Ctrl Pts',(89.2659633980586,64.0123635226596,12.2729920673909));
#67443=CARTESIAN_POINT('Ctrl Pts',(89.2470553414833,64.0039384684211,12.3581822357299));
#67444=CARTESIAN_POINT('Ctrl Pts',(89.2429329344428,64.0022476046765,12.3751026403264));
#67445=CARTESIAN_POINT('Ctrl Pts',(89.2356416927185,63.9994710390202,12.402561551866));
#67446=CARTESIAN_POINT('Ctrl Pts',(89.2326813562891,63.998392004269,12.4131535665589));
#67447=CARTESIAN_POINT('Ctrl Pts',(89.2271043923316,63.9964411675885,12.4321524376983));
#67448=CARTESIAN_POINT('Ctrl Pts',(89.2245371501587,63.995571018517,12.4405731917736));
#67449=CARTESIAN_POINT('Ctrl Pts',(89.2188397980792,63.9936972333885,12.458587373693));
#67450=CARTESIAN_POINT('Ctrl Pts',(89.2156824987669,63.9926927606254,12.4681714632859));
#67451=CARTESIAN_POINT('Ctrl Pts',(89.2066325511026,63.9899032026671,12.4945797054699));
#67452=CARTESIAN_POINT('Ctrl Pts',(89.2004996484263,63.9881103511096,12.5113181611129));
#67453=CARTESIAN_POINT('Ctrl Pts',(89.1896312321367,63.9850851977706,12.5391530546905));
#67454=CARTESIAN_POINT('Ctrl Pts',(89.1850859926142,63.9838593386643,12.5503216407021));
#67455=CARTESIAN_POINT('Ctrl Pts',(89.1727458331034,63.9806299811763,12.5794489880605));
#67456=CARTESIAN_POINT('Ctrl Pts',(89.1646937922239,63.9786187057474,12.5972944380734));
#67457=CARTESIAN_POINT('Ctrl Pts',(89.1240535654536,63.9689024317577,12.6820797693294));
#67458=CARTESIAN_POINT('Ctrl Pts',(89.0860369561961,63.9610479965126,12.7462464655865));
#67459=CARTESIAN_POINT('Ctrl Pts',(89.0092613097242,63.9471774561566,12.8531767326428));
#67460=CARTESIAN_POINT('Ctrl Pts',(88.9727879642447,63.941174782896,12.8973475802332));
#67461=CARTESIAN_POINT('Ctrl Pts',(88.926626713661,63.9343183923013,12.9461286217911));
#67462=CARTESIAN_POINT('Ctrl Pts',(88.9197144473054,63.9333094337404,12.9532636278205));
#67463=CARTESIAN_POINT('Ctrl Pts',(88.9087577170494,63.9317384973029,12.9643110387754));
#67464=CARTESIAN_POINT('Ctrl Pts',(88.9047700162786,63.9311724952946,12.9682786728214));
#67465=CARTESIAN_POINT('Ctrl Pts',(88.8971594450982,63.9301032999136,12.9757509778697));
#67466=CARTESIAN_POINT('Ctrl Pts',(88.8935420313433,63.9295997617446,12.9792606247455));
#67467=CARTESIAN_POINT('Ctrl Pts',(88.8847846003723,63.9283916656196,12.9876565313533));
#67468=CARTESIAN_POINT('Ctrl Pts',(88.8796243546938,63.927688721315,12.9925214669654));
#67469=CARTESIAN_POINT('Ctrl Pts',(88.8612230594843,63.925212086356,13.0095808175414));
#67470=CARTESIAN_POINT('Ctrl Pts',(88.8477628096726,63.9234547410478,13.0215376130314));
#67471=CARTESIAN_POINT('Ctrl Pts',(88.8224231326715,63.9202341145056,13.0431006298191));
#67472=CARTESIAN_POINT('Ctrl Pts',(88.8106164088786,63.9187669975777,13.052786093961));
#67473=CARTESIAN_POINT('Ctrl Pts',(88.7469704637981,63.9110150096771,13.1031043569611));
#67474=CARTESIAN_POINT('Ctrl Pts',(88.6921995914175,63.9048808839701,13.1398746330204));
#67475=CARTESIAN_POINT('Ctrl Pts',(88.570800145194,63.8918157099872,13.2083333263439));
#67476=CARTESIAN_POINT('Ctrl Pts',(88.5037799042016,63.8848962314556,13.2388029095509));
#67477=CARTESIAN_POINT('Ctrl Pts',(88.4195586494435,63.8762343506057,13.2685935873224));
#67478=CARTESIAN_POINT('Ctrl Pts',(88.4045105475992,63.8746884308345,13.2736013007533));
#67479=CARTESIAN_POINT('Ctrl Pts',(88.3801278952293,63.8721835678532,13.2812112586279));
#67480=CARTESIAN_POINT('Ctrl Pts',(88.3708499972099,63.8712304458611,13.2839908754675));
#67481=CARTESIAN_POINT('Ctrl Pts',(88.3529927141046,63.8693953435514,13.2891190018694));
#67482=CARTESIAN_POINT('Ctrl Pts',(88.3444186257631,63.8685139581952,13.2914840345707));
#67483=CARTESIAN_POINT('Ctrl Pts',(88.3244629813498,63.8664614495658,13.2967635782903));
#67484=CARTESIAN_POINT('Ctrl Pts',(88.3130646401807,63.8652882312671,13.2996105364436));
#67485=CARTESIAN_POINT('Ctrl Pts',(88.2756418075873,63.8614321516787,13.308407889798));
#67486=CARTESIAN_POINT('Ctrl Pts',(88.2494711694235,63.858728735124,13.3136954273214));
#67487=CARTESIAN_POINT('Ctrl Pts',(88.1852859641988,63.8520745933887,13.3245704977946));
#67488=CARTESIAN_POINT('Ctrl Pts',(88.1471491657478,63.8481002872882,13.3292648279829));
#67489=CARTESIAN_POINT('Ctrl Pts',(88.0606165737377,63.8390379911835,13.3359526659121));
#67490=CARTESIAN_POINT('Ctrl Pts',(88.0121996398267,63.8339354444197,13.3369207655648));
#67491=CARTESIAN_POINT('Ctrl Pts',(87.9016608098566,63.822275129154,13.3328139660754));
#67492=CARTESIAN_POINT('Ctrl Pts',(87.8397169563649,63.8157317057502,13.3259353877943));
#67493=CARTESIAN_POINT('Ctrl Pts',(87.7687925704164,63.8083657652721,13.312729096893));
#67494=CARTESIAN_POINT('Ctrl Pts',(87.7590872561698,63.8073607064224,13.3108043506762));
#67495=CARTESIAN_POINT('Ctrl Pts',(87.7438492447954,63.8057882010956,13.3075968374524));
#67496=CARTESIAN_POINT('Ctrl Pts',(87.7383013018057,63.805216829394,13.3063901230714));
#67497=CARTESIAN_POINT('Ctrl Pts',(87.7278556634671,63.8041434526552,13.3040446537746));
#67498=CARTESIAN_POINT('Ctrl Pts',(87.7229565760114,63.803641059109,13.3029140099103));
#67499=CARTESIAN_POINT('Ctrl Pts',(87.7112540187223,63.8024432242681,13.3001399147128));
#67500=CARTESIAN_POINT('Ctrl Pts',(87.7044571699791,63.8017493215497,13.2984692629455));
#67501=CARTESIAN_POINT('Ctrl Pts',(87.6808244473056,63.799341708248,13.2924527791167));
#67502=CARTESIAN_POINT('Ctrl Pts',(87.6640630560064,63.7976431602856,13.2878171632395));
#67503=CARTESIAN_POINT('Ctrl Pts',(87.6218336721022,63.7933735247816,13.2751987448215));
#67504=CARTESIAN_POINT('Ctrl Pts',(87.5965113144636,63.7908223617457,13.2667545277613));
#67505=CARTESIAN_POINT('Ctrl Pts',(87.4769298164312,63.7787299554461,13.2226431690182));
#67506=CARTESIAN_POINT('Ctrl Pts',(87.3868753899381,63.7694599997669,13.1766411877438));
#67507=CARTESIAN_POINT('Ctrl Pts',(87.2751706148619,63.7566423927022,13.1016616172297));
#67508=CARTESIAN_POINT('Ctrl Pts',(87.2479025986241,63.7533972341194,13.0817370620718));
#67509=CARTESIAN_POINT('Ctrl Pts',(87.211192502205,63.7488346316453,13.0526001736404));
#67510=CARTESIAN_POINT('Ctrl Pts',(87.2010492700679,63.7475523062412,13.0442902024588));
#67511=CARTESIAN_POINT('Ctrl Pts',(87.1875562592843,63.7458157261342,13.0328821963127));
#67512=CARTESIAN_POINT('Ctrl Pts',(87.1840915006016,63.7453670099197,13.0299206956189));
#67513=CARTESIAN_POINT('Ctrl Pts',(87.1806428353965,63.7449175370261,13.0269406741269));
#67514=CARTESIAN_POINT('Origin',(88.011,66.41344859951,12.066));
#67515=CARTESIAN_POINT('',(87.1797597215505,62.780326894738,13.0279488901568));
#67516=CARTESIAN_POINT('',(87.1806428339316,62.9499311262155,13.0269406728612));
#67517=CARTESIAN_POINT('',(87.1806428354228,66.41344859951,13.0269406741497));
#67518=CARTESIAN_POINT('',(86.7419560246514,63.4657506420021,12.0649467613062));
#67519=CARTESIAN_POINT('Ctrl Pts',(86.7419560246514,63.4657506420021,12.0649467613062));
#67520=CARTESIAN_POINT('Ctrl Pts',(86.7409244756087,63.4525560590529,11.9320771572024));
#67521=CARTESIAN_POINT('Ctrl Pts',(86.8212857002323,63.3973567279427,11.37743698812));
#67522=CARTESIAN_POINT('Ctrl Pts',(87.6251828593756,63.3001526486715,10.6153602361256));
#67523=CARTESIAN_POINT('Ctrl Pts',(89.0204464687028,63.1741384041882,10.9550414954645));
#67524=CARTESIAN_POINT('Ctrl Pts',(89.4918622599116,63.0481241597051,12.3114749020928));
#67525=CARTESIAN_POINT('Ctrl Pts',(88.6079892037427,62.9221099152218,13.443248983286));
#67526=CARTESIAN_POINT('Ctrl Pts',(87.5948389254085,62.8328441602328,13.3520895155867));
#67527=CARTESIAN_POINT('Ctrl Pts',(87.2193328732881,62.7855831534049,13.062732661936));
#67528=CARTESIAN_POINT('Ctrl Pts',(87.1797597215505,62.780326894738,13.0279488901567));
#67529=CARTESIAN_POINT('Ctrl Pts',(86.7410003896142,63.4652041016888,12.0650052036116));
#67530=CARTESIAN_POINT('Ctrl Pts',(86.7409713236518,63.4687020212302,12.1021120541925));
#67531=CARTESIAN_POINT('Ctrl Pts',(86.7425685365845,63.4722221260772,12.1391996150127));
#67532=CARTESIAN_POINT('Ctrl Pts',(86.7476703066644,63.4778718902256,12.1977936676512));
#67533=CARTESIAN_POINT('Ctrl Pts',(86.750108113238,63.4799715403944,12.2193721184907));
#67534=CARTESIAN_POINT('Ctrl Pts',(86.7544144072352,63.4830201377987,12.2503477553927));
#67535=CARTESIAN_POINT('Ctrl Pts',(86.7558380734332,63.4839554676294,12.2598039548382));
#67536=CARTESIAN_POINT('Ctrl Pts',(86.7586878084231,63.485703446774,12.2773815359158));
#67537=CARTESIAN_POINT('Ctrl Pts',(86.7600864601472,63.4865152030011,12.2855069172544));
#67538=CARTESIAN_POINT('Ctrl Pts',(86.7631563847018,63.4882069175507,12.3023582919543));
#67539=CARTESIAN_POINT('Ctrl Pts',(86.7648403033542,63.4890872318153,12.3110814776042));
#67540=CARTESIAN_POINT('Ctrl Pts',(86.7689097559293,63.4911119410671,12.3310351531677));
#67541=CARTESIAN_POINT('Ctrl Pts',(86.7713562966672,63.4922582120445,12.342252191584));
#67542=CARTESIAN_POINT('Ctrl Pts',(86.7798019162478,63.4960002128208,12.3786000626144));
#67543=CARTESIAN_POINT('Ctrl Pts',(86.7864153797502,63.4986151269625,12.4035792948837));
#67544=CARTESIAN_POINT('Ctrl Pts',(86.8150619224439,63.5088697567477,12.4998128233256));
#67545=CARTESIAN_POINT('Ctrl Pts',(86.8425886954972,63.5166728019777,12.5692617160998));
#67546=CARTESIAN_POINT('Ctrl Pts',(86.9082538467012,63.5320964874793,12.7000383366934));
#67547=CARTESIAN_POINT('Ctrl Pts',(86.9458532142023,63.539684769947,12.7613549836031));
#67548=CARTESIAN_POINT('Ctrl Pts',(86.9955183424985,63.5482693734341,12.8287840674081));
#67549=CARTESIAN_POINT('Ctrl Pts',(87.0027341681018,63.5494862787891,12.8382969502422));
#67550=CARTESIAN_POINT('Ctrl Pts',(87.0139651411797,63.5513332201002,12.852677353808));
#67551=CARTESIAN_POINT('Ctrl Pts',(87.0178838616202,63.5519692151185,12.8576186648877));
#67552=CARTESIAN_POINT('Ctrl Pts',(87.0249516937241,63.553101075651,12.8663957535368));
#67553=CARTESIAN_POINT('Ctrl Pts',(87.0280866399815,63.5535978647649,12.8702424726002));
#67554=CARTESIAN_POINT('Ctrl Pts',(87.0351536752969,63.554706127321,12.8788109877208));
#67555=CARTESIAN_POINT('Ctrl Pts',(87.039097580909,63.5553167430409,12.8835227487692));
#67556=CARTESIAN_POINT('Ctrl Pts',(87.0511383886331,63.5571580349622,12.8976975326192));
#67557=CARTESIAN_POINT('Ctrl Pts',(87.0593408319984,63.558381511451,12.9070707279191));
#67558=CARTESIAN_POINT('Ctrl Pts',(87.103024587476,63.5647485768805,12.9555320454869));
#67559=CARTESIAN_POINT('Ctrl Pts',(87.1407551420657,63.5697471123937,12.9924733889405));
#67560=CARTESIAN_POINT('Ctrl Pts',(87.1806430603713,63.5747053956106,13.0269408685296));
#67561=CARTESIAN_POINT('',(86.7410002780733,63.6360809738954,12.0668404202127));
#67562=CARTESIAN_POINT('Ctrl Pts',(87.1806428353965,63.7449175370261,13.0269406741269));
#67563=CARTESIAN_POINT('Ctrl Pts',(87.1778788344965,63.7445572980906,13.0245522769948));
#67564=CARTESIAN_POINT('Ctrl Pts',(87.1751251713004,63.7441965731412,13.0221519829543));
#67565=CARTESIAN_POINT('Ctrl Pts',(87.1659580280572,63.7429894889965,13.014091365608));
#67566=CARTESIAN_POINT('Ctrl Pts',(87.1595915709135,63.7421409630232,13.0083782943341));
#67567=CARTESIAN_POINT('Ctrl Pts',(87.1529095443805,63.741239248717,13.0022590598248));
#67568=CARTESIAN_POINT('Ctrl Pts',(87.1525357886098,63.7411887745264,13.0019163717393));
#67569=CARTESIAN_POINT('Ctrl Pts',(87.1518123142576,63.7410909999996,13.0012522367258));
#67570=CARTESIAN_POINT('Ctrl Pts',(87.1514625704879,63.7410437008327,13.0009308171722));
#67571=CARTESIAN_POINT('Ctrl Pts',(87.1507806068307,63.7409514084119,13.0003033766582));
#67572=CARTESIAN_POINT('Ctrl Pts',(87.1504483696968,63.7409064159682,12.9999973745148));
#67573=CARTESIAN_POINT('Ctrl Pts',(87.1497962050958,63.7408180397169,12.999396064489));
#67574=CARTESIAN_POINT('Ctrl Pts',(87.1494762660274,63.7407746564444,12.9991007691357));
#67575=CARTESIAN_POINT('Ctrl Pts',(87.1488443509107,63.7406889150047,12.9985169260302));
#67576=CARTESIAN_POINT('Ctrl Pts',(87.1485323676797,63.7406465571727,12.9982283860665));
#67577=CARTESIAN_POINT('Ctrl Pts',(87.1479125877201,63.740562357434,12.9976546006264));
#67578=CARTESIAN_POINT('Ctrl Pts',(87.1476047874424,63.7405205157009,12.9973693590814));
#67579=CARTESIAN_POINT('Ctrl Pts',(87.1469899506854,63.7404368845232,12.9967990171017));
#67580=CARTESIAN_POINT('Ctrl Pts',(87.1466829137761,63.7403950951006,12.9965139171525));
#67581=CARTESIAN_POINT('Ctrl Pts',(87.1357377501743,63.7389044792801,12.9863406648321));
#67582=CARTESIAN_POINT('Ctrl Pts',(87.1252704729314,63.7374479672294,12.9762714458703));
#67583=CARTESIAN_POINT('Ctrl Pts',(87.102570979154,63.7342183613692,12.9536729414441));
#67584=CARTESIAN_POINT('Ctrl Pts',(87.0904208160166,63.7324420838182,12.9410659553854));
#67585=CARTESIAN_POINT('Ctrl Pts',(87.0544416730841,63.7270326830765,12.9021552974288));
#67586=CARTESIAN_POINT('Ctrl Pts',(87.0314531185552,63.7233684024862,12.8751025100768));
#67587=CARTESIAN_POINT('Ctrl Pts',(86.9780054478688,63.7143148678151,12.8065848418268));
#67588=CARTESIAN_POINT('Ctrl Pts',(86.9488746554184,63.7088963998614,12.7641637642627));
#67589=CARTESIAN_POINT('Ctrl Pts',(86.8917177396462,63.697196099985,12.6690385322688));
#67590=CARTESIAN_POINT('Ctrl Pts',(86.8646645435672,63.690926387005,12.6158773931494));
#67591=CARTESIAN_POINT('Ctrl Pts',(86.8364194656174,63.6834929624039,12.5491423666132));
#67592=CARTESIAN_POINT('Ctrl Pts',(86.8315784424978,63.68217936296,12.5372014580475));
#67593=CARTESIAN_POINT('Ctrl Pts',(86.8246685914241,63.6802454217344,12.5193834476938));
#67594=CARTESIAN_POINT('Ctrl Pts',(86.8224601543705,63.6796176759507,12.5135620660421));
#67595=CARTESIAN_POINT('Ctrl Pts',(86.8185693728157,63.6784943314309,12.5030741367298));
#67596=CARTESIAN_POINT('Ctrl Pts',(86.8168714706041,63.6779978737666,12.4984137603813));
#67597=CARTESIAN_POINT('Ctrl Pts',(86.8131066870418,63.6768827325442,12.4878889297532));
#67598=CARTESIAN_POINT('Ctrl Pts',(86.811055510164,63.6762649676082,12.4820190928084));
#67599=CARTESIAN_POINT('Ctrl Pts',(86.8068366330882,63.6749719576557,12.4696551152142));
#67600=CARTESIAN_POINT('Ctrl Pts',(86.8046781557314,63.6742972303955,12.4631580058806));
#67601=CARTESIAN_POINT('Ctrl Pts',(86.7990370416351,63.6724967885898,12.4457076226712));
#67602=CARTESIAN_POINT('Ctrl Pts',(86.795650251061,63.6713758818327,12.4347236219992));
#67603=CARTESIAN_POINT('Ctrl Pts',(86.7583954637183,63.6585482493522,12.3078046967755));
#67604=CARTESIAN_POINT('Ctrl Pts',(86.7410802204873,63.647543432149,12.1876452771149));
#67605=CARTESIAN_POINT('Ctrl Pts',(86.7410002780733,63.6360809738954,12.0668404202127));
#67606=CARTESIAN_POINT('Ctrl Pts',(86.7410002770608,63.636080828584,12.0668388887506));
#67607=CARTESIAN_POINT('Ctrl Pts',(86.740974721301,63.6324098526892,12.0281498399178));
#67608=CARTESIAN_POINT('Ctrl Pts',(86.7427170789926,63.6287054753803,11.9894835192214));
#67609=CARTESIAN_POINT('Ctrl Pts',(86.7472007747758,63.6238967995667,11.9401886312309));
#67610=CARTESIAN_POINT('Ctrl Pts',(86.7483180247715,63.6228421524889,11.9294306236973));
#67611=CARTESIAN_POINT('Ctrl Pts',(86.7505582519984,63.620951283067,11.9102475602277));
#67612=CARTESIAN_POINT('Ctrl Pts',(86.7516286790657,63.6201167157255,11.9018169011103));
#67613=CARTESIAN_POINT('Ctrl Pts',(86.753964519267,63.6184234482191,11.8847893451752));
#67614=CARTESIAN_POINT('Ctrl Pts',(86.7552337148474,63.6175646738771,11.8761934436443));
#67615=CARTESIAN_POINT('Ctrl Pts',(86.7581571400063,63.6157089053529,11.8577086470707));
#67616=CARTESIAN_POINT('Ctrl Pts',(86.7598404591185,63.6147110479245,11.8478250518197));
#67617=CARTESIAN_POINT('Ctrl Pts',(86.7647003723756,63.612006910065,11.8211987908639));
#67618=CARTESIAN_POINT('Ctrl Pts',(86.7680970918383,63.6102938089331,11.8044991736362));
#67619=CARTESIAN_POINT('Ctrl Pts',(86.7852454194015,63.6023723622384,11.7280959774561));
#67620=CARTESIAN_POINT('Ctrl Pts',(86.8029673952892,63.5960422064472,11.6693795107205));
#67621=CARTESIAN_POINT('Ctrl Pts',(86.848504660637,63.5826946719617,11.5503585883345));
#67622=CARTESIAN_POINT('Ctrl Pts',(86.8769539359867,63.5756819554171,11.4904822905562));
#67623=CARTESIAN_POINT('Ctrl Pts',(86.9263682775954,63.5652919173396,11.4045162151344));
#67624=CARTESIAN_POINT('Ctrl Pts',(86.9439055312159,63.5618616976349,11.3765823693931));
#67625=CARTESIAN_POINT('Ctrl Pts',(86.969119568661,63.5572826287202,11.3396927115061));
#67626=CARTESIAN_POINT('Ctrl Pts',(86.9758608092795,63.5560893402348,11.3301168562208));
#67627=CARTESIAN_POINT('Ctrl Pts',(86.9864181605426,63.5542686928016,11.3155524937501));
#67628=CARTESIAN_POINT('Ctrl Pts',(86.9901401357136,63.5536356603764,11.3104971548669));
#67629=CARTESIAN_POINT('Ctrl Pts',(86.9968701658313,63.5525069531342,11.3014967061526));
#67630=CARTESIAN_POINT('Ctrl Pts',(86.9998639960061,63.5520103774356,11.29754141839));
#67631=CARTESIAN_POINT('Ctrl Pts',(87.0066323639656,63.5508999997015,11.2887074587019));
#67632=CARTESIAN_POINT('Ctrl Pts',(87.0104193614826,63.5502870756844,11.2838386133593));
#67633=CARTESIAN_POINT('Ctrl Pts',(87.0220374601805,63.5484311197828,11.2691240059134));
#67634=CARTESIAN_POINT('Ctrl Pts',(87.0299799035996,63.5471954573424,11.2593663350289));
#67635=CARTESIAN_POINT('Ctrl Pts',(87.0859781184939,63.5386948477733,11.1926208017888));
#67636=CARTESIAN_POINT('Ctrl Pts',(87.1388341623373,63.5317192327556,11.1398316765309));
#67637=CARTESIAN_POINT('Ctrl Pts',(87.2411061227295,63.5192270717127,11.0542598194228));
#67638=CARTESIAN_POINT('Ctrl Pts',(87.2887456790517,63.5137304606804,11.0197196343669));
#67639=CARTESIAN_POINT('Ctrl Pts',(87.3587933606617,63.5058685016279,10.9760032382588));
#67640=CARTESIAN_POINT('Ctrl Pts',(87.3793327625204,63.5035883119976,10.9639733246264));
#67641=CARTESIAN_POINT('Ctrl Pts',(87.4165491533752,63.4994874586822,10.9435579924292));
#67642=CARTESIAN_POINT('Ctrl Pts',(87.433096205729,63.4976745975404,10.9349496082414));
#67643=CARTESIAN_POINT('Ctrl Pts',(87.4589139148312,63.4948575063346,10.9222327216637));
#67644=CARTESIAN_POINT('Ctrl Pts',(87.4680549216134,63.4938622631665,10.9178653129466));
#67645=CARTESIAN_POINT('Ctrl Pts',(87.4830235823059,63.4922354082331,10.910932282714));
#67646=CARTESIAN_POINT('Ctrl Pts',(87.4888201910716,63.4916061059377,10.908300223472));
#67647=CARTESIAN_POINT('Ctrl Pts',(87.5035065002921,63.4900132391179,10.9017643653714));
#67648=CARTESIAN_POINT('Ctrl Pts',(87.5124214427587,63.4890477384642,10.8979188067478));
#67649=CARTESIAN_POINT('Ctrl Pts',(87.5361223890301,63.4864838919034,10.8880158913315));
#67650=CARTESIAN_POINT('Ctrl Pts',(87.5509795352429,63.4848797594324,10.8821349663878));
#67651=CARTESIAN_POINT('Ctrl Pts',(87.6330632860795,63.476028650612,10.8514219985663));
#67652=CARTESIAN_POINT('Ctrl Pts',(87.7021732161494,63.4686072973881,10.8320399275856));
#67653=CARTESIAN_POINT('Ctrl Pts',(87.8384575622074,63.4540365493605,10.8059865229269));
#67654=CARTESIAN_POINT('Ctrl Pts',(87.9052774317555,63.4469232689498,10.798629548326));
#67655=CARTESIAN_POINT('Ctrl Pts',(87.9877845416672,63.4383111584455,10.7961185188733));
#67656=CARTESIAN_POINT('Ctrl Pts',(88.0032106377316,63.436708687352,10.7959301940393));
#67657=CARTESIAN_POINT('Ctrl Pts',(88.0274280404582,63.4342081562478,10.7960758282989));
#67658=CARTESIAN_POINT('Ctrl Pts',(88.0362184949775,63.4333036562283,10.796219970864));
#67659=CARTESIAN_POINT('Ctrl Pts',(88.0570943431383,63.4311640237176,10.796779168949));
#67660=CARTESIAN_POINT('Ctrl Pts',(88.0691771630497,63.4299323075439,10.7972755764752));
#67661=CARTESIAN_POINT('Ctrl Pts',(88.0873153298456,63.4280949804343,10.7982804532267));
#67662=CARTESIAN_POINT('Ctrl Pts',(88.09337657037,63.4274829608338,10.7986598779004));
#67663=CARTESIAN_POINT('Ctrl Pts',(88.1043873265174,63.4263749970188,10.7994284657178));
#67664=CARTESIAN_POINT('Ctrl Pts',(88.1093374504023,63.4258783210353,10.7998031776724));
#67665=CARTESIAN_POINT('Ctrl Pts',(88.1206493612484,63.4247465164422,10.8007262016051));
#67666=CARTESIAN_POINT('Ctrl Pts',(88.1270093857434,63.4241124409511,10.8012934742789));
#67667=CARTESIAN_POINT('Ctrl Pts',(88.1465567868154,63.422169818513,10.8031856793412));
#67668=CARTESIAN_POINT('Ctrl Pts',(88.1597286159383,63.4208694842112,10.8046691550774));
#67669=CARTESIAN_POINT('Ctrl Pts',(88.2556597223201,63.4114456100984,10.8169972037597));
#67670=CARTESIAN_POINT('Ctrl Pts',(88.3372097345119,63.4036796444376,10.8357728125829));
#67671=CARTESIAN_POINT('Ctrl Pts',(88.4655506297708,63.3909903389589,10.878995316022));
#67672=CARTESIAN_POINT('Ctrl Pts',(88.5136946194585,63.3861167990531,10.8985696051021));
#67673=CARTESIAN_POINT('Ctrl Pts',(88.5804897238031,63.3790492965879,10.9306265072419));
#67674=CARTESIAN_POINT('Ctrl Pts',(88.6002212043818,63.3769217009862,10.9407401356802));
#67675=CARTESIAN_POINT('Ctrl Pts',(88.6353048853998,63.3730553897976,10.9598985206803));
#67676=CARTESIAN_POINT('Ctrl Pts',(88.6507508934359,63.3713229815764,10.9687599205163));
#67677=CARTESIAN_POINT('Ctrl Pts',(88.674650222375,63.3685906635285,10.9831471861076));
#67678=CARTESIAN_POINT('Ctrl Pts',(88.6832331625781,63.3675986646713,10.9884544581321));
#67679=CARTESIAN_POINT('Ctrl Pts',(88.6991896284926,63.3657334651901,10.9985859926686));
#67680=CARTESIAN_POINT('Ctrl Pts',(88.7065780201813,63.364861209331,11.0033858481464));
#67681=CARTESIAN_POINT('Ctrl Pts',(88.7230905723576,63.362891790435,11.0143592003217));
#67682=CARTESIAN_POINT('Ctrl Pts',(88.732185403177,63.3617930839797,11.0205752301688));
#67683=CARTESIAN_POINT('Ctrl Pts',(88.7554859699839,63.3589408438276,11.0369491727886));
#67684=CARTESIAN_POINT('Ctrl Pts',(88.769564513932,63.357180761172,11.0472827845639));
#67685=CARTESIAN_POINT('Ctrl Pts',(88.8386572720735,63.3483519730182,11.1002230628853));
#67686=CARTESIAN_POINT('Ctrl Pts',(88.8903065736056,63.3411247217809,11.1470017822481));
#67687=CARTESIAN_POINT('Ctrl Pts',(88.9815908506844,63.3270878005585,11.2444492537588));
#67688=CARTESIAN_POINT('Ctrl Pts',(89.0217352194448,63.3203121268649,11.2943738164153));
#67689=CARTESIAN_POINT('Ctrl Pts',(89.066452752112,63.3120738872346,11.3594978866205));
#67690=CARTESIAN_POINT('Ctrl Pts',(89.0747376630095,63.3105136989364,11.3720345961342));
#67691=CARTESIAN_POINT('Ctrl Pts',(89.0923468274495,63.307125599561,11.3997374023389));
#67692=CARTESIAN_POINT('Ctrl Pts',(89.1015791064942,63.3053017272696,11.4149591905281));
#67693=CARTESIAN_POINT('Ctrl Pts',(89.1140230828377,63.3027793325172,11.4364843635714));
#67694=CARTESIAN_POINT('Ctrl Pts',(89.117506189909,63.3020658353789,11.4426269832534));
#67695=CARTESIAN_POINT('Ctrl Pts',(89.1233854997704,63.3008488742855,11.4531999818722));
#67696=CARTESIAN_POINT('Ctrl Pts',(89.1258068557812,63.3003438851715,11.4576160411502));
#67697=CARTESIAN_POINT('Ctrl Pts',(89.1308860462559,63.2992765674508,11.4670116042895));
#67698=CARTESIAN_POINT('Ctrl Pts',(89.133537043653,63.2987146615583,11.4719945749487));
#67699=CARTESIAN_POINT('Ctrl Pts',(89.1407968601497,63.2971617872738,11.4858627438029));
#67700=CARTESIAN_POINT('Ctrl Pts',(89.1453341689594,63.2961750874136,11.4947853316033));
#67701=CARTESIAN_POINT('Ctrl Pts',(89.1773106872067,63.2890947249251,11.559550980414));
#67702=CARTESIAN_POINT('Ctrl Pts',(89.2007242013001,63.2832144724285,11.6173011677033));
#67703=CARTESIAN_POINT('Ctrl Pts',(89.2346374149941,63.2728292436425,11.7225632016002));
#67704=CARTESIAN_POINT('Ctrl Pts',(89.2468232308826,63.2683193639547,11.7693887082757));
#67705=CARTESIAN_POINT('Ctrl Pts',(89.2638600710811,63.2601484879769,11.8545238882428));
#67706=CARTESIAN_POINT('Ctrl Pts',(89.2696910935403,63.256506910786,11.892573461));
#67707=CARTESIAN_POINT('Ctrl Pts',(89.2766307282201,63.2502576874316,11.9574030926379));
#67708=CARTESIAN_POINT('Ctrl Pts',(89.2786356637877,63.2476755652195,11.9840608989241));
#67709=CARTESIAN_POINT('Ctrl Pts',(89.2803092410926,63.2439208875251,12.0225009981682));
#67710=CARTESIAN_POINT('Ctrl Pts',(89.2806573961418,63.2427693165201,12.0342480471408));
#67711=CARTESIAN_POINT('Ctrl Pts',(89.2809825347437,63.2407373898654,12.0548894792292));
#67712=CARTESIAN_POINT('Ctrl Pts',(89.2810291938153,63.2398592575688,12.0637821299032));
#67713=CARTESIAN_POINT('Ctrl Pts',(89.2809315937911,63.2380191318709,12.0823535359837));
#67714=CARTESIAN_POINT('Ctrl Pts',(89.2807700718168,63.2370566576788,12.0920315669013));
#67715=CARTESIAN_POINT('Ctrl Pts',(89.2800526317046,63.2345099097434,12.1175392356436));
#67716=CARTESIAN_POINT('Ctrl Pts',(89.2793111871343,63.2329199880404,12.1333613324134));
#67717=CARTESIAN_POINT('Ctrl Pts',(89.273640825396,63.2241765755638,12.2197671933302));
#67718=CARTESIAN_POINT('Ctrl Pts',(89.2631167562541,63.2168531806329,12.2898426582664));
#67719=CARTESIAN_POINT('Ctrl Pts',(89.2311345598257,63.202283925184,12.4248927202992));
#67720=CARTESIAN_POINT('Ctrl Pts',(89.2101518089455,63.1950694746176,12.4897540328759));
#67721=CARTESIAN_POINT('Ctrl Pts',(89.1781175456923,63.1863457211623,12.5669772062672));
#67722=CARTESIAN_POINT('Ctrl Pts',(89.1718993658539,63.1847309801808,12.5812225175145));
#67723=CARTESIAN_POINT('Ctrl Pts',(89.1578257297474,63.1812443265186,12.6119146374463));
#67724=CARTESIAN_POINT('Ctrl Pts',(89.1498742233914,63.1793764102443,12.6283145644598));
#67725=CARTESIAN_POINT('Ctrl Pts',(89.1383263850097,63.176804243065,12.6508811640239));
#67726=CARTESIAN_POINT('Ctrl Pts',(89.1350275555832,63.1760842551329,12.6571960904888));
#67727=CARTESIAN_POINT('Ctrl Pts',(89.1293017132122,63.1748598108925,12.6679358268252));
#67728=CARTESIAN_POINT('Ctrl Pts',(89.1269012079024,63.1743537796587,12.6723744391024));
#67729=CARTESIAN_POINT('Ctrl Pts',(89.1217737075779,63.1732882761929,12.6817217698689));
#67730=CARTESIAN_POINT('Ctrl Pts',(89.1190405308374,63.1727291988858,12.6866268716887));
#67731=CARTESIAN_POINT('Ctrl Pts',(89.1114121067439,63.1711925109648,12.7001061973528));
#67732=CARTESIAN_POINT('Ctrl Pts',(89.1064490951487,63.1702190251029,12.7086420281));
#67733=CARTESIAN_POINT('Ctrl Pts',(89.0750072113904,63.1642057379163,12.7612956636711));
#67734=CARTESIAN_POINT('Ctrl Pts',(89.0459624246218,63.159310196051,12.8038361059621));
#67735=CARTESIAN_POINT('Ctrl Pts',(88.9674603394924,63.1472403727625,12.9050172090907));
#67736=CARTESIAN_POINT('Ctrl Pts',(88.9151333661631,63.1401388838155,12.9611586597914));
#67737=CARTESIAN_POINT('Ctrl Pts',(88.8260415889831,63.1288094857315,13.0409127104838));
#67738=CARTESIAN_POINT('Ctrl Pts',(88.7925850252321,63.1246978942121,13.0679339198044));
#67739=CARTESIAN_POINT('Ctrl Pts',(88.7466167636479,63.1191716667531,13.1013550478156));
#67740=CARTESIAN_POINT('Ctrl Pts',(88.7352744079717,63.1178175435534,13.1093209686171));
#67741=CARTESIAN_POINT('Ctrl Pts',(88.7161332721881,63.115546074811,13.122301557047));
#67742=CARTESIAN_POINT('Ctrl Pts',(88.7084055926599,63.1146326762375,13.1274194924266));
#67743=CARTESIAN_POINT('Ctrl Pts',(88.693067454899,63.1128263003296,13.1373379209636));
#67744=CARTESIAN_POINT('Ctrl Pts',(88.6854606161328,63.111933558945,13.1421430297959));
#67745=CARTESIAN_POINT('Ctrl Pts',(88.6668008790737,63.109750644741,13.1536545135305));
#67746=CARTESIAN_POINT('Ctrl Pts',(88.6556956824345,63.1084573857454,13.1602735394108));
#67747=CARTESIAN_POINT('Ctrl Pts',(88.616380980306,63.1038975407184,13.1829001016026));
#67748=CARTESIAN_POINT('Ctrl Pts',(88.5876640577248,63.1005994501151,13.1979938393671));
#67749=CARTESIAN_POINT('Ctrl Pts',(88.4794661495387,63.0882746394056,13.2496775315404));
#67750=CARTESIAN_POINT('Ctrl Pts',(88.3968547200154,63.0790388568864,13.2791216559667));
#67751=CARTESIAN_POINT('Ctrl Pts',(88.2641322189051,63.064654316586,13.3114881361545));
#67752=CARTESIAN_POINT('Ctrl Pts',(88.2157300598901,63.0595035031374,13.3203538319252));
#67753=CARTESIAN_POINT('Ctrl Pts',(88.1547180398456,63.053202723132,13.3279019494363));
#67754=CARTESIAN_POINT('Ctrl Pts',(88.142484322706,63.0519489755785,13.3292352585699));
#67755=CARTESIAN_POINT('Ctrl Pts',(88.1241449180876,63.0500856002784,13.3309646690371));
#67756=CARTESIAN_POINT('Ctrl Pts',(88.1180531830252,63.0494693019542,13.3314947681054));
#67757=CARTESIAN_POINT('Ctrl Pts',(88.1075050201404,63.0484069847799,13.3323359478733));
#67758=CARTESIAN_POINT('Ctrl Pts',(88.1030505749248,63.0479598808253,13.3326675356406));
#67759=CARTESIAN_POINT('Ctrl Pts',(88.0925318053475,63.0469076111327,13.3333947660591));
#67760=CARTESIAN_POINT('Ctrl Pts',(88.0864662489153,63.0463035582571,13.3337703968814));
#67761=CARTESIAN_POINT('Ctrl Pts',(88.0683028681735,63.0445022121795,13.3347644035184));
#67762=CARTESIAN_POINT('Ctrl Pts',(88.0561980720637,63.0433116704835,13.3352532860217));
#67763=CARTESIAN_POINT('Ctrl Pts',(87.9465910620129,63.032605431056,13.3381098484464));
#67764=CARTESIAN_POINT('Ctrl Pts',(87.8491062050064,63.0235961835048,13.3294121332167));
#67765=CARTESIAN_POINT('Ctrl Pts',(87.6930982747609,63.0086411893832,13.2971178019581));
#67766=CARTESIAN_POINT('Ctrl Pts',(87.6336365895338,63.0028095373435,13.2802106558396));
#67767=CARTESIAN_POINT('Ctrl Pts',(87.5587237698494,62.9950984732415,13.2528743482221));
#67768=CARTESIAN_POINT('Ctrl Pts',(87.5419355399343,62.9933462132126,13.2463401890123));
#67769=CARTESIAN_POINT('Ctrl Pts',(87.5159291872691,62.990589694004,13.2355758169293));
#67770=CARTESIAN_POINT('Ctrl Pts',(87.5066125217897,62.9895935839611,13.2315882455934));
#67771=CARTESIAN_POINT('Ctrl Pts',(87.4892910978402,62.9877247563071,13.223928050818));
#67772=CARTESIAN_POINT('Ctrl Pts',(87.481274819796,62.9868530182226,13.2202827959413));
#67773=CARTESIAN_POINT('Ctrl Pts',(87.4633719291289,62.984890206739,13.2119160206114));
#67774=CARTESIAN_POINT('Ctrl Pts',(87.4535073561872,62.983797635278,13.2071494043554));
#67775=CARTESIAN_POINT('Ctrl Pts',(87.428268049815,62.9809726494415,13.1945482777152));
#67776=CARTESIAN_POINT('Ctrl Pts',(87.4129897234114,62.9792338961734,13.1865272754547));
#67777=CARTESIAN_POINT('Ctrl Pts',(87.3226930091744,62.9687784660065,13.1367495580658));
#67778=CARTESIAN_POINT('Ctrl Pts',(87.2519201410562,62.9598099227285,13.0877935866203));
#67779=CARTESIAN_POINT('Ctrl Pts',(87.1846354640199,62.9504866605631,13.0303799027871));
#67780=CARTESIAN_POINT('Ctrl Pts',(87.1826364289937,62.9502088975538,13.0286633556373));
#67781=CARTESIAN_POINT('Ctrl Pts',(87.1806428339316,62.9499311262155,13.0269406728612));
#67782=CARTESIAN_POINT('Origin',(88.011,66.41344859951,12.066));
#67783=CARTESIAN_POINT('',(87.1806428354228,61.9866340346925,13.0269406741497));
#67784=CARTESIAN_POINT('',(87.180642835277,62.1551929346177,13.0269406740237));
#67785=CARTESIAN_POINT('',(87.1806428354228,66.41344859951,13.0269406741497));
#67786=CARTESIAN_POINT('',(86.7407830691985,62.6720014274556,12.065881049187));
#67787=CARTESIAN_POINT('Ctrl Pts',(86.741000005594,62.67200140049,12.0658807996838));
#67788=CARTESIAN_POINT('Ctrl Pts',(86.7410006057567,62.6713614090784,12.0594864653682));
#67789=CARTESIAN_POINT('Ctrl Pts',(86.7410494978638,62.6707214176669,12.0530923928506));
#67790=CARTESIAN_POINT('Ctrl Pts',(86.7411466724212,62.6700814262553,12.0466990560575));
#67791=CARTESIAN_POINT('Ctrl Pts',(86.7418979703423,62.6651333798744,11.9972694443311));
#67792=CARTESIAN_POINT('Ctrl Pts',(86.7455413478563,62.6601853334935,11.9477745076525));
#67793=CARTESIAN_POINT('Ctrl Pts',(86.7520835395843,62.6552372871125,11.8985803306225));
#67794=CARTESIAN_POINT('Ctrl Pts',(86.7586136938254,62.6502983450267,11.8494766697819));
#67795=CARTESIAN_POINT('Ctrl Pts',(86.7680320119969,62.6453594029408,11.8006732098016));
#67796=CARTESIAN_POINT('Ctrl Pts',(86.7802932726123,62.6404204608549,11.7525339712782));
#67797=CARTESIAN_POINT('Ctrl Pts',(86.7925420837303,62.6354865335345,11.7044436110343));
#67798=CARTESIAN_POINT('Ctrl Pts',(86.8076279882371,62.6305526062142,11.6570166655944));
#67799=CARTESIAN_POINT('Ctrl Pts',(86.8254545663108,62.6256186788938,11.6106078342146));
#67800=CARTESIAN_POINT('Ctrl Pts',(86.8432706298085,62.6206876617311,11.564226375962));
#67801=CARTESIAN_POINT('Ctrl Pts',(86.8638239683567,62.6157566445685,11.5188623527093));
#67802=CARTESIAN_POINT('Ctrl Pts',(86.8869688672123,62.6108256274059,11.4748536454278));
#67803=CARTESIAN_POINT('Ctrl Pts',(86.9101099627559,62.6058954205383,11.4308521699275));
#67804=CARTESIAN_POINT('Ctrl Pts',(86.9358415173653,62.6009652136707,11.3882060525231));
#67805=CARTESIAN_POINT('Ctrl Pts',(86.9639715443507,62.5960350068031,11.3472292346925));
#67806=CARTESIAN_POINT('Ctrl Pts',(86.992129055113,62.5910999829936,11.3062123814323));
#67807=CARTESIAN_POINT('Ctrl Pts',(87.022689405474,62.5861649591841,11.2668685361716));
#67808=CARTESIAN_POINT('Ctrl Pts',(87.0554178905788,62.5812299353746,11.2294817203706));
#67809=CARTESIAN_POINT('Ctrl Pts',(87.088163989134,62.5762922556892,11.192074784151));
#67810=CARTESIAN_POINT('Ctrl Pts',(87.1230801610023,62.5713545760037,11.1566273654471));
#67811=CARTESIAN_POINT('Ctrl Pts',(87.159894543864,62.5664168963183,11.1233868754703));
#67812=CARTESIAN_POINT('Ctrl Pts',(87.1967776730886,62.5614699961192,11.0900843129392));
#67813=CARTESIAN_POINT('Ctrl Pts',(87.235565660193,62.5565230959201,11.0589972473201));
#67814=CARTESIAN_POINT('Ctrl Pts',(87.2759545580742,62.551576195721,11.0303320038236));
#67815=CARTESIAN_POINT('Ctrl Pts',(87.2963903047281,62.5490731910714,11.015828125664));
#67816=CARTESIAN_POINT('Ctrl Pts',(87.3172354577096,62.5465701864218,11.0019435539194));
#67817=CARTESIAN_POINT('Ctrl Pts',(87.3384482567997,62.5440671817721,10.9887005278391));
#67818=CARTESIAN_POINT('Ctrl Pts',(87.3803826224638,62.5391191354633,10.9625211492575));
#67819=CARTESIAN_POINT('Ctrl Pts',(87.4239405293717,62.5341710891545,10.9387360357047));
#67820=CARTESIAN_POINT('Ctrl Pts',(87.468818074963,62.5292230428457,10.9175494089151));
#67821=CARTESIAN_POINT('Ctrl Pts',(87.5136130468598,62.524284100833,10.8964017650517));
#67822=CARTESIAN_POINT('Ctrl Pts',(87.5597223501887,62.5193451588204,10.8778433573357));
#67823=CARTESIAN_POINT('Ctrl Pts',(87.6068156354732,62.5144062168077,10.8620336385629));
#67824=CARTESIAN_POINT('Ctrl Pts',(87.6538611044828,62.5094722895611,10.8462399722243));
#67825=CARTESIAN_POINT('Ctrl Pts',(87.7018880606137,62.5045383623145,10.8331896433857));
#67826=CARTESIAN_POINT('Ctrl Pts',(87.7505462155302,62.4996044350679,10.8229940361546));
#67827=CARTESIAN_POINT('Ctrl Pts',(87.7991756706055,62.4946734179794,10.8128044425569));
#67828=CARTESIAN_POINT('Ctrl Pts',(87.848435051608,62.489742400891,10.8054663470793));
#67829=CARTESIAN_POINT('Ctrl Pts',(87.897961462094,62.4848113838026,10.8010405979052));
#67830=CARTESIAN_POINT('Ctrl Pts',(87.9474797340928,62.4798811770095,10.7966155759977));
#67831=CARTESIAN_POINT('Ctrl Pts',(87.9972644028728,62.4749509702165,10.7951019980655));
#67832=CARTESIAN_POINT('Ctrl Pts',(88.0469475862184,62.4700207634234,10.7965088534988));
#67833=CARTESIAN_POINT('Ctrl Pts',(88.0966793113441,62.4650857396883,10.7979170834669));
#67834=CARTESIAN_POINT('Ctrl Pts',(88.1463088042846,62.4601507159532,10.8022514272422));
#67835=CARTESIAN_POINT('Ctrl Pts',(88.1954701489838,62.4552156922181,10.8094687571995));
#67836=CARTESIAN_POINT('Ctrl Pts',(88.2446579507863,62.4502780126071,10.8166899712987));
#67837=CARTESIAN_POINT('Ctrl Pts',(88.2933765655566,62.4453403329961,10.8267971497315));
#67838=CARTESIAN_POINT('Ctrl Pts',(88.3412706801208,62.440402653385,10.8396960907457));
#67839=CARTESIAN_POINT('Ctrl Pts',(88.3892542311027,62.4354557532595,10.852619118959));
#67840=CARTESIAN_POINT('Ctrl Pts',(88.4364096888277,62.4305088531341,10.8683441413176));
#67841=CARTESIAN_POINT('Ctrl Pts',(88.4823988545942,62.4255619530086,10.8867277159675));
#67842=CARTESIAN_POINT('Ctrl Pts',(88.5056681990265,62.4230589477687,10.8960293356707));
#67843=CARTESIAN_POINT('Ctrl Pts',(88.5286393123781,62.4205559425288,10.906010817654));
#67844=CARTESIAN_POINT('Ctrl Pts',(88.5512708602641,62.4180529372889,10.9166491407975));
#67845=CARTESIAN_POINT('Ctrl Pts',(88.5960098583555,62.4131048909947,10.937679426539));
#67846=CARTESIAN_POINT('Ctrl Pts',(88.6396179904876,62.4081568447004,10.9613723300261));
#67847=CARTESIAN_POINT('Ctrl Pts',(88.6817588492855,62.4032087984061,10.9875833059039));
#67848=CARTESIAN_POINT('Ctrl Pts',(88.7238221698255,62.3982698564088,11.0137460541597));
#67849=CARTESIAN_POINT('Ctrl Pts',(88.7644231100233,62.3933309144115,11.0424173985487));
#67850=CARTESIAN_POINT('Ctrl Pts',(88.8032485290623,62.3883919724141,11.0734062924849));
#67851=CARTESIAN_POINT('Ctrl Pts',(88.8420345266195,62.3834580451833,11.1043637217737));
#67852=CARTESIAN_POINT('Ctrl Pts',(88.8790481456838,62.3785241179525,11.1376337020299));
#67853=CARTESIAN_POINT('Ctrl Pts',(88.9140058141485,62.3735901907217,11.1729823632122));
#67854=CARTESIAN_POINT('Ctrl Pts',(88.9489428636708,62.3686591736495,11.2083101748345));
#67855=CARTESIAN_POINT('Ctrl Pts',(88.981825980317,62.3637281565774,11.2457138496118));
#67856=CARTESIAN_POINT('Ctrl Pts',(89.0124072096571,62.3587971395052,11.2849215145411));
#67857=CARTESIAN_POINT('Ctrl Pts',(89.0429834136973,62.3538669327288,11.3241227366203));
#67858=CARTESIAN_POINT('Ctrl Pts',(89.07125814532,62.3489367259524,11.3651269278832));
#67859=CARTESIAN_POINT('Ctrl Pts',(89.0970243134888,62.344006519176,11.4076298985288));
#67860=CARTESIAN_POINT('Ctrl Pts',(89.1228156558807,62.339071495458,11.4501743956931));
#67861=CARTESIAN_POINT('Ctrl Pts',(89.1460932575231,62.3341364717401,11.4942201259434));
#67862=CARTESIAN_POINT('Ctrl Pts',(89.1666948784301,62.3292014480221,11.539436283086));
#67863=CARTESIAN_POINT('Ctrl Pts',(89.187307586486,62.3242637684286,11.5846767741521));
#67864=CARTESIAN_POINT('Ctrl Pts',(89.2052412483597,62.319326088835,11.6310884347458));
#67865=CARTESIAN_POINT('Ctrl Pts',(89.2203822835105,62.3143884092415,11.678321663836));
#67866=CARTESIAN_POINT('Ctrl Pts',(89.235551592697,62.3094415091337,11.7256430952184));
#67867=CARTESIAN_POINT('Ctrl Pts',(89.2479177305411,62.304494609026,11.7737886260868));
#67868=CARTESIAN_POINT('Ctrl Pts',(89.2574177670228,62.2995477089182,11.8223963258696));
#67869=CARTESIAN_POINT('Ctrl Pts',(89.2622245433512,62.2970447035474,11.8469905830755));
#67870=CARTESIAN_POINT('Ctrl Pts',(89.2662983927379,62.2945416981765,11.8717030465113));
#67871=CARTESIAN_POINT('Ctrl Pts',(89.2696362359932,62.2920386928057,11.8964865036503));
#67872=CARTESIAN_POINT('Ctrl Pts',(89.2762346249657,62.2870906464855,11.9454794843787));
#67873=CARTESIAN_POINT('Ctrl Pts',(89.2799827120667,62.2821426001653,11.9949666012378));
#67874=CARTESIAN_POINT('Ctrl Pts',(89.2808194659684,62.2771945538451,12.0445868300438));
#67875=CARTESIAN_POINT('Ctrl Pts',(89.2816546802615,62.2722556118212,12.094115758722));
#67876=CARTESIAN_POINT('Ctrl Pts',(89.2795891765119,62.2673166697972,12.1437767701432));
#67877=CARTESIAN_POINT('Ctrl Pts',(89.2746136098131,62.2623777277733,12.1932031646421));
#67878=CARTESIAN_POINT('Ctrl Pts',(89.2696430950675,62.2574438005155,12.2425793739378));
#67879=CARTESIAN_POINT('Ctrl Pts',(89.2617684213628,62.2525098732577,12.291720895308));
#67880=CARTESIAN_POINT('Ctrl Pts',(89.2510322587157,62.2475759459999,12.3402626429981));
#67881=CARTESIAN_POINT('Ctrl Pts',(89.2403024285359,62.2426449289003,12.3887757595062));
#67882=CARTESIAN_POINT('Ctrl Pts',(89.2267145710931,62.2377139118008,12.4366892691107));
#67883=CARTESIAN_POINT('Ctrl Pts',(89.2103626024801,62.2327828947013,12.4836473964628));
#67884=CARTESIAN_POINT('Ctrl Pts',(89.1940133209245,62.2278526878972,12.5305978073627));
#67885=CARTESIAN_POINT('Ctrl Pts',(89.1749010109705,62.2229224810932,12.5765926307948));
#67886=CARTESIAN_POINT('Ctrl Pts',(89.1531689029913,62.2179922742891,12.6212928930209));
#67887=CARTESIAN_POINT('Ctrl Pts',(89.1314155621709,62.2130572505433,12.6660368285792));
#67888=CARTESIAN_POINT('Ctrl Pts',(89.1070375537581,62.2081222267974,12.7094831842614));
#67889=CARTESIAN_POINT('Ctrl Pts',(89.0802247962751,62.2031872030516,12.7513162299482));
#67890=CARTESIAN_POINT('Ctrl Pts',(89.0533976090026,62.19824952343,12.7931717888749));
#67891=CARTESIAN_POINT('Ctrl Pts',(89.0241333860616,62.1933118438083,12.8334118652639));
#67892=CARTESIAN_POINT('Ctrl Pts',(88.9926642287378,62.1883741641867,12.8717514145297));
#67893=CARTESIAN_POINT('Ctrl Pts',(88.9611363066031,62.1834272640509,12.9101625582249));
#67894=CARTESIAN_POINT('Ctrl Pts',(88.9273956043593,62.1784803639152,12.9466656888443));
#67895=CARTESIAN_POINT('Ctrl Pts',(88.8917120543797,62.1735334637794,12.9810116268498));
#67896=CARTESIAN_POINT('Ctrl Pts',(88.8736570892498,62.1710304586271,12.9983897944759));
#67897=CARTESIAN_POINT('Ctrl Pts',(88.8551052779863,62.1685274534748,13.0152163296696));
#67898=CARTESIAN_POINT('Ctrl Pts',(88.8360946146734,62.1660244483225,13.0314630375301));
#67899=CARTESIAN_POINT('Ctrl Pts',(88.7985135324435,62.1610764020127,13.0635802158748));
#67900=CARTESIAN_POINT('Ctrl Pts',(88.758971315785,62.156128355703,13.0935708141126));
#67901=CARTESIAN_POINT('Ctrl Pts',(88.7177381654394,62.1511803093933,13.1211877394622));
#67902=CARTESIAN_POINT('Ctrl Pts',(88.6765808831835,62.1462413673799,13.1487538502766));
#67903=CARTESIAN_POINT('Ctrl Pts',(88.6337392895444,62.1413024253665,13.1739546479818));
#67904=CARTESIAN_POINT('Ctrl Pts',(88.5895163880066,62.1363634833532,13.196583384279));
#67905=CARTESIAN_POINT('Ctrl Pts',(88.5453383882945,62.1314295561061,13.2191891444363));
#67906=CARTESIAN_POINT('Ctrl Pts',(88.4997823426521,62.126495628859,13.2392277647408));
#67907=CARTESIAN_POINT('Ctrl Pts',(88.4531781115136,62.1215617016119,13.2565370711147));
#67908=CARTESIAN_POINT('Ctrl Pts',(88.4066013687604,62.1166306845231,13.2738361680103));
#67909=CARTESIAN_POINT('Ctrl Pts',(88.3589781780092,62.1116996674344,13.2884089496651));
#67910=CARTESIAN_POINT('Ctrl Pts',(88.310658373634,62.1067686503456,13.3001413448674));
#67911=CARTESIAN_POINT('Ctrl Pts',(88.2623465094706,62.1018384435524,13.3118718121292));
#67912=CARTESIAN_POINT('Ctrl Pts',(88.213338791383,62.0969082367592,13.3207626912895));
#67913=CARTESIAN_POINT('Ctrl Pts',(88.1639976863608,62.091978029966,13.3267504542804));
#67914=CARTESIAN_POINT('Ctrl Pts',(88.1146083737807,62.087043006231,13.3327440674733));
#67915=CARTESIAN_POINT('Ctrl Pts',(88.0648855690676,62.082107982496,13.3358288361475));
#67916=CARTESIAN_POINT('Ctrl Pts',(88.015197535349,62.077172958761,13.3359930632476));
#67917=CARTESIAN_POINT('Ctrl Pts',(87.965482761081,62.0722352791502,13.3361573787296));
#67918=CARTESIAN_POINT('Ctrl Pts',(87.9158033427583,62.0672975995394,13.3333980532336));
#67919=CARTESIAN_POINT('Ctrl Pts',(87.8665246438208,62.0623599199287,13.3277554721327));
#67920=CARTESIAN_POINT('Ctrl Pts',(87.8171539229256,62.0574130198037,13.3221023542001));
#67921=CARTESIAN_POINT('Ctrl Pts',(87.7681859550106,62.0524661196787,13.3135553289302));
#67922=CARTESIAN_POINT('Ctrl Pts',(87.7199764920651,62.0475192195537,13.302206017551));
#67923=CARTESIAN_POINT('Ctrl Pts',(87.6955837339273,62.0450162143155,13.2964635555821));
#67924=CARTESIAN_POINT('Ctrl Pts',(87.6713849251587,62.0425132090774,13.2900044778591));
#67925=CARTESIAN_POINT('Ctrl Pts',(87.6474243608414,62.0400102038392,13.2828454111391));
#67926=CARTESIAN_POINT('Ctrl Pts',(87.6000738932191,62.0350638066293,13.2686977828762));
#67927=CARTESIAN_POINT('Ctrl Pts',(87.5534458113065,62.0301174094194,13.2517509792419));
#67928=CARTESIAN_POINT('Ctrl Pts',(87.5078939073899,62.0251710122095,13.2320978773579));
#67929=CARTESIAN_POINT('Ctrl Pts',(87.4624076610314,62.0202317446326,13.2124731030424));
#67930=CARTESIAN_POINT('Ctrl Pts',(87.417995021762,62.0152924770558,13.1901499645511));
#67931=CARTESIAN_POINT('Ctrl Pts',(87.3749941041958,62.010353209479,13.1652708949583));
#67932=CARTESIAN_POINT('Ctrl Pts',(87.3320398447943,62.0054193012567,13.1404188204109));
#67933=CARTESIAN_POINT('Ctrl Pts',(87.2904947446986,62.0004853930343,13.1130165818873));
#67934=CARTESIAN_POINT('Ctrl Pts',(87.2506739689398,61.995551484812,13.0832533246405));
#67935=CARTESIAN_POINT('Ctrl Pts',(87.2266835360991,61.9925790014388,13.0653221464931));
#67936=CARTESIAN_POINT('Ctrl Pts',(87.2033185036515,61.9896065180656,13.0465349155861));
#67937=CARTESIAN_POINT('Ctrl Pts',(87.1806428354228,61.9866340346925,13.0269406741497));
#67938=CARTESIAN_POINT('Ctrl Pts',(87.1797597215505,62.780326894738,13.0279488901567));
#67939=CARTESIAN_POINT('Ctrl Pts',(86.9079078714374,62.7442184833402,12.788998179968));
#67940=CARTESIAN_POINT('Ctrl Pts',(86.7393936515874,62.7081100719423,12.4272468679575));
#67941=CARTESIAN_POINT('Ctrl Pts',(86.7389078838356,62.6720016605445,12.0658832058784));
#67942=CARTESIAN_POINT('Ctrl Pts',(87.1806428339316,62.9499311262155,13.0269406728612));
#67943=CARTESIAN_POINT('Ctrl Pts',(87.1433791946131,62.944739113474,12.9947408390777));
#67944=CARTESIAN_POINT('Ctrl Pts',(87.108016329931,62.9395420260643,12.960397503884));
#67945=CARTESIAN_POINT('Ctrl Pts',(87.0625530535798,62.9325407977779,12.9107919488461));
#67946=CARTESIAN_POINT('Ctrl Pts',(87.0506551050908,62.9306754776798,12.8972417369129));
#67947=CARTESIAN_POINT('Ctrl Pts',(87.0306252328578,62.927482436221,12.873425905078));
#67948=CARTESIAN_POINT('Ctrl Pts',(87.0223562773478,62.9261477280882,12.8632796963223));
#67949=CARTESIAN_POINT('Ctrl Pts',(87.0103629800675,62.9241889703896,12.8480900200647));
#67950=CARTESIAN_POINT('Ctrl Pts',(87.0065171522817,62.9235572508871,12.8431444266552));
#67951=CARTESIAN_POINT('Ctrl Pts',(86.9996918831079,62.9224298617817,12.8342320610732));
#67952=CARTESIAN_POINT('Ctrl Pts',(86.9966989327656,62.9219333018418,12.8302760988669));
#67953=CARTESIAN_POINT('Ctrl Pts',(86.9900289722101,62.9208216979861,12.821351811777));
#67954=CARTESIAN_POINT('Ctrl Pts',(86.9863649519595,62.920207542262,12.8163740556274));
#67955=CARTESIAN_POINT('Ctrl Pts',(86.9753153668611,62.9183438972974,12.8011307761641));
#67956=CARTESIAN_POINT('Ctrl Pts',(86.9680462789525,62.917101866923,12.7907809998036));
#67957=CARTESIAN_POINT('Ctrl Pts',(86.9076245032036,62.9066218592343,12.7019599974306));
#67958=CARTESIAN_POINT('Ctrl Pts',(86.8632451504339,62.8978556902477,12.6178592567991));
#67959=CARTESIAN_POINT('Ctrl Pts',(86.8120435309469,62.8846939376316,12.4872710647938));
#67960=CARTESIAN_POINT('Ctrl Pts',(86.797737170153,62.8804118909068,12.4440986417557));
#67961=CARTESIAN_POINT('Ctrl Pts',(86.7778977787751,62.8732063716651,12.3713767649928));
#67962=CARTESIAN_POINT('Ctrl Pts',(86.7710435342713,62.8703207914111,12.3422312372952));
#67963=CARTESIAN_POINT('Ctrl Pts',(86.7628438354002,62.8662083313521,12.3008538486188));
#67964=CARTESIAN_POINT('Ctrl Pts',(86.760636128876,62.86500858807,12.2888010451757));
#67965=CARTESIAN_POINT('Ctrl Pts',(86.7571150434095,62.8629210377034,12.2678736370288));
#67966=CARTESIAN_POINT('Ctrl Pts',(86.7557206356046,62.8620358443886,12.2590133586977));
#67967=CARTESIAN_POINT('Ctrl Pts',(86.753210552202,62.8603214536186,12.2418843732614));
#67968=CARTESIAN_POINT('Ctrl Pts',(86.7520822810731,62.8594927010816,12.2336179471988));
#67969=CARTESIAN_POINT('Ctrl Pts',(86.749296409748,62.8572800408884,12.211589133669));
#67970=CARTESIAN_POINT('Ctrl Pts',(86.7477826072347,62.8558917132922,12.1978101852589));
#67971=CARTESIAN_POINT('Ctrl Pts',(86.7428025431166,62.8504959103562,12.1444475692518));
#67972=CARTESIAN_POINT('Ctrl Pts',(86.7409696098582,62.8464392205915,12.1047396041735));
#67973=CARTESIAN_POINT('Ctrl Pts',(86.7410589749626,62.8345149724814,11.9893751411073));
#67974=CARTESIAN_POINT('Ctrl Pts',(86.7478752831577,62.8265310814682,11.9138991982498));
#67975=CARTESIAN_POINT('Ctrl Pts',(86.7712715191255,62.8127130106134,11.784824310722));
#67976=CARTESIAN_POINT('Ctrl Pts',(86.7847581257179,62.8068881620656,11.7308593486531));
#67977=CARTESIAN_POINT('Ctrl Pts',(86.8047731226141,62.8002010235078,11.6684885787134));
#67978=CARTESIAN_POINT('Ctrl Pts',(86.8079183356741,62.7991923889187,11.659068628593));
#67979=CARTESIAN_POINT('Ctrl Pts',(86.8130185285439,62.7976215560043,11.6443697599716));
#67980=CARTESIAN_POINT('Ctrl Pts',(86.8148985357381,62.7970553418018,11.6390656292004));
#67981=CARTESIAN_POINT('Ctrl Pts',(86.8185297461466,62.7959857694399,11.62903305095));
#67982=CARTESIAN_POINT('Ctrl Pts',(86.820273868521,62.7954820668185,11.6243024760838));
#67983=CARTESIAN_POINT('Ctrl Pts',(86.8245409864969,62.7942732402089,11.612937773907));
#67984=CARTESIAN_POINT('Ctrl Pts',(86.8270915145438,62.7935697338764,11.606314152707));
#67985=CARTESIAN_POINT('Ctrl Pts',(86.8363212762383,62.7910885876214,11.5829313086721));
#67986=CARTESIAN_POINT('Ctrl Pts',(86.8433024251292,62.7893273737669,11.5662921268863));
#67987=CARTESIAN_POINT('Ctrl Pts',(86.8568627030759,62.7860982077692,11.5358096956931));
#67988=CARTESIAN_POINT('Ctrl Pts',(86.8633420674851,62.7846264287682,11.5219264894434));
#67989=CARTESIAN_POINT('Ctrl Pts',(86.8991752926949,62.7768324716451,11.4486377717621));
#67990=CARTESIAN_POINT('Ctrl Pts',(86.9328956309561,62.77066260478,11.3914757807092));
#67991=CARTESIAN_POINT('Ctrl Pts',(87.0128023029992,62.7576084276197,11.2774402711952));
#67992=CARTESIAN_POINT('Ctrl Pts',(87.0597439113232,62.7507365325286,11.2214089448764));
#67993=CARTESIAN_POINT('Ctrl Pts',(87.1224224945011,62.7421252329423,11.1584860495682));
#67994=CARTESIAN_POINT('Ctrl Pts',(87.1338245763913,62.7405791787491,11.1474605201462));
#67995=CARTESIAN_POINT('Ctrl Pts',(87.152515989458,62.7380743166155,11.1300518265597));
#67996=CARTESIAN_POINT('Ctrl Pts',(87.1596774556089,62.7371213335899,11.1235331877363));
#67997=CARTESIAN_POINT('Ctrl Pts',(87.1735559808104,62.7352866523315,11.1111876760583));
#67998=CARTESIAN_POINT('Ctrl Pts',(87.1802610984983,62.7344055500059,11.1053481762235));
#67999=CARTESIAN_POINT('Ctrl Pts',(87.1959621840866,62.7323539453808,11.091961376563));
#68000=CARTESIAN_POINT('Ctrl Pts',(87.205002436343,62.7311813508958,11.0844676343211));
#68001=CARTESIAN_POINT('Ctrl Pts',(87.2349106283793,62.7273286283388,11.0603676137202));
#68002=CARTESIAN_POINT('Ctrl Pts',(87.2561961454741,62.7246279843959,11.0442945248148));
#68003=CARTESIAN_POINT('Ctrl Pts',(87.3092895191518,62.7179824610759,11.0067675505312));
#68004=CARTESIAN_POINT('Ctrl Pts',(87.3415921612879,62.7140140732761,10.9860632174867));
#68005=CARTESIAN_POINT('Ctrl Pts',(87.4167386008631,62.7049481046193,10.9425659921023));
#68006=CARTESIAN_POINT('Ctrl Pts',(87.4600529630847,62.6998356123842,10.9207020514793));
#68007=CARTESIAN_POINT('Ctrl Pts',(87.5616385382153,62.68815776398,10.8765230210915));
#68008=CARTESIAN_POINT('Ctrl Pts',(87.620528822372,62.6816067513663,10.8559108080824));
#68009=CARTESIAN_POINT('Ctrl Pts',(87.6903679333165,62.6742218425332,10.8370999757573));
#68010=CARTESIAN_POINT('Ctrl Pts',(87.7000640618789,62.6732050309305,10.8346109238143));
#68011=CARTESIAN_POINT('Ctrl Pts',(87.7152722625885,62.6716243546968,10.8308979953796));
#68012=CARTESIAN_POINT('Ctrl Pts',(87.7207644347833,62.6710563946387,10.8295958679565));
#68013=CARTESIAN_POINT('Ctrl Pts',(87.7311733995009,62.669985619489,10.8272012116369));
#68014=CARTESIAN_POINT('Ctrl Pts',(87.7360880687867,62.6694824444908,10.8261012959068));
#68015=CARTESIAN_POINT('Ctrl Pts',(87.7479089375651,62.6682777200108,10.8235294976661));
#68016=CARTESIAN_POINT('Ctrl Pts',(87.7548211289282,62.6675777592842,10.8220859149863));
#68017=CARTESIAN_POINT('Ctrl Pts',(87.7791973950296,62.6651238706717,10.8172068505516));
#68018=CARTESIAN_POINT('Ctrl Pts',(87.7967225959644,62.6633858956163,10.8140806385057));
#68019=CARTESIAN_POINT('Ctrl Pts',(87.8291518133399,62.6602077265317,10.8089968373496));
#68020=CARTESIAN_POINT('Ctrl Pts',(87.8440353196457,62.6587636566323,10.8069334557988));
#68021=CARTESIAN_POINT('Ctrl Pts',(87.9224506713874,62.6512142320144,10.7974773835015));
#68022=CARTESIAN_POINT('Ctrl Pts',(87.9864424020208,62.6452522442995,10.7946270746109));
#68023=CARTESIAN_POINT('Ctrl Pts',(88.1199609341826,62.6327333142382,10.7987693895041));
#68024=CARTESIAN_POINT('Ctrl Pts',(88.1892343164074,62.626189479526,10.8066445604288));
#68025=CARTESIAN_POINT('Ctrl Pts',(88.2746226438355,62.6177857247768,10.8235397279944));
#68026=CARTESIAN_POINT('Ctrl Pts',(88.2916660001255,62.6160916433296,10.8272785006196));
#68027=CARTESIAN_POINT('Ctrl Pts',(88.3193309958117,62.6133104794803,10.8339475442777));
#68028=CARTESIAN_POINT('Ctrl Pts',(88.3300015623747,62.6122300912854,10.8366671560904));
#68029=CARTESIAN_POINT('Ctrl Pts',(88.3491433812361,62.6102772115095,10.8418118300876));
#68030=CARTESIAN_POINT('Ctrl Pts',(88.3576274477218,62.6094063786029,10.8441869929377));
#68031=CARTESIAN_POINT('Ctrl Pts',(88.3757776516177,62.6075315428667,10.8494724986596));
#68032=CARTESIAN_POINT('Ctrl Pts',(88.385435092201,62.606526705791,10.8524101832707));
#68033=CARTESIAN_POINT('Ctrl Pts',(88.4120432692606,62.6037372065946,10.8608519161765));
#68034=CARTESIAN_POINT('Ctrl Pts',(88.4289139243583,62.6019447918908,10.866597866962));
#68035=CARTESIAN_POINT('Ctrl Pts',(88.4569810053032,62.5989207250518,10.8768212125249));
#68036=CARTESIAN_POINT('Ctrl Pts',(88.4682451948143,62.5976955105722,10.8811067336158));
#68037=CARTESIAN_POINT('Ctrl Pts',(88.4976272202324,62.5944685153569,10.8927666250495));
#68038=CARTESIAN_POINT('Ctrl Pts',(88.5156379010013,62.5924589797896,10.9004001137468));
#68039=CARTESIAN_POINT('Ctrl Pts',(88.6012220653557,62.5827559232614,10.939028674083));
#68040=CARTESIAN_POINT('Ctrl Pts',(88.6661560173032,62.5749135399887,10.9754981660358));
#68041=CARTESIAN_POINT('Ctrl Pts',(88.7748062549928,62.5610482153719,11.0497420662984));
#68042=CARTESIAN_POINT('Ctrl Pts',(88.8198610111603,62.5550388882672,11.0852216938908));
#68043=CARTESIAN_POINT('Ctrl Pts',(88.869745794583,62.5481756287941,11.1302893566437));
#68044=CARTESIAN_POINT('Ctrl Pts',(88.8770414251558,62.5471662782208,11.1370376648898));
#68045=CARTESIAN_POINT('Ctrl Pts',(88.8883443961492,62.5455945830015,11.1477415981505));
#68046=CARTESIAN_POINT('Ctrl Pts',(88.8924056700894,62.545028215541,11.151639167899));
#68047=CARTESIAN_POINT('Ctrl Pts',(88.9000551195701,62.5439585387242,11.1590786086015));
#68048=CARTESIAN_POINT('Ctrl Pts',(88.9036481661449,62.5434548835483,11.1626148832188));
#68049=CARTESIAN_POINT('Ctrl Pts',(88.9122465863263,62.5422464217476,11.1711788356179));
#68050=CARTESIAN_POINT('Ctrl Pts',(88.917231086483,62.5415432302122,11.1762272468921));
#68051=CARTESIAN_POINT('Ctrl Pts',(88.9347252923499,62.5390645134546,11.1942452928932));
#68052=CARTESIAN_POINT('Ctrl Pts',(88.9470019555683,62.5373053718389,11.2074400754319));
#68053=CARTESIAN_POINT('Ctrl Pts',(88.9691707308139,62.53408076329,11.2323077897075));
#68054=CARTESIAN_POINT('Ctrl Pts',(88.9791403513253,62.5326114648582,11.2439062299215));
#68055=CARTESIAN_POINT('Ctrl Pts',(89.0310413237334,62.5248397364948,11.3065408089215));
#68056=CARTESIAN_POINT('Ctrl Pts',(89.0691562555416,62.5186887949476,11.360613900233));
#68057=CARTESIAN_POINT('Ctrl Pts',(89.1402993869349,62.505629442459,11.4803828552764));
#68058=CARTESIAN_POINT('Ctrl Pts',(89.1721808417437,62.4987329955045,11.5464610835943));
#68059=CARTESIAN_POINT('Ctrl Pts',(89.2038215845881,62.4900957292954,11.6297338543119));
#68060=CARTESIAN_POINT('Ctrl Pts',(89.2091757823394,62.488549889618,11.6446613909262));
#68061=CARTESIAN_POINT('Ctrl Pts',(89.2173468917407,62.4860452898067,11.6688590334791));
#68062=CARTESIAN_POINT('Ctrl Pts',(89.2203398312756,62.4850923523463,11.6780683951022));
#68063=CARTESIAN_POINT('Ctrl Pts',(89.2258783888689,62.4832577023811,11.6957979444549));
#68064=CARTESIAN_POINT('Ctrl Pts',(89.2284404166907,62.4823765853551,11.704312450803));
#68065=CARTESIAN_POINT('Ctrl Pts',(89.2341781972224,62.4803248618264,11.7241330618631));
#68066=CARTESIAN_POINT('Ctrl Pts',(89.2372868869979,62.4791521623453,11.7354574876019));
#68067=CARTESIAN_POINT('Ctrl Pts',(89.2469419002753,62.4752986946338,11.7726415753913));
#68068=CARTESIAN_POINT('Ctrl Pts',(89.2528300575248,62.4725973993981,11.79866241952));
#68069=CARTESIAN_POINT('Ctrl Pts',(89.265179396688,62.4659498580604,11.8625153029414));
#68070=CARTESIAN_POINT('Ctrl Pts',(89.2707530312328,62.461980084049,11.900489853666));
#68071=CARTESIAN_POINT('Ctrl Pts',(89.2794593312291,62.4529141160188,11.9868788144894));
#68072=CARTESIAN_POINT('Ctrl Pts',(89.2815544512035,62.4478030726399,12.0353394041807));
#68073=CARTESIAN_POINT('Ctrl Pts',(89.2800023232546,62.4361275012476,12.1460834024374));
#68074=CARTESIAN_POINT('Ctrl Pts',(89.2745478735421,62.4295773198751,12.2082301121597));
#68075=CARTESIAN_POINT('Ctrl Pts',(89.2629462537092,62.4221932266182,12.2796135867246));
#68076=CARTESIAN_POINT('Ctrl Pts',(89.2612237193261,62.4211764415598,12.2894745198848));
#68077=CARTESIAN_POINT('Ctrl Pts',(89.2583477839624,62.4195957976267,12.3048626418574));
#68078=CARTESIAN_POINT('Ctrl Pts',(89.2572738835781,62.4190278435774,12.3104039023854));
#68079=CARTESIAN_POINT('Ctrl Pts',(89.255171880457,62.4179570729542,12.3208758451309));
#68080=CARTESIAN_POINT('Ctrl Pts',(89.2541513827881,62.4174538965239,12.3258076326089));
#68081=CARTESIAN_POINT('Ctrl Pts',(89.2516296345187,62.4162491598077,12.3376394076895));
#68082=CARTESIAN_POINT('Ctrl Pts',(89.2501001246333,62.4155491883655,12.3445332072949));
#68083=CARTESIAN_POINT('Ctrl Pts',(89.244513063512,62.4130952176246,12.3687578668005));
#68084=CARTESIAN_POINT('Ctrl Pts',(89.2401484677956,62.4113571725731,12.3860171302879));
#68085=CARTESIAN_POINT('Ctrl Pts',(89.2314330436529,62.408178850244,12.4176659301506));
#68086=CARTESIAN_POINT('Ctrl Pts',(89.2271870719114,62.4067346972337,12.432080318919));
#68087=CARTESIAN_POINT('Ctrl Pts',(89.2035260151192,62.3991845513688,12.5074444266972));
#68088=CARTESIAN_POINT('Ctrl Pts',(89.1797809556355,62.3932219515589,12.5669432457179));
#68089=CARTESIAN_POINT('Ctrl Pts',(89.1210479956575,62.3807034005792,12.6869169268394));
#68090=CARTESIAN_POINT('Ctrl Pts',(89.0853626190001,62.3741605695807,12.7467988218024));
#68091=CARTESIAN_POINT('Ctrl Pts',(89.0348245758325,62.3657577642902,12.8176566415711));
#68092=CARTESIAN_POINT('Ctrl Pts',(89.0244013519534,62.364063565159,12.8316514216929));
#68093=CARTESIAN_POINT('Ctrl Pts',(89.0069354096129,62.3612822479815,12.8541205011843));
#68094=CARTESIAN_POINT('Ctrl Pts',(89.0000645723537,62.3602018254031,12.8627261245267));
#68095=CARTESIAN_POINT('Ctrl Pts',(88.9874967836739,62.3582489085707,12.8780539721045));
#68096=CARTESIAN_POINT('Ctrl Pts',(88.9818400409602,62.3573780732614,12.8848084190568));
#68097=CARTESIAN_POINT('Ctrl Pts',(88.9695524438061,62.3555032600932,12.899174113933));
#68098=CARTESIAN_POINT('Ctrl Pts',(88.9629002557104,62.3544984481892,12.9067661861288));
#68099=CARTESIAN_POINT('Ctrl Pts',(88.9442556777132,62.3517090953319,12.927540135494));
#68100=CARTESIAN_POINT('Ctrl Pts',(88.9320758217262,62.3499168031515,12.9405494913639));
#68101=CARTESIAN_POINT('Ctrl Pts',(88.91120774864,62.3468929722629,12.9619192088314));
#68102=CARTESIAN_POINT('Ctrl Pts',(88.9026664921936,62.3456678705976,12.970420290242));
#68103=CARTESIAN_POINT('Ctrl Pts',(88.8799489236012,62.3424412366849,12.9923963938229));
#68104=CARTESIAN_POINT('Ctrl Pts',(88.8655806194148,62.3404319516515,13.0056671632343));
#68105=CARTESIAN_POINT('Ctrl Pts',(88.7951641216555,62.3307308995756,13.0677537629437));
#68106=CARTESIAN_POINT('Ctrl Pts',(88.7352149377256,62.3228903338298,13.1119129491414));
#68107=CARTESIAN_POINT('Ctrl Pts',(88.6228297269834,62.3090244060096,13.1803819340748));
#68108=CARTESIAN_POINT('Ctrl Pts',(88.5719311668976,62.3030127076248,13.2068509874287));
#68109=CARTESIAN_POINT('Ctrl Pts',(88.5103050122751,62.2961471849633,13.2337727751677));
#68110=CARTESIAN_POINT('Ctrl Pts',(88.501151844084,62.2951378245419,13.2376441190833));
#68111=CARTESIAN_POINT('Ctrl Pts',(88.4867442014944,62.2935661173436,13.2435394418066));
#68112=CARTESIAN_POINT('Ctrl Pts',(88.4815204377722,62.2929997476592,13.2456364713034));
#68113=CARTESIAN_POINT('Ctrl Pts',(88.4715918361634,62.2919300691468,13.2495457643093));
#68114=CARTESIAN_POINT('Ctrl Pts',(88.4668900937431,62.2914264144808,13.2513647709104));
#68115=CARTESIAN_POINT('Ctrl Pts',(88.4555461109623,62.2902179572032,13.2556760400377));
#68116=CARTESIAN_POINT('Ctrl Pts',(88.4488935667797,62.2895147696475,13.2581407458328));
#68117=CARTESIAN_POINT('Ctrl Pts',(88.4252721772428,62.287036084062,13.2666678300997));
#68118=CARTESIAN_POINT('Ctrl Pts',(88.408194066485,62.2852769690884,13.2724251607249));
#68119=CARTESIAN_POINT('Ctrl Pts',(88.3764063644706,62.2820524191901,13.282393040631));
#68120=CARTESIAN_POINT('Ctrl Pts',(88.3617327589074,62.2805831527074,13.2867048898454));
#68121=CARTESIAN_POINT('Ctrl Pts',(88.2832901774769,62.2728117103869,13.3082239202145));
#68122=CARTESIAN_POINT('Ctrl Pts',(88.2183243942324,62.266661012315,13.3207033314787));
#68123=CARTESIAN_POINT('Ctrl Pts',(88.0798879341141,62.2536015935324,13.3362438765491));
#68124=CARTESIAN_POINT('Ctrl Pts',(88.0065406774849,62.2467048311341,13.3381015112467));
#68125=CARTESIAN_POINT('Ctrl Pts',(87.9176221056591,62.2380672313637,13.3326617742859));
#68126=CARTESIAN_POINT('Ctrl Pts',(87.901813929081,62.2365213945311,13.3313971036218));
#68127=CARTESIAN_POINT('Ctrl Pts',(87.8763978805762,62.2340167981256,13.3288840167805));
#68128=CARTESIAN_POINT('Ctrl Pts',(87.8667729144214,62.2330638611957,13.3278210274302));
#68129=CARTESIAN_POINT('Ctrl Pts',(87.8483351807288,62.2312292114518,13.3255710453545));
#68130=CARTESIAN_POINT('Ctrl Pts',(87.8395208366278,62.2303480941103,13.3244013461605));
#68131=CARTESIAN_POINT('Ctrl Pts',(87.8190953670635,62.2282963686421,13.3214722289983));
#68132=CARTESIAN_POINT('Ctrl Pts',(87.8074951481664,62.2271236675252,13.3196441510184));
#68133=CARTESIAN_POINT('Ctrl Pts',(87.7696328270019,62.2232701887127,13.3131380993795));
#68134=CARTESIAN_POINT('Ctrl Pts',(87.7434947366105,62.2205688838502,13.3077939493914));
#68135=CARTESIAN_POINT('Ctrl Pts',(87.6802183364985,62.2139213128436,13.2927662722651));
#68136=CARTESIAN_POINT('Ctrl Pts',(87.6433154714811,62.209951518508,13.2822151990422));
#68137=CARTESIAN_POINT('Ctrl Pts',(87.5610003636374,62.200885550192,13.2545914120624));
#68138=CARTESIAN_POINT('Ctrl Pts',(87.5159730832973,62.1957745277555,13.2365541499383));
#68139=CARTESIAN_POINT('Ctrl Pts',(87.4157226182924,62.1841034336349,13.189574573481));
#68140=CARTESIAN_POINT('Ctrl Pts',(87.361365105638,62.1775576871242,13.1590470561495));
#68141=CARTESIAN_POINT('Ctrl Pts',(87.3011922078794,62.1701869844216,13.1191719957983));
#68142=CARTESIAN_POINT('Ctrl Pts',(87.2929892300229,62.1691794445907,13.1135967310127));
#68143=CARTESIAN_POINT('Ctrl Pts',(87.280190913868,62.167604071799,13.1046772150821));
#68144=CARTESIAN_POINT('Ctrl Pts',(87.2755515539515,62.1670322871443,13.1013974431837));
#68145=CARTESIAN_POINT('Ctrl Pts',(87.2669730803864,62.1659738993181,13.0952461809038));
#68146=CARTESIAN_POINT('Ctrl Pts',(87.2630284318849,62.1654868006496,13.0923831122532));
#68147=CARTESIAN_POINT('Ctrl Pts',(87.2590170003332,62.164990941786,13.0894361625684));
#68148=CARTESIAN_POINT('Ctrl Pts',(87.2589338756575,62.1649806663939,13.0893750804359));
#68149=CARTESIAN_POINT('Ctrl Pts',(87.2587683973564,62.164960210461,13.0892534517079));
#68150=CARTESIAN_POINT('Ctrl Pts',(87.2586860435144,62.1649500298977,13.0891929052359));
#68151=CARTESIAN_POINT('Ctrl Pts',(87.2585219935161,62.1649297496186,13.0890722653085));
#68152=CARTESIAN_POINT('Ctrl Pts',(87.25844029735,62.1649196499052,13.0890121720844));
#68153=CARTESIAN_POINT('Ctrl Pts',(87.2582774551191,62.1648995180339,13.0888923602115));
#68154=CARTESIAN_POINT('Ctrl Pts',(87.2581963090161,62.1648894858743,13.0888326417317));
#68155=CARTESIAN_POINT('Ctrl Pts',(87.2580344644899,62.1648694764549,13.088713504544));
#68156=CARTESIAN_POINT('Ctrl Pts',(87.2579537658418,62.1648594991696,13.0886540858292));
#68157=CARTESIAN_POINT('Ctrl Pts',(87.2577927172652,62.1648395872686,13.0885354757635));
#68158=CARTESIAN_POINT('Ctrl Pts',(87.2577123673709,62.164829652659,13.0884762845601));
#68159=CARTESIAN_POINT('Ctrl Pts',(87.2575519213096,62.1648098143674,13.088358059888));
#68160=CARTESIAN_POINT('Ctrl Pts',(87.2574718251357,62.164799910686,13.0882990265015));
#68161=CARTESIAN_POINT('Ctrl Pts',(87.2573117946532,62.1647801228943,13.0881810500028));
#68162=CARTESIAN_POINT('Ctrl Pts',(87.2572318602742,62.1647702387761,13.0881221068924));
#68163=CARTESIAN_POINT('Ctrl Pts',(87.2570720638502,62.1647504790402,13.0880042450705));
#68164=CARTESIAN_POINT('Ctrl Pts',(87.2569922018351,62.1647406034266,13.0879453264025));
#68165=CARTESIAN_POINT('Ctrl Pts',(87.2568324626802,62.1647208498836,13.08782744899));
#68166=CARTESIAN_POINT('Ctrl Pts',(87.2567525856333,62.1647109719655,13.0877684903037));
#68167=CARTESIAN_POINT('Ctrl Pts',(87.2565927311676,62.1646912032691,13.0876504698856));
#68168=CARTESIAN_POINT('Ctrl Pts',(87.256512753621,62.1646813124743,13.087591408018));
#68169=CARTESIAN_POINT('Ctrl Pts',(87.2508373134831,62.1639794167997,13.0833991755097));
#68170=CARTESIAN_POINT('Ctrl Pts',(87.2452756632314,62.1632904898426,13.0792199368835));
#68171=CARTESIAN_POINT('Ctrl Pts',(87.2329558257454,62.1617611950182,13.069802948668));
#68172=CARTESIAN_POINT('Ctrl Pts',(87.2262155353611,62.1609223058157,13.0645421645983));
#68173=CARTESIAN_POINT('Ctrl Pts',(87.2069824453511,62.1585204073847,13.0492157100055));
#68174=CARTESIAN_POINT('Ctrl Pts',(87.1946259607741,62.1569672034051,13.0389804022322));
#68175=CARTESIAN_POINT('Ctrl Pts',(87.181857685817,62.1553471829244,13.0279894317539));
#68176=CARTESIAN_POINT('Ctrl Pts',(87.1812500062644,62.1552700449772,13.0274653357362));
#68177=CARTESIAN_POINT('Ctrl Pts',(87.180642835277,62.1551929346177,13.0269406740237));
#68178=CARTESIAN_POINT('Origin',(88.011,66.41344859951,12.066));
#68179=CARTESIAN_POINT('',(87.1806429942553,61.1927093932679,13.0269408113983));
#68180=CARTESIAN_POINT('',(87.1806428320421,61.3633558149692,13.0269406712284));
#68181=CARTESIAN_POINT('',(87.1806428354228,66.41344859951,13.0269406741497));
#68182=CARTESIAN_POINT('',(86.7410004953938,61.8782514005452,12.0671217397436));
#68183=CARTESIAN_POINT('Ctrl Pts',(87.1806429942554,61.1927093932679,13.0269408113983));
#68184=CARTESIAN_POINT('Ctrl Pts',(87.226202739937,61.1983609392697,13.0663093693343));
#68185=CARTESIAN_POINT('Ctrl Pts',(87.2745233771969,61.2040483236492,13.1024044361032));
#68186=CARTESIAN_POINT('Ctrl Pts',(87.3398033310188,61.2115377385228,13.1442829214061));
#68187=CARTESIAN_POINT('Ctrl Pts',(87.3545464917767,61.2132169908147,13.1533213651565));
#68188=CARTESIAN_POINT('Ctrl Pts',(87.3789344233228,61.2159789596357,13.167595842728));
#68189=CARTESIAN_POINT('Ctrl Pts',(87.3884710784503,61.2170551410657,13.1730131061858));
#68190=CARTESIAN_POINT('Ctrl Pts',(87.4057913394993,61.2190036867216,13.1825572407154));
#68191=CARTESIAN_POINT('Ctrl Pts',(87.4135501138054,61.2198744265838,13.186727985794));
#68192=CARTESIAN_POINT('Ctrl Pts',(87.4303228075975,61.2217527048303,13.1955205187292));
#68193=CARTESIAN_POINT('Ctrl Pts',(87.4393498166435,61.2227611042524,13.2001158038841));
#68194=CARTESIAN_POINT('Ctrl Pts',(87.4645542245857,61.2255706365563,13.2125689926564));
#68195=CARTESIAN_POINT('Ctrl Pts',(87.4808442502163,61.2273797059881,13.2201915942497));
#68196=CARTESIAN_POINT('Ctrl Pts',(87.5178291351539,61.2314746860894,13.2365498283068));
#68197=CARTESIAN_POINT('Ctrl Pts',(87.5386043843642,61.2337664975491,13.2450872012963));
#68198=CARTESIAN_POINT('Ctrl Pts',(87.6092134874384,61.2415315852857,13.2719377200415));
#68199=CARTESIAN_POINT('Ctrl Pts',(87.6599609025706,61.2470756255832,13.2876743688528));
#68200=CARTESIAN_POINT('Ctrl Pts',(87.7935595927618,61.2615398492225,13.3200906863389));
#68201=CARTESIAN_POINT('Ctrl Pts',(87.8773693634491,61.2704976609898,13.3317683761111));
#68202=CARTESIAN_POINT('Ctrl Pts',(87.9732851900097,61.2803264147909,13.3354925817345));
#68203=CARTESIAN_POINT('Ctrl Pts',(87.9848509626102,61.2815043310443,13.3357834791417));
#68204=CARTESIAN_POINT('Ctrl Pts',(88.0024612729697,61.2832853737246,13.3359856668994));
#68205=CARTESIAN_POINT('Ctrl Pts',(88.0085033752815,61.2838942139818,13.3360119197725));
#68206=CARTESIAN_POINT('Ctrl Pts',(88.019015068809,61.2849493069948,13.3359825724927));
#68207=CARTESIAN_POINT('Ctrl Pts',(88.0234843566758,61.2853965855964,13.3359465023504));
#68208=CARTESIAN_POINT('Ctrl Pts',(88.0341075069042,61.2864566486703,13.3358046779072));
#68209=CARTESIAN_POINT('Ctrl Pts',(88.0402609381663,61.2870682604056,13.335677785987));
#68210=CARTESIAN_POINT('Ctrl Pts',(88.0589150464705,61.2889157031898,13.3351574213276));
#68211=CARTESIAN_POINT('Ctrl Pts',(88.0714116832344,61.2901442641383,13.3346240118687));
#68212=CARTESIAN_POINT('Ctrl Pts',(88.1347917163672,61.2963391007048,13.3309799269565));
#68213=CARTESIAN_POINT('Ctrl Pts',(88.1854705936178,61.3011749427533,13.3249917987697));
#68214=CARTESIAN_POINT('Ctrl Pts',(88.3269870846292,61.3147063336274,13.2995567484761));
#68215=CARTESIAN_POINT('Ctrl Pts',(88.4162328832904,61.3232923762391,13.2731847002324));
#68216=CARTESIAN_POINT('Ctrl Pts',(88.5266621450235,61.3347600478721,13.2269129237382));
#68217=CARTESIAN_POINT('Ctrl Pts',(88.5511776277616,61.337361531208,13.2157104656436));
#68218=CARTESIAN_POINT('Ctrl Pts',(88.5850962488991,61.3410536478627,13.1988868761668));
#68219=CARTESIAN_POINT('Ctrl Pts',(88.5948128305017,61.3421223011867,13.1939103413491));
#68220=CARTESIAN_POINT('Ctrl Pts',(88.6124264363243,61.3440806079502,13.1846006259585));
#68221=CARTESIAN_POINT('Ctrl Pts',(88.6203439220776,61.3449688157178,13.180307449877));
#68222=CARTESIAN_POINT('Ctrl Pts',(88.636308819522,61.3467764981403,13.1714296230262));
#68223=CARTESIAN_POINT('Ctrl Pts',(88.6443530586291,61.3476960896704,13.1668404347347));
#68224=CARTESIAN_POINT('Ctrl Pts',(88.664270802737,61.3499955643799,13.1551869140628));
#68225=CARTESIAN_POINT('Ctrl Pts',(88.676080217368,61.3513792163533,13.1480162388583));
#68226=CARTESIAN_POINT('Ctrl Pts',(88.7237582802333,61.3570514906309,13.1179907160773));
#68227=CARTESIAN_POINT('Ctrl Pts',(88.7585799835022,61.3613976006141,13.0935368368419));
#68228=CARTESIAN_POINT('Ctrl Pts',(88.8511827005763,61.3735549601707,13.0213045195983));
#68229=CARTESIAN_POINT('Ctrl Pts',(88.9060602632938,61.3814686671783,12.9700897233082));
#68230=CARTESIAN_POINT('Ctrl Pts',(88.9919041594862,61.3950012984119,12.8744555545538));
#68231=CARTESIAN_POINT('Ctrl Pts',(89.0251551104515,61.4006166018615,12.8323318759416));
#68232=CARTESIAN_POINT('Ctrl Pts',(89.0612864701626,61.4071026191606,12.7800704712377));
#68233=CARTESIAN_POINT('Ctrl Pts',(89.0668295745033,61.4081096824103,12.7718485950256));
#68234=CARTESIAN_POINT('Ctrl Pts',(89.0753655271757,61.4096786967616,12.7588619352497));
#68235=CARTESIAN_POINT('Ctrl Pts',(89.0784237862478,61.4102446480521,12.7541410479154));
#68236=CARTESIAN_POINT('Ctrl Pts',(89.084165076899,61.4113141920218,12.745148115447));
#68237=CARTESIAN_POINT('Ctrl Pts',(89.0868540583634,61.4118181258645,12.7408803538612));
#68238=CARTESIAN_POINT('Ctrl Pts',(89.0932705223589,61.4130281625144,12.7305607792229));
#68239=CARTESIAN_POINT('Ctrl Pts',(89.096972778952,61.4137326402702,12.7244934661483));
#68240=CARTESIAN_POINT('Ctrl Pts',(89.1099227638895,61.4162207128967,12.7028645260095));
#68241=CARTESIAN_POINT('Ctrl Pts',(89.118889226718,61.417987762615,12.6871354507227));
#68242=CARTESIAN_POINT('Ctrl Pts',(89.1348522018291,61.4212296792539,12.6576866943066));
#68243=CARTESIAN_POINT('Ctrl Pts',(89.1419411249495,61.4227083610607,12.6440217507854));
#68244=CARTESIAN_POINT('Ctrl Pts',(89.1784772357889,61.4305642392608,12.5703460703639));
#68245=CARTESIAN_POINT('Ctrl Pts',(89.2034028057491,61.4367868304831,12.5082050131075));
#68246=CARTESIAN_POINT('Ctrl Pts',(89.2447796625721,61.4498077663473,12.3756362576421));
#68247=CARTESIAN_POINT('Ctrl Pts',(89.2603471258637,61.4565921357858,12.3051982879379));
#68248=CARTESIAN_POINT('Ctrl Pts',(89.2719724658581,61.4651205091818,12.2179983969105));
#68249=CARTESIAN_POINT('Ctrl Pts',(89.273784087429,61.4666771594713,12.202129960316));
#68250=CARTESIAN_POINT('Ctrl Pts',(89.2762150400988,61.469195084633,12.1765674402439));
#68251=CARTESIAN_POINT('Ctrl Pts',(89.2770232738425,61.4701504239857,12.1668925845295));
#68252=CARTESIAN_POINT('Ctrl Pts',(89.2783587093729,61.4719869451115,12.1483460621131));
#68253=CARTESIAN_POINT('Ctrl Pts',(89.2789038635231,61.4728675102045,12.1394762193943));
#68254=CARTESIAN_POINT('Ctrl Pts',(89.2799507912079,61.4749138442851,12.1189213808966));
#68255=CARTESIAN_POINT('Ctrl Pts',(89.2803843078585,61.4760816687021,12.1072339482793));
#68256=CARTESIAN_POINT('Ctrl Pts',(89.2812698902079,61.4798999463446,12.0691742707471));
#68257=CARTESIAN_POINT('Ctrl Pts',(89.2810617980457,61.482570402152,12.0427957863362));
#68258=CARTESIAN_POINT('Ctrl Pts',(89.2785598504354,61.4891224931139,11.9787240779547));
#68259=CARTESIAN_POINT('Ctrl Pts',(89.2754059352939,61.4930267431569,11.9410918475918));
#68260=CARTESIAN_POINT('Ctrl Pts',(89.2643048376743,61.5020905419596,11.8549594080511));
#68261=CARTESIAN_POINT('Ctrl Pts',(89.2552093068928,61.5072678714401,11.8066667097667));
#68262=CARTESIAN_POINT('Ctrl Pts',(89.2281916228537,61.5190514146889,11.6982049817284));
#68263=CARTESIAN_POINT('Ctrl Pts',(89.2085572671254,61.5256434354852,11.6385802708363));
#68264=CARTESIAN_POINT('Ctrl Pts',(89.1808091521236,61.533056949719,11.5714853649247));
#68265=CARTESIAN_POINT('Ctrl Pts',(89.1769151936337,61.5340635645813,11.5623731936873));
#68266=CARTESIAN_POINT('Ctrl Pts',(89.1706217593238,61.5356378866358,11.548110399672));
#68267=CARTESIAN_POINT('Ctrl Pts',(89.1682938354428,61.5362095362179,11.5429290240215));
#68268=CARTESIAN_POINT('Ctrl Pts',(89.1638403235007,61.5372830838689,11.5331919133314));
#68269=CARTESIAN_POINT('Ctrl Pts',(89.1617224284848,61.5377853733405,11.5286331204347));
#68270=CARTESIAN_POINT('Ctrl Pts',(89.156594195425,61.5389823720837,11.5177639037361));
#68271=CARTESIAN_POINT('Ctrl Pts',(89.1535587111232,61.5396755483464,11.5114655305448));
#68272=CARTESIAN_POINT('Ctrl Pts',(89.14281586985,61.5420774524038,11.4896378021043));
#68273=CARTESIAN_POINT('Ctrl Pts',(89.134842125066,61.5437711118576,11.4742403089391));
#68274=CARTESIAN_POINT('Ctrl Pts',(89.113855017367,61.5480252175316,11.4356692392767));
#68275=CARTESIAN_POINT('Ctrl Pts',(89.1004245704549,61.5505659213823,11.4127309658727));
#68276=CARTESIAN_POINT('Ctrl Pts',(89.0557922227107,61.5585246538168,11.3417122335432));
#68277=CARTESIAN_POINT('Ctrl Pts',(89.0220510698514,61.5638656778992,11.295311950015));
#68278=CARTESIAN_POINT('Ctrl Pts',(88.9394071484531,61.5759464932351,11.1964734289822));
#68279=CARTESIAN_POINT('Ctrl Pts',(88.8889789013189,61.5826865179429,11.1455834825062));
#68280=CARTESIAN_POINT('Ctrl Pts',(88.8224299876539,61.5911621594658,11.0888948065194));
#68281=CARTESIAN_POINT('Ctrl Pts',(88.8101249990369,61.5927131332464,11.0788058115395));
#68282=CARTESIAN_POINT('Ctrl Pts',(88.7900221656423,61.5952241294975,11.0629454251947));
#68283=CARTESIAN_POINT('Ctrl Pts',(88.7823417024375,61.596178276283,11.0570272651263));
#68284=CARTESIAN_POINT('Ctrl Pts',(88.7674906014966,61.5980139905157,11.0458524576989));
#68285=CARTESIAN_POINT('Ctrl Pts',(88.7603310135025,61.5988949526088,11.040582007087));
#68286=CARTESIAN_POINT('Ctrl Pts',(88.7436039352837,61.6009444295243,11.0285372807499));
#68287=CARTESIAN_POINT('Ctrl Pts',(88.733996992695,61.6021150205043,11.0218195823129));
#68288=CARTESIAN_POINT('Ctrl Pts',(88.7023402600098,61.6059527369942,11.0003297774613));
#68289=CARTESIAN_POINT('Ctrl Pts',(88.6799220277723,61.6086401519575,10.9861169365844));
#68290=CARTESIAN_POINT('Ctrl Pts',(88.6242867486978,61.6152445478641,10.9532421660584));
#68291=CARTESIAN_POINT('Ctrl Pts',(88.590645310124,61.6191846396407,10.9353535975616));
#68292=CARTESIAN_POINT('Ctrl Pts',(88.5122164309577,61.6282501476519,10.8980703179564));
#68293=CARTESIAN_POINT('Ctrl Pts',(88.4670114113355,61.6333917404362,10.8796903120918));
#68294=CARTESIAN_POINT('Ctrl Pts',(88.3617473026455,61.6451159608629,10.8437980755069));
#68295=CARTESIAN_POINT('Ctrl Pts',(88.3012138961776,61.651684309547,10.828026048106));
#68296=CARTESIAN_POINT('Ctrl Pts',(88.2299044629803,61.6590863666561,10.8149679612656));
#68297=CARTESIAN_POINT('Ctrl Pts',(88.2200304442919,61.6601038679105,10.8132803098658));
#68298=CARTESIAN_POINT('Ctrl Pts',(88.2045604724411,61.6616854468799,10.8108242257314));
#68299=CARTESIAN_POINT('Ctrl Pts',(88.1989779641956,61.6622536262999,10.8099760470663));
#68300=CARTESIAN_POINT('Ctrl Pts',(88.1884048909593,61.6633247015835,10.8084417002965));
#68301=CARTESIAN_POINT('Ctrl Pts',(88.1834158400728,61.6638279583402,10.8077479773424));
#68302=CARTESIAN_POINT('Ctrl Pts',(88.171423457607,61.6650327421636,10.8061531175499));
#68303=CARTESIAN_POINT('Ctrl Pts',(88.1644164746966,61.6657326811863,10.8052806629401));
#68304=CARTESIAN_POINT('Ctrl Pts',(88.139729985067,61.6681858268034,10.8024157697009));
#68305=CARTESIAN_POINT('Ctrl Pts',(88.1220149268341,61.6699230956557,10.8007362655214));
#68306=CARTESIAN_POINT('Ctrl Pts',(88.0892954620566,61.6730996258294,10.7983268409895));
#68307=CARTESIAN_POINT('Ctrl Pts',(88.074302830087,61.6745427657311,10.7974897626058));
#68308=CARTESIAN_POINT('Ctrl Pts',(87.9954649992886,61.6820838362316,10.7944893949248));
#68309=CARTESIAN_POINT('Ctrl Pts',(87.9315334858944,61.6880387094762,10.7968793578557));
#68310=CARTESIAN_POINT('Ctrl Pts',(87.7987559737044,61.700561632184,10.811920470054));
#68311=CARTESIAN_POINT('Ctrl Pts',(87.7302385640439,61.7071167161125,10.825462338102));
#68312=CARTESIAN_POINT('Ctrl Pts',(87.6464175564511,61.7155311713836,10.8493309375516));
#68313=CARTESIAN_POINT('Ctrl Pts',(87.6297506195043,61.7172239940159,10.8544502459733));
#68314=CARTESIAN_POINT('Ctrl Pts',(87.6027402170429,61.7200036371134,10.863359093958));
#68315=CARTESIAN_POINT('Ctrl Pts',(87.5923308708438,61.7210837777869,10.8669431452794));
#68316=CARTESIAN_POINT('Ctrl Pts',(87.573676054421,61.7230365610186,10.8736387231184));
#68317=CARTESIAN_POINT('Ctrl Pts',(87.5654137575607,61.7239075479385,10.8767016612133));
#68318=CARTESIAN_POINT('Ctrl Pts',(87.5564992318225,61.7248541601265,10.8801123199549));
#68319=CARTESIAN_POINT('Ctrl Pts',(87.5558144310191,61.7249269215843,10.8803750020591));
#68320=CARTESIAN_POINT('Ctrl Pts',(87.5547625100692,61.7250387582622,10.8807795531267));
#68321=CARTESIAN_POINT('Ctrl Pts',(87.5543952263649,61.7250778193648,10.8809210002714));
#68322=CARTESIAN_POINT('Ctrl Pts',(87.5538322525775,61.7251377119292,10.8811381115352));
#68323=CARTESIAN_POINT('Ctrl Pts',(87.5536365150372,61.7251585393026,10.8812136535888));
#68324=CARTESIAN_POINT('Ctrl Pts',(87.5530826468201,61.7252174836991,10.8814275686724));
#68325=CARTESIAN_POINT('Ctrl Pts',(87.5527245605298,61.7252556045258,10.8815660554584));
#68326=CARTESIAN_POINT('Ctrl Pts',(87.5520467871796,61.7253277813617,10.8818285318353));
#68327=CARTESIAN_POINT('Ctrl Pts',(87.5517270873131,61.7253618362699,10.8819524886031));
#68328=CARTESIAN_POINT('Ctrl Pts',(87.5511216901121,61.7254263425105,10.8821875004668));
#68329=CARTESIAN_POINT('Ctrl Pts',(87.5508359826368,61.7254567929691,10.8822985295776));
#68330=CARTESIAN_POINT('Ctrl Pts',(87.5502947119431,61.7255144958882,10.8825090989883));
#68331=CARTESIAN_POINT('Ctrl Pts',(87.5500391406471,61.7255417476572,10.8826086186872));
#68332=CARTESIAN_POINT('Ctrl Pts',(87.549554755207,61.7255934098882,10.8827974195494));
#68333=CARTESIAN_POINT('Ctrl Pts',(87.5493259346289,61.7256178198007,10.8828866843406));
#68334=CARTESIAN_POINT('Ctrl Pts',(87.5488920745094,61.7256641122354,10.8830560817768));
#68335=CARTESIAN_POINT('Ctrl Pts',(87.5486870298516,61.725685994318,10.8831362013761));
#68336=CARTESIAN_POINT('Ctrl Pts',(87.5482981034366,61.7257275076507,10.8832882879127));
#68337=CARTESIAN_POINT('Ctrl Pts',(87.5481142175871,61.7257471385503,10.8833602444397));
#68338=CARTESIAN_POINT('Ctrl Pts',(87.547765302289,61.7257843934745,10.8834968726241));
#68339=CARTESIAN_POINT('Ctrl Pts',(87.5476002695476,61.7258020172203,10.8835615359632));
#68340=CARTESIAN_POINT('Ctrl Pts',(87.5472870252589,61.7258354733534,10.8836843473908));
#68341=CARTESIAN_POINT('Ctrl Pts',(87.5471388110959,61.7258513055146,10.8837424888053));
#68342=CARTESIAN_POINT('Ctrl Pts',(87.5468574054316,61.725881369135,10.8838529396122));
#68343=CARTESIAN_POINT('Ctrl Pts',(87.5467242117966,61.7258956004162,10.8839052436609));
#68344=CARTESIAN_POINT('Ctrl Pts',(87.546471255137,61.7259226312072,10.884004627016));
#68345=CARTESIAN_POINT('Ctrl Pts',(87.5463514903956,61.7259354305739,10.8840517020267));
#68346=CARTESIAN_POINT('Ctrl Pts',(87.5461239800973,61.7259597474311,10.8841411676831));
#68347=CARTESIAN_POINT('Ctrl Pts',(87.5460162331613,61.7259712648059,10.8841835548688));
#68348=CARTESIAN_POINT('Ctrl Pts',(87.5458115050845,61.7259931508957,10.8842641263541));
#68349=CARTESIAN_POINT('Ctrl Pts',(87.5457145229153,61.7260035195085,10.884302307831));
#68350=CARTESIAN_POINT('Ctrl Pts',(87.5455302102126,61.7260232265774,10.8843748971836));
#68351=CARTESIAN_POINT('Ctrl Pts',(87.5454428787162,61.7260325649649,10.8844093028326));
#68352=CARTESIAN_POINT('Ctrl Pts',(87.5343117565712,61.7272229135989,10.8887960132382));
#68353=CARTESIAN_POINT('Ctrl Pts',(87.5233300207363,61.7284090700988,10.8933027353222));
#68354=CARTESIAN_POINT('Ctrl Pts',(87.486257465773,61.7324550371401,10.9091274622259));
#68355=CARTESIAN_POINT('Ctrl Pts',(87.4604866248465,61.7353387217691,10.9211666098219));
#68356=CARTESIAN_POINT('Ctrl Pts',(87.3973577272725,61.7425910885303,10.9532823833756));
#68357=CARTESIAN_POINT('Ctrl Pts',(87.3605625577542,61.7469899738083,10.9743830338249));
#68358=CARTESIAN_POINT('Ctrl Pts',(87.2545094905754,61.7601843116504,11.0424678188431));
#68359=CARTESIAN_POINT('Ctrl Pts',(87.1887610927681,61.7690748134121,11.0944963736558));
#68360=CARTESIAN_POINT('Ctrl Pts',(87.1113234548237,61.7802588183569,11.1693063588163));
#68361=CARTESIAN_POINT('Ctrl Pts',(87.0945173811954,61.7827345799203,11.1864903452943));
#68362=CARTESIAN_POINT('Ctrl Pts',(87.0726913868365,61.7860060052116,11.2101127332265));
#68363=CARTESIAN_POINT('Ctrl Pts',(87.0672325659757,61.7868291470079,11.2161358284276));
#68364=CARTESIAN_POINT('Ctrl Pts',(87.0586961424002,61.7881237265417,11.2257383531058));
#68365=CARTESIAN_POINT('Ctrl Pts',(87.0555801800205,61.7885978602121,11.2292830569781));
#68366=CARTESIAN_POINT('Ctrl Pts',(87.0490945564464,61.7895879368212,11.2367445442307));
#68367=CARTESIAN_POINT('Ctrl Pts',(87.0457289068002,61.7901035573684,11.2406646666474));
#68368=CARTESIAN_POINT('Ctrl Pts',(87.038963018133,61.7911440990802,11.2486432019622));
#68369=CARTESIAN_POINT('Ctrl Pts',(87.03556402159,61.791668930026,11.2527025851185));
#68370=CARTESIAN_POINT('Ctrl Pts',(87.0231015165286,61.7936015669048,11.2677769386517));
#68371=CARTESIAN_POINT('Ctrl Pts',(87.0141978009505,61.7949988132923,11.278923823769));
#68372=CARTESIAN_POINT('Ctrl Pts',(86.9741931207279,61.8013673011782,11.3307753020688));
#68373=CARTESIAN_POINT('Ctrl Pts',(86.9453803986258,61.8062149785939,11.3731938484325));
#68374=CARTESIAN_POINT('Ctrl Pts',(86.8784122344624,61.8185380260373,11.485894800254));
#68375=CARTESIAN_POINT('Ctrl Pts',(86.8441872383224,61.825949051452,11.5582361458506));
#68376=CARTESIAN_POINT('Ctrl Pts',(86.8054383949488,61.8367836788245,11.6651643772905));
#68377=CARTESIAN_POINT('Ctrl Pts',(86.7951754145612,61.8400401063371,11.6974649176347));
#68378=CARTESIAN_POINT('Ctrl Pts',(86.7827442295446,61.8446159864587,11.7427970119311));
#68379=CARTESIAN_POINT('Ctrl Pts',(86.7794684810918,61.8459000410156,11.7555124866401));
#68380=CARTESIAN_POINT('Ctrl Pts',(86.7744647080963,61.8479977955314,11.776262251709));
#68381=CARTESIAN_POINT('Ctrl Pts',(86.7726164071108,61.8488076090809,11.7842668641605));
#68382=CARTESIAN_POINT('Ctrl Pts',(86.7690484418068,61.8504446302505,11.8004328946085));
#68383=CARTESIAN_POINT('Ctrl Pts',(86.7673312634105,61.8512718735468,11.8085944337633));
#68384=CARTESIAN_POINT('Ctrl Pts',(86.7639520337192,61.8529852793786,11.8254792687191));
#68385=CARTESIAN_POINT('Ctrl Pts',(86.7623008505689,61.8538717398495,11.8342042358313));
#68386=CARTESIAN_POINT('Ctrl Pts',(86.7586393092271,61.8559599218336,11.8547278035169));
#68387=CARTESIAN_POINT('Ctrl Pts',(86.7567040227462,61.8571639310088,11.8665386826224));
#68388=CARTESIAN_POINT('Ctrl Pts',(86.745598878384,61.8647592814387,11.9408824265292));
#68389=CARTESIAN_POINT('Ctrl Pts',(86.7409429218177,61.8712869956939,12.0039849629062));
#68390=CARTESIAN_POINT('Ctrl Pts',(86.7410005280162,61.8779044320784,12.0671580849455));
#68391=CARTESIAN_POINT('Ctrl Pts',(87.1806428354228,61.9866340346925,13.0269406741497));
#68392=CARTESIAN_POINT('Ctrl Pts',(87.1430320818341,61.9817037570677,12.994440896018));
#68393=CARTESIAN_POINT('Ctrl Pts',(87.1073198343453,61.9767734794429,12.959719041223));
#68394=CARTESIAN_POINT('Ctrl Pts',(87.0737708946988,61.9718432018181,12.9230306903352));
#68395=CARTESIAN_POINT('Ctrl Pts',(87.0401932787146,61.9669087099825,12.8863109796621));
#68396=CARTESIAN_POINT('Ctrl Pts',(87.0087830388915,61.9619742181468,12.8476218169232));
#68397=CARTESIAN_POINT('Ctrl Pts',(86.9797666153935,61.9570397263112,12.8072541443209));
#68398=CARTESIAN_POINT('Ctrl Pts',(86.9507389769443,61.9521033272768,12.7668708694692));
#68399=CARTESIAN_POINT('Ctrl Pts',(86.9241072961311,61.9471669282425,12.7248082534978));
#68400=CARTESIAN_POINT('Ctrl Pts',(86.9000542692074,61.9422305292081,12.6813857190687));
#68401=CARTESIAN_POINT('Ctrl Pts',(86.8759531642927,61.937284263135,12.637876390232));
#68402=CARTESIAN_POINT('Ctrl Pts',(86.8544412525289,61.9323379970619,12.5930022062731));
#68403=CARTESIAN_POINT('Ctrl Pts',(86.8356542887356,61.9273917309888,12.5471054551886));
#68404=CARTESIAN_POINT('Ctrl Pts',(86.8186942982478,61.9229264737779,12.5056720191969));
#68405=CARTESIAN_POINT('Ctrl Pts',(86.8039544882604,61.9184612165669,12.4634057728746));
#68406=CARTESIAN_POINT('Ctrl Pts',(86.7914994313964,61.913995959356,12.4205678541202));
#68407=CARTESIAN_POINT('Ctrl Pts',(86.7744754181363,61.9078926875044,12.36201546814));
#68408=CARTESIAN_POINT('Ctrl Pts',(86.761658527776,61.9017894156528,12.3021883648507));
#68409=CARTESIAN_POINT('Ctrl Pts',(86.7532024055706,61.8956861438012,12.2416280485787));
#68410=CARTESIAN_POINT('Ctrl Pts',(86.7451504227884,61.8898745627158,12.1839620626737));
#68411=CARTESIAN_POINT('Ctrl Pts',(86.7410521745367,61.8840629816305,12.1256312882053));
#68412=CARTESIAN_POINT('Ctrl Pts',(86.7410004953938,61.8782514005452,12.0671217397436));
#68413=CARTESIAN_POINT('',(86.7409997144605,62.0467094537538,12.065715168206));
#68414=CARTESIAN_POINT('Ctrl Pts',(87.180642835277,62.1551929346177,13.0269406740237));
#68415=CARTESIAN_POINT('Ctrl Pts',(87.1258041329939,62.1482284515714,12.9795540761038));
#68416=CARTESIAN_POINT('Ctrl Pts',(87.0751143957215,62.1414835135495,12.9275532301801));
#68417=CARTESIAN_POINT('Ctrl Pts',(86.982329632258,62.1277709095857,12.8144534499568));
#68418=CARTESIAN_POINT('Ctrl Pts',(86.940595638107,62.1208256454524,12.7534422569748));
#68419=CARTESIAN_POINT('Ctrl Pts',(86.8965423834688,62.112122338035,12.6752129982176));
#68420=CARTESIAN_POINT('Ctrl Pts',(86.8889524671294,62.1105621404608,12.6611180850041));
#68421=CARTESIAN_POINT('Ctrl Pts',(86.8771878063937,62.1080400149971,12.6382449579432));
#68422=CARTESIAN_POINT('Ctrl Pts',(86.8728436805683,62.1070840610393,12.6295552872296));
#68423=CARTESIAN_POINT('Ctrl Pts',(86.8647194887141,62.1052473721894,12.6128271058738));
#68424=CARTESIAN_POINT('Ctrl Pts',(86.8609232129233,62.1043672614304,12.6047970563204));
#68425=CARTESIAN_POINT('Ctrl Pts',(86.8523328864518,62.1023234980466,12.5861219212143));
#68426=CARTESIAN_POINT('Ctrl Pts',(86.8476008686531,62.1011578049328,12.5754494388245));
#68427=CARTESIAN_POINT('Ctrl Pts',(86.8327056874406,62.0973535821993,12.5405650531874));
#68428=CARTESIAN_POINT('Ctrl Pts',(86.8231469645094,62.094695252629,12.51610485739));
#68429=CARTESIAN_POINT('Ctrl Pts',(86.8017898676855,62.088180254359,12.4560230689288));
#68430=CARTESIAN_POINT('Ctrl Pts',(86.7907994632039,62.0843013155685,12.4201428434782));
#68431=CARTESIAN_POINT('Ctrl Pts',(86.7691936428836,62.0752925712175,12.3365573507273));
#68432=CARTESIAN_POINT('Ctrl Pts',(86.7597109154249,62.0701449566621,12.2886192700193));
#68433=CARTESIAN_POINT('Ctrl Pts',(86.7450013314751,62.0588429392308,12.1824289822729));
#68434=CARTESIAN_POINT('Ctrl Pts',(86.7409870002166,62.0527003764799,12.1241101969471));
#68435=CARTESIAN_POINT('Ctrl Pts',(86.7410000316247,62.04670904774,12.0657165805304));
#68436=CARTESIAN_POINT('Ctrl Pts',(86.7410000319281,62.0467089085791,12.0657152242193));
#68437=CARTESIAN_POINT('Ctrl Pts',(86.7410028199225,62.0454332038684,12.0532817480931));
#68438=CARTESIAN_POINT('Ctrl Pts',(86.7411881963702,62.0441648464695,12.0408480693285));
#68439=CARTESIAN_POINT('Ctrl Pts',(86.7417089181389,62.0423826618144,12.0232590341084));
#68440=CARTESIAN_POINT('Ctrl Pts',(86.7418931107228,62.0418614665008,12.0181006513168));
#68441=CARTESIAN_POINT('Ctrl Pts',(86.7423038126814,62.0408720051917,12.0082783886585));
#68442=CARTESIAN_POINT('Ctrl Pts',(86.7425246029727,62.0404034401319,12.0036143389891));
#68443=CARTESIAN_POINT('Ctrl Pts',(86.7430549289509,62.0393985551119,11.9935831833163));
#68444=CARTESIAN_POINT('Ctrl Pts',(86.7433728278458,62.038862708404,11.9882166152299));
#68445=CARTESIAN_POINT('Ctrl Pts',(86.7442988734846,62.0374576512393,11.9741025623904));
#68446=CARTESIAN_POINT('Ctrl Pts',(86.7449635668555,62.0365914747207,11.9653588119135));
#68447=CARTESIAN_POINT('Ctrl Pts',(86.748336277368,62.0327425734185,11.9263433338939));
#68448=CARTESIAN_POINT('Ctrl Pts',(86.7520401459002,62.0298085641766,11.8961640765638));
#68449=CARTESIAN_POINT('Ctrl Pts',(86.7697652971787,62.0190523885109,11.7849322938948));
#68450=CARTESIAN_POINT('Ctrl Pts',(86.7905646280958,62.0114430278792,11.7051641760554));
#68451=CARTESIAN_POINT('Ctrl Pts',(86.8371075865748,61.9987448109254,11.5785032807828));
#68452=CARTESIAN_POINT('Ctrl Pts',(86.8583395542204,61.9937483060922,11.5302304232081));
#68453=CARTESIAN_POINT('Ctrl Pts',(86.8907031728052,61.9869250408361,11.4675399605217));
#68454=CARTESIAN_POINT('Ctrl Pts',(86.8992351703239,61.9851863929965,11.4518352926345));
#68455=CARTESIAN_POINT('Ctrl Pts',(86.9131052702072,61.9824464676901,11.4275414901062));
#68456=CARTESIAN_POINT('Ctrl Pts',(86.918219725893,61.9814531757426,11.4188266349074));
#68457=CARTESIAN_POINT('Ctrl Pts',(86.927986497966,61.979586842588,11.4026303019402));
#68458=CARTESIAN_POINT('Ctrl Pts',(86.9326137689311,61.978714757115,11.395134343847));
#68459=CARTESIAN_POINT('Ctrl Pts',(86.9431919772588,61.9767474523965,11.3783904030365));
#68460=CARTESIAN_POINT('Ctrl Pts',(86.9491857186099,61.9756507042034,11.3691705061139));
#68461=CARTESIAN_POINT('Ctrl Pts',(86.9649687275369,61.9728071711409,11.3455687236375));
#68462=CARTESIAN_POINT('Ctrl Pts',(86.9749347463562,61.9710539047597,11.3313086632255));
#68463=CARTESIAN_POINT('Ctrl Pts',(87.0257859179714,61.9623060378165,11.2616402153814));
#68464=CARTESIAN_POINT('Ctrl Pts',(87.0708292505141,61.9551563369666,11.2094273892294));
#68465=CARTESIAN_POINT('Ctrl Pts',(87.165921409992,61.9411288684737,11.1157792026558));
#68466=CARTESIAN_POINT('Ctrl Pts',(87.2153673299618,61.9342821610506,11.0740088530863));
#68467=CARTESIAN_POINT('Ctrl Pts',(87.2841847601351,61.9254309942041,11.0243431771584));
#68468=CARTESIAN_POINT('Ctrl Pts',(87.3008722713642,61.9233329925577,11.0128959855754));
#68469=CARTESIAN_POINT('Ctrl Pts',(87.3262006894194,61.9202263791202,10.9963973803056));
#68470=CARTESIAN_POINT('Ctrl Pts',(87.3346384516869,61.919203961748,10.9910418909633));
#68471=CARTESIAN_POINT('Ctrl Pts',(87.3484590123076,61.917550442911,10.9824970875497));
#68472=CARTESIAN_POINT('Ctrl Pts',(87.3538034691465,61.9169160777634,10.979247108508));
#68473=CARTESIAN_POINT('Ctrl Pts',(87.3640622425559,61.9157083111018,10.9731120796999));
#68474=CARTESIAN_POINT('Ctrl Pts',(87.3689723768306,61.9151345235978,10.9702203670039));
#68475=CARTESIAN_POINT('Ctrl Pts',(87.377218578839,61.9141782228872,10.9654384119774));
#68476=CARTESIAN_POINT('Ctrl Pts',(87.3805438429761,61.9137945853355,10.9635301662902));
#68477=CARTESIAN_POINT('Ctrl Pts',(87.389125172068,61.9128096153146,10.9586571843795));
#68478=CARTESIAN_POINT('Ctrl Pts',(87.3943938408958,61.9122097086623,10.9557147830471));
#68479=CARTESIAN_POINT('Ctrl Pts',(87.4097950771983,61.9104694611233,10.9472570807477));
#68480=CARTESIAN_POINT('Ctrl Pts',(87.419982513142,61.9093350726934,10.9418418958677));
#68481=CARTESIAN_POINT('Ctrl Pts',(87.5054489629294,61.8999438497759,10.8978948939304));
#68482=CARTESIAN_POINT('Ctrl Pts',(87.5843454823855,61.8920707804842,10.8668239435082));
#68483=CARTESIAN_POINT('Ctrl Pts',(87.7167709292999,61.8791784072329,10.8294164137846));
#68484=CARTESIAN_POINT('Ctrl Pts',(87.7686292085582,61.8742064696035,10.8182158418731));
#68485=CARTESIAN_POINT('Ctrl Pts',(87.8537009602796,61.8660015737358,10.8053459254994));
#68486=CARTESIAN_POINT('Ctrl Pts',(87.8865468478743,61.8628227863612,10.8016809450371));
#68487=CARTESIAN_POINT('Ctrl Pts',(87.9321571752695,61.8583679425721,10.7983861112518));
#68488=CARTESIAN_POINT('Ctrl Pts',(87.9448315697366,61.8571257400884,10.7976613730748));
#68489=CARTESIAN_POINT('Ctrl Pts',(87.9665515414348,61.8549882740241,10.7967458276447));
#68490=CARTESIAN_POINT('Ctrl Pts',(87.9755924420562,61.8540959772331,10.7964614563854));
#68491=CARTESIAN_POINT('Ctrl Pts',(87.9928799902242,61.8523843514883,10.7961024965952));
#68492=CARTESIAN_POINT('Ctrl Pts',(88.0011258797463,61.8515655764097,10.7960116152273));
#68493=CARTESIAN_POINT('Ctrl Pts',(88.0226900943668,61.8494177547867,10.7959839692702));
#68494=CARTESIAN_POINT('Ctrl Pts',(88.0360071363192,61.8480847650173,10.7961763961106));
#68495=CARTESIAN_POINT('Ctrl Pts',(88.0845728089279,61.8431973241815,10.7976423720828));
#68496=CARTESIAN_POINT('Ctrl Pts',(88.1197632634945,61.8396049491638,10.8001745891025));
#68497=CARTESIAN_POINT('Ctrl Pts',(88.2537733853057,61.8257098836156,10.8154464007892));
#68498=CARTESIAN_POINT('Ctrl Pts',(88.3510675993396,61.8151353341048,10.8383309125452));
#68499=CARTESIAN_POINT('Ctrl Pts',(88.4811154812576,61.8006340727124,10.8855783712691));
#68500=CARTESIAN_POINT('Ctrl Pts',(88.5169430754296,61.796602833171,10.9004845548079));
#68501=CARTESIAN_POINT('Ctrl Pts',(88.5602931877284,61.791718694583,10.9208972642893));
#68502=CARTESIAN_POINT('Ctrl Pts',(88.5685078079727,61.790792912838,10.92487408975));
#68503=CARTESIAN_POINT('Ctrl Pts',(88.5815619275314,61.7893220478666,10.9313684176577));
#68504=CARTESIAN_POINT('Ctrl Pts',(88.5864290588108,61.7887737201429,10.9338290132583));
#68505=CARTESIAN_POINT('Ctrl Pts',(88.5957804158729,61.7877205419562,10.9386325093589));
#68506=CARTESIAN_POINT('Ctrl Pts',(88.6002665871631,61.7872154686659,10.9409708958824));
#68507=CARTESIAN_POINT('Ctrl Pts',(88.6113607303852,61.7859665754378,10.9468382124495));
#68508=CARTESIAN_POINT('Ctrl Pts',(88.6179517588532,61.7852247212754,10.9503989575729));
#68509=CARTESIAN_POINT('Ctrl Pts',(88.6414219955573,61.782581931677,10.9633481353055));
#68510=CARTESIAN_POINT('Ctrl Pts',(88.658119405484,61.7806997288893,10.9730637500738));
#68511=CARTESIAN_POINT('Ctrl Pts',(88.7408430946724,61.7713283041086,11.0237586855808));
#68512=CARTESIAN_POINT('Ctrl Pts',(88.8032399604741,61.764101069542,11.0703608325041));
#68513=CARTESIAN_POINT('Ctrl Pts',(88.9138215166358,61.7501513437213,11.1699704676299));
#68514=CARTESIAN_POINT('Ctrl Pts',(88.9625533990916,61.7434626154976,11.2219033295985));
#68515=CARTESIAN_POINT('Ctrl Pts',(89.0177284563536,61.7348656799369,11.2915875858614));
#68516=CARTESIAN_POINT('Ctrl Pts',(89.0284815860225,61.7331340796478,11.3057711401159));
#68517=CARTESIAN_POINT('Ctrl Pts',(89.044857746256,61.7304027474901,11.3283415699957));
#68518=CARTESIAN_POINT('Ctrl Pts',(89.0506852230236,61.7294109170032,11.3365780224454));
#68519=CARTESIAN_POINT('Ctrl Pts',(89.0614166236631,61.7275458660714,11.3521354835805));
#68520=CARTESIAN_POINT('Ctrl Pts',(89.0663437276059,61.7266735889723,11.3594398555397));
#68521=CARTESIAN_POINT('Ctrl Pts',(89.077260630831,61.7247038974704,11.3759929878436));
#68522=CARTESIAN_POINT('Ctrl Pts',(89.0832067670937,61.7236049377698,11.3852694816493));
#68523=CARTESIAN_POINT('Ctrl Pts',(89.0982676274108,61.7207515670569,11.409452687925));
#68524=CARTESIAN_POINT('Ctrl Pts',(89.107196390347,61.7189905982982,11.4244716197857));
#68525=CARTESIAN_POINT('Ctrl Pts',(89.1500840920726,61.7101698658229,11.5001230674396));
#68526=CARTESIAN_POINT('Ctrl Pts',(89.1793291489598,61.7029520231919,11.5632750179026));
#68527=CARTESIAN_POINT('Ctrl Pts',(89.2253163104422,61.6889189597483,11.6885941927771));
#68528=CARTESIAN_POINT('Ctrl Pts',(89.2427964755464,61.6821374134764,11.750283183016));
#68529=CARTESIAN_POINT('Ctrl Pts',(89.2585445650095,61.6738926551828,11.8277595331751));
#68530=CARTESIAN_POINT('Ctrl Pts',(89.261277187835,61.6723317174103,11.84254314808));
#68531=CARTESIAN_POINT('Ctrl Pts',(89.2666717190363,61.6689422583581,11.8749357346361));
#68532=CARTESIAN_POINT('Ctrl Pts',(89.2692272121659,61.6671177753191,11.8925600536375));
#68533=CARTESIAN_POINT('Ctrl Pts',(89.2722775473009,61.6645946864081,11.9172424140383));
#68534=CARTESIAN_POINT('Ctrl Pts',(89.2730852600916,61.6638810956051,11.9242584199928));
#68535=CARTESIAN_POINT('Ctrl Pts',(89.2743686749144,61.6626640235626,11.9362889545822));
#68536=CARTESIAN_POINT('Ctrl Pts',(89.2748731381651,61.6621590164857,11.9413001224971));
#68537=CARTESIAN_POINT('Ctrl Pts',(89.2758796667905,61.6610917139736,11.9519330042115));
#68538=CARTESIAN_POINT('Ctrl Pts',(89.2763740906652,61.6605298408851,11.95755523881));
#68539=CARTESIAN_POINT('Ctrl Pts',(89.2776412269268,61.6589771708189,11.9731552449886));
#68540=CARTESIAN_POINT('Ctrl Pts',(89.2783335425097,61.6579906404385,11.9831395068201));
#68541=CARTESIAN_POINT('Ctrl Pts',(89.2824745699471,61.6509158291123,12.0551931314855));
#68542=CARTESIAN_POINT('Ctrl Pts',(89.2814805335318,61.6450405748864,12.1174457634074));
#68543=CARTESIAN_POINT('Ctrl Pts',(89.2716212554652,61.6346702014124,12.2274351010088));
#68544=CARTESIAN_POINT('Ctrl Pts',(89.2645800550495,61.6301700405048,12.2751990635647));
#68545=CARTESIAN_POINT('Ctrl Pts',(89.2470499440718,61.6220003956576,12.3602251447053));
#68546=CARTESIAN_POINT('Ctrl Pts',(89.2375445688236,61.6183499769934,12.3976260666504));
#68547=CARTESIAN_POINT('Ctrl Pts',(89.2185832334045,61.6120873521357,12.4601568841308));
#68548=CARTESIAN_POINT('Ctrl Pts',(89.2100057992326,61.6095008227215,12.4855256500594));
#68549=CARTESIAN_POINT('Ctrl Pts',(89.1965169643472,61.6057409156812,12.5216180642673));
#68550=CARTESIAN_POINT('Ctrl Pts',(89.1922474505703,61.6045886059016,12.5325755363549));
#68551=CARTESIAN_POINT('Ctrl Pts',(89.1844827770048,61.6025558291926,12.5517131609034));
#68552=CARTESIAN_POINT('Ctrl Pts',(89.1810526124823,61.6016775914689,12.5599189979002));
#68553=CARTESIAN_POINT('Ctrl Pts',(89.1737112431256,61.5998376918088,12.5769757262692));
#68554=CARTESIAN_POINT('Ctrl Pts',(89.1697845196326,61.5988755521522,12.5858192488831));
#68555=CARTESIAN_POINT('Ctrl Pts',(89.159171125065,61.5963307390361,12.6090040892284));
#68556=CARTESIAN_POINT('Ctrl Pts',(89.1523170710355,61.5947424334543,12.6232662366914));
#68557=CARTESIAN_POINT('Ctrl Pts',(89.113485644348,61.5860278813024,12.7003451288164));
#68558=CARTESIAN_POINT('Ctrl Pts',(89.0765944984042,61.5787330923175,12.7605303808079));
#68559=CARTESIAN_POINT('Ctrl Pts',(89.0002316581315,61.5651840946521,12.8645970484931));
#68560=CARTESIAN_POINT('Ctrl Pts',(88.962320720361,61.5589790397651,12.9094010456045));
#68561=CARTESIAN_POINT('Ctrl Pts',(88.9029671412863,61.5500548139998,12.9704321438013));
#68562=CARTESIAN_POINT('Ctrl Pts',(88.8838911541433,61.5472906586879,12.9888565190327));
#68563=CARTESIAN_POINT('Ctrl Pts',(88.8514308595378,61.5427697947982,13.0183001329849));
#68564=CARTESIAN_POINT('Ctrl Pts',(88.8383734114396,61.5409970255744,13.0296663922288));
#68565=CARTESIAN_POINT('Ctrl Pts',(88.8197245374676,61.5385325667359,13.0452412509537));
#68566=CARTESIAN_POINT('Ctrl Pts',(88.8143254366397,61.5378267658218,13.0496752798563));
#68567=CARTESIAN_POINT('Ctrl Pts',(88.8049803162172,61.5366186233422,13.0572217250383));
#68568=CARTESIAN_POINT('Ctrl Pts',(88.801052008383,61.5361148157008,13.0603556101724));
#68569=CARTESIAN_POINT('Ctrl Pts',(88.7926434254985,61.5350450903718,13.066982429417));
#68570=CARTESIAN_POINT('Ctrl Pts',(88.7881581847139,61.5344796296872,13.070468729832));
#68571=CARTESIAN_POINT('Ctrl Pts',(88.7757814636557,61.5329328266663,13.0799564083644));
#68572=CARTESIAN_POINT('Ctrl Pts',(88.7678425853573,61.5319556028821,13.0858958812332));
#68573=CARTESIAN_POINT('Ctrl Pts',(88.7091107381839,61.5248276813325,13.1287725789126));
#68574=CARTESIAN_POINT('Ctrl Pts',(88.6556994824167,61.5188945516076,13.1619972134143));
#68575=CARTESIAN_POINT('Ctrl Pts',(88.5555188933138,61.5082772582139,13.2144443250592));
#68576=CARTESIAN_POINT('Ctrl Pts',(88.509656082103,61.5035906647227,13.2350882015239));
#68577=CARTESIAN_POINT('Ctrl Pts',(88.428111734402,61.4953729266357,13.2661194542478));
#68578=CARTESIAN_POINT('Ctrl Pts',(88.3929767189535,61.4918675952603,13.277759983306));
#68579=CARTESIAN_POINT('Ctrl Pts',(88.3454882189434,61.487133560578,13.2912226637341));
#68580=CARTESIAN_POINT('Ctrl Pts',(88.3335418484475,61.4859430321718,13.2944216205689));
#68581=CARTESIAN_POINT('Ctrl Pts',(88.3039349389782,61.4829910387025,13.3018880154039));
#68582=CARTESIAN_POINT('Ctrl Pts',(88.2862265835771,61.4812240870242,13.3059517383963));
#68583=CARTESIAN_POINT('Ctrl Pts',(88.2584834508096,61.4784496629028,13.311694699743));
#68584=CARTESIAN_POINT('Ctrl Pts',(88.2485046867726,61.47745051783,13.3136357049626));
#68585=CARTESIAN_POINT('Ctrl Pts',(88.2298431210603,61.4755789713147,13.3170336474334));
#68586=CARTESIAN_POINT('Ctrl Pts',(88.2211663106254,61.4747075748821,13.3185205030736));
#68587=CARTESIAN_POINT('Ctrl Pts',(88.2017003306559,61.4727494437517,13.3216482289899));
#68588=CARTESIAN_POINT('Ctrl Pts',(88.1909042198743,61.4716612433343,13.3232404478233));
#68589=CARTESIAN_POINT('Ctrl Pts',(88.1631342445674,61.4688556244314,13.326970989135));
#68590=CARTESIAN_POINT('Ctrl Pts',(88.1461359403385,61.4671320144544,13.3289057242592));
#68591=CARTESIAN_POINT('Ctrl Pts',(88.0401074397547,61.4563357863369,13.338808854493));
#68592=CARTESIAN_POINT('Ctrl Pts',(87.9505025925264,61.4469875989152,13.3377005012535));
#68593=CARTESIAN_POINT('Ctrl Pts',(87.8126183112931,61.4323493303676,13.321386512206));
#68594=CARTESIAN_POINT('Ctrl Pts',(87.7638367075291,61.4271262506289,13.312700261283));
#68595=CARTESIAN_POINT('Ctrl Pts',(87.6986031353953,61.4201512268202,13.2971038252658));
#68596=CARTESIAN_POINT('Ctrl Pts',(87.6816076574998,61.4183351472497,13.2926658891446));
#68597=CARTESIAN_POINT('Ctrl Pts',(87.6523615453121,61.4152172273181,13.2843772615347));
#68598=CARTESIAN_POINT('Ctrl Pts',(87.6400674484234,61.4139088047979,13.2806908168292));
#68599=CARTESIAN_POINT('Ctrl Pts',(87.6219037560744,61.4119809465445,13.2749428262475));
#68600=CARTESIAN_POINT('Ctrl Pts',(87.6159906173178,61.4113541719552,13.2730237105095));
#68601=CARTESIAN_POINT('Ctrl Pts',(87.6053849337812,61.4102317765184,13.2694953354569));
#68602=CARTESIAN_POINT('Ctrl Pts',(87.6006875091621,61.4097353047805,13.2679019375483));
#68603=CARTESIAN_POINT('Ctrl Pts',(87.5901133215982,61.4086191465328,13.2642458801508));
#68604=CARTESIAN_POINT('Ctrl Pts',(87.5842422398027,61.4080003866912,13.2621674654846));
#68605=CARTESIAN_POINT('Ctrl Pts',(87.5662647073072,61.4061079374555,13.2556540439802));
#68606=CARTESIAN_POINT('Ctrl Pts',(87.5542096783003,61.4048420457589,13.2510775814095));
#68607=CARTESIAN_POINT('Ctrl Pts',(87.4860058371124,61.397685632907,13.2239897836112));
#68608=CARTESIAN_POINT('Ctrl Pts',(87.4314427977759,61.3919806488829,13.1976692407666));
#68609=CARTESIAN_POINT('Ctrl Pts',(87.3149673821541,61.3793791376846,13.1308385449483));
#68610=CARTESIAN_POINT('Ctrl Pts',(87.2543042240963,61.3725153337452,13.0886206264755));
#68611=CARTESIAN_POINT('Ctrl Pts',(87.191938763816,61.3647774823412,13.0366152717074));
#68612=CARTESIAN_POINT('Ctrl Pts',(87.1862692440195,61.3640674112978,13.0318025026143));
#68613=CARTESIAN_POINT('Ctrl Pts',(87.1806428320421,61.3633558149692,13.0269406712284));
#68614=CARTESIAN_POINT('Origin',(88.011,66.41344859951,12.066));
#68615=CARTESIAN_POINT('',(87.1806428354305,60.4003450897931,13.0269406741564));
#68616=CARTESIAN_POINT('',(87.180642808438,60.5693987930815,13.0269406508319));
#68617=CARTESIAN_POINT('',(87.1806428354228,66.41344859951,13.0269406741497));
#68618=CARTESIAN_POINT('Ctrl Pts',(87.1806428354305,60.4003450897931,13.0269406741563));
#68619=CARTESIAN_POINT('Ctrl Pts',(87.1818235457003,60.4005030384075,13.0279609361332));
#68620=CARTESIAN_POINT('Ctrl Pts',(87.183006150907,60.4006608448018,13.0289790345607));
#68621=CARTESIAN_POINT('Ctrl Pts',(87.1883032417142,60.4013659091017,13.0335222992003));
#68622=CARTESIAN_POINT('Ctrl Pts',(87.1924385094708,60.4019115463032,13.0370234012454));
#68623=CARTESIAN_POINT('Ctrl Pts',(87.2001912229078,60.4029254359064,13.0435024694305));
#68624=CARTESIAN_POINT('Ctrl Pts',(87.2038028005578,60.4033941165757,13.046486937284));
#68625=CARTESIAN_POINT('Ctrl Pts',(87.2123614349539,60.4044963384234,13.053480116595));
#68626=CARTESIAN_POINT('Ctrl Pts',(87.2173222500813,60.4051286646051,13.0574717211992));
#68627=CARTESIAN_POINT('Ctrl Pts',(87.2329986405361,60.4071071941662,13.0698922970969));
#68628=CARTESIAN_POINT('Ctrl Pts',(87.2438206326235,60.4084445437355,13.0781866096631));
#68629=CARTESIAN_POINT('Ctrl Pts',(87.3215569159369,60.4178691040628,13.1358028049835));
#68630=CARTESIAN_POINT('Ctrl Pts',(87.3930503351943,60.4256038617588,13.1786334918077));
#68631=CARTESIAN_POINT('Ctrl Pts',(87.515181244556,60.4382618428318,13.2363677913222));
#68632=CARTESIAN_POINT('Ctrl Pts',(87.5634452938574,60.4431359090961,13.2556600366186));
#68633=CARTESIAN_POINT('Ctrl Pts',(87.6338056398892,60.4502041844216,13.2788957251422));
#68634=CARTESIAN_POINT('Ctrl Pts',(87.6550369818825,60.4523320140989,13.285295629218));
#68635=CARTESIAN_POINT('Ctrl Pts',(87.6936033195649,60.4561987754467,13.2958278334117));
#68636=CARTESIAN_POINT('Ctrl Pts',(87.7108787134513,60.4579313985905,13.3001573202425));
#68637=CARTESIAN_POINT('Ctrl Pts',(87.7380781588305,60.4606641076622,13.3063691139301));
#68638=CARTESIAN_POINT('Ctrl Pts',(87.7479439690297,60.461656280952,13.3084988451494));
#68639=CARTESIAN_POINT('Ctrl Pts',(87.7664694706385,60.4635218446625,13.3122674198115));
#68640=CARTESIAN_POINT('Ctrl Pts',(87.7751229431287,60.4643942901964,13.3139341591509));
#68641=CARTESIAN_POINT('Ctrl Pts',(87.7946340537761,60.46636419222,13.3174820001018));
#68642=CARTESIAN_POINT('Ctrl Pts',(87.8055000673036,60.4674631932169,13.3193120829443));
#68643=CARTESIAN_POINT('Ctrl Pts',(87.8336509584641,60.4703163338593,13.3236774190162));
#68644=CARTESIAN_POINT('Ctrl Pts',(87.850966083578,60.4720770275225,13.325997714557));
#68645=CARTESIAN_POINT('Ctrl Pts',(87.9374121288136,60.4809011960646,13.3357713264499));
#68646=CARTESIAN_POINT('Ctrl Pts',(88.0070116415135,60.4881229405543,13.3378941071811));
#68647=CARTESIAN_POINT('Ctrl Pts',(88.14033476812,60.502157152959,13.3310171185709));
#68648=CARTESIAN_POINT('Ctrl Pts',(88.2039085896951,60.5089358068787,13.3228939852102));
#68649=CARTESIAN_POINT('Ctrl Pts',(88.2813220326698,60.517177406491,13.3069882621684));
#68650=CARTESIAN_POINT('Ctrl Pts',(88.2959893885601,60.5187380173635,13.3037022929366));
#68651=CARTESIAN_POINT('Ctrl Pts',(88.3278965393121,60.5221269677771,13.2959567227708));
#68652=CARTESIAN_POINT('Ctrl Pts',(88.3451086933597,60.5239512677949,13.2913931819824));
#68653=CARTESIAN_POINT('Ctrl Pts',(88.3690077503675,60.5264742388476,13.2845156256566));
#68654=CARTESIAN_POINT('Ctrl Pts',(88.375778714417,60.5271878908095,13.2825058065376));
#68655=CARTESIAN_POINT('Ctrl Pts',(88.3873496830548,60.5284051169061,13.2789659061668));
#68656=CARTESIAN_POINT('Ctrl Pts',(88.3921578798775,60.5289102168012,13.2774635978164));
#68657=CARTESIAN_POINT('Ctrl Pts',(88.4023357079058,60.529977786217,13.2742169650245));
#68658=CARTESIAN_POINT('Ctrl Pts',(88.4077028162123,60.5305398327136,13.2724653957062));
#68659=CARTESIAN_POINT('Ctrl Pts',(88.4225554360673,60.5320931508309,13.2675083712489));
#68660=CARTESIAN_POINT('Ctrl Pts',(88.4320153458227,60.5330801511957,13.2642263328636));
#68661=CARTESIAN_POINT('Ctrl Pts',(88.5000220765551,60.5401659294441,13.2397270471169));
#68662=CARTESIAN_POINT('Ctrl Pts',(88.5569886562945,60.5460509438944,13.2143367338943));
#68663=CARTESIAN_POINT('Ctrl Pts',(88.6545537301216,60.5564504935943,13.1619405892929));
#68664=CARTESIAN_POINT('Ctrl Pts',(88.6958888513917,60.5609697956643,13.1365953465336));
#68665=CARTESIAN_POINT('Ctrl Pts',(88.7671948193609,60.5691416584645,13.087049738998));
#68666=CARTESIAN_POINT('Ctrl Pts',(88.7977030773002,60.5727744517393,13.0637329175712));
#68667=CARTESIAN_POINT('Ctrl Pts',(88.8475515616372,60.579010451814,13.0219254676001));
#68668=CARTESIAN_POINT('Ctrl Pts',(88.8674492276917,60.5815882885321,13.0041399150839));
#68669=CARTESIAN_POINT('Ctrl Pts',(88.8952771946967,60.5853380351467,12.9776423735909));
#68670=CARTESIAN_POINT('Ctrl Pts',(88.9036707639428,60.5864890432026,12.9694250710635));
#68671=CARTESIAN_POINT('Ctrl Pts',(88.91821700976,60.5885204883688,12.9547836595667));
#68672=CARTESIAN_POINT('Ctrl Pts',(88.9244185530755,60.5893987076884,12.9484089942142));
#68673=CARTESIAN_POINT('Ctrl Pts',(88.9372328688173,60.5912395269298,12.9349571222238));
#68674=CARTESIAN_POINT('Ctrl Pts',(88.9438326139202,60.5922026113499,12.9278683824296));
#68675=CARTESIAN_POINT('Ctrl Pts',(88.9610248223903,60.5947521932668,12.9089735519185));
#68676=CARTESIAN_POINT('Ctrl Pts',(88.9714778832212,60.5963443595617,12.8970437712062));
#68677=CARTESIAN_POINT('Ctrl Pts',(89.0289240580398,60.6053401616578,12.8289503018001));
#68678=CARTESIAN_POINT('Ctrl Pts',(89.0712031951646,60.6129267965022,12.7690128165869));
#68679=CARTESIAN_POINT('Ctrl Pts',(89.141358493305,60.6275566034683,12.6487128009007));
#68680=CARTESIAN_POINT('Ctrl Pts',(89.1701360753813,60.6345569155692,12.5891332674651));
#68681=CARTESIAN_POINT('Ctrl Pts',(89.1997068907329,60.6430441963511,12.5133363729505));
#68682=CARTESIAN_POINT('Ctrl Pts',(89.2050079721939,60.6446328049968,12.4989883560411));
#68683=CARTESIAN_POINT('Ctrl Pts',(89.2159880026012,60.6480724241271,12.4675329091262));
#68684=CARTESIAN_POINT('Ctrl Pts',(89.2215648760738,60.6499194150829,12.4503924570919));
#68685=CARTESIAN_POINT('Ctrl Pts',(89.2288265944031,60.6524680472548,12.4263452907856));
#68686=CARTESIAN_POINT('Ctrl Pts',(89.2308208555399,60.6531850601008,12.41953561584));
#68687=CARTESIAN_POINT('Ctrl Pts',(89.2341345518813,60.6544061558909,12.4078585851044));
#68688=CARTESIAN_POINT('Ctrl Pts',(89.2354822311421,60.65491179038,12.4029995469194));
#68689=CARTESIAN_POINT('Ctrl Pts',(89.2382734172852,60.6559783944958,12.3926981142844));
#68690=CARTESIAN_POINT('Ctrl Pts',(89.2397097240939,60.6565389556276,12.3872539760174));
#68691=CARTESIAN_POINT('Ctrl Pts',(89.2435816974858,60.6580837784724,12.372171808707));
#68692=CARTESIAN_POINT('Ctrl Pts',(89.2459405754572,60.6590638446109,12.3625141060716));
#68693=CARTESIAN_POINT('Ctrl Pts',(89.2612211512837,60.665697018692,12.2966040914199));
#68694=CARTESIAN_POINT('Ctrl Pts',(89.270410985598,60.6711671553571,12.2395445707144));
#68695=CARTESIAN_POINT('Ctrl Pts',(89.2824480332011,60.6835540456412,12.1083646942831));
#68696=CARTESIAN_POINT('Ctrl Pts',(89.282756795416,60.6904252659034,12.0342351866708));
#68697=CARTESIAN_POINT('Ctrl Pts',(89.274989777182,60.6993003612147,11.9410578186938));
#68698=CARTESIAN_POINT('Ctrl Pts',(89.2729211592636,60.7011610843257,11.9216545174111));
#68699=CARTESIAN_POINT('Ctrl Pts',(89.2688559280903,60.7041878769031,11.890377711165));
#68700=CARTESIAN_POINT('Ctrl Pts',(89.2671359706872,60.7053465992457,11.8784709982653));
#68701=CARTESIAN_POINT('Ctrl Pts',(89.2624525692833,60.7082315952085,11.8490132446152));
#68702=CARTESIAN_POINT('Ctrl Pts',(89.2592889111503,60.7099632312611,11.8314973246124));
#68703=CARTESIAN_POINT('Ctrl Pts',(89.2537565683444,60.7126947366908,11.804164290217));
#68704=CARTESIAN_POINT('Ctrl Pts',(89.2516369724662,60.7136867051908,11.7942984816242));
#68705=CARTESIAN_POINT('Ctrl Pts',(89.2474464429995,60.7155520897741,11.7758657909649));
#68706=CARTESIAN_POINT('Ctrl Pts',(89.2454034378665,60.7164245627095,11.7672931063713));
#68707=CARTESIAN_POINT('Ctrl Pts',(89.2406048145838,60.7183948018869,11.7480479803434));
#68708=CARTESIAN_POINT('Ctrl Pts',(89.237799180225,60.7194941149436,11.7373889250765));
#68709=CARTESIAN_POINT('Ctrl Pts',(89.230186224627,60.7223486445919,11.7099234726828));
#68710=CARTESIAN_POINT('Ctrl Pts',(89.2251702066942,60.7241104259952,11.6931780922213));
#68711=CARTESIAN_POINT('Ctrl Pts',(89.1985235430636,60.7329242255433,11.6104713120563));
#68712=CARTESIAN_POINT('Ctrl Pts',(89.1718600995691,60.7401339181801,11.5462707161571));
#68713=CARTESIAN_POINT('Ctrl Pts',(89.1107606974387,60.7541635742319,11.4276179459689));
#68714=CARTESIAN_POINT('Ctrl Pts',(89.0771587470441,60.7609501413926,11.3729551363371));
#68715=CARTESIAN_POINT('Ctrl Pts',(89.0307531605401,60.7692005270281,11.3088806905279));
#68716=CARTESIAN_POINT('Ctrl Pts',(89.0217159320494,60.7707621534588,11.296857938134));
#68717=CARTESIAN_POINT('Ctrl Pts',(89.0015135749182,60.774152945064,11.2709527705344));
#68718=CARTESIAN_POINT('Ctrl Pts',(88.9902651036156,60.7759780713757,11.2571383251341));
#68719=CARTESIAN_POINT('Ctrl Pts',(88.9741543530414,60.7785019775746,11.2381814278303));
#68720=CARTESIAN_POINT('Ctrl Pts',(88.9695349496019,60.7792157525372,11.2328369576447));
#68721=CARTESIAN_POINT('Ctrl Pts',(88.9615452521861,60.7804331200762,11.2237476038366));
#68722=CARTESIAN_POINT('Ctrl Pts',(88.9581969108303,60.7809382393567,11.2199838109235));
#68723=CARTESIAN_POINT('Ctrl Pts',(88.9510490725428,60.7820057726023,11.212044728525));
#68724=CARTESIAN_POINT('Ctrl Pts',(88.947244018508,60.7825677640794,11.2078747137815));
#68725=CARTESIAN_POINT('Ctrl Pts',(88.9366151718135,60.7841207672902,11.1963812652628));
#68726=CARTESIAN_POINT('Ctrl Pts',(88.9297321621756,60.7851075105839,11.1891126484477));
#68727=CARTESIAN_POINT('Ctrl Pts',(88.8794707434954,60.7921851921374,11.1372770370207));
#68728=CARTESIAN_POINT('Ctrl Pts',(88.8329477885672,60.798062921411,11.0958594470615));
#68729=CARTESIAN_POINT('Ctrl Pts',(88.7452332758582,60.8084411299462,11.0286311007822));
#68730=CARTESIAN_POINT('Ctrl Pts',(88.7052547864094,60.8129465739439,11.0014611384871));
#68731=CARTESIAN_POINT('Ctrl Pts',(88.6307849874536,60.821116789458,10.9568334812509));
#68732=CARTESIAN_POINT('Ctrl Pts',(88.5968628543753,60.8247623030063,10.9385479870025));
#68733=CARTESIAN_POINT('Ctrl Pts',(88.5380648875935,60.8310175850487,10.9102239866045));
#68734=CARTESIAN_POINT('Ctrl Pts',(88.5136062182713,60.8336017636904,10.8993799497752));
#68735=CARTESIAN_POINT('Ctrl Pts',(88.4779320745104,60.8373590267209,10.8848934552966));
#68736=CARTESIAN_POINT('Ctrl Pts',(88.4669783100613,60.8385110891188,10.8806215835111));
#68737=CARTESIAN_POINT('Ctrl Pts',(88.4476359648191,60.8405437364103,10.8733859980256));
#68738=CARTESIAN_POINT('Ctrl Pts',(88.4392724302413,60.8414220950631,10.8703571441139));
#68739=CARTESIAN_POINT('Ctrl Pts',(88.42174188407,60.8432625561468,10.864215985656));
#68740=CARTESIAN_POINT('Ctrl Pts',(88.412569770061,60.8442251386009,10.8611201641078));
#68741=CARTESIAN_POINT('Ctrl Pts',(88.3883005701939,60.8467718616328,10.8532365800518));
#68742=CARTESIAN_POINT('Ctrl Pts',(88.373148354498,60.8483616478028,10.8486260459293));
#68743=CARTESIAN_POINT('Ctrl Pts',(88.2851879697798,60.8575943736303,10.8236487498949));
#68744=CARTESIAN_POINT('Ctrl Pts',(88.2107801797756,60.865433453224,10.8095373426119));
#68745=CARTESIAN_POINT('Ctrl Pts',(88.0716513455794,60.8801291206798,10.7958238113302));
#68746=CARTESIAN_POINT('Ctrl Pts',(88.0073392444037,60.8869331618185,10.7943816821399));
#68747=CARTESIAN_POINT('Ctrl Pts',(87.9281544325711,60.8952029446871,10.7986155252594));
#68748=CARTESIAN_POINT('Ctrl Pts',(87.9131308565589,60.8967668094308,10.7996870547881));
#68749=CARTESIAN_POINT('Ctrl Pts',(87.880370959071,60.9001616581843,10.8026101488551));
#68750=CARTESIAN_POINT('Ctrl Pts',(87.8626465375777,60.9019886048038,10.8045685806001));
#68751=CARTESIAN_POINT('Ctrl Pts',(87.8379619933267,60.9045145709251,10.8078236285326));
#68752=CARTESIAN_POINT('Ctrl Pts',(87.8309638087539,60.9052286166913,10.8088059370702));
#68753=CARTESIAN_POINT('Ctrl Pts',(87.8189910262652,60.9064462956846,10.8105885402172));
#68754=CARTESIAN_POINT('Ctrl Pts',(87.8140124437935,60.9069514576935,10.8113600967529));
#68755=CARTESIAN_POINT('Ctrl Pts',(87.8034664913107,60.9080189115332,10.8130587830223));
#68756=CARTESIAN_POINT('Ctrl Pts',(87.797900534944,60.9085807820554,10.8139934213466));
#68757=CARTESIAN_POINT('Ctrl Pts',(87.7824865048628,60.9101330930373,10.8166875266389));
#68758=CARTESIAN_POINT('Ctrl Pts',(87.7726523430076,60.9111192712444,10.8185263566091));
#68759=CARTESIAN_POINT('Ctrl Pts',(87.7020269615263,60.9181785548535,10.8325978982789));
#68760=CARTESIAN_POINT('Ctrl Pts',(87.6421700351697,60.9240397109677,10.8491546507382));
#68761=CARTESIAN_POINT('Ctrl Pts',(87.5386139137096,60.9343668730824,10.8861487892692));
#68762=CARTESIAN_POINT('Ctrl Pts',(87.4944249805767,60.938838327223,10.904816245598));
#68763=CARTESIAN_POINT('Ctrl Pts',(87.4165215302357,60.9470037629158,10.9430553396457));
#68764=CARTESIAN_POINT('Ctrl Pts',(87.3824528756208,60.9506796972496,10.9617638866863));
#68765=CARTESIAN_POINT('Ctrl Pts',(87.3263289178861,60.9569810451816,10.9960235266602));
#68766=CARTESIAN_POINT('Ctrl Pts',(87.3038136527362,60.9595803392451,11.0107695162515));
#68767=CARTESIAN_POINT('Ctrl Pts',(87.2721381929844,60.9633555102512,11.0329839906344));
#68768=CARTESIAN_POINT('Ctrl Pts',(87.2625859596756,60.9645100774377,11.0398834145438));
#68769=CARTESIAN_POINT('Ctrl Pts',(87.2459908340444,60.9665455835743,11.0522247958457));
#68770=CARTESIAN_POINT('Ctrl Pts',(87.2389064224069,60.9674242761944,11.0576098543521));
#68771=CARTESIAN_POINT('Ctrl Pts',(87.224243725225,60.969263901424,11.0690004748285));
#68772=CARTESIAN_POINT('Ctrl Pts',(87.21667630813,60.9702253034973,11.0750189969647));
#68773=CARTESIAN_POINT('Ctrl Pts',(87.1969391023736,60.9727653039277,11.0910877200085));
#68774=CARTESIAN_POINT('Ctrl Pts',(87.1848871442495,60.9743494934518,11.1012790089521));
#68775=CARTESIAN_POINT('Ctrl Pts',(87.1208285702406,60.982956709329,11.15752836861));
#68776=CARTESIAN_POINT('Ctrl Pts',(87.0724891052819,60.9901431269842,11.2075600840623));
#68777=CARTESIAN_POINT('Ctrl Pts',(86.984660276668,61.0046878356518,11.3147933334829));
#68778=CARTESIAN_POINT('Ctrl Pts',(86.9452760834755,61.0120213220525,11.3717973221253));
#68779=CARTESIAN_POINT('Ctrl Pts',(86.9029004350045,61.0208762787525,11.4453059659719));
#68780=CARTESIAN_POINT('Ctrl Pts',(86.8953231713088,61.0225052556663,11.4590313036091));
#68781=CARTESIAN_POINT('Ctrl Pts',(86.8838468872093,61.0250431114313,11.4807607286703));
#68782=CARTESIAN_POINT('Ctrl Pts',(86.8797747993739,61.0259586279153,11.4886710619168));
#68783=CARTESIAN_POINT('Ctrl Pts',(86.8703168278749,61.0281204190384,11.5075282296498));
#68784=CARTESIAN_POINT('Ctrl Pts',(86.8650046735154,61.029363248991,11.5185115811269));
#68785=CARTESIAN_POINT('Ctrl Pts',(86.8572770465514,61.0312137873292,11.5350946509773));
#68786=CARTESIAN_POINT('Ctrl Pts',(86.8547425174462,61.031828035699,11.5406374750529));
#68787=CARTESIAN_POINT('Ctrl Pts',(86.8504196176335,61.0328883104789,11.5502741722144));
#68788=CARTESIAN_POINT('Ctrl Pts',(86.8486128588339,61.0333354059779,11.5543594134715));
#68789=CARTESIAN_POINT('Ctrl Pts',(86.844390175985,61.0343898403386,11.5640451056216));
#68790=CARTESIAN_POINT('Ctrl Pts',(86.8419929803356,61.0349960489823,11.5696535573522));
#68791=CARTESIAN_POINT('Ctrl Pts',(86.8350613103306,61.0367723789586,11.5861996434745));
#68792=CARTESIAN_POINT('Ctrl Pts',(86.8306390634038,61.0379361722533,11.5971841723812));
#68793=CARTESIAN_POINT('Ctrl Pts',(86.7969364963393,61.0470682195402,11.6844004936831));
#68794=CARTESIAN_POINT('Ctrl Pts',(86.7749112460985,61.0546819141872,11.7632486704293));
#68795=CARTESIAN_POINT('Ctrl Pts',(86.747586714649,61.0693042938117,11.916929712529));
#68796=CARTESIAN_POINT('Ctrl Pts',(86.7410263188956,61.0762791249421,11.9911708868403));
#68797=CARTESIAN_POINT('Ctrl Pts',(86.7409937160777,61.0851952413026,12.0835881886303));
#68798=CARTESIAN_POINT('Ctrl Pts',(86.7413715720823,61.0869454454075,12.1016213816465));
#68799=CARTESIAN_POINT('Ctrl Pts',(86.7426055350587,61.0897997207293,12.1308114111767));
#68800=CARTESIAN_POINT('Ctrl Pts',(86.7432253267581,61.0908964873843,12.1419762859805));
#68801=CARTESIAN_POINT('Ctrl Pts',(86.7445980041939,61.0928672786699,12.1619369299044));
#68802=CARTESIAN_POINT('Ctrl Pts',(86.7452953406335,61.0937395163781,12.1707359290083));
#68803=CARTESIAN_POINT('Ctrl Pts',(86.7469769078808,61.0956047155684,12.1894719742893));
#68804=CARTESIAN_POINT('Ctrl Pts',(86.7479867296546,61.0965984206984,12.1994060349801));
#68805=CARTESIAN_POINT('Ctrl Pts',(86.751064811346,61.0993230420021,12.2265062679242));
#68806=CARTESIAN_POINT('Ctrl Pts',(86.7533665709165,61.1010611189094,12.2436429677218));
#68807=CARTESIAN_POINT('Ctrl Pts',(86.7690739057215,61.1114251476751,12.3448744677802));
#68808=CARTESIAN_POINT('Ctrl Pts',(86.7905573747488,61.1203012032526,12.427475203825));
#68809=CARTESIAN_POINT('Ctrl Pts',(86.8460860157505,61.1371390301722,12.5773262869857));
#68810=CARTESIAN_POINT('Ctrl Pts',(86.8781710899104,61.1450429541316,12.6449476925472));
#68811=CARTESIAN_POINT('Ctrl Pts',(86.9223877843024,61.1539922390763,12.7202029611383));
#68812=CARTESIAN_POINT('Ctrl Pts',(86.9289179388271,61.1552736962705,12.7309485142304));
#68813=CARTESIAN_POINT('Ctrl Pts',(86.9388877847896,61.1571698641732,12.7468182080522));
#68814=CARTESIAN_POINT('Ctrl Pts',(86.9422066463362,61.1577915801697,12.7520166232814));
#68815=CARTESIAN_POINT('Ctrl Pts',(86.9482638459595,61.1589090498527,12.7613534979219));
#68816=CARTESIAN_POINT('Ctrl Pts',(86.9509886757856,61.159405613115,12.7655002614634));
#68817=CARTESIAN_POINT('Ctrl Pts',(86.9572181881596,61.1605271525424,12.7748606009751));
#68818=CARTESIAN_POINT('Ctrl Pts',(86.9607373373136,61.161151159148,12.7800642857004));
#68819=CARTESIAN_POINT('Ctrl Pts',(86.9717556774926,61.1630763550506,12.7960991574369));
#68820=CARTESIAN_POINT('Ctrl Pts',(86.9793852818383,61.1643693537997,12.8068405123835));
#68821=CARTESIAN_POINT('Ctrl Pts',(86.997942895831,61.1674263987363,12.8321240730532));
#68822=CARTESIAN_POINT('Ctrl Pts',(87.0090191575784,61.1691821336079,12.8465544737062));
#68823=CARTESIAN_POINT('Ctrl Pts',(87.0533894015635,61.1759776120283,12.9018592103304));
#68824=CARTESIAN_POINT('Ctrl Pts',(87.088907793503,61.1809202758021,12.9408861691967));
#68825=CARTESIAN_POINT('Ctrl Pts',(87.1442488648199,61.188144009566,12.9945669604313));
#68826=CARTESIAN_POINT('Ctrl Pts',(87.1622201789556,61.1904240998232,13.0110215023542));
#68827=CARTESIAN_POINT('Ctrl Pts',(87.1806429942554,61.1927093932679,13.0269408113983));
#68828=CARTESIAN_POINT('Ctrl Pts',(87.1806428320421,61.3633558149692,13.0269406712284));
#68829=CARTESIAN_POINT('Ctrl Pts',(87.1604885363056,61.3608068151966,13.0095251694904));
#68830=CARTESIAN_POINT('Ctrl Pts',(87.1408873812754,61.3582380582144,12.9914801488475));
#68831=CARTESIAN_POINT('Ctrl Pts',(87.1127044862172,61.3543939148636,12.9638473539881));
#68832=CARTESIAN_POINT('Ctrl Pts',(87.103677906826,61.3531383888453,12.9547245305709));
#68833=CARTESIAN_POINT('Ctrl Pts',(87.0885102340277,61.3509851290083,12.9389231959377));
#68834=CARTESIAN_POINT('Ctrl Pts',(87.0822994499866,61.350090474729,12.9323126179523));
#68835=CARTESIAN_POINT('Ctrl Pts',(87.0705959386853,61.3483791469246,12.9195852492142));
#68836=CARTESIAN_POINT('Ctrl Pts',(87.0650907243153,61.3475630596248,12.9134805073078));
#68837=CARTESIAN_POINT('Ctrl Pts',(87.0523180097064,61.3456429490747,12.8990373235115));
#68838=CARTESIAN_POINT('Ctrl Pts',(87.0450995568168,61.3445369685392,12.8906566890633));
#68839=CARTESIAN_POINT('Ctrl Pts',(87.0200884312836,61.3406292549831,12.8608398151946));
#68840=CARTESIAN_POINT('Ctrl Pts',(87.0028940895592,61.337804144048,12.8389154116862));
#68841=CARTESIAN_POINT('Ctrl Pts',(86.9321560112146,61.3255473174032,12.7423385423571));
#68842=CARTESIAN_POINT('Ctrl Pts',(86.8860859670684,61.3158598779851,12.6625737176514));
#68843=CARTESIAN_POINT('Ctrl Pts',(86.8285799303909,61.3008521932784,12.5322074239055));
#68844=CARTESIAN_POINT('Ctrl Pts',(86.8109224720278,61.2955400149956,12.4846668162996));
#68845=CARTESIAN_POINT('Ctrl Pts',(86.79251601967,61.2890665721679,12.4242629102094));
#68846=CARTESIAN_POINT('Ctrl Pts',(86.7890565392687,61.2877956355853,12.4122798638718));
#68847=CARTESIAN_POINT('Ctrl Pts',(86.7841561763778,61.2859119585795,12.3943169431151));
#68848=CARTESIAN_POINT('Ctrl Pts',(86.782581441654,61.2852923404082,12.3883749897075));
#68849=CARTESIAN_POINT('Ctrl Pts',(86.7799366135299,61.2842265496947,12.3780943811035));
#68850=CARTESIAN_POINT('Ctrl Pts',(86.7788462158416,61.2837792670188,12.3737613017979));
#68851=CARTESIAN_POINT('Ctrl Pts',(86.7763341001985,61.2827298252713,12.3635511269907));
#68852=CARTESIAN_POINT('Ctrl Pts',(86.7749314472001,61.2821287541778,12.3576694972454));
#68853=CARTESIAN_POINT('Ctrl Pts',(86.7709622309102,61.2803818012319,12.34048263653));
#68854=CARTESIAN_POINT('Ctrl Pts',(86.768508266707,61.2792419410337,12.3291515038521));
#68855=CARTESIAN_POINT('Ctrl Pts',(86.7495248860956,61.2698861062995,12.2353012656534));
#68856=CARTESIAN_POINT('Ctrl Pts',(86.7410768704604,61.2620495744167,12.1513431498856));
#68857=CARTESIAN_POINT('Ctrl Pts',(86.740934028576,61.2472922714272,11.993827225442));
#68858=CARTESIAN_POINT('Ctrl Pts',(86.7472175375862,61.240411302849,11.9206458297219));
#68859=CARTESIAN_POINT('Ctrl Pts',(86.7627722994671,61.231645973084,11.8311950488852));
#68860=CARTESIAN_POINT('Ctrl Pts',(86.7661232965139,61.2299482547671,11.8140323811844));
#68861=CARTESIAN_POINT('Ctrl Pts',(86.7721625378048,61.2271623559286,11.7861728360493));
#68862=CARTESIAN_POINT('Ctrl Pts',(86.7746377912754,61.2260809086662,11.7754316440335));
#68863=CARTESIAN_POINT('Ctrl Pts',(86.7793426699757,61.224126891157,11.7561647888799));
#68864=CARTESIAN_POINT('Ctrl Pts',(86.7815218522959,61.2232559879457,11.7476274021184));
#68865=CARTESIAN_POINT('Ctrl Pts',(86.7863858478783,61.2213818584544,11.7293667869308));
#68866=CARTESIAN_POINT('Ctrl Pts',(86.789098002472,61.2203778041361,11.7196515698128));
#68867=CARTESIAN_POINT('Ctrl Pts',(86.7969111550221,61.2175928385922,11.6928987224275));
#68868=CARTESIAN_POINT('Ctrl Pts',(86.8022545213241,61.215804216653,11.6759351691524));
#68869=CARTESIAN_POINT('Ctrl Pts',(86.8150438105204,61.2117633614103,11.6381230059911));
#68870=CARTESIAN_POINT('Ctrl Pts',(86.8226820462052,61.2095054611166,11.6173462140696));
#68871=CARTESIAN_POINT('Ctrl Pts',(86.8588691665552,61.1994417745509,11.526331293098));
#68872=CARTESIAN_POINT('Ctrl Pts',(86.8931274079359,61.191470383299,11.4585422020029));
#68873=CARTESIAN_POINT('Ctrl Pts',(86.965202114098,61.1771042629775,11.3429072263564));
#68874=CARTESIAN_POINT('Ctrl Pts',(87.0008155311453,61.1707375673016,11.2939341729726));
#68875=CARTESIAN_POINT('Ctrl Pts',(87.0480951903352,61.1632107300248,11.2378209507132));
#68876=CARTESIAN_POINT('Ctrl Pts',(87.0565524969098,61.1618962034919,11.2280881786942));
#68877=CARTESIAN_POINT('Ctrl Pts',(87.0693130828877,61.1599611637829,11.213847118109));
#68878=CARTESIAN_POINT('Ctrl Pts',(87.0735032483444,61.1593332354386,11.2092394555024));
#68879=CARTESIAN_POINT('Ctrl Pts',(87.0810914547256,61.1582096809646,11.2010175135799));
#68880=CARTESIAN_POINT('Ctrl Pts',(87.0844769280797,61.1577131947244,11.1973921455412));
#68881=CARTESIAN_POINT('Ctrl Pts',(87.0921532048355,61.1565981260506,11.1892678786788));
#68882=CARTESIAN_POINT('Ctrl Pts',(87.0964559088106,61.1559804611541,11.1847805285864));
#68883=CARTESIAN_POINT('Ctrl Pts',(87.1097416404478,61.1540948872056,11.1711267818698));
#68884=CARTESIAN_POINT('Ctrl Pts',(87.1188312642634,61.1528346942871,11.1620643271838));
#68885=CARTESIAN_POINT('Ctrl Pts',(87.1406815195704,61.1498699967572,11.1409301609979));
#68886=CARTESIAN_POINT('Ctrl Pts',(87.1535585926777,61.1481731429188,11.1289819682498));
#68887=CARTESIAN_POINT('Ctrl Pts',(87.2036620712746,61.1417388791285,11.0843909242261));
#68888=CARTESIAN_POINT('Ctrl Pts',(87.2425406993975,61.1370881237777,11.0536649486747));
#68889=CARTESIAN_POINT('Ctrl Pts',(87.356348863081,61.1240699380585,10.9740668895071));
#68890=CARTESIAN_POINT('Ctrl Pts',(87.4347697595617,61.1157448178542,10.9307284802098));
#68891=CARTESIAN_POINT('Ctrl Pts',(87.5328437137496,61.105462649378,10.8893270340845));
#68892=CARTESIAN_POINT('Ctrl Pts',(87.5487373255274,61.1038009429318,10.8829928752773));
#68893=CARTESIAN_POINT('Ctrl Pts',(87.5749705045162,61.1010619571658,10.8731473780626));
#68894=CARTESIAN_POINT('Ctrl Pts',(87.5852364499097,61.0999910288497,10.8694447443717));
#68895=CARTESIAN_POINT('Ctrl Pts',(87.6038674442362,61.0980482446964,10.8629951865937));
#68896=CARTESIAN_POINT('Ctrl Pts',(87.6122158885585,61.0971779728037,10.8602020394627));
#68897=CARTESIAN_POINT('Ctrl Pts',(87.6302657337038,61.0952965013182,10.8543710317888));
#68898=CARTESIAN_POINT('Ctrl Pts',(87.6399758362254,61.0942844103567,10.8513624439303));
#68899=CARTESIAN_POINT('Ctrl Pts',(87.6671365777793,61.0914527806203,10.8433029941487));
#68900=CARTESIAN_POINT('Ctrl Pts',(87.6846601772915,61.0896250953969,10.8385097745132));
#68901=CARTESIAN_POINT('Ctrl Pts',(87.714274428277,61.0865329805987,10.8310883223467));
#68902=CARTESIAN_POINT('Ctrl Pts',(87.7263121731393,61.0852751641626,10.8282578091236));
#68903=CARTESIAN_POINT('Ctrl Pts',(87.774521455922,61.0802331881509,10.8176624944004));
#68904=CARTESIAN_POINT('Ctrl Pts',(87.8109795044834,61.0764091539188,10.8113048901459));
#68905=CARTESIAN_POINT('Ctrl Pts',(87.8974968938016,61.067309091157,10.8000842701767));
#68906=CARTESIAN_POINT('Ctrl Pts',(87.9476713247721,61.0620107311654,10.7965850118377));
#68907=CARTESIAN_POINT('Ctrl Pts',(88.0607301794632,61.0500912236701,10.7954202989757));
#68908=CARTESIAN_POINT('Ctrl Pts',(88.1235143050014,61.0434843535356,10.7994342424218));
#68909=CARTESIAN_POINT('Ctrl Pts',(88.1955697362612,61.0360563850724,10.809444286739));
#68910=CARTESIAN_POINT('Ctrl Pts',(88.2053717229579,61.0350493984819,10.8109231483707));
#68911=CARTESIAN_POINT('Ctrl Pts',(88.2207621876077,61.0334746972684,10.8134298069568));
#68912=CARTESIAN_POINT('Ctrl Pts',(88.2263624573441,61.0329030362407,10.8143805368816));
#68913=CARTESIAN_POINT('Ctrl Pts',(88.2369050316431,61.0318296238916,10.8162431554671));
#68914=CARTESIAN_POINT('Ctrl Pts',(88.2418483653488,61.0313274801299,10.8171468108872));
#68915=CARTESIAN_POINT('Ctrl Pts',(88.253651932329,61.0301310568997,10.819377019088));
#68916=CARTESIAN_POINT('Ctrl Pts',(88.2605068330879,61.0294383075161,10.8207308863672));
#68917=CARTESIAN_POINT('Ctrl Pts',(88.2843077099293,61.0270390483697,10.825636079233));
#68918=CARTESIAN_POINT('Ctrl Pts',(88.3011932016384,61.0253475649794,10.8294775484408));
#68919=CARTESIAN_POINT('Ctrl Pts',(88.3437333254339,61.0211001923123,10.8400750290017));
#68920=CARTESIAN_POINT('Ctrl Pts',(88.3692656287461,61.0185639679914,10.8472918696938));
#68921=CARTESIAN_POINT('Ctrl Pts',(88.4501762774964,61.0105104628984,10.8729248259525));
#68922=CARTESIAN_POINT('Ctrl Pts',(88.5045198787597,61.005073948271,10.8943587963042));
#68923=CARTESIAN_POINT('Ctrl Pts',(88.6210301410554,60.9929708391837,10.9498628262516));
#68924=CARTESIAN_POINT('Ctrl Pts',(88.6821990394206,60.9863054711784,10.9855426450779));
#68925=CARTESIAN_POINT('Ctrl Pts',(88.753044660125,60.9779160091621,11.0352135982266));
#68926=CARTESIAN_POINT('Ctrl Pts',(88.7658419663205,60.9763719803194,11.0445478786973));
#68927=CARTESIAN_POINT('Ctrl Pts',(88.7861729448367,60.9738695905455,11.0599678936001));
#68928=CARTESIAN_POINT('Ctrl Pts',(88.7938177910461,60.9729170333199,11.0659050111927));
#68929=CARTESIAN_POINT('Ctrl Pts',(88.8083545369346,60.9710826353569,11.0774632904678));
#68930=CARTESIAN_POINT('Ctrl Pts',(88.8152567515651,60.970201386458,11.0830706276716));
#68931=CARTESIAN_POINT('Ctrl Pts',(88.8311424705024,60.9681486344805,11.0962554757889));
#68932=CARTESIAN_POINT('Ctrl Pts',(88.8400806297975,60.9669750316463,11.1038859737154));
#68933=CARTESIAN_POINT('Ctrl Pts',(88.8689971129555,60.9631151768505,11.1292741111193));
#68934=CARTESIAN_POINT('Ctrl Pts',(88.8885192136849,60.9604083025854,11.1475370490353));
#68935=CARTESIAN_POINT('Ctrl Pts',(88.9347047723489,60.9537434668865,11.193560855304));
#68936=CARTESIAN_POINT('Ctrl Pts',(88.9607088606649,60.9497618104299,11.2219425553835));
#68937=CARTESIAN_POINT('Ctrl Pts',(89.0163915522431,60.9406959988066,11.2885519780994));
#68938=CARTESIAN_POINT('Ctrl Pts',(89.0452557537259,60.9355975275298,11.327385017742));
#68939=CARTESIAN_POINT('Ctrl Pts',(89.1060456107791,60.9239415903658,11.4197437121655));
#68940=CARTESIAN_POINT('Ctrl Pts',(89.1363959033959,60.9173984971018,11.4741735715995));
#68941=CARTESIAN_POINT('Ctrl Pts',(89.1668546779078,60.9100213509881,11.5396920034315));
#68942=CARTESIAN_POINT('Ctrl Pts',(89.1709661546454,60.9090047869203,11.5488165832606));
#68943=CARTESIAN_POINT('Ctrl Pts',(89.1772270701165,60.9074244088925,11.5631617838762));
#68944=CARTESIAN_POINT('Ctrl Pts',(89.179450151319,60.9068565019175,11.5683494206702));
#68945=CARTESIAN_POINT('Ctrl Pts',(89.1835915678772,60.9057857640645,11.5781943204696));
#68946=CARTESIAN_POINT('Ctrl Pts',(89.1855168093425,60.9052825737449,11.5828482303154));
#68947=CARTESIAN_POINT('Ctrl Pts',(89.1900751038955,60.9040777278912,11.5940553306564));
#68948=CARTESIAN_POINT('Ctrl Pts',(89.1926812861844,60.9033776619704,11.6006192762808));
#68949=CARTESIAN_POINT('Ctrl Pts',(89.2016649977172,60.9009229681647,11.623807852012));
#68950=CARTESIAN_POINT('Ctrl Pts',(89.2077480261505,60.8991843069884,11.6405457599817));
#68951=CARTESIAN_POINT('Ctrl Pts',(89.2183138738299,60.896004635772,11.6716407926697));
#68952=CARTESIAN_POINT('Ctrl Pts',(89.2228974043795,60.8945597512141,11.6859595955782));
#68953=CARTESIAN_POINT('Ctrl Pts',(89.2456589669431,60.8870032528819,11.7616706560523));
#68954=CARTESIAN_POINT('Ctrl Pts',(89.2594309872615,60.8810352614868,11.8242961205546));
#68955=CARTESIAN_POINT('Ctrl Pts',(89.2781796805407,60.8685199852618,11.9565160652157));
#68956=CARTESIAN_POINT('Ctrl Pts',(89.2822707927093,60.8619859315341,12.0260082065138));
#68957=CARTESIAN_POINT('Ctrl Pts',(89.280252563712,60.8535914638408,12.1129335871577));
#68958=CARTESIAN_POINT('Ctrl Pts',(89.2794874279133,60.8518962720116,12.1303770765571));
#68959=CARTESIAN_POINT('Ctrl Pts',(89.2776535696369,60.8491136624061,12.1587904374643));
#68960=CARTESIAN_POINT('Ctrl Pts',(89.2768011647089,60.8480329507486,12.169772459961));
#68961=CARTESIAN_POINT('Ctrl Pts',(89.2750100442652,60.8460797235869,12.1895161292931));
#68962=CARTESIAN_POINT('Ctrl Pts',(89.274122767168,60.8452088693105,12.1982818633572));
#68963=CARTESIAN_POINT('Ctrl Pts',(89.2720236368538,60.8433342498632,12.2170669934459));
#68964=CARTESIAN_POINT('Ctrl Pts',(89.2707834174856,60.8423296523453,12.2270825103945));
#68965=CARTESIAN_POINT('Ctrl Pts',(89.2670248058407,60.8395415410742,12.254729674854));
#68966=CARTESIAN_POINT('Ctrl Pts',(89.2642547881442,60.8377502875678,12.2723239112516));
#68967=CARTESIAN_POINT('Ctrl Pts',(89.2589934742126,60.8347284564266,12.3017059307708));
#68968=CARTESIAN_POINT('Ctrl Pts',(89.2567026399418,60.8335043106551,12.3135275855586));
#68969=CARTESIAN_POINT('Ctrl Pts',(89.2389980980549,60.824652893876,12.3984093721431));
#68970=CARTESIAN_POINT('Ctrl Pts',(89.2173384930778,60.8168427602217,12.4700031991672));
#68971=CARTESIAN_POINT('Ctrl Pts',(89.1626360546246,60.8013719478287,12.6062225263108));
#68972=CARTESIAN_POINT('Ctrl Pts',(89.1300881947497,60.7937436940406,12.6707727794641));
#68973=CARTESIAN_POINT('Ctrl Pts',(89.0856267235519,60.7850533668111,12.7429311819748));
#68974=CARTESIAN_POINT('Ctrl Pts',(89.0788647144251,60.783770472458,12.7535488455974));
#68975=CARTESIAN_POINT('Ctrl Pts',(89.0685546012126,60.7818726872346,12.7692185460344));
#68976=CARTESIAN_POINT('Ctrl Pts',(89.0651260620089,60.7812507729356,12.7743475907114));
#68977=CARTESIAN_POINT('Ctrl Pts',(89.0588733419653,60.7801332160649,12.7835556202448));
#68978=CARTESIAN_POINT('Ctrl Pts',(89.0560625253225,60.7796367615692,12.7876432153033));
#68979=CARTESIAN_POINT('Ctrl Pts',(89.0496409850005,60.7785158198425,12.7968654462353));
#68980=CARTESIAN_POINT('Ctrl Pts',(89.0460160555439,60.7778922988448,12.8019899232609));
#68981=CARTESIAN_POINT('Ctrl Pts',(89.0346789594999,60.7759697717492,12.8177674790722));
#68982=CARTESIAN_POINT('Ctrl Pts',(89.0268387989926,60.7746789252239,12.8283283668475));
#68983=CARTESIAN_POINT('Ctrl Pts',(89.0077931929692,60.7716278772176,12.8531674889036));
#68984=CARTESIAN_POINT('Ctrl Pts',(88.9964426871776,60.7698759442727,12.8673314783633));
#68985=CARTESIAN_POINT('Ctrl Pts',(88.9510873718701,60.7631039097122,12.9215071458703));
#68986=CARTESIAN_POINT('Ctrl Pts',(88.9149153462751,60.7581802009993,12.9596413994253));
#68987=CARTESIAN_POINT('Ctrl Pts',(88.8143090140788,60.7452996489449,13.0533257270498));
#68988=CARTESIAN_POINT('Ctrl Pts',(88.7464928553373,60.7373692821362,13.1048284635556));
#68989=CARTESIAN_POINT('Ctrl Pts',(88.6593103316625,60.7274982961221,13.1581961392912));
#68990=CARTESIAN_POINT('Ctrl Pts',(88.6443882420474,60.7258199663285,13.1669168725673));
#68991=CARTESIAN_POINT('Ctrl Pts',(88.6197168925839,60.7230593173874,13.1806676413267));
#68992=CARTESIAN_POINT('Ctrl Pts',(88.6100717616313,60.7219835244706,13.1858808918232));
#68993=CARTESIAN_POINT('Ctrl Pts',(88.5925596452606,60.7200355639199,13.1950553301142));
#68994=CARTESIAN_POINT('Ctrl Pts',(88.5847165324487,60.7191650186697,13.1990608500753));
#68995=CARTESIAN_POINT('Ctrl Pts',(88.5677650927728,60.7172870337944,13.2074969186101));
#68996=CARTESIAN_POINT('Ctrl Pts',(88.5586442293293,60.7162787325571,13.2119006791855));
#68997=CARTESIAN_POINT('Ctrl Pts',(88.5331827029968,60.7134691410883,13.2238206775217));
#68998=CARTESIAN_POINT('Ctrl Pts',(88.5167343548591,60.7116599115199,13.2310992119881));
#68999=CARTESIAN_POINT('Ctrl Pts',(88.479408356469,60.7075643917685,13.2466770004623));
#69000=CARTESIAN_POINT('Ctrl Pts',(88.4584544621202,60.7052721971682,13.2547762260141));
#69001=CARTESIAN_POINT('Ctrl Pts',(88.3872739183882,60.6975047363219,13.280140911208));
#69002=CARTESIAN_POINT('Ctrl Pts',(88.336187508737,60.6919586518948,13.2948091072172));
#69003=CARTESIAN_POINT('Ctrl Pts',(88.2019451115022,60.6774955219948,13.3243952643226));
#69004=CARTESIAN_POINT('Ctrl Pts',(88.1179380832077,60.6685410013155,13.3343003868593));
#69005=CARTESIAN_POINT('Ctrl Pts',(88.0219927568398,60.6587150348582,13.3360051344541));
#69006=CARTESIAN_POINT('Ctrl Pts',(88.0104208184317,60.6575368493075,13.3360525898162));
#69007=CARTESIAN_POINT('Ctrl Pts',(87.9928077368159,60.6557555584152,13.3358840668625));
#69008=CARTESIAN_POINT('Ctrl Pts',(87.98676660887,60.6551467357265,13.3357831507682));
#69009=CARTESIAN_POINT('Ctrl Pts',(87.9762590791396,60.654091762245,13.3355326049295));
#69010=CARTESIAN_POINT('Ctrl Pts',(87.9717925690407,60.6536445851165,13.3354025154184));
#69011=CARTESIAN_POINT('Ctrl Pts',(87.9611784734092,60.6525848889832,13.3350372962565));
#69012=CARTESIAN_POINT('Ctrl Pts',(87.9550317626866,60.65197354117,13.3347810709605));
#69013=CARTESIAN_POINT('Ctrl Pts',(87.9364053494587,60.650127336134,13.3338690000461));
#69014=CARTESIAN_POINT('Ctrl Pts',(87.923932617156,60.6488997362385,13.3330735878738));
#69015=CARTESIAN_POINT('Ctrl Pts',(87.8607344508875,60.6427137320059,13.3281056032403));
#69016=CARTESIAN_POINT('Ctrl Pts',(87.8102730065004,60.6378853542181,13.3210699938175));
#69017=CARTESIAN_POINT('Ctrl Pts',(87.669639195398,60.6243844507333,13.2927587679696));
#69018=CARTESIAN_POINT('Ctrl Pts',(87.5811911999741,60.6158212116285,13.2646355601221));
#69019=CARTESIAN_POINT('Ctrl Pts',(87.4717296322412,60.6043568101499,13.216141992184));
#69020=CARTESIAN_POINT('Ctrl Pts',(87.4472349491453,60.601732816823,13.2043355626842));
#69021=CARTESIAN_POINT('Ctrl Pts',(87.4134303393534,60.5980142202727,13.1866830431926));
#69022=CARTESIAN_POINT('Ctrl Pts',(87.4037871783418,60.596942031329,13.1814875856111));
#69023=CARTESIAN_POINT('Ctrl Pts',(87.3866573811285,60.5950159276153,13.1719706137417));
#69024=CARTESIAN_POINT('Ctrl Pts',(87.3791452659407,60.5941637161662,13.1676960969297));
#69025=CARTESIAN_POINT('Ctrl Pts',(87.3644879467617,60.5924855983681,13.1591566226551));
#69026=CARTESIAN_POINT('Ctrl Pts',(87.3573398616816,60.5916599360368,13.1548974477872));
#69027=CARTESIAN_POINT('Ctrl Pts',(87.3425504892741,60.5899360419425,13.145887127631));
#69028=CARTESIAN_POINT('Ctrl Pts',(87.3349168460184,60.5890374233177,13.1411244183783));
#69029=CARTESIAN_POINT('Ctrl Pts',(87.3169723512385,60.586903576258,13.1296619832101));
#69030=CARTESIAN_POINT('Ctrl Pts',(87.306707156875,60.5856658523402,13.1228929726749));
#69031=CARTESIAN_POINT('Ctrl Pts',(87.2794312088592,60.5823298592722,13.1043330195237));
#69032=CARTESIAN_POINT('Ctrl Pts',(87.2626085781958,60.5802219721444,13.0922740917119));
#69033=CARTESIAN_POINT('Ctrl Pts',(87.2236901005184,60.5752223005046,13.0629104536629));
#69034=CARTESIAN_POINT('Ctrl Pts',(87.201862967003,60.5723202688287,13.0452771747944));
#69035=CARTESIAN_POINT('Ctrl Pts',(87.180642808438,60.5693987930815,13.0269406508319));
#69036=CARTESIAN_POINT('Origin',(88.011,66.41344859951,12.066));
#69037=CARTESIAN_POINT('',(87.1806428411249,59.6047173123478,13.026940679077));
#69038=CARTESIAN_POINT('',(87.1806428354195,59.7737921350435,13.0269406741468));
#69039=CARTESIAN_POINT('',(87.1806428354228,66.41344859951,13.0269406741497));
#69040=CARTESIAN_POINT('',(86.7410003192602,60.2915568442934,12.0650994886321));
#69041=CARTESIAN_POINT('Ctrl Pts',(87.1806428411249,59.6047173123478,13.026940679077));
#69042=CARTESIAN_POINT('Ctrl Pts',(87.1864097172424,59.6055103894119,13.0319238866493));
#69043=CARTESIAN_POINT('Ctrl Pts',(87.1922216809976,59.606304961203,13.0368553793557));
#69044=CARTESIAN_POINT('Ctrl Pts',(87.2352838327035,59.6121574675507,13.072732113043));
#69045=CARTESIAN_POINT('Ctrl Pts',(87.2742300148467,59.6172640675625,13.1015745071691));
#69046=CARTESIAN_POINT('Ctrl Pts',(87.3667989435877,59.6289324183003,13.1622581943341));
#69047=CARTESIAN_POINT('Ctrl Pts',(87.4213210504429,59.6354798136871,13.1925248111393));
#69048=CARTESIAN_POINT('Ctrl Pts',(87.4868321943151,59.6428495403356,13.2228258344779));
#69049=CARTESIAN_POINT('Ctrl Pts',(87.4958612845595,59.6438547139304,13.2268746813009));
#69050=CARTESIAN_POINT('Ctrl Pts',(87.5101440154885,59.6454272862379,13.2330799073028));
#69051=CARTESIAN_POINT('Ctrl Pts',(87.5153660527098,59.6459986135798,13.2353071547618));
#69052=CARTESIAN_POINT('Ctrl Pts',(87.5252408018775,59.6470719273441,13.2394407864639));
#69053=CARTESIAN_POINT('Ctrl Pts',(87.5298899555873,59.6475743023467,13.2413545869324));
#69054=CARTESIAN_POINT('Ctrl Pts',(87.541037097452,59.6487720045797,13.2458660246204));
#69055=CARTESIAN_POINT('Ctrl Pts',(87.5475454258268,59.6494657938174,13.2484376651068));
#69056=CARTESIAN_POINT('Ctrl Pts',(87.5702883978015,59.6518723037355,13.257207474264));
#69057=CARTESIAN_POINT('Ctrl Pts',(87.5866299078509,59.6535698789825,13.2631265999381));
#69058=CARTESIAN_POINT('Ctrl Pts',(87.6283376759949,59.6578363645302,13.2772722072251));
#69059=CARTESIAN_POINT('Ctrl Pts',(87.6538519698315,59.6603853856485,13.2850391172413));
#69060=CARTESIAN_POINT('Ctrl Pts',(87.7780622303438,59.67259281175,13.3186150362462));
#69061=CARTESIAN_POINT('Ctrl Pts',(87.8793770561229,59.6819728373679,13.3332729795152));
#69062=CARTESIAN_POINT('Ctrl Pts',(87.9960907178478,59.6931026882281,13.3359980075827));
#69063=CARTESIAN_POINT('Ctrl Pts',(88.0108295516206,59.6945133750901,13.3360854940337));
#69064=CARTESIAN_POINT('Ctrl Pts',(88.0485557527999,59.6981421129972,13.3356527730552));
#69065=CARTESIAN_POINT('Ctrl Pts',(88.0715323361801,59.7003692108582,13.33476486405));
#69066=CARTESIAN_POINT('Ctrl Pts',(88.1055527931119,59.703700584226,13.3325240299627));
#69067=CARTESIAN_POINT('Ctrl Pts',(88.1166245510807,59.7047900686572,13.331648760194));
#69068=CARTESIAN_POINT('Ctrl Pts',(88.1364654235879,59.7067529318179,13.3298181100854));
#69069=CARTESIAN_POINT('Ctrl Pts',(88.1452388992882,59.7076245811301,13.3289163455667));
#69070=CARTESIAN_POINT('Ctrl Pts',(88.1639721613022,59.7094941193103,13.3267934797504));
#69071=CARTESIAN_POINT('Ctrl Pts',(88.1739282115889,59.7104927918946,13.3255455782775));
#69072=CARTESIAN_POINT('Ctrl Pts',(88.2012288276228,59.7132460293099,13.3217946005028));
#69073=CARTESIAN_POINT('Ctrl Pts',(88.2185371968415,59.7150080124499,13.3190504054622));
#69074=CARTESIAN_POINT('Ctrl Pts',(88.3157681182293,59.7250055510302,13.3015650725707));
#69075=CARTESIAN_POINT('Ctrl Pts',(88.394169293903,59.7334663216204,13.2795402324954));
#69076=CARTESIAN_POINT('Ctrl Pts',(88.5433942704597,59.7503199452271,13.2217105435813));
#69077=CARTESIAN_POINT('Ctrl Pts',(88.6140739312873,59.7586695006284,13.1864530980265));
#69078=CARTESIAN_POINT('Ctrl Pts',(88.6913663863026,59.7679925812268,13.1384502198198));
#69079=CARTESIAN_POINT('Ctrl Pts',(88.701605302034,59.7692314905063,13.1318856644774));
#69080=CARTESIAN_POINT('Ctrl Pts',(88.7168255736375,59.7710773894026,13.1218159459799));
#69081=CARTESIAN_POINT('Ctrl Pts',(88.7218781294407,59.7716908725467,13.1184207062269));
#69082=CARTESIAN_POINT('Ctrl Pts',(88.7305961863776,59.772750421393,13.1124708718982));
#69083=CARTESIAN_POINT('Ctrl Pts',(88.7342727838351,59.7731975499993,13.1099331586263));
#69084=CARTESIAN_POINT('Ctrl Pts',(88.7429434987344,59.7742527741648,13.1038805356081));
#69085=CARTESIAN_POINT('Ctrl Pts',(88.7479257749815,59.7748597336624,13.1003489253615));
#69086=CARTESIAN_POINT('Ctrl Pts',(88.7628342433868,59.7766784885708,13.0896188781199));
#69087=CARTESIAN_POINT('Ctrl Pts',(88.7726823438275,59.7778833397084,13.0823121494428));
#69088=CARTESIAN_POINT('Ctrl Pts',(88.8211592819316,59.7838406141739,13.0452444361687));
#69089=CARTESIAN_POINT('Ctrl Pts',(88.8581633820857,59.7884735469755,13.0134141081119));
#69090=CARTESIAN_POINT('Ctrl Pts',(88.9553545022076,59.8012014539556,12.9195507615541));
#69091=CARTESIAN_POINT('Ctrl Pts',(89.0111779383046,59.8091935424723,12.8533993574653));
#69092=CARTESIAN_POINT('Ctrl Pts',(89.0788260111468,59.8206247317788,12.7543162161129));
#69093=CARTESIAN_POINT('Ctrl Pts',(89.0966804607157,59.823858328215,12.7257947399214));
#69094=CARTESIAN_POINT('Ctrl Pts',(89.1198832983829,59.8284075651725,12.6852328744903));
#69095=CARTESIAN_POINT('Ctrl Pts',(89.126209721781,59.8296883706978,12.6737653887985));
#69096=CARTESIAN_POINT('Ctrl Pts',(89.136211366755,59.831782303417,12.6549539678651));
#69097=CARTESIAN_POINT('Ctrl Pts',(89.1399948398496,59.832591573042,12.6476683245687));
#69098=CARTESIAN_POINT('Ctrl Pts',(89.1478162076839,59.8343017754174,12.6322432858404));
#69099=CARTESIAN_POINT('Ctrl Pts',(89.1518378942699,59.8352032178089,12.6240962612856));
#69100=CARTESIAN_POINT('Ctrl Pts',(89.1613608888962,59.8373928856997,12.6042717208092));
#69101=CARTESIAN_POINT('Ctrl Pts',(89.1667720959559,59.8386841189874,12.5925524196967));
#69102=CARTESIAN_POINT('Ctrl Pts',(89.1860430979034,59.84346339771,12.5490875137389));
#69103=CARTESIAN_POINT('Ctrl Pts',(89.1987795089136,59.8469882551037,12.5168648171855));
#69104=CARTESIAN_POINT('Ctrl Pts',(89.2290399227496,59.8564470715648,12.4300864458039));
#69105=CARTESIAN_POINT('Ctrl Pts',(89.2442154831554,59.8624416981865,12.3748009500596));
#69106=CARTESIAN_POINT('Ctrl Pts',(89.2709802489522,59.876610886668,12.2429718009351));
#69107=CARTESIAN_POINT('Ctrl Pts',(89.2794129723557,59.8847926316677,12.1660025816947));
#69108=CARTESIAN_POINT('Ctrl Pts',(89.2810159498217,59.8939688087022,12.0764783079947));
#69109=CARTESIAN_POINT('Ctrl Pts',(89.281057939044,59.8952179381108,12.0642169003687));
#69110=CARTESIAN_POINT('Ctrl Pts',(89.2808548198468,59.8970759276727,12.0458499340424));
#69111=CARTESIAN_POINT('Ctrl Pts',(89.2807432524481,59.8976914027513,12.039744197116));
#69112=CARTESIAN_POINT('Ctrl Pts',(89.2804738281,59.8987528852676,12.0291740447635));
#69113=CARTESIAN_POINT('Ctrl Pts',(89.2803364583437,59.8991999714567,12.0247094549634));
#69114=CARTESIAN_POINT('Ctrl Pts',(89.2799562305113,59.9002532161487,12.0141624067431));
#69115=CARTESIAN_POINT('Ctrl Pts',(89.2796931961772,59.9008582537826,12.0080808266201));
#69116=CARTESIAN_POINT('Ctrl Pts',(89.2787736243369,59.9026652327298,11.9898559320102));
#69117=CARTESIAN_POINT('Ctrl Pts',(89.2779863633824,59.9038603613856,11.977719330808));
#69118=CARTESIAN_POINT('Ctrl Pts',(89.2763244812151,59.9059127747364,11.9567643369617));
#69119=CARTESIAN_POINT('Ctrl Pts',(89.2755317333161,59.9067735818509,11.9479407712464));
#69120=CARTESIAN_POINT('Ctrl Pts',(89.2730897073606,59.909138897631,11.9236185738));
#69121=CARTESIAN_POINT('Ctrl Pts',(89.271247309638,59.9106357267777,11.9081403248429));
#69122=CARTESIAN_POINT('Ctrl Pts',(89.2597845629129,59.9186578040058,11.8249237544407));
#69123=CARTESIAN_POINT('Ctrl Pts',(89.2449866405748,59.9250221903631,11.75800758475));
#69124=CARTESIAN_POINT('Ctrl Pts',(89.2041894126595,59.9380363026289,11.6253803430995));
#69125=CARTESIAN_POINT('Ctrl Pts',(89.1779660158645,59.9446679931572,11.5600016955939));
#69126=CARTESIAN_POINT('Ctrl Pts',(89.1393850022589,59.9530198165272,11.4829926702472));
#69127=CARTESIAN_POINT('Ctrl Pts',(89.1320357610648,59.9545619574872,11.4689832255249));
#69128=CARTESIAN_POINT('Ctrl Pts',(89.1197725492024,59.9570621731697,11.4466317146102));
#69129=CARTESIAN_POINT('Ctrl Pts',(89.1150212922957,59.9580144648305,11.4382017743882));
#69130=CARTESIAN_POINT('Ctrl Pts',(89.1057179510166,59.9598489450729,11.4221275340114));
#69131=CARTESIAN_POINT('Ctrl Pts',(89.1011809354346,59.9607305460383,11.414475125187));
#69132=CARTESIAN_POINT('Ctrl Pts',(89.0904576251176,59.9627850188581,11.3968141746501));
#69133=CARTESIAN_POINT('Ctrl Pts',(89.0842120113998,59.9639599998065,11.3868428842323));
#69134=CARTESIAN_POINT('Ctrl Pts',(89.0632870827719,59.9678287305611,11.3544451587661));
#69135=CARTESIAN_POINT('Ctrl Pts',(89.0480375049121,59.9705432319403,11.3323983821087));
#69136=CARTESIAN_POINT('Ctrl Pts',(89.0091343643087,59.9772315374075,11.2797939179607));
#69137=CARTESIAN_POINT('Ctrl Pts',(88.9847630422855,59.9812292611661,11.2498032924139));
#69138=CARTESIAN_POINT('Ctrl Pts',(88.9270065427525,59.9902944739702,11.185004216518));
#69139=CARTESIAN_POINT('Ctrl Pts',(88.8929278862889,59.9953755545205,11.1508911396011));
#69140=CARTESIAN_POINT('Ctrl Pts',(88.8106526160103,60.0070045235533,11.0774067049815));
#69141=CARTESIAN_POINT('Ctrl Pts',(88.7613264999452,60.0135380054576,11.0394652815236));
#69142=CARTESIAN_POINT('Ctrl Pts',(88.7010562978377,60.0209058781142,10.9997812520955));
#69143=CARTESIAN_POINT('Ctrl Pts',(88.6926342869865,60.0219222813916,10.9943774759073));
#69144=CARTESIAN_POINT('Ctrl Pts',(88.6793628225291,60.0235025390601,10.9860819509878));
#69145=CARTESIAN_POINT('Ctrl Pts',(88.6745567692603,60.0240704844305,10.9831222258957));
#69146=CARTESIAN_POINT('Ctrl Pts',(88.6654237918273,60.0251413967369,10.9775814772922));
#69147=CARTESIAN_POINT('Ctrl Pts',(88.6611011912416,60.0256447224984,10.9749941233115));
#69148=CARTESIAN_POINT('Ctrl Pts',(88.6506791329427,60.0268500484688,10.9688397893295));
#69149=CARTESIAN_POINT('Ctrl Pts',(88.6445650759542,60.02755045681,10.9652978494961));
#69150=CARTESIAN_POINT('Ctrl Pts',(88.62292558838,60.0300071937132,10.9530019196291));
#69151=CARTESIAN_POINT('Ctrl Pts',(88.607244606253,60.0317475226326,10.9445232332478));
#69152=CARTESIAN_POINT('Ctrl Pts',(88.5780001452554,60.0349307524802,10.9294977277729));
#69153=CARTESIAN_POINT('Ctrl Pts',(88.5644893508698,60.0363775259461,10.922856889301));
#69154=CARTESIAN_POINT('Ctrl Pts',(88.4927741574754,60.0439501632778,10.8891770815599));
#69155=CARTESIAN_POINT('Ctrl Pts',(88.43269557612,60.049931829868,10.8663363191612));
#69156=CARTESIAN_POINT('Ctrl Pts',(88.2985520681039,60.06304185434,10.8266679337592));
#69157=CARTESIAN_POINT('Ctrl Pts',(88.2242004812316,60.0701614273871,10.8117382201878));
#69158=CARTESIAN_POINT('Ctrl Pts',(88.1332438405693,60.0790334730091,10.8017979816399));
#69159=CARTESIAN_POINT('Ctrl Pts',(88.1174867396182,60.0805757348901,10.8003733485823));
#69160=CARTESIAN_POINT('Ctrl Pts',(88.0920556933111,60.0830760981488,10.7985523211855));
#69161=CARTESIAN_POINT('Ctrl Pts',(88.0823961825634,60.0840284152009,10.7979715239093));
#69162=CARTESIAN_POINT('Ctrl Pts',(88.0638455724982,60.0858629121552,10.7970687612349));
#69163=CARTESIAN_POINT('Ctrl Pts',(88.0549558346225,60.0867445041974,10.7967297302787));
#69164=CARTESIAN_POINT('Ctrl Pts',(88.0343028683971,60.0887989077393,10.7961593030879));
#69165=CARTESIAN_POINT('Ctrl Pts',(88.0225387612108,60.0899738278763,10.7959979321907));
#69166=CARTESIAN_POINT('Ctrl Pts',(87.9839753426639,60.0938421275821,10.7960047761247));
#69167=CARTESIAN_POINT('Ctrl Pts',(87.9571856743054,60.096556252264,10.7968577924654));
#69168=CARTESIAN_POINT('Ctrl Pts',(87.8919016807957,60.1032433876287,10.8010070282923));
#69169=CARTESIAN_POINT('Ctrl Pts',(87.8534943888634,60.1072403065903,10.8052133700512));
#69170=CARTESIAN_POINT('Ctrl Pts',(87.7677270955098,60.116305550617,10.8185864142649));
#69171=CARTESIAN_POINT('Ctrl Pts',(87.7205753850193,60.1213875033316,10.8287145161416));
#69172=CARTESIAN_POINT('Ctrl Pts',(87.6187766849386,60.1325175375429,10.856721232812));
#69173=CARTESIAN_POINT('Ctrl Pts',(87.5645253362169,60.1385536229741,10.8756822297417));
#69174=CARTESIAN_POINT('Ctrl Pts',(87.4998954229557,60.1457636480785,10.9033143340654));
#69175=CARTESIAN_POINT('Ctrl Pts',(87.4881309988338,60.1470767142894,10.9085571719467));
#69176=CARTESIAN_POINT('Ctrl Pts',(87.4708001538758,60.1490101144421,10.916598900991));
#69177=CARTESIAN_POINT('Ctrl Pts',(87.4651718654194,60.1496378446864,10.9192609653247));
#69178=CARTESIAN_POINT('Ctrl Pts',(87.4584587260366,60.1503862057366,10.9224967670559));
#69179=CARTESIAN_POINT('Ctrl Pts',(87.4573550483126,60.1505092286417,10.9230307218889));
#69180=CARTESIAN_POINT('Ctrl Pts',(87.4518139404406,60.1511268101697,10.9257213967998));
#69181=CARTESIAN_POINT('Ctrl Pts',(87.447388432745,60.1516198142492,10.9279023129664));
#69182=CARTESIAN_POINT('Ctrl Pts',(87.4369574145216,60.1527814766958,10.9331185480976));
#69183=CARTESIAN_POINT('Ctrl Pts',(87.430963106902,60.153448774139,10.9361759056805));
#69184=CARTESIAN_POINT('Ctrl Pts',(87.4180891489265,60.1548820069591,10.9428716541163));
#69185=CARTESIAN_POINT('Ctrl Pts',(87.4112180120408,60.1556470071798,10.9465259556218));
#69186=CARTESIAN_POINT('Ctrl Pts',(87.3921310462667,60.1577735138657,10.9569032395713));
#69187=CARTESIAN_POINT('Ctrl Pts',(87.379991180918,60.1591277146882,10.9637648492937));
#69188=CARTESIAN_POINT('Ctrl Pts',(87.3389280877992,60.1637232982886,10.9878751295065));
#69189=CARTESIAN_POINT('Ctrl Pts',(87.3105766907857,60.166922265155,11.0060747442042));
#69190=CARTESIAN_POINT('Ctrl Pts',(87.1896864994572,60.1808407732127,11.0906499720599));
#69191=CARTESIAN_POINT('Ctrl Pts',(87.1056036715962,60.1913174326432,11.1681589650204));
#69192=CARTESIAN_POINT('Ctrl Pts',(87.0216008061686,60.2040500693866,11.2695658862431));
#69193=CARTESIAN_POINT('Ctrl Pts',(87.0105150689038,60.205784669366,11.2835372916383));
#69194=CARTESIAN_POINT('Ctrl Pts',(86.9935569676644,60.2085296434995,11.3058593985644));
#69195=CARTESIAN_POINT('Ctrl Pts',(86.9874844467381,60.2095321587437,11.3140558829107));
#69196=CARTESIAN_POINT('Ctrl Pts',(86.9764062663062,60.2113986689382,11.3293916798485));
#69197=CARTESIAN_POINT('Ctrl Pts',(86.9713740751679,60.2122615789653,11.3365111804052));
#69198=CARTESIAN_POINT('Ctrl Pts',(86.9602553064012,60.2142029402878,11.3525906441391));
#69199=CARTESIAN_POINT('Ctrl Pts',(86.9542093497211,60.2152828483266,11.3615776671915));
#69200=CARTESIAN_POINT('Ctrl Pts',(86.9368718658452,60.2184529129293,11.3880746152205));
#69201=CARTESIAN_POINT('Ctrl Pts',(86.9258960611566,60.2205544333014,11.4057853483354));
#69202=CARTESIAN_POINT('Ctrl Pts',(86.9109833777392,60.2235513745861,11.4312257205569));
#69203=CARTESIAN_POINT('Ctrl Pts',(86.906681793585,60.2244338403733,11.4387390933388));
#69204=CARTESIAN_POINT('Ctrl Pts',(86.859744542713,60.2342672364061,11.5227016095568));
#69205=CARTESIAN_POINT('Ctrl Pts',(86.8250534618013,60.2434742647721,11.6033045255132));
#69206=CARTESIAN_POINT('Ctrl Pts',(86.7837308148364,60.258063347428,11.7353926333651));
#69207=CARTESIAN_POINT('Ctrl Pts',(86.7714658491329,60.2634163764788,11.7848468198341));
#69208=CARTESIAN_POINT('Ctrl Pts',(86.759208191377,60.2703618972674,11.8510862059905));
#69209=CARTESIAN_POINT('Ctrl Pts',(86.7565289271417,60.2720465568103,11.8673216457429));
#69210=CARTESIAN_POINT('Ctrl Pts',(86.753249072366,60.2743635426589,11.8899223411687));
#69211=CARTESIAN_POINT('Ctrl Pts',(86.7523800106275,60.2750087739223,11.8962458644839));
#69212=CARTESIAN_POINT('Ctrl Pts',(86.7509044314333,60.2761633440632,11.9076175386922));
#69213=CARTESIAN_POINT('Ctrl Pts',(86.7502804857078,60.2766736045223,11.9126632568548));
#69214=CARTESIAN_POINT('Ctrl Pts',(86.7491470064829,60.2776445714408,11.9223044967434));
#69215=CARTESIAN_POINT('Ctrl Pts',(86.7486322439709,60.2781055773062,11.9268992236152));
#69216=CARTESIAN_POINT('Ctrl Pts',(86.7475693927491,60.2791032882756,11.9368783878494));
#69217=CARTESIAN_POINT('Ctrl Pts',(86.7470306024409,60.2796394848085,11.9422637646658));
#69218=CARTESIAN_POINT('Ctrl Pts',(86.7457924025061,60.2809515945659,11.9554932170553));
#69219=CARTESIAN_POINT('Ctrl Pts',(86.7451314758564,60.2817255473663,11.9633408346356));
#69220=CARTESIAN_POINT('Ctrl Pts',(86.7422046944127,60.2855620549366,12.0024381294605));
#69221=CARTESIAN_POINT('Ctrl Pts',(86.7410225400618,60.288574242465,12.0337612824082));
#69222=CARTESIAN_POINT('Ctrl Pts',(86.7410003192602,60.2915568442934,12.0650994886321));
#69223=CARTESIAN_POINT('Ctrl Pts',(86.7410003205439,60.2915566721542,12.0650976799659));
#69224=CARTESIAN_POINT('Ctrl Pts',(86.7409240894383,60.3017683369366,12.172391628948));
#69225=CARTESIAN_POINT('Ctrl Pts',(86.754444143447,60.311612008104,12.2792703672195));
#69226=CARTESIAN_POINT('Ctrl Pts',(86.7868810513014,60.323995469413,12.4050305636389));
#69227=CARTESIAN_POINT('Ctrl Pts',(86.7930959706329,60.3261595322167,12.4267195163374));
#69228=CARTESIAN_POINT('Ctrl Pts',(86.8038000312691,60.3295984662617,12.4606358664787));
#69229=CARTESIAN_POINT('Ctrl Pts',(86.8079055126792,60.3308617568952,12.4729801683709));
#69230=CARTESIAN_POINT('Ctrl Pts',(86.816091144573,60.3332812383934,12.4963856159086));
#69231=CARTESIAN_POINT('Ctrl Pts',(86.8201371385682,60.3344362366402,12.5074573293389));
#69232=CARTESIAN_POINT('Ctrl Pts',(86.8275071434947,60.3364722351848,12.5267861308992));
#69233=CARTESIAN_POINT('Ctrl Pts',(86.8307650107969,60.3373509856935,12.5350677562282));
#69234=CARTESIAN_POINT('Ctrl Pts',(86.8377427669702,60.3391904691869,12.5522724710941));
#69235=CARTESIAN_POINT('Ctrl Pts',(86.8414780275297,60.3401516698282,12.5611886445296));
#69236=CARTESIAN_POINT('Ctrl Pts',(86.8515750531427,60.3426905230499,12.5845389049693));
#69237=CARTESIAN_POINT('Ctrl Pts',(86.8581043362792,60.3442737575296,12.5988980524637));
#69238=CARTESIAN_POINT('Ctrl Pts',(86.8946905820938,60.3528479841825,12.6755369723726));
#69239=CARTESIAN_POINT('Ctrl Pts',(86.9295224661454,60.3600007777607,12.735391022093));
#69240=CARTESIAN_POINT('Ctrl Pts',(87.0006619609761,60.3730558770103,12.8374762724348));
#69241=CARTESIAN_POINT('Ctrl Pts',(87.0352106775988,60.3789064665732,12.8807352945362));
#69242=CARTESIAN_POINT('Ctrl Pts',(87.0923204614892,60.3878080199549,12.9433803113379));
#69243=CARTESIAN_POINT('Ctrl Pts',(87.1129261481408,60.3908867910529,12.9644608840851));
#69244=CARTESIAN_POINT('Ctrl Pts',(87.143513253291,60.3952544368415,12.9936479634496));
#69245=CARTESIAN_POINT('Ctrl Pts',(87.1529119460423,60.3965707182698,13.0023487229686));
#69246=CARTESIAN_POINT('Ctrl Pts',(87.1684569822063,60.3987043115595,13.0163087069261));
#69247=CARTESIAN_POINT('Ctrl Pts',(87.1745244669532,60.3995266097241,13.02165373893));
#69248=CARTESIAN_POINT('Ctrl Pts',(87.1806428354305,60.4003450897931,13.0269406741563));
#69249=CARTESIAN_POINT('',(86.7410004024462,60.4614604378065,12.0655714700173));
#69250=CARTESIAN_POINT('Ctrl Pts',(87.180642808438,60.5693987930815,13.0269406508319));
#69251=CARTESIAN_POINT('Ctrl Pts',(87.1668514509425,60.5675000741667,13.01502341862));
#69252=CARTESIAN_POINT('Ctrl Pts',(87.1533164697531,60.5655932091657,13.0028091364898));
#69253=CARTESIAN_POINT('Ctrl Pts',(87.0902562106591,60.5565023682665,12.9433888841665));
#69254=CARTESIAN_POINT('Ctrl Pts',(87.0443378827768,60.5492501406696,12.8925257476688));
#69255=CARTESIAN_POINT('Ctrl Pts',(86.9836260945219,60.5388235484186,12.8132556304197));
#69256=CARTESIAN_POINT('Ctrl Pts',(86.9654433422184,60.5355685429781,12.7875953848512));
#69257=CARTESIAN_POINT('Ctrl Pts',(86.9433660937757,60.5314600235669,12.7538493754804));
#69258=CARTESIAN_POINT('Ctrl Pts',(86.9385804134176,60.5305591617554,12.7463639964599));
#69259=CARTESIAN_POINT('Ctrl Pts',(86.9310121372483,60.5291184268294,12.7342479970414));
#69260=CARTESIAN_POINT('Ctrl Pts',(86.9281799871311,60.528575528943,12.7296489983488));
#69261=CARTESIAN_POINT('Ctrl Pts',(86.922704460818,60.5275187001039,12.7206291674848));
#69262=CARTESIAN_POINT('Ctrl Pts',(86.9200585628836,60.5270046387168,12.7162102050521));
#69263=CARTESIAN_POINT('Ctrl Pts',(86.9135217458638,60.5257257833404,12.705140708422));
#69264=CARTESIAN_POINT('Ctrl Pts',(86.9096642653894,60.5249630975142,12.6984705322085));
#69265=CARTESIAN_POINT('Ctrl Pts',(86.8947589117912,60.5219823209744,12.6721469433502));
#69266=CARTESIAN_POINT('Ctrl Pts',(86.8841734188367,60.519790652363,12.6522340506068));
#69267=CARTESIAN_POINT('Ctrl Pts',(86.8264091406283,60.5073140274506,12.536217506743));
#69268=CARTESIAN_POINT('Ctrl Pts',(86.7909981577031,60.4975005910672,12.434729157224));
#69269=CARTESIAN_POINT('Ctrl Pts',(86.7594527720076,60.4831399417659,12.2862858467083));
#69270=CARTESIAN_POINT('Ctrl Pts',(86.7524792764846,60.4788719375758,12.2421277125554));
#69271=CARTESIAN_POINT('Ctrl Pts',(86.7463868075961,60.4731635595118,12.1836934824722));
#69272=CARTESIAN_POINT('Ctrl Pts',(86.7451596832995,60.471788774652,12.169665504591));
#69273=CARTESIAN_POINT('Ctrl Pts',(86.743501041776,60.4694817297081,12.1462197636754));
#69274=CARTESIAN_POINT('Ctrl Pts',(86.7429406715925,60.468553531286,12.1368120560072));
#69275=CARTESIAN_POINT('Ctrl Pts',(86.7420794162229,60.4667926861632,12.1190184430685));
#69276=CARTESIAN_POINT('Ctrl Pts',(86.7417568407576,60.4659607651159,12.1106340379479));
#69277=CARTESIAN_POINT('Ctrl Pts',(86.7413353038258,60.4644916989347,12.0958706284977));
#69278=CARTESIAN_POINT('Ctrl Pts',(86.7412012842004,60.4638556810233,12.089492822161));
#69279=CARTESIAN_POINT('Ctrl Pts',(86.7410365108009,60.4626336662859,12.0772666904037));
#69280=CARTESIAN_POINT('Ctrl Pts',(86.7409980955029,60.4620479267567,12.0714186239221));
#69281=CARTESIAN_POINT('Ctrl Pts',(86.7410000725785,60.461460928294,12.0655706407219));
#69282=CARTESIAN_POINT('Ctrl Pts',(86.7410000723177,60.461461005802,12.0655714128966));
#69283=CARTESIAN_POINT('Ctrl Pts',(86.7410035807468,60.4604174682608,12.0551751485843));
#69284=CARTESIAN_POINT('Ctrl Pts',(86.7411347450475,60.4593700001011,12.0447796619893));
#69285=CARTESIAN_POINT('Ctrl Pts',(86.7418258923645,60.4565618163828,12.017022315309));
#69286=CARTESIAN_POINT('Ctrl Pts',(86.7426144618169,60.4547943684841,11.9996691485679));
#69287=CARTESIAN_POINT('Ctrl Pts',(86.7511911621361,60.4414687211118,11.8697555220417));
#69288=CARTESIAN_POINT('Ctrl Pts',(86.7735938023613,60.4294794896274,11.7586792191251));
#69289=CARTESIAN_POINT('Ctrl Pts',(86.8183459995588,60.4151066597492,11.6288758128013));
#69290=CARTESIAN_POINT('Ctrl Pts',(86.8270075634458,60.412554435905,11.6059312774439));
#69291=CARTESIAN_POINT('Ctrl Pts',(86.8406456191914,60.4088572623326,11.572745910137));
#69292=CARTESIAN_POINT('Ctrl Pts',(86.8451034389896,60.4076925848355,11.5622994822151));
#69293=CARTESIAN_POINT('Ctrl Pts',(86.8534249291597,60.405596820135,11.5435015922258));
#69294=CARTESIAN_POINT('Ctrl Pts',(86.8572403075064,60.4046634579642,11.535129751527));
#69295=CARTESIAN_POINT('Ctrl Pts',(86.8634687010888,60.4031834317717,11.5218476008105));
#69296=CARTESIAN_POINT('Ctrl Pts',(86.8658229229311,60.4026334552944,11.5169104063442));
#69297=CARTESIAN_POINT('Ctrl Pts',(86.8704123063253,60.4015794416878,11.5074436264952));
#69298=CARTESIAN_POINT('Ctrl Pts',(86.872642630001,60.4010751666809,11.5029120765135));
#69299=CARTESIAN_POINT('Ctrl Pts',(86.8782274057073,60.3998315914154,11.4917337937369));
#69300=CARTESIAN_POINT('Ctrl Pts',(86.8816134170237,60.3990942195876,11.4851029504363));
#69301=CARTESIAN_POINT('Ctrl Pts',(86.8938590972146,60.3964840240597,11.4616340557894));
#69302=CARTESIAN_POINT('Ctrl Pts',(86.903039280859,60.3946293413746,11.4449644339018));
#69303=CARTESIAN_POINT('Ctrl Pts',(86.9517207621961,60.3852583232002,11.3610857758765));
#69304=CARTESIAN_POINT('Ctrl Pts',(86.9969802688381,60.3780078841744,11.2974011283249));
#69305=CARTESIAN_POINT('Ctrl Pts',(87.0564013825561,60.3694627320686,11.2282556696287));
#69306=CARTESIAN_POINT('Ctrl Pts',(87.0651560968994,60.3682252131986,11.218383702993));
#69307=CARTESIAN_POINT('Ctrl Pts',(87.1022505248767,60.3630621687693,11.1778458292569));
#69308=CARTESIAN_POINT('Ctrl Pts',(87.1319375668493,60.3591192240722,11.1484532035725));
#69309=CARTESIAN_POINT('Ctrl Pts',(87.184065838396,60.3524164661497,11.1016974168239));
#69310=CARTESIAN_POINT('Ctrl Pts',(87.2057386177599,60.3496876729087,11.0835268911102));
#69311=CARTESIAN_POINT('Ctrl Pts',(87.2353850712284,60.3460149119566,11.0603114216465));
#69312=CARTESIAN_POINT('Ctrl Pts',(87.2428359185309,60.3450967167567,11.0546088951904));
#69313=CARTESIAN_POINT('Ctrl Pts',(87.2508293253045,60.3441164270506,11.0486303989867));
#69314=CARTESIAN_POINT('Ctrl Pts',(87.2513098777843,60.3440575115723,11.0482715106976));
#69315=CARTESIAN_POINT('Ctrl Pts',(87.2522663812217,60.3439402807316,11.0475582255901));
#69316=CARTESIAN_POINT('Ctrl Pts',(87.252742326716,60.3438819656568,11.0472038216451));
#69317=CARTESIAN_POINT('Ctrl Pts',(87.2537139055923,60.3437629591703,11.046481411499));
#69318=CARTESIAN_POINT('Ctrl Pts',(87.2542095591504,60.343702266734,11.0461134329164));
#69319=CARTESIAN_POINT('Ctrl Pts',(87.2552549889167,60.3435742945126,11.0453384762276));
#69320=CARTESIAN_POINT('Ctrl Pts',(87.255804825802,60.3435070116127,11.0449315807693));
#69321=CARTESIAN_POINT('Ctrl Pts',(87.2570208608039,60.3433582579121,11.0440331986613));
#69322=CARTESIAN_POINT('Ctrl Pts',(87.2576872106543,60.3432767792883,11.0435419193037));
#69323=CARTESIAN_POINT('Ctrl Pts',(87.2592921318584,60.3430806167553,11.0423610805626));
#69324=CARTESIAN_POINT('Ctrl Pts',(87.260231170386,60.3429659086248,11.0416721614296));
#69325=CARTESIAN_POINT('Ctrl Pts',(87.2621136708337,60.3427360838546,11.0402950571854));
#69326=CARTESIAN_POINT('Ctrl Pts',(87.263057136918,60.3426209670621,11.0396068797636));
#69327=CARTESIAN_POINT('Ctrl Pts',(87.2709222483913,60.3416618527035,11.0338865598796));
#69328=CARTESIAN_POINT('Ctrl Pts',(87.2778934288681,60.340815259967,11.0289233499963));
#69329=CARTESIAN_POINT('Ctrl Pts',(87.2935367570152,60.3389228130798,11.0180224474262));
#69330=CARTESIAN_POINT('Ctrl Pts',(87.3022334074025,60.3378756486871,11.012121280272));
#69331=CARTESIAN_POINT('Ctrl Pts',(87.3267690010726,60.3349340319622,10.99591354545));
#69332=CARTESIAN_POINT('Ctrl Pts',(87.3427653999889,60.3330307288329,10.9858520930195));
#69333=CARTESIAN_POINT('Ctrl Pts',(87.418702325631,60.3240562334648,10.9404214924469));
#69334=CARTESIAN_POINT('Ctrl Pts',(87.4812483949609,60.3168282414633,10.9096683593934));
#69335=CARTESIAN_POINT('Ctrl Pts',(87.6056152978249,60.3027788501164,10.8607325657639));
#69336=CARTESIAN_POINT('Ctrl Pts',(87.666937179747,60.2959913578817,10.8418155617989));
#69337=CARTESIAN_POINT('Ctrl Pts',(87.7440912572341,60.2877399980517,10.824273016366));
#69338=CARTESIAN_POINT('Ctrl Pts',(87.7588150967908,60.2861782974198,10.8211992115709));
#69339=CARTESIAN_POINT('Ctrl Pts',(87.7910878738539,60.2827874553803,10.8150579995158));
#69340=CARTESIAN_POINT('Ctrl Pts',(87.8086545999132,60.2809623517163,10.8120966209827));
#69341=CARTESIAN_POINT('Ctrl Pts',(87.8332670448773,60.2784385604387,10.808478278488));
#69342=CARTESIAN_POINT('Ctrl Pts',(87.8402635047551,60.2777248772666,10.8075092606052));
#69343=CARTESIAN_POINT('Ctrl Pts',(87.852262361929,60.2765076989983,10.8059493154246));
#69344=CARTESIAN_POINT('Ctrl Pts',(87.8572607360853,60.2760026773558,10.8053296985583));
#69345=CARTESIAN_POINT('Ctrl Pts',(87.8678673663526,60.2749354019706,10.8040788870211));
#69346=CARTESIAN_POINT('Ctrl Pts',(87.8734763180977,60.274373570172,10.8034553126008));
#69347=CARTESIAN_POINT('Ctrl Pts',(87.8890406482697,60.2728211364145,10.8018299073994));
#69348=CARTESIAN_POINT('Ctrl Pts',(87.8990043603895,60.2718347989403,10.8009082617405));
#69349=CARTESIAN_POINT('Ctrl Pts',(87.9708800065457,60.2647662168117,10.7951156341521));
#69350=CARTESIAN_POINT('Ctrl Pts',(88.0330768875784,60.2588965723373,10.7946729880727));
#69351=CARTESIAN_POINT('Ctrl Pts',(88.143081768284,60.248543272269,10.8019707624097));
#69352=CARTESIAN_POINT('Ctrl Pts',(88.1908756794449,60.2440544141098,10.8078822746404));
#69353=CARTESIAN_POINT('Ctrl Pts',(88.2762782741895,60.2358863023116,10.8234124275309));
#69354=CARTESIAN_POINT('Ctrl Pts',(88.3139984831386,60.2322257082214,10.8320681210994));
#69355=CARTESIAN_POINT('Ctrl Pts',(88.3771099069978,60.2259476711114,10.8496187638149));
#69356=CARTESIAN_POINT('Ctrl Pts',(88.4027211524813,60.2233560817217,10.8576233716813));
#69357=CARTESIAN_POINT('Ctrl Pts',(88.4391735922175,60.2195901794098,10.8702969124738));
#69358=CARTESIAN_POINT('Ctrl Pts',(88.4502347460606,60.2184370305506,10.8743157659184));
#69359=CARTESIAN_POINT('Ctrl Pts',(88.4695554479623,60.2164032963423,10.8816410909241));
#69360=CARTESIAN_POINT('Ctrl Pts',(88.4778392527569,60.2155249469263,10.8848817898675));
#69361=CARTESIAN_POINT('Ctrl Pts',(88.4950580776298,60.2136853282097,10.8918273848197));
#69362=CARTESIAN_POINT('Ctrl Pts',(88.5039861316425,60.2127235847301,10.8955478593701));
#69363=CARTESIAN_POINT('Ctrl Pts',(88.5273888837836,60.2101810279045,10.9056154465698));
#69364=CARTESIAN_POINT('Ctrl Pts',(88.5417885325414,60.2085946007076,10.9121311743097));
#69365=CARTESIAN_POINT('Ctrl Pts',(88.6193866698178,60.199920133697,10.9490035458384));
#69366=CARTESIAN_POINT('Ctrl Pts',(88.6800962160467,60.1926654590606,10.9842784650478));
#69367=CARTESIAN_POINT('Ctrl Pts',(88.7860179497301,60.1791111783608,11.0581628201464));
#69368=CARTESIAN_POINT('Ctrl Pts',(88.832044237341,60.1728589534857,11.0952915641633));
#69369=CARTESIAN_POINT('Ctrl Pts',(88.8947304013727,60.1638904419361,11.1535185163842));
#69370=CARTESIAN_POINT('Ctrl Pts',(88.9135742311848,60.1611283003945,11.1721533269596));
#69371=CARTESIAN_POINT('Ctrl Pts',(88.9437367336272,60.1566103283159,11.2039086714241));
#69372=CARTESIAN_POINT('Ctrl Pts',(88.9553942355162,60.1548384607041,11.2166950457194));
#69373=CARTESIAN_POINT('Ctrl Pts',(88.9713871659355,60.1523750259205,11.2349733591058));
#69374=CARTESIAN_POINT('Ctrl Pts',(88.9759432948644,60.1516693624717,11.2402680626605));
#69375=CARTESIAN_POINT('Ctrl Pts',(88.9837016489877,60.1504613770383,11.2494360093404));
#69376=CARTESIAN_POINT('Ctrl Pts',(88.9869249149359,60.1499575900331,11.2532910644673));
#69377=CARTESIAN_POINT('Ctrl Pts',(88.993743647671,60.1488878194823,11.2615454026442));
#69378=CARTESIAN_POINT('Ctrl Pts',(88.9973325879527,60.1483222935644,11.2659498097992));
#69379=CARTESIAN_POINT('Ctrl Pts',(89.007104646624,60.1467751317129,11.278107953104));
#69380=CARTESIAN_POINT('Ctrl Pts',(89.0132269183259,60.1457976174498,11.2859105364497));
#69381=CARTESIAN_POINT('Ctrl Pts',(89.0574941722516,60.1386613871084,11.3437088969176));
#69382=CARTESIAN_POINT('Ctrl Pts',(89.0919779055933,60.1327208098248,11.3964147368404));
#69383=CARTESIAN_POINT('Ctrl Pts',(89.1462822463006,60.1221838011303,11.4946276801337));
#69384=CARTESIAN_POINT('Ctrl Pts',(89.16761116009,60.1175837780683,11.5391388604007));
#69385=CARTESIAN_POINT('Ctrl Pts',(89.2005041785097,60.1094098795592,11.6194739592221));
#69386=CARTESIAN_POINT('Ctrl Pts',(89.2131660534888,60.105859016346,11.6547798270784));
#69387=CARTESIAN_POINT('Ctrl Pts',(89.2320060692898,60.0997475788723,11.7156670526248));
#69388=CARTESIAN_POINT('Ctrl Pts',(89.2389851802726,60.0972109851532,11.7409751273761));
#69389=CARTESIAN_POINT('Ctrl Pts',(89.2479277393318,60.0935103013973,11.777822926435));
#69390=CARTESIAN_POINT('Ctrl Pts',(89.250524086615,60.0923663414885,11.7892035502385));
#69391=CARTESIAN_POINT('Ctrl Pts',(89.254819109716,60.0903430669625,11.8093038507849));
#69392=CARTESIAN_POINT('Ctrl Pts',(89.2565838894772,60.0894659147324,11.8180087604568));
#69393=CARTESIAN_POINT('Ctrl Pts',(89.2600876186308,60.0876230875028,11.8362729515883));
#69394=CARTESIAN_POINT('Ctrl Pts',(89.261808450685,60.0866568989133,11.8458350571947));
#69395=CARTESIAN_POINT('Ctrl Pts',(89.2660742599571,60.0840890239914,11.8712053258467));
#69396=CARTESIAN_POINT('Ctrl Pts',(89.2684301742466,60.082481517482,11.8870428550306));
#69397=CARTESIAN_POINT('Ctrl Pts',(89.2803290575921,60.0731227931811,11.978939199359));
#69398=CARTESIAN_POINT('Ctrl Pts',(89.2832672337271,60.0651698650312,12.0556750447371));
#69399=CARTESIAN_POINT('Ctrl Pts',(89.2759825011512,60.0504723506936,12.1952581467968));
#69400=CARTESIAN_POINT('Ctrl Pts',(89.2679913186369,60.0437843209604,12.2579939507808));
#69401=CARTESIAN_POINT('Ctrl Pts',(89.2523839156594,60.0356434746613,12.3344930333221));
#69402=CARTESIAN_POINT('Ctrl Pts',(89.2491443787244,60.0340946241693,12.3490566743505));
#69403=CARTESIAN_POINT('Ctrl Pts',(89.2414992647507,60.0307270969404,12.3807780454337));
#69404=CARTESIAN_POINT('Ctrl Pts',(89.2369896492882,60.0289124659539,12.3979083451577));
#69405=CARTESIAN_POINT('Ctrl Pts',(89.2301863727758,60.0264005306688,12.4217165405199));
#69406=CARTESIAN_POINT('Ctrl Pts',(89.2281935443151,60.0256884096909,12.4284769688235));
#69407=CARTESIAN_POINT('Ctrl Pts',(89.2246809140559,60.0244730269173,12.4400374059579));
#69408=CARTESIAN_POINT('Ctrl Pts',(89.2231886980304,60.0239682505586,12.4448454926776));
#69409=CARTESIAN_POINT('Ctrl Pts',(89.219960934189,60.0229005114568,12.4550313449205));
#69410=CARTESIAN_POINT('Ctrl Pts',(89.2182180376411,60.0223379774899,12.4604065692954));
#69411=CARTESIAN_POINT('Ctrl Pts',(89.2132791408332,60.0207815236983,12.4752989762207));
#69412=CARTESIAN_POINT('Ctrl Pts',(89.2100059659657,60.0197919043522,12.4847905218853));
#69413=CARTESIAN_POINT('Ctrl Pts',(89.1853562213914,60.0126264878535,12.5536106804058));
#69414=CARTESIAN_POINT('Ctrl Pts',(89.159695304005,60.0066699312221,12.6113246708353));
#69415=CARTESIAN_POINT('Ctrl Pts',(89.1064504115018,59.9961046686516,12.7104635749966));
#69416=CARTESIAN_POINT('Ctrl Pts',(89.08053128416,59.99149256359,12.7526204619303));
#69417=CARTESIAN_POINT('Ctrl Pts',(89.0308598552331,59.9833230716655,12.8237451421177));
#69418=CARTESIAN_POINT('Ctrl Pts',(89.0081635509789,59.9797893012435,12.8533729973936));
#69419=CARTESIAN_POINT('Ctrl Pts',(88.9673921916165,59.97370389382,12.9020013105836));
#69420=CARTESIAN_POINT('Ctrl Pts',(88.9499725673572,59.971175952334,12.9215200236929));
#69421=CARTESIAN_POINT('Ctrl Pts',(88.923936967622,59.9674855406958,12.9489394073195));
#69422=CARTESIAN_POINT('Ctrl Pts',(88.91579406881,59.9663430403737,12.9572819838977));
#69423=CARTESIAN_POINT('Ctrl Pts',(88.9012483083111,59.9643214218385,12.9717796664334));
#69424=CARTESIAN_POINT('Ctrl Pts',(88.8948934384974,59.9634444543544,12.9779820359312));
#69425=CARTESIAN_POINT('Ctrl Pts',(88.8814453254431,59.9616010900584,12.9908348337416));
#69426=CARTESIAN_POINT('Ctrl Pts',(88.8743397418646,59.9606341732648,12.9974714224986));
#69427=CARTESIAN_POINT('Ctrl Pts',(88.8553078899832,59.9580621497967,13.0148422603398));
#69428=CARTESIAN_POINT('Ctrl Pts',(88.8432536697442,59.9564511888635,13.0254327577625));
#69429=CARTESIAN_POINT('Ctrl Pts',(88.7747344669429,59.9473883160021,13.083368858269));
#69430=CARTESIAN_POINT('Ctrl Pts',(88.7144457707105,59.9397513181878,13.1259476384312));
#69431=CARTESIAN_POINT('Ctrl Pts',(88.5943043129406,59.9251372769315,13.1960162677878));
#69432=CARTESIAN_POINT('Ctrl Pts',(88.5353238618296,59.9182053643943,13.2245618378079));
#69433=CARTESIAN_POINT('Ctrl Pts',(88.4602416383834,59.9097938564587,13.2539871106655));
#69434=CARTESIAN_POINT('Ctrl Pts',(88.445978479973,59.9082138332476,13.2592833685066));
#69435=CARTESIAN_POINT('Ctrl Pts',(88.4146823637691,59.9047898163276,13.2702686108586));
#69436=CARTESIAN_POINT('Ctrl Pts',(88.3976161507287,59.9029498475891,13.2758555308192));
#69437=CARTESIAN_POINT('Ctrl Pts',(88.3736577803236,59.9004092422257,13.283139893964));
#69438=CARTESIAN_POINT('Ctrl Pts',(88.3668624355003,59.8996933544845,13.2851440122975));
#69439=CARTESIAN_POINT('Ctrl Pts',(88.3552047631862,59.898473638634,13.2884763718148));
#69440=CARTESIAN_POINT('Ctrl Pts',(88.3503507650248,59.897968267069,13.2898326935102));
#69441=CARTESIAN_POINT('Ctrl Pts',(88.3400542305945,59.8969016283688,13.2926438139266));
#69442=CARTESIAN_POINT('Ctrl Pts',(88.3346099184957,59.8963407736305,13.2940913476253));
#69443=CARTESIAN_POINT('Ctrl Pts',(88.3195151938453,59.8947939288,13.2979973795316));
#69444=CARTESIAN_POINT('Ctrl Pts',(88.3098448673158,59.8938121533718,13.3003787652032));
#69445=CARTESIAN_POINT('Ctrl Pts',(88.2417261463093,59.8869539501636,13.3163059729705));
#69446=CARTESIAN_POINT('Ctrl Pts',(88.1823988697835,59.8812757216819,13.3258114299898));
#69447=CARTESIAN_POINT('Ctrl Pts',(88.0201373592412,59.86596941425,13.3401267949362));
#69448=CARTESIAN_POINT('Ctrl Pts',(87.916959183455,59.8564458532353,13.3366830576952));
#69449=CARTESIAN_POINT('Ctrl Pts',(87.7975017999039,59.8447555443272,13.3180559818069));
#69450=CARTESIAN_POINT('Ctrl Pts',(87.7797335304784,59.84300021778,13.314896074688));
#69451=CARTESIAN_POINT('Ctrl Pts',(87.7520956316299,59.840239960759,13.3093709676742));
#69452=CARTESIAN_POINT('Ctrl Pts',(87.7421761491564,59.839243216483,13.3072640966704));
#69453=CARTESIAN_POINT('Ctrl Pts',(87.7236923906209,59.8373738231152,13.3031062508994));
#69454=CARTESIAN_POINT('Ctrl Pts',(87.7151220824073,59.8365021588852,13.30108452601));
#69455=CARTESIAN_POINT('Ctrl Pts',(87.6959461452258,59.8345403378165,13.2963499096497));
#69456=CARTESIAN_POINT('Ctrl Pts',(87.685353339423,59.8334486897486,13.2935887197072));
#69457=CARTESIAN_POINT('Ctrl Pts',(87.6581885350384,59.8306277992675,13.2861314411078));
#69458=CARTESIAN_POINT('Ctrl Pts',(87.6416746636329,59.8288922492665,13.2812347035655));
#69459=CARTESIAN_POINT('Ctrl Pts',(87.5425887613669,59.818346943232,13.249647407893));
#69460=CARTESIAN_POINT('Ctrl Pts',(87.4628497427745,59.8092792674951,13.2148927773552));
#69461=CARTESIAN_POINT('Ctrl Pts',(87.3426482152655,59.7947334783239,13.1471256126053));
#69462=CARTESIAN_POINT('Ctrl Pts',(87.2995650812477,59.7893228471679,13.1192747533207));
#69463=CARTESIAN_POINT('Ctrl Pts',(87.2438584374867,59.7821274010227,13.0782818073894));
#69464=CARTESIAN_POINT('Ctrl Pts',(87.2296612000493,59.7802750336801,13.0673642733483));
#69465=CARTESIAN_POINT('Ctrl Pts',(87.2055470978375,59.777101726245,13.0479954994836));
#69466=CARTESIAN_POINT('Ctrl Pts',(87.1955208469836,59.7757739068447,13.0396854405763));
#69467=CARTESIAN_POINT('Ctrl Pts',(87.1839596089517,59.7742344080539,13.0297992449294));
#69468=CARTESIAN_POINT('Ctrl Pts',(87.1822993815485,59.7740131259758,13.0283721100135));
#69469=CARTESIAN_POINT('Ctrl Pts',(87.1806428354195,59.7737921350435,13.0269406741468));
#69470=CARTESIAN_POINT('Origin',(88.011,66.41344859951,12.066));
#69471=CARTESIAN_POINT('',(87.1806428565926,58.8108193550848,13.0269406924427));
#69472=CARTESIAN_POINT('',(87.1806427698474,58.9814779498304,13.0269406174855));
#69473=CARTESIAN_POINT('',(87.1806428354228,66.41344859951,13.0269406741497));
#69474=CARTESIAN_POINT('Ctrl Pts',(87.1806428565926,58.8108193550848,13.0269406924427));
#69475=CARTESIAN_POINT('Ctrl Pts',(87.20042835637,58.8133182957622,13.0440375135111));
#69476=CARTESIAN_POINT('Ctrl Pts',(87.2207392038508,58.8158360863611,13.0605209604405));
#69477=CARTESIAN_POINT('Ctrl Pts',(87.2527546337551,58.8197477207029,13.0849025608701));
#69478=CARTESIAN_POINT('Ctrl Pts',(87.2641030172102,58.8211237165168,13.0932503701278));
#69479=CARTESIAN_POINT('Ctrl Pts',(87.2780236979588,58.8228003901362,13.1031377298773));
#69480=CARTESIAN_POINT('Ctrl Pts',(87.2804660979789,58.8230941523717,13.1048595418577));
#69481=CARTESIAN_POINT('Ctrl Pts',(87.2836168211224,58.8234725926762,13.107064093018));
#69482=CARTESIAN_POINT('Ctrl Pts',(87.2843196109945,58.8235569733901,13.1075547738411));
#69483=CARTESIAN_POINT('Ctrl Pts',(87.2920511895596,58.8244849088787,13.1129412498741));
#69484=CARTESIAN_POINT('Ctrl Pts',(87.2991286210109,58.8253310756176,13.1177663730261));
#69485=CARTESIAN_POINT('Ctrl Pts',(87.3141869378347,58.8271250357397,13.1278109468503));
#69486=CARTESIAN_POINT('Ctrl Pts',(87.3221788350464,58.828073422718,13.1330128023858));
#69487=CARTESIAN_POINT('Ctrl Pts',(87.3432463527802,58.8305644699172,13.1463901453943));
#69488=CARTESIAN_POINT('Ctrl Pts',(87.3564131430209,58.8321124069524,13.1544180228542));
#69489=CARTESIAN_POINT('Ctrl Pts',(87.4296178306994,58.8406746803733,13.1972426789486));
#69490=CARTESIAN_POINT('Ctrl Pts',(87.49227059893,58.8478524819101,13.2273057100564));
#69491=CARTESIAN_POINT('Ctrl Pts',(87.6217876555552,58.8624035273499,13.2768750985825));
#69492=CARTESIAN_POINT('Ctrl Pts',(87.6884439007816,58.8697525513365,13.296309898838));
#69493=CARTESIAN_POINT('Ctrl Pts',(87.7717278820269,58.8786246089714,13.3133552530622));
#69494=CARTESIAN_POINT('Ctrl Pts',(87.7871601715485,58.8802554192932,13.3162168051109));
#69495=CARTESIAN_POINT('Ctrl Pts',(87.8114252777765,58.8827958521998,13.3202524480686));
#69496=CARTESIAN_POINT('Ctrl Pts',(87.8202236684018,58.8837121261571,13.3216208334788));
#69497=CARTESIAN_POINT('Ctrl Pts',(87.841116556915,58.8858754362119,13.3246455468171));
#69498=CARTESIAN_POINT('Ctrl Pts',(87.8532224412059,58.8871190257414,13.3262203293242));
#69499=CARTESIAN_POINT('Ctrl Pts',(87.8714056624524,58.8889704627371,13.3283195243027));
#69500=CARTESIAN_POINT('Ctrl Pts',(87.8774665695662,58.8895848592042,13.3289750548276));
#69501=CARTESIAN_POINT('Ctrl Pts',(87.8879766019236,58.8906452875258,13.3300352832618));
#69502=CARTESIAN_POINT('Ctrl Pts',(87.892423339008,58.8910923895879,13.3304601739987));
#69503=CARTESIAN_POINT('Ctrl Pts',(87.9029453796193,58.8921466909904,13.3314095697335));
#69504=CARTESIAN_POINT('Ctrl Pts',(87.909022361407,58.8927527612634,13.3319137992205));
#69505=CARTESIAN_POINT('Ctrl Pts',(87.927282728033,58.8945660621896,13.3332965775776));
#69506=CARTESIAN_POINT('Ctrl Pts',(87.9394759827535,58.8957664096804,13.3340431982068));
#69507=CARTESIAN_POINT('Ctrl Pts',(88.0293939076067,58.9045545341321,13.338247809032));
#69508=CARTESIAN_POINT('Ctrl Pts',(88.1072944280662,58.9118233216788,13.334733626028));
#69509=CARTESIAN_POINT('Ctrl Pts',(88.2408111521557,58.9244485726821,13.3163319226117));
#69510=CARTESIAN_POINT('Ctrl Pts',(88.2966345062918,58.9297790612417,13.3047716316912));
#69511=CARTESIAN_POINT('Ctrl Pts',(88.3847479776103,58.938491664867,13.2802504559741));
#69512=CARTESIAN_POINT('Ctrl Pts',(88.4176106472612,58.9418099046252,13.2696440607536));
#69513=CARTESIAN_POINT('Ctrl Pts',(88.4620957264268,58.9464267017707,13.2532568700053));
#69514=CARTESIAN_POINT('Ctrl Pts',(88.474124855026,58.9476879396393,13.2486164081792));
#69515=CARTESIAN_POINT('Ctrl Pts',(88.4945041336013,58.9498481266325,13.240396121808));
#69516=CARTESIAN_POINT('Ctrl Pts',(88.5028905644028,58.9507439484894,13.2369082628568));
#69517=CARTESIAN_POINT('Ctrl Pts',(88.5187868651132,58.9524555884808,13.2300961898133));
#69518=CARTESIAN_POINT('Ctrl Pts',(88.5263033532051,58.9532708071425,13.2267884758215));
#69519=CARTESIAN_POINT('Ctrl Pts',(88.5457367153453,58.9553942618235,13.2180106657623));
#69520=CARTESIAN_POINT('Ctrl Pts',(88.5576015170478,58.9567062640746,13.212428662046));
#69521=CARTESIAN_POINT('Ctrl Pts',(88.5996908155426,58.9614184437597,13.1918251361288));
#69522=CARTESIAN_POINT('Ctrl Pts',(88.629396994961,58.9648530345703,13.1757854436728));
#69523=CARTESIAN_POINT('Ctrl Pts',(88.7326226601733,58.9771992434842,13.1146176228813));
#69524=CARTESIAN_POINT('Ctrl Pts',(88.8021374202715,58.9863069869873,13.0632136702568));
#69525=CARTESIAN_POINT('Ctrl Pts',(88.9019303280797,59.000514619764,12.9723760070195));
#69526=CARTESIAN_POINT('Ctrl Pts',(88.936051838383,59.0056190514468,12.9375243571157));
#69527=CARTESIAN_POINT('Ctrl Pts',(88.976146442892,59.0118702069012,12.8915559221556));
#69528=CARTESIAN_POINT('Ctrl Pts',(88.9840696552696,59.013119037286,12.8822020111672));
#69529=CARTESIAN_POINT('Ctrl Pts',(88.9957353056992,59.0149766732382,12.8680184907107));
#69530=CARTESIAN_POINT('Ctrl Pts',(88.9995799937007,59.0155920901654,12.8632746599897));
#69531=CARTESIAN_POINT('Ctrl Pts',(89.0061781467855,59.0166535780965,12.8550123022171));
#69532=CARTESIAN_POINT('Ctrl Pts',(89.00894739034,59.0171007270134,12.8515068207103));
#69533=CARTESIAN_POINT('Ctrl Pts',(89.0154467524411,59.0181541200805,12.8431896700297));
#69534=CARTESIAN_POINT('Ctrl Pts',(89.0191608609133,59.0187592430454,12.838365681435));
#69535=CARTESIAN_POINT('Ctrl Pts',(89.0301921724978,59.0205667439344,12.8238227401848));
#69536=CARTESIAN_POINT('Ctrl Pts',(89.037404924874,59.0217623033926,12.8140247055767));
#69537=CARTESIAN_POINT('Ctrl Pts',(89.090239810529,59.0306381076001,12.7400485060891));
#69538=CARTESIAN_POINT('Ctrl Pts',(89.1299546589741,59.0379909803779,12.6718426987577));
#69539=CARTESIAN_POINT('Ctrl Pts',(89.1868169011372,59.0506497537866,12.5492511874));
#69540=CARTESIAN_POINT('Ctrl Pts',(89.2071018933188,59.0559273217316,12.4966001691001));
#69541=CARTESIAN_POINT('Ctrl Pts',(89.2340006019402,59.0645654925653,12.4100154148328));
#69542=CARTESIAN_POINT('Ctrl Pts',(89.2428462254894,59.0678637077985,12.3768560527067));
#69543=CARTESIAN_POINT('Ctrl Pts',(89.2531480468877,59.0724573103752,12.3308277667658));
#69544=CARTESIAN_POINT('Ctrl Pts',(89.2557669168646,59.0737158869787,12.3182316589206));
#69545=CARTESIAN_POINT('Ctrl Pts',(89.2599064864946,59.0758729107632,12.2966837523067));
#69546=CARTESIAN_POINT('Ctrl Pts',(89.2615234095638,59.0767682533639,12.2877512051467));
#69547=CARTESIAN_POINT('Ctrl Pts',(89.2644212435786,59.0784799146793,12.2707015047651));
#69548=CARTESIAN_POINT('Ctrl Pts',(89.2657194051358,59.0792956402615,12.2625877060577));
#69549=CARTESIAN_POINT('Ctrl Pts',(89.2685771599844,59.0812134016638,12.2435432165187));
#69550=CARTESIAN_POINT('Ctrl Pts',(89.2700730876087,59.0823173810698,12.2326038633817));
#69551=CARTESIAN_POINT('Ctrl Pts',(89.2748242710187,59.0862098080011,12.1941288388923));
#69552=CARTESIAN_POINT('Ctrl Pts',(89.2773199658707,59.0890213908358,12.166509835723));
#69553=CARTESIAN_POINT('Ctrl Pts',(89.2841856217554,59.1012771224713,12.0469909280814));
#69554=CARTESIAN_POINT('Ctrl Pts',(89.2794655964512,59.1109784350131,11.9548624127588));
#69555=CARTESIAN_POINT('Ctrl Pts',(89.2567821845668,59.1260050797377,11.8140122977366));
#69556=CARTESIAN_POINT('Ctrl Pts',(89.2457281555832,59.1313220014191,11.7644725044365));
#69557=CARTESIAN_POINT('Ctrl Pts',(89.2282980038939,59.1378006255098,11.7037276722194));
#69558=CARTESIAN_POINT('Ctrl Pts',(89.2246799980459,59.1390721698871,11.6917853899793));
#69559=CARTESIAN_POINT('Ctrl Pts',(89.2190170220599,59.1409566416904,11.6740399503544));
#69560=CARTESIAN_POINT('Ctrl Pts',(89.2171051321596,59.1415764536782,11.6681957490556));
#69561=CARTESIAN_POINT('Ctrl Pts',(89.2137304100429,59.1426425369518,11.6581280423667));
#69562=CARTESIAN_POINT('Ctrl Pts',(89.2122876642428,59.143089919284,11.6538981639411));
#69563=CARTESIAN_POINT('Ctrl Pts',(89.2088401792962,59.1441395514509,11.6439627111359));
#69564=CARTESIAN_POINT('Ctrl Pts',(89.2068169742698,59.1447407131677,11.6382637051677));
#69565=CARTESIAN_POINT('Ctrl Pts',(89.2007965305368,59.1464878362064,11.6216818467075));
#69566=CARTESIAN_POINT('Ctrl Pts',(89.196690714073,59.1476277754067,11.6108385223394));
#69567=CARTESIAN_POINT('Ctrl Pts',(89.161560846331,59.1569836003768,11.521764767786));
#69568=CARTESIAN_POINT('Ctrl Pts',(89.1229732973776,59.1648200580543,11.4467234370874));
#69569=CARTESIAN_POINT('Ctrl Pts',(89.036087144621,59.1798035551961,11.3124531627067));
#69570=CARTESIAN_POINT('Ctrl Pts',(88.9893407595759,59.1869118510022,11.2526839429608));
#69571=CARTESIAN_POINT('Ctrl Pts',(88.9252419498696,59.1959748567709,11.184305158124));
#69572=CARTESIAN_POINT('Ctrl Pts',(88.9126518999797,59.1977261352381,11.17143423319));
#69573=CARTESIAN_POINT('Ctrl Pts',(88.8925549813114,59.2004815879532,11.1517442917592));
#69574=CARTESIAN_POINT('Ctrl Pts',(88.8852323409658,59.201477625847,11.144739730361));
#69575=CARTESIAN_POINT('Ctrl Pts',(88.8713893423093,59.2033465992572,11.131811706739));
#69576=CARTESIAN_POINT('Ctrl Pts',(88.8648895949125,59.2042185572042,11.1258669576052));
#69577=CARTESIAN_POINT('Ctrl Pts',(88.8501630272104,59.2061822418571,11.1126765573942));
#69578=CARTESIAN_POINT('Ctrl Pts',(88.8419032935047,59.207275470377,11.1054689646174));
#69579=CARTESIAN_POINT('Ctrl Pts',(88.8203908190485,59.2101029595542,11.0871819011128));
#69580=CARTESIAN_POINT('Ctrl Pts',(88.8070040030946,59.2118435763466,11.076264721991));
#69581=CARTESIAN_POINT('Ctrl Pts',(88.7262081480871,59.2222448987157,11.0130738036725));
#69582=CARTESIAN_POINT('Ctrl Pts',(88.6539092432021,59.2311538713852,10.9674385199425));
#69583=CARTESIAN_POINT('Ctrl Pts',(88.5308236030654,59.2456499173512,10.9060795073854));
#69584=CARTESIAN_POINT('Ctrl Pts',(88.4826464475312,59.2511698430702,10.8856685180178));
#69585=CARTESIAN_POINT('Ctrl Pts',(88.4081413378865,59.2593906019846,10.8593960815787));
#69586=CARTESIAN_POINT('Ctrl Pts',(88.3826595355958,59.2621483006796,10.851305065599));
#69587=CARTESIAN_POINT('Ctrl Pts',(88.3490770164703,59.2656988046165,10.841797938812));
#69588=CARTESIAN_POINT('Ctrl Pts',(88.3411938796637,59.2665262908386,10.8396481865353));
#69589=CARTESIAN_POINT('Ctrl Pts',(88.3282149127199,59.2678783704152,10.836243019787));
#69590=CARTESIAN_POINT('Ctrl Pts',(88.3231312718628,59.2684053742483,10.8349428915374));
#69591=CARTESIAN_POINT('Ctrl Pts',(88.3135282096159,59.2693958546461,10.83255024509));
#69592=CARTESIAN_POINT('Ctrl Pts',(88.3090106071136,59.269859718943,10.8314509745845));
#69593=CARTESIAN_POINT('Ctrl Pts',(88.2969446227447,59.2710933422148,10.8285850459517));
#69594=CARTESIAN_POINT('Ctrl Pts',(88.289385717149,59.2718606427278,10.8268625986448));
#69595=CARTESIAN_POINT('Ctrl Pts',(88.2611205236775,59.2747110025524,10.8206935239507));
#69596=CARTESIAN_POINT('Ctrl Pts',(88.2403180102299,59.2767712421674,10.8166954207947));
#69597=CARTESIAN_POINT('Ctrl Pts',(88.144290196095,59.2861533146342,10.800719429957));
#69598=CARTESIAN_POINT('Ctrl Pts',(88.0681746429535,59.2932369390329,10.7950021774295));
#69599=CARTESIAN_POINT('Ctrl Pts',(87.9426409780847,59.3050057424609,10.7968807936223));
#69600=CARTESIAN_POINT('Ctrl Pts',(87.893374824232,59.3096451917788,10.8004961095204));
#69601=CARTESIAN_POINT('Ctrl Pts',(87.8231179570695,59.3164107584551,10.8097901261253));
#69602=CARTESIAN_POINT('Ctrl Pts',(87.8018649828742,59.318476958615,10.8131531060513));
#69603=CARTESIAN_POINT('Ctrl Pts',(87.7635949953298,59.3222427143637,10.8202096448806));
#69604=CARTESIAN_POINT('Ctrl Pts',(87.7465487434599,59.3239364586888,10.8237164944718));
#69605=CARTESIAN_POINT('Ctrl Pts',(87.7198209668696,59.3266217440068,10.829790088454));
#69606=CARTESIAN_POINT('Ctrl Pts',(87.7100879642262,59.3276058298153,10.832123139344));
#69607=CARTESIAN_POINT('Ctrl Pts',(87.6918286584813,59.3294644461623,10.8367288730171));
#69608=CARTESIAN_POINT('Ctrl Pts',(87.683296425485,59.3303381010539,10.8389758738516));
#69609=CARTESIAN_POINT('Ctrl Pts',(87.6640411194625,59.3323219442653,10.8442619969252));
#69610=CARTESIAN_POINT('Ctrl Pts',(87.6533334280845,59.3334337719267,10.847353695317));
#69611=CARTESIAN_POINT('Ctrl Pts',(87.6204610892129,59.3368749005233,10.8573156705795));
#69612=CARTESIAN_POINT('Ctrl Pts',(87.5984445170747,59.3392190550098,10.864652322754));
#69613=CARTESIAN_POINT('Ctrl Pts',(87.4850780319608,59.3515077337974,10.9059134233345));
#69614=CARTESIAN_POINT('Ctrl Pts',(87.3976715855024,59.361767224919,10.9496601802298));
#69615=CARTESIAN_POINT('Ctrl Pts',(87.2834896249894,59.3761395652548,11.0242943647909));
#69616=CARTESIAN_POINT('Ctrl Pts',(87.251832404272,59.3802381198795,11.0471344355979));
#69617=CARTESIAN_POINT('Ctrl Pts',(87.2037183856132,59.386608476093,11.0853375000817));
#69618=CARTESIAN_POINT('Ctrl Pts',(87.1865323817673,59.3889143995621,11.099741286753));
#69619=CARTESIAN_POINT('Ctrl Pts',(87.1639740662499,59.3919742167761,11.119688103195));
#69620=CARTESIAN_POINT('Ctrl Pts',(87.1582591960133,59.3927523402118,11.1248346210421));
#69621=CARTESIAN_POINT('Ctrl Pts',(87.1487970147668,59.3940451945232,11.1335127257806));
#69622=CARTESIAN_POINT('Ctrl Pts',(87.1450238936592,59.394561947883,11.137015666303));
#69623=CARTESIAN_POINT('Ctrl Pts',(87.1373318641946,59.3956177661504,11.1442444877149));
#69624=CARTESIAN_POINT('Ctrl Pts',(87.1334152742032,59.3961566506239,11.1479726098554));
#69625=CARTESIAN_POINT('Ctrl Pts',(87.1231090258598,59.3975785375933,11.1579091539092));
#69626=CARTESIAN_POINT('Ctrl Pts',(87.1167604782221,59.3984583751657,11.1641601799838));
#69627=CARTESIAN_POINT('Ctrl Pts',(87.0881157300684,59.4024497217391,11.1929648585689));
#69628=CARTESIAN_POINT('Ctrl Pts',(87.0666005671462,59.4055080814184,11.2162847546263));
#69629=CARTESIAN_POINT('Ctrl Pts',(87.001638542249,59.4150398291157,11.2922161011766));
#69630=CARTESIAN_POINT('Ctrl Pts',(86.9615420501439,59.4213830409135,11.3475351957514));
#69631=CARTESIAN_POINT('Ctrl Pts',(86.8929888236457,59.4337545119134,11.460192029403));
#69632=CARTESIAN_POINT('Ctrl Pts',(86.8640377282759,59.4397578093198,11.5169755367276));
#69633=CARTESIAN_POINT('Ctrl Pts',(86.8322438536021,59.4477144488283,11.5929418828067));
#69634=CARTESIAN_POINT('Ctrl Pts',(86.8254033875868,59.4495331718521,11.6103569144862));
#69635=CARTESIAN_POINT('Ctrl Pts',(86.8154051157657,59.4523707714907,11.6375627134683));
#69636=CARTESIAN_POINT('Ctrl Pts',(86.8119771344629,59.4533806799752,11.6472521184742));
#69637=CARTESIAN_POINT('Ctrl Pts',(86.8058339135177,59.455262312639,11.6653104693713));
#69638=CARTESIAN_POINT('Ctrl Pts',(86.803087287703,59.4561329437163,11.6736681690772));
#69639=CARTESIAN_POINT('Ctrl Pts',(86.7971702585409,59.458076390183,11.6923243891));
#69640=CARTESIAN_POINT('Ctrl Pts',(86.7940436972816,59.4591505661996,11.7026359369477));
#69641=CARTESIAN_POINT('Ctrl Pts',(86.7864256821505,59.4618939360299,11.7289623611367));
#69642=CARTESIAN_POINT('Ctrl Pts',(86.7821171183554,59.4635688562637,11.7450273751129));
#69643=CARTESIAN_POINT('Ctrl Pts',(86.7533768577916,59.4757006435426,11.8612669109769));
#69644=CARTESIAN_POINT('Ctrl Pts',(86.7409162936534,59.4865367345118,11.9639798325527));
#69645=CARTESIAN_POINT('Ctrl Pts',(86.74104864501,59.5036229477905,12.1261075805094));
#69646=CARTESIAN_POINT('Ctrl Pts',(86.7452181313658,59.5098257394367,12.1851125158358));
#69647=CARTESIAN_POINT('Ctrl Pts',(86.7548737243046,59.5168739471894,12.2534720238416));
#69648=CARTESIAN_POINT('Ctrl Pts',(86.7563809530928,59.5178845017504,12.2633069936988));
#69649=CARTESIAN_POINT('Ctrl Pts',(86.7589222007596,59.5194577196056,12.2786802835506));
#69650=CARTESIAN_POINT('Ctrl Pts',(86.759877689846,59.5200244169316,12.2842308134261));
#69651=CARTESIAN_POINT('Ctrl Pts',(86.7617584837041,59.521094468543,12.2947379595655));
#69652=CARTESIAN_POINT('Ctrl Pts',(86.7626763869126,59.5215981706109,12.2996954837547));
#69653=CARTESIAN_POINT('Ctrl Pts',(86.7649564113522,59.522806425434,12.3116128335686));
#69654=CARTESIAN_POINT('Ctrl Pts',(86.7663473512566,59.5235093656812,12.3185669841474));
#69655=CARTESIAN_POINT('Ctrl Pts',(86.7714737600949,59.525985557474,12.3431255119582));
#69656=CARTESIAN_POINT('Ctrl Pts',(86.7755253409287,59.5277424718368,12.3606630872153));
#69657=CARTESIAN_POINT('Ctrl Pts',(86.7836996735767,59.5309620891077,12.392904976564));
#69658=CARTESIAN_POINT('Ctrl Pts',(86.7877172404363,59.5324286298095,12.4076318202338));
#69659=CARTESIAN_POINT('Ctrl Pts',(86.8104630413104,59.540175427238,12.4854550706755));
#69660=CARTESIAN_POINT('Ctrl Pts',(86.8338108622215,59.5463051252134,12.5471017748254));
#69661=CARTESIAN_POINT('Ctrl Pts',(86.8931428388922,59.5593698738862,12.6732097604881));
#69662=CARTESIAN_POINT('Ctrl Pts',(86.9301660976612,59.5662934406023,12.7368975075675));
#69663=CARTESIAN_POINT('Ctrl Pts',(86.981612859275,59.5749595443459,12.8099849243284));
#69664=CARTESIAN_POINT('Ctrl Pts',(86.9909819323649,59.5765052960202,12.8227790570389));
#69665=CARTESIAN_POINT('Ctrl Pts',(87.0064547594228,59.5790099184621,12.8430988688454));
#69666=CARTESIAN_POINT('Ctrl Pts',(87.0124096649597,59.579962968376,12.8507363392715));
#69667=CARTESIAN_POINT('Ctrl Pts',(87.023999666922,59.5817979498255,12.8652555555867));
#69668=CARTESIAN_POINT('Ctrl Pts',(87.0296208830115,59.5826792864769,12.8721477030477));
#69669=CARTESIAN_POINT('Ctrl Pts',(87.0428342296356,59.5847317012978,12.8880055089261));
#69670=CARTESIAN_POINT('Ctrl Pts',(87.0504791555469,59.5859048749956,12.896925808437));
#69671=CARTESIAN_POINT('Ctrl Pts',(87.0758970956893,59.5897608126251,12.9257645922062));
#69672=CARTESIAN_POINT('Ctrl Pts',(87.0941730110331,59.59246413685,12.9452272714945));
#69673=CARTESIAN_POINT('Ctrl Pts',(87.1348137693455,59.5983384439217,12.9858614793107));
#69674=CARTESIAN_POINT('Ctrl Pts',(87.1573608824744,59.6015155117477,13.006822537074));
#69675=CARTESIAN_POINT('Ctrl Pts',(87.1806428411249,59.6047173123478,13.026940679077));
#69676=CARTESIAN_POINT('Ctrl Pts',(87.1806428354195,59.7737921350435,13.0269406741468));
#69677=CARTESIAN_POINT('Ctrl Pts',(87.1775687030115,59.7733820315304,13.0242842896909));
#69678=CARTESIAN_POINT('Ctrl Pts',(87.1745072481833,59.7729729306308,13.0216130936167));
#69679=CARTESIAN_POINT('Ctrl Pts',(87.1677366033509,59.7720667300509,13.015648066149));
#69680=CARTESIAN_POINT('Ctrl Pts',(87.1640338713773,59.7715701992528,13.0123471804472));
#69681=CARTESIAN_POINT('Ctrl Pts',(87.1557520415292,59.7704574349153,13.0048766044911));
#69682=CARTESIAN_POINT('Ctrl Pts',(87.1511839790451,59.7698420994443,13.0006950117345));
#69683=CARTESIAN_POINT('Ctrl Pts',(87.1373352292863,59.7679711011719,12.9878304525414));
#69684=CARTESIAN_POINT('Ctrl Pts',(87.1281536532909,59.7667229830059,12.9790410111749));
#69685=CARTESIAN_POINT('Ctrl Pts',(87.0695725790788,59.758696016311,12.9212516882754));
#69686=CARTESIAN_POINT('Ctrl Pts',(87.0241297518223,59.752167136254,12.8683913087438));
#69687=CARTESIAN_POINT('Ctrl Pts',(86.9350170653384,59.737951773346,12.7456318500562));
#69688=CARTESIAN_POINT('Ctrl Pts',(86.8933540033589,59.7302944763121,12.6746900289191));
#69689=CARTESIAN_POINT('Ctrl Pts',(86.8495629533283,59.7202723018389,12.5802462782872));
#69690=CARTESIAN_POINT('Ctrl Pts',(86.8408188455265,59.7181368831593,12.5600254818589));
#69691=CARTESIAN_POINT('Ctrl Pts',(86.8285309583209,59.714915887302,12.5294504889283));
#69692=CARTESIAN_POINT('Ctrl Pts',(86.8245875550023,59.7138436757156,12.5192602809311));
#69693=CARTESIAN_POINT('Ctrl Pts',(86.8177050436893,59.7118995292467,12.500769665071));
#69694=CARTESIAN_POINT('Ctrl Pts',(86.8147198025089,59.7110291884513,12.4924870380719));
#69695=CARTESIAN_POINT('Ctrl Pts',(86.8084770616258,59.7091486524475,12.4745850205568));
#69696=CARTESIAN_POINT('Ctrl Pts',(86.8052483833388,59.7081375738011,12.4649563383163));
#69697=CARTESIAN_POINT('Ctrl Pts',(86.7967309594642,59.7053604379232,12.4385071576622));
#69698=CARTESIAN_POINT('Ctrl Pts',(86.7916767389639,59.703586918852,12.4216143841025));
#69699=CARTESIAN_POINT('Ctrl Pts',(86.756373901532,59.6901824515533,12.2940048476749));
#69700=CARTESIAN_POINT('Ctrl Pts',(86.7409157376895,59.678069612099,12.1797740406136));
#69701=CARTESIAN_POINT('Ctrl Pts',(86.7410363465161,59.660868729895,12.0162530732113));
#69702=CARTESIAN_POINT('Ctrl Pts',(86.7438862449935,59.6557670195673,11.9674778025694));
#69703=CARTESIAN_POINT('Ctrl Pts',(86.7506721580243,59.6497842119694,11.9092529076282));
#69704=CARTESIAN_POINT('Ctrl Pts',(86.7519184841986,59.6487896291652,11.8995377573297));
#69705=CARTESIAN_POINT('Ctrl Pts',(86.7540536492045,59.6472357210878,11.8842936204428));
#69706=CARTESIAN_POINT('Ctrl Pts',(86.7548668196986,59.6466725152218,11.8787547732185));
#69707=CARTESIAN_POINT('Ctrl Pts',(86.7564835233413,59.6456049469763,11.8682275671591));
#69708=CARTESIAN_POINT('Ctrl Pts',(86.7572802040074,59.6451002669231,11.8632385626636));
#69709=CARTESIAN_POINT('Ctrl Pts',(86.759278313206,59.6438840597824,11.8511881761662));
#69710=CARTESIAN_POINT('Ctrl Pts',(86.760509749671,59.64317420222,11.844131922957));
#69711=CARTESIAN_POINT('Ctrl Pts',(86.7651321695339,59.6406435483792,11.8189070486074));
#69712=CARTESIAN_POINT('Ctrl Pts',(86.7688602124104,59.6388400565203,11.8008011043753));
#69713=CARTESIAN_POINT('Ctrl Pts',(86.7765198997636,59.6355174631427,11.7673187551984));
#69714=CARTESIAN_POINT('Ctrl Pts',(86.7803468330588,59.6339946413354,11.7519228633101));
#69715=CARTESIAN_POINT('Ctrl Pts',(86.8028102751746,59.6257271890354,11.668278576211));
#69716=CARTESIAN_POINT('Ctrl Pts',(86.8268373938344,59.6191528676266,11.6016020627902));
#69717=CARTESIAN_POINT('Ctrl Pts',(86.8844327363165,59.6061710091304,11.4758186262596));
#69718=CARTESIAN_POINT('Ctrl Pts',(86.9174258561234,59.5997896423517,11.4167227378667));
#69719=CARTESIAN_POINT('Ctrl Pts',(86.9636996266891,59.5917112425151,11.3474531604039));
#69720=CARTESIAN_POINT('Ctrl Pts',(86.972682846553,59.5901770833041,11.3345322501892));
#69721=CARTESIAN_POINT('Ctrl Pts',(86.9875628362294,59.5876867382795,11.313956353478));
#69722=CARTESIAN_POINT('Ctrl Pts',(86.9933112175547,59.5867362532257,11.306195549019));
#69723=CARTESIAN_POINT('Ctrl Pts',(87.0045257829804,59.5849032096789,11.2914105233264));
#69724=CARTESIAN_POINT('Ctrl Pts',(87.0099784208113,59.5840212230813,11.2843766926243));
#69725=CARTESIAN_POINT('Ctrl Pts',(87.0228323379905,59.5819627696884,11.2681504253961));
#69726=CARTESIAN_POINT('Ctrl Pts',(87.030288575361,59.5807841655702,11.2590028814561));
#69727=CARTESIAN_POINT('Ctrl Pts',(87.055239165879,59.5768887855074,11.2292492239817));
#69728=CARTESIAN_POINT('Ctrl Pts',(87.0732624626855,59.5741508529629,11.2090993866752));
#69729=CARTESIAN_POINT('Ctrl Pts',(87.1188993892084,59.5673893805207,11.16124280233));
#69730=CARTESIAN_POINT('Ctrl Pts',(87.1471749435473,59.5633411989541,11.1342089011216));
#69731=CARTESIAN_POINT('Ctrl Pts',(87.2125730646819,59.5542790536115,11.0772204776791));
#69732=CARTESIAN_POINT('Ctrl Pts',(87.2502285805024,59.5492537564951,11.0479642152911));
#69733=CARTESIAN_POINT('Ctrl Pts',(87.3403632700887,59.5377075891573,10.9857332504184));
#69734=CARTESIAN_POINT('Ctrl Pts',(87.393800342804,59.5312012305805,10.9543360147804));
#69735=CARTESIAN_POINT('Ctrl Pts',(87.4582878093801,59.5238600275004,10.9225363287019));
#69736=CARTESIAN_POINT('Ctrl Pts',(87.4673060571095,59.5228445478086,10.9182209043483));
#69737=CARTESIAN_POINT('Ctrl Pts',(87.4814920068698,59.5212654747772,10.9116373574472));
#69738=CARTESIAN_POINT('Ctrl Pts',(87.4866251352479,59.5206977990061,10.9092965673608));
#69739=CARTESIAN_POINT('Ctrl Pts',(87.4963708534544,59.5196272218521,10.9049305727487));
#69740=CARTESIAN_POINT('Ctrl Pts',(87.5009799484567,59.5191239630705,10.9028985760763));
#69741=CARTESIAN_POINT('Ctrl Pts',(87.5120843617653,59.5179185803153,10.8980817131152));
#69742=CARTESIAN_POINT('Ctrl Pts',(87.5185910786153,59.5172180497405,10.8953235281889));
#69743=CARTESIAN_POINT('Ctrl Pts',(87.541600773772,59.514759797852,10.8857955575515));
#69744=CARTESIAN_POINT('Ctrl Pts',(87.5582242388993,59.5130181046345,10.8793187512209));
#69745=CARTESIAN_POINT('Ctrl Pts',(87.5891348776697,59.509831792911,10.8680196385438));
#69746=CARTESIAN_POINT('Ctrl Pts',(87.6033814241371,59.5083833059317,10.8630975608054));
#69747=CARTESIAN_POINT('Ctrl Pts',(87.6788702439027,59.5007954455854,10.8385120148546));
#69748=CARTESIAN_POINT('Ctrl Pts',(87.7414580836853,59.4948008291481,10.8232668530131));
#69749=CARTESIAN_POINT('Ctrl Pts',(87.8794203547817,59.481697196394,10.8005812642215));
#69750=CARTESIAN_POINT('Ctrl Pts',(87.9548344247613,59.4745971736984,10.7950003455266));
#69751=CARTESIAN_POINT('Ctrl Pts',(88.0461250336752,59.4657444414998,10.7963870382767));
#69752=CARTESIAN_POINT('Ctrl Pts',(88.0619543923873,59.4642005431782,10.7969237859735));
#69753=CARTESIAN_POINT('Ctrl Pts',(88.0874346192412,59.4616983127024,10.7982652339914));
#69754=CARTESIAN_POINT('Ctrl Pts',(88.0970940138646,59.4607457828876,10.7988845767473));
#69755=CARTESIAN_POINT('Ctrl Pts',(88.1156127389095,59.4589114030595,10.8002846844128));
#69756=CARTESIAN_POINT('Ctrl Pts',(88.1244728400448,59.458030144622,10.801048226379));
#69757=CARTESIAN_POINT('Ctrl Pts',(88.1450221050418,59.4559773183308,10.8030367366401));
#69758=CARTESIAN_POINT('Ctrl Pts',(88.1567035038372,59.4548036502318,10.804331028232));
#69759=CARTESIAN_POINT('Ctrl Pts',(88.1948916107426,59.4509433336054,10.8090996374006));
#69760=CARTESIAN_POINT('Ctrl Pts',(88.221304558554,59.4482360558747,10.8132484825475));
#69761=CARTESIAN_POINT('Ctrl Pts',(88.2853771750694,59.4415699687114,10.8253959713326));
#69762=CARTESIAN_POINT('Ctrl Pts',(88.3228397922843,59.4375874521361,10.8342790673587));
#69763=CARTESIAN_POINT('Ctrl Pts',(88.4063179390522,59.4285216584483,10.8581256356881));
#69764=CARTESIAN_POINT('Ctrl Pts',(88.4520000035814,59.4234241038386,10.8740456358033));
#69765=CARTESIAN_POINT('Ctrl Pts',(88.5541526719112,59.4117695876333,10.9163232318382));
#69766=CARTESIAN_POINT('Ctrl Pts',(88.609827460965,59.4052270005217,10.9443139702107));
#69767=CARTESIAN_POINT('Ctrl Pts',(88.6718193091844,59.397850350359,10.9814180615258));
#69768=CARTESIAN_POINT('Ctrl Pts',(88.680345274137,59.3968338019355,10.9866589661164));
#69769=CARTESIAN_POINT('Ctrl Pts',(88.6935814950587,59.3952534427346,10.9950124403596));
#69770=CARTESIAN_POINT('Ctrl Pts',(88.6983341598425,59.3946855390946,10.9980563649833));
#69771=CARTESIAN_POINT('Ctrl Pts',(88.7072895256839,59.3936148035626,11.0038765313924));
#69772=CARTESIAN_POINT('Ctrl Pts',(88.7114960576605,59.393111612259,11.006646120843));
#69773=CARTESIAN_POINT('Ctrl Pts',(88.7215614239542,59.3919067586762,11.0133593512951));
#69774=CARTESIAN_POINT('Ctrl Pts',(88.727404064009,59.391206686065,11.0173269822442));
#69775=CARTESIAN_POINT('Ctrl Pts',(88.7478600191035,59.3887519410587,11.0314690140069));
#69776=CARTESIAN_POINT('Ctrl Pts',(88.7622932610998,59.3870132362549,11.0419025434653));
#69777=CARTESIAN_POINT('Ctrl Pts',(88.7884987538707,59.3838334695196,11.061698412505));
#69778=CARTESIAN_POINT('Ctrl Pts',(88.8003328145283,59.3823885331565,11.0709724867041));
#69779=CARTESIAN_POINT('Ctrl Pts',(88.8616875060043,59.3748315847663,11.120838414535));
#69780=CARTESIAN_POINT('Ctrl Pts',(88.9082546248101,59.3688632113717,11.1649254331858));
#69781=CARTESIAN_POINT('Ctrl Pts',(88.9980166167357,59.3563481608872,11.2637978184337));
#69782=CARTESIAN_POINT('Ctrl Pts',(89.040422579967,59.3498147227811,11.3189946510523));
#69783=CARTESIAN_POINT('Ctrl Pts',(89.087564994343,59.3414208424022,11.3920469826745));
#69784=CARTESIAN_POINT('Ctrl Pts',(89.0967281837991,59.3397255835919,11.4069104020161));
#69785=CARTESIAN_POINT('Ctrl Pts',(89.1111676166378,59.3369428867795,11.4314509077059));
#69786=CARTESIAN_POINT('Ctrl Pts',(89.1166296901801,59.3358621556153,11.4410165564696));
#69787=CARTESIAN_POINT('Ctrl Pts',(89.1262354061474,59.3339089075042,11.4583589749287));
#69788=CARTESIAN_POINT('Ctrl Pts',(89.1304239095464,59.3330380519393,11.4661102373577));
#69789=CARTESIAN_POINT('Ctrl Pts',(89.1392363104646,59.3311634455286,11.4828322075904));
#69790=CARTESIAN_POINT('Ctrl Pts',(89.1438345620471,59.3301588624505,11.4918156338765));
#69791=CARTESIAN_POINT('Ctrl Pts',(89.1562502987068,59.3273708348178,11.5168015549994));
#69792=CARTESIAN_POINT('Ctrl Pts',(89.1638385967034,59.3255796512824,11.5329143915446));
#69793=CARTESIAN_POINT('Ctrl Pts',(89.1801091563551,59.321532010175,11.5694362941811));
#69794=CARTESIAN_POINT('Ctrl Pts',(89.188600382898,59.3192698564289,11.589923408886));
#69795=CARTESIAN_POINT('Ctrl Pts',(89.2151772370692,59.3116537690743,11.6591145272864));
#69796=CARTESIAN_POINT('Ctrl Pts',(89.2308086071154,59.3062320730919,11.7086987779864));
#69797=CARTESIAN_POINT('Ctrl Pts',(89.2635481026253,59.2919834056348,11.8401619153047));
#69798=CARTESIAN_POINT('Ctrl Pts',(89.2756903839064,59.2831146054344,11.9230303097981));
#69799=CARTESIAN_POINT('Ctrl Pts',(89.2801702207618,59.273299975523,12.0185413451439));
#69800=CARTESIAN_POINT('Ctrl Pts',(89.2805636191433,59.2720692182234,12.0305933997062));
#69801=CARTESIAN_POINT('Ctrl Pts',(89.2808980580573,59.2702251665408,12.0487803525101));
#69802=CARTESIAN_POINT('Ctrl Pts',(89.280966396804,59.2696057476745,12.0549116860172));
#69803=CARTESIAN_POINT('Ctrl Pts',(89.2810099256633,59.2684833635755,12.0660649661424));
#69804=CARTESIAN_POINT('Ctrl Pts',(89.2809997423851,59.2679796322227,12.0710867029397));
#69805=CARTESIAN_POINT('Ctrl Pts',(89.2809157406367,59.2669245590828,12.0816400660853));
#69806=CARTESIAN_POINT('Ctrl Pts',(89.2808355694342,59.2663735691534,12.0871714643996));
#69807=CARTESIAN_POINT('Ctrl Pts',(89.2805197944581,59.2648828748999,12.1021868266455));
#69808=CARTESIAN_POINT('Ctrl Pts',(89.2802140604217,59.2639468987511,12.1116692846327));
#69809=CARTESIAN_POINT('Ctrl Pts',(89.277819126275,59.2585346990348,12.1667701124972));
#69810=CARTESIAN_POINT('Ctrl Pts',(89.2733766094805,59.2541721118022,12.2122602170451));
#69811=CARTESIAN_POINT('Ctrl Pts',(89.2524073825708,59.2410214654827,12.3497942815233));
#69812=CARTESIAN_POINT('Ctrl Pts',(89.2281723648696,59.232398921879,12.4403300246576));
#69813=CARTESIAN_POINT('Ctrl Pts',(89.1818046795263,59.2202430267664,12.559239471477));
#69814=CARTESIAN_POINT('Ctrl Pts',(89.1681047975308,59.2169578471152,12.5905729689641));
#69815=CARTESIAN_POINT('Ctrl Pts',(89.1474000411343,59.2123485878971,12.6331582022505));
#69816=CARTESIAN_POINT('Ctrl Pts',(89.1414572346811,59.2110606237555,12.6449126782262));
#69817=CARTESIAN_POINT('Ctrl Pts',(89.1315100541561,59.2089583917186,12.6638501513143));
#69818=CARTESIAN_POINT('Ctrl Pts',(89.1276166807497,59.2081480457571,12.6710907082465));
#69819=CARTESIAN_POINT('Ctrl Pts',(89.1192805777984,59.2064383664324,12.6862390067684));
#69820=CARTESIAN_POINT('Ctrl Pts',(89.1148229022142,59.2055385407913,12.6941379261746));
#69821=CARTESIAN_POINT('Ctrl Pts',(89.1038558267501,59.2033583100933,12.7130940954957));
#69822=CARTESIAN_POINT('Ctrl Pts',(89.0972628793226,59.2020749591309,12.7241014757712));
#69823=CARTESIAN_POINT('Ctrl Pts',(89.0725642201419,59.1973625527552,12.7639550697698));
#69824=CARTESIAN_POINT('Ctrl Pts',(89.0534689672233,59.1938980280824,12.7921664894641));
#69825=CARTESIAN_POINT('Ctrl Pts',(88.9895394103307,59.1828143381107,12.8788905984753));
#69826=CARTESIAN_POINT('Ctrl Pts',(88.9407398803989,59.1750647491252,12.9342804660689));
#69827=CARTESIAN_POINT('Ctrl Pts',(88.8435584940192,59.1609069904611,13.0269475010758));
#69828=CARTESIAN_POINT('Ctrl Pts',(88.7967490268963,59.1545248419355,13.0655869873199));
#69829=CARTESIAN_POINT('Ctrl Pts',(88.7368477457672,59.1469831778354,13.1082146060289));
#69830=CARTESIAN_POINT('Ctrl Pts',(88.72622895842,59.1456685513683,13.1155302846455));
#69831=CARTESIAN_POINT('Ctrl Pts',(88.7103180724264,59.1437333941151,13.1261382078961));
#69832=CARTESIAN_POINT('Ctrl Pts',(88.705110734582,59.1431054469085,13.1295549258966));
#69833=CARTESIAN_POINT('Ctrl Pts',(88.6957111152456,59.1419818734538,13.1356239026172));
#69834=CARTESIAN_POINT('Ctrl Pts',(88.6915282389876,59.1414853869444,13.1382900370571));
#69835=CARTESIAN_POINT('Ctrl Pts',(88.6820680105997,59.1403703359417,13.1442422586879));
#69836=CARTESIAN_POINT('Ctrl Pts',(88.6767820167762,59.1397526888371,13.1475141956512));
#69837=CARTESIAN_POINT('Ctrl Pts',(88.6605110417331,59.1378672264789,13.1574211328747));
#69838=CARTESIAN_POINT('Ctrl Pts',(88.6494487797031,59.1366071260384,13.1639289069564));
#69839=CARTESIAN_POINT('Ctrl Pts',(88.6230193045955,59.133642687993,13.178942394603));
#69840=CARTESIAN_POINT('Ctrl Pts',(88.6075701675413,59.1319459993446,13.1872994838511));
#69841=CARTESIAN_POINT('Ctrl Pts',(88.5479360131498,59.125512727448,13.2179764575562));
#69842=CARTESIAN_POINT('Ctrl Pts',(88.5026296342627,59.1208627709275,13.2380287485289));
#69843=CARTESIAN_POINT('Ctrl Pts',(88.3725590638776,59.1078441305012,13.2867225186989));
#69844=CARTESIAN_POINT('Ctrl Pts',(88.285792999167,59.0995178121364,13.3091306915422));
#69845=CARTESIAN_POINT('Ctrl Pts',(88.1804787445415,59.0892344098652,13.3247571779809));
#69846=CARTESIAN_POINT('Ctrl Pts',(88.1635081609346,59.0875727726781,13.3269258001105));
#69847=CARTESIAN_POINT('Ctrl Pts',(88.1356491520638,59.0848338771964,13.3299152198127));
#69848=CARTESIAN_POINT('Ctrl Pts',(88.1247842935386,59.0837629691797,13.3309396073695));
#69849=CARTESIAN_POINT('Ctrl Pts',(88.1051336008588,59.0818202065573,13.3325371546034));
#69850=CARTESIAN_POINT('Ctrl Pts',(88.0963523141284,59.0809499357357,13.3331592131248));
#69851=CARTESIAN_POINT('Ctrl Pts',(88.0774183424928,59.07906844936,13.3343027813302));
#69852=CARTESIAN_POINT('Ctrl Pts',(88.0672645337648,59.0780563423113,13.3347937689663));
#69853=CARTESIAN_POINT('Ctrl Pts',(88.0389510199128,59.0752246188918,13.3358223456954));
#69854=CARTESIAN_POINT('Ctrl Pts',(88.0207849372825,59.0733968551869,13.3360922078435));
#69855=CARTESIAN_POINT('Ctrl Pts',(87.9902541179674,59.0703045886684,13.3358907599685));
#69856=CARTESIAN_POINT('Ctrl Pts',(87.9778901498451,59.0690466993831,13.3356285460765));
#69857=CARTESIAN_POINT('Ctrl Pts',(87.928558390022,59.0640043542464,13.3338612783503));
#69858=CARTESIAN_POINT('Ctrl Pts',(87.8916642327907,59.0601800178747,13.3309218166989));
#69859=CARTESIAN_POINT('Ctrl Pts',(87.8050826073693,59.0510798606278,13.3202022977591));
#69860=CARTESIAN_POINT('Ctrl Pts',(87.7556238678647,59.0457817207991,13.3110733917178));
#69861=CARTESIAN_POINT('Ctrl Pts',(87.6504357810763,59.0343602010464,13.2851260876271));
#69862=CARTESIAN_POINT('Ctrl Pts',(87.5950454516706,59.0282489514472,13.2673569744814));
#69863=CARTESIAN_POINT('Ctrl Pts',(87.5290886683098,59.0209663168652,13.2410861765387));
#69864=CARTESIAN_POINT('Ctrl Pts',(87.5171895707621,59.0196524175389,13.2361356161176));
#69865=CARTESIAN_POINT('Ctrl Pts',(87.4996553280921,59.0177181155823,13.2285254389165));
#69866=CARTESIAN_POINT('Ctrl Pts',(87.4939616586705,59.0170903056412,13.2260043660288));
#69867=CARTESIAN_POINT('Ctrl Pts',(87.4837658884295,59.0159668702914,13.2213998424652));
#69868=CARTESIAN_POINT('Ctrl Pts',(87.479257239905,59.0154703857178,13.2193318016494));
#69869=CARTESIAN_POINT('Ctrl Pts',(87.4747189595692,59.0149709276236,13.2172178976095));
#69870=CARTESIAN_POINT('Ctrl Pts',(87.4746774000621,59.014966353836,13.217198536699));
#69871=CARTESIAN_POINT('Ctrl Pts',(87.4745975007062,59.0149575606398,13.217161309522));
#69872=CARTESIAN_POINT('Ctrl Pts',(87.4745591608392,59.0149533412259,13.2171434436549));
#69873=CARTESIAN_POINT('Ctrl Pts',(87.4744854462499,59.0149452287573,13.217109089156));
#69874=CARTESIAN_POINT('Ctrl Pts',(87.4744500713418,59.0149413356793,13.2170926007842));
#69875=CARTESIAN_POINT('Ctrl Pts',(87.4743603401096,59.0149314606222,13.2170507716993));
#69876=CARTESIAN_POINT('Ctrl Pts',(87.474305984671,59.0149254787623,13.2170254286968));
#69877=CARTESIAN_POINT('Ctrl Pts',(87.4741981788308,59.0149136147174,13.2169751553652));
#69878=CARTESIAN_POINT('Ctrl Pts',(87.474144728382,59.0149077325259,13.2169502251681));
#69879=CARTESIAN_POINT('Ctrl Pts',(87.4740387115215,59.0148960655027,13.2169007681118));
#69880=CARTESIAN_POINT('Ctrl Pts',(87.4739861451921,59.0148902806789,13.2168762414391));
#69881=CARTESIAN_POINT('Ctrl Pts',(87.4738818762983,59.0148788061562,13.2168275824148));
#69882=CARTESIAN_POINT('Ctrl Pts',(87.4738301737658,59.0148731164596,13.2168034502203));
#69883=CARTESIAN_POINT('Ctrl Pts',(87.473727613119,59.0148618300587,13.2167555715466));
#69884=CARTESIAN_POINT('Ctrl Pts',(87.4736767548182,59.0148562333327,13.2167318251173));
#69885=CARTESIAN_POINT('Ctrl Pts',(87.4735758629358,59.0148451307014,13.2166847091842));
#69886=CARTESIAN_POINT('Ctrl Pts',(87.4735258294574,59.0148396248064,13.2166613398602));
#69887=CARTESIAN_POINT('Ctrl Pts',(87.4734265689441,59.0148287018227,13.2166149699944));
#69888=CARTESIAN_POINT('Ctrl Pts',(87.4733773417245,59.0148232847127,13.2165919694927));
#69889=CARTESIAN_POINT('Ctrl Pts',(87.4732796753336,59.0148125372712,13.216546329054));
#69890=CARTESIAN_POINT('Ctrl Pts',(87.4732312361289,59.0148072069352,13.2165236892231));
#69891=CARTESIAN_POINT('Ctrl Pts',(87.4674760496392,59.0141738994355,13.2138333498241));
#69892=CARTESIAN_POINT('Ctrl Pts',(87.4617890066033,59.0135484914819,13.2111231263483));
#69893=CARTESIAN_POINT('Ctrl Pts',(87.4436846533991,59.0115580331591,13.202329390986));
#69894=CARTESIAN_POINT('Ctrl Pts',(87.431345719996,59.0102021865128,13.1960850233949));
#69895=CARTESIAN_POINT('Ctrl Pts',(87.4017719098353,59.0069479368493,13.1805066937269));
#69896=CARTESIAN_POINT('Ctrl Pts',(87.3846457807235,59.0050595671684,13.1709726483241));
#69897=CARTESIAN_POINT('Ctrl Pts',(87.3154370641298,58.9973820615851,13.1303178940989));
#69898=CARTESIAN_POINT('Ctrl Pts',(87.2653919453477,58.9917178198013,13.0958788629775));
#69899=CARTESIAN_POINT('Ctrl Pts',(87.2053439521476,58.9845156109244,13.0478761243235));
#69900=CARTESIAN_POINT('Ctrl Pts',(87.1928905788101,58.9829980406649,13.0375240568162));
#69901=CARTESIAN_POINT('Ctrl Pts',(87.1806427698475,58.9814779498304,13.0269406174854));
#69902=CARTESIAN_POINT('Origin',(88.011,66.41344859951,12.066));
#69903=CARTESIAN_POINT('',(87.1795113209163,58.0179748583214,13.028265366586));
#69904=CARTESIAN_POINT('',(87.1806428261678,58.1885986874538,13.0269406661524));
#69905=CARTESIAN_POINT('',(87.1806428354228,66.41344859951,13.0269406741497));
#69906=CARTESIAN_POINT('',(86.7429300722972,58.7031861779361,12.066150707506));
#69907=CARTESIAN_POINT('Ctrl Pts',(86.7430439769444,58.70325140049,12.0661441982405));
#69908=CARTESIAN_POINT('Ctrl Pts',(86.7432677167238,58.6813761345907,11.8453854404656));
#69909=CARTESIAN_POINT('Ctrl Pts',(86.9032087774569,58.6174961205304,11.200423640207));
#69910=CARTESIAN_POINT('Ctrl Pts',(87.9302701790554,58.5116113583089,10.567102535751));
#69911=CARTESIAN_POINT('Ctrl Pts',(89.2264677377329,58.3855971138258,11.1851770377356));
#69912=CARTESIAN_POINT('Ctrl Pts',(89.4102662159187,58.2595828693425,12.6093828938329));
#69913=CARTESIAN_POINT('Ctrl Pts',(88.3436856703656,58.1370421175078,13.5107340312985));
#69914=CARTESIAN_POINT('Ctrl Pts',(87.4731169939088,58.056506113834,13.2786948377731));
#69915=CARTESIAN_POINT('Ctrl Pts',(87.1795113209163,58.0179748583214,13.028265366586));
#69916=CARTESIAN_POINT('Ctrl Pts',(86.7410000268199,58.7020810211383,12.06626100308));
#69917=CARTESIAN_POINT('Ctrl Pts',(86.7410018040281,58.702942207406,12.074908618816));
#69918=CARTESIAN_POINT('Ctrl Pts',(86.7410919053835,58.703806135607,12.0835557449932));
#69919=CARTESIAN_POINT('Ctrl Pts',(86.7415580182283,58.7060706472586,12.1061440589256));
#69920=CARTESIAN_POINT('Ctrl Pts',(86.7420753634555,58.707475518576,12.1200806591847));
#69921=CARTESIAN_POINT('Ctrl Pts',(86.746768418057,58.7163494988146,12.2075978878099));
#69922=CARTESIAN_POINT('Ctrl Pts',(86.7571121162255,58.7240041119405,12.280690462698));
#69923=CARTESIAN_POINT('Ctrl Pts',(86.7891895874481,58.7389602834226,12.4192392532306));
#69924=CARTESIAN_POINT('Ctrl Pts',(86.8100325125482,58.7462237510326,12.4846604536736));
#69925=CARTESIAN_POINT('Ctrl Pts',(86.8454095501306,58.7559058844029,12.5708824252684));
#69926=CARTESIAN_POINT('Ctrl Pts',(86.8554272387554,58.7584451220267,12.5934080250685));
#69927=CARTESIAN_POINT('Ctrl Pts',(86.8695357928023,58.7617597370289,12.6227967860943));
#69928=CARTESIAN_POINT('Ctrl Pts',(86.8730436278863,58.7625645312254,12.6299312940433));
#69929=CARTESIAN_POINT('Ctrl Pts',(86.8789567462526,58.7638892888397,12.6416779636251));
#69930=CARTESIAN_POINT('Ctrl Pts',(86.8813237029761,58.7644114831957,12.646308981877));
#69931=CARTESIAN_POINT('Ctrl Pts',(86.8861759776172,58.7654656107405,12.6556603884779));
#69932=CARTESIAN_POINT('Ctrl Pts',(86.8886627078911,58.7659974467432,12.6603798968008));
#69933=CARTESIAN_POINT('Ctrl Pts',(86.8952239367357,58.7673794680054,12.6726442930866));
#69934=CARTESIAN_POINT('Ctrl Pts',(86.8993453542373,58.7682267976695,12.6801640539018));
#69935=CARTESIAN_POINT('Ctrl Pts',(86.9172956736287,58.771832675551,12.7121426107563));
#69936=CARTESIAN_POINT('Ctrl Pts',(86.9318595553397,58.7745498882907,12.7361833539785));
#69937=CARTESIAN_POINT('Ctrl Pts',(87.0016234939353,58.786770857829,12.8431626629664));
#69938=CARTESIAN_POINT('Ctrl Pts',(87.0656672784881,58.7959285372272,12.9199158702169));
#69939=CARTESIAN_POINT('Ctrl Pts',(87.1519442992313,58.8071691545005,13.001569548852));
#69940=CARTESIAN_POINT('Ctrl Pts',(87.1661526887944,58.8089892234156,13.0144196134261));
#69941=CARTESIAN_POINT('Ctrl Pts',(87.1806428565926,58.8108193550848,13.0269406924427));
#69942=CARTESIAN_POINT('',(86.7410003988283,58.8721740503657,12.0670064908467));
#69943=CARTESIAN_POINT('Ctrl Pts',(87.1806427698475,58.9814779498304,13.0269406174854));
#69944=CARTESIAN_POINT('Ctrl Pts',(87.1370767857196,58.9760709212452,12.9892948678408));
#69945=CARTESIAN_POINT('Ctrl Pts',(87.0961118985498,58.9706283137381,12.9487219918335));
#69946=CARTESIAN_POINT('Ctrl Pts',(87.046488376277,58.9633806464135,12.8923911806852));
#69947=CARTESIAN_POINT('Ctrl Pts',(87.0352153516528,58.9616848434087,12.8790493874646));
#69948=CARTESIAN_POINT('Ctrl Pts',(87.0172863890674,58.9589014380845,12.8569201167021));
#69949=CARTESIAN_POINT('Ctrl Pts',(87.0104630860139,58.9578205484458,12.848270564808));
#69950=CARTESIAN_POINT('Ctrl Pts',(86.998386982045,58.9558671301214,12.8325458268004));
#69951=CARTESIAN_POINT('Ctrl Pts',(86.9930935744683,58.954996264069,12.8255025527875));
#69952=CARTESIAN_POINT('Ctrl Pts',(86.9818958327033,58.9531217634808,12.8102757795346));
#69953=CARTESIAN_POINT('Ctrl Pts',(86.9760149465933,58.9521172976422,12.8020759113662));
#69954=CARTESIAN_POINT('Ctrl Pts',(86.964170595174,58.9500520129862,12.7851384369864));
#69955=CARTESIAN_POINT('Ctrl Pts',(86.9582173669713,58.9489909004524,12.7763946822364));
#69956=CARTESIAN_POINT('Ctrl Pts',(86.9276630636191,58.943420692495,12.7302906495264));
#69957=CARTESIAN_POINT('Ctrl Pts',(86.904943165941,58.9388443760581,12.6917300161594));
#69958=CARTESIAN_POINT('Ctrl Pts',(86.8627625679972,58.9293682023556,12.610637976312));
#69959=CARTESIAN_POINT('Ctrl Pts',(86.8435204478985,58.9244698166207,12.5680661457923));
#69960=CARTESIAN_POINT('Ctrl Pts',(86.8057233730358,58.9134398154253,12.4704416824064));
#69961=CARTESIAN_POINT('Ctrl Pts',(86.7885092840389,58.9073082070982,12.4149729282886));
#69962=CARTESIAN_POINT('Ctrl Pts',(86.7695260317669,58.8987446860058,12.3347711262844));
#69963=CARTESIAN_POINT('Ctrl Pts',(86.7645901871672,58.896229604006,12.3108639874167));
#69964=CARTESIAN_POINT('Ctrl Pts',(86.758925072365,58.8929152561057,12.278779590411));
#69965=CARTESIAN_POINT('Ctrl Pts',(86.7575817969577,58.8920876253673,12.2707183422853));
#69966=CARTESIAN_POINT('Ctrl Pts',(86.7555844325409,58.8907877905039,12.2579742130376));
#69967=CARTESIAN_POINT('Ctrl Pts',(86.7548785547574,58.8903128530538,12.2532999279555));
#69968=CARTESIAN_POINT('Ctrl Pts',(86.7535263231813,58.8893710399795,12.2439938783842));
#69969=CARTESIAN_POINT('Ctrl Pts',(86.7528794396254,58.888904167553,12.2393624123626));
#69970=CARTESIAN_POINT('Ctrl Pts',(86.7515738464782,58.8879260168383,12.2296224062515));
#69971=CARTESIAN_POINT('Ctrl Pts',(86.7509206057112,58.8874150485045,12.2245132532131));
#69972=CARTESIAN_POINT('Ctrl Pts',(86.7494288906419,58.8861937344408,12.2122537603548));
#69973=CARTESIAN_POINT('Ctrl Pts',(86.7486200793685,58.8854849261736,12.2050998591358));
#69974=CARTESIAN_POINT('Ctrl Pts',(86.7433293527182,58.8804911841479,12.1544487596178));
#69975=CARTESIAN_POINT('Ctrl Pts',(86.7410350631278,58.8763112249515,12.1107462294122));
#69976=CARTESIAN_POINT('Ctrl Pts',(86.7410003988283,58.8721740503657,12.0670064908467));
#69977=CARTESIAN_POINT('Ctrl Pts',(86.7410004001107,58.8721742032935,12.0670081076555));
#69978=CARTESIAN_POINT('Ctrl Pts',(86.7409117877615,58.8616153025445,11.9553755380898));
#69979=CARTESIAN_POINT('Ctrl Pts',(86.7555409402393,58.8513590986153,11.8442192881856));
#69980=CARTESIAN_POINT('Ctrl Pts',(86.788652066914,58.8390852970701,11.7210078015403));
#69981=CARTESIAN_POINT('Ctrl Pts',(86.7930781763349,58.8375441668072,11.7056939255015));
#69982=CARTESIAN_POINT('Ctrl Pts',(86.8008723323203,58.8349809045229,11.6805137991907));
#69983=CARTESIAN_POINT('Ctrl Pts',(86.8040758469691,58.8339639243966,11.6705981075384));
#69984=CARTESIAN_POINT('Ctrl Pts',(86.8105862816504,58.8319650394509,11.651263284215));
#69985=CARTESIAN_POINT('Ctrl Pts',(86.8138829697394,58.8309835284974,11.6418414914347));
#69986=CARTESIAN_POINT('Ctrl Pts',(86.8203028284725,58.8291272884535,11.6241650474497));
#69987=CARTESIAN_POINT('Ctrl Pts',(86.8234016777888,58.8282534141291,11.6159021276743));
#69988=CARTESIAN_POINT('Ctrl Pts',(86.830621571191,58.8262656671969,11.5972444221609));
#69989=CARTESIAN_POINT('Ctrl Pts',(86.834794226551,58.8251501267197,11.5868705969163));
#69990=CARTESIAN_POINT('Ctrl Pts',(86.8460551654791,58.8222226105092,11.5599081757565));
#69991=CARTESIAN_POINT('Ctrl Pts',(86.8533605720975,58.820403489325,11.5434138620995));
#69992=CARTESIAN_POINT('Ctrl Pts',(86.9039389873504,58.8083048477157,11.4354856982928));
#69993=CARTESIAN_POINT('Ctrl Pts',(86.9576436566689,58.7976670723019,11.3493670463497));
#69994=CARTESIAN_POINT('Ctrl Pts',(87.0459893537253,58.7828032407126,11.239410576555));
#69995=CARTESIAN_POINT('Ctrl Pts',(87.0724658980973,58.7786048267982,11.2094663575879));
#69996=CARTESIAN_POINT('Ctrl Pts',(87.1111100452255,58.7728541027258,11.1697087077035));
#69997=CARTESIAN_POINT('Ctrl Pts',(87.1221111980039,58.7712559615836,11.1587972806687));
#69998=CARTESIAN_POINT('Ctrl Pts',(87.1393460502387,58.7688143821583,11.1423176212434));
#69999=CARTESIAN_POINT('Ctrl Pts',(87.1454391614459,58.7679627251687,11.1366054700783));
#70000=CARTESIAN_POINT('Ctrl Pts',(87.1565861965223,58.766426000806,11.1263601062111));
#70001=CARTESIAN_POINT('Ctrl Pts',(87.1616208960014,58.7657396245582,11.1218065755442));
#70002=CARTESIAN_POINT('Ctrl Pts',(87.1703544593622,58.7645624953415,11.1140340806524));
#70003=CARTESIAN_POINT('Ctrl Pts',(87.1740358354661,58.7640703743801,11.1107958188212));
#70004=CARTESIAN_POINT('Ctrl Pts',(87.1812876699972,58.763109024542,11.1044909785051));
#70005=CARTESIAN_POINT('Ctrl Pts',(87.1848565589396,58.7626396705554,11.1014228043025));
#70006=CARTESIAN_POINT('Ctrl Pts',(87.1945858387831,58.7613700223425,11.0931521547797));
#70007=CARTESIAN_POINT('Ctrl Pts',(87.2007790360743,58.7605724558272,11.0879882338703));
#70008=CARTESIAN_POINT('Ctrl Pts',(87.2252140227933,58.7574649368521,11.0680056508454));
#70009=CARTESIAN_POINT('Ctrl Pts',(87.2438182685265,58.7551834181135,11.0536340776646));
#70010=CARTESIAN_POINT('Ctrl Pts',(87.3471877401853,58.7428863943113,10.9782699792461));
#70011=CARTESIAN_POINT('Ctrl Pts',(87.4388353139457,58.7333041414434,10.9273885918752));
#70012=CARTESIAN_POINT('Ctrl Pts',(87.5783697371137,58.7190710324237,10.8710734169435));
#70013=CARTESIAN_POINT('Ctrl Pts',(87.6219507121271,58.7146756262845,10.8561826098825));
#70014=CARTESIAN_POINT('Ctrl Pts',(87.6798584196734,58.7088278358892,10.839849312189));
#70015=CARTESIAN_POINT('Ctrl Pts',(87.6935407575736,58.7074457508682,10.8362358574955));
#70016=CARTESIAN_POINT('Ctrl Pts',(87.7163370649298,58.7051404629563,10.8306212071289));
#70017=CARTESIAN_POINT('Ctrl Pts',(87.7254181552078,58.7042214644977,10.8284904018527));
#70018=CARTESIAN_POINT('Ctrl Pts',(87.743262549955,58.7024137538193,10.8245102242282));
#70019=CARTESIAN_POINT('Ctrl Pts',(87.7520235928515,58.7015253453244,10.8226531394818));
#70020=CARTESIAN_POINT('Ctrl Pts',(87.7732504249262,58.6993701950009,10.818387749608));
#70021=CARTESIAN_POINT('Ctrl Pts',(87.7857337963603,58.698100555286,10.8160734840956));
#70022=CARTESIAN_POINT('Ctrl Pts',(87.8286137385708,58.6937300750784,10.8087872579349));
#70023=CARTESIAN_POINT('Ctrl Pts',(87.8591523925783,58.6906011732947,10.8047345569668));
#70024=CARTESIAN_POINT('Ctrl Pts',(87.9784353889358,58.6783012289841,10.7932992900981));
#70025=CARTESIAN_POINT('Ctrl Pts',(88.067699914573,58.6689047041998,10.794148126335));
#70026=CARTESIAN_POINT('Ctrl Pts',(88.2054946442493,58.6542982785079,10.809997750042));
#70027=CARTESIAN_POINT('Ctrl Pts',(88.2544974247389,58.6490896776457,10.8185705767224));
#70028=CARTESIAN_POINT('Ctrl Pts',(88.3149112348361,58.6427270035871,10.8328370560962));
#70029=CARTESIAN_POINT('Ctrl Pts',(88.3269035998228,58.6414670526868,10.8358545444968));
#70030=CARTESIAN_POINT('Ctrl Pts',(88.3447692409538,58.6395963491309,10.8406283734652));
#70031=CARTESIAN_POINT('Ctrl Pts',(88.3506764199351,58.6389788514012,10.8422526956962));
#70032=CARTESIAN_POINT('Ctrl Pts',(88.3608704792266,58.63791528378,10.845135304943));
#70033=CARTESIAN_POINT('Ctrl Pts',(88.3651626780616,58.6374681197263,10.8463735179295));
#70034=CARTESIAN_POINT('Ctrl Pts',(88.3752675515055,58.6364168922349,10.8493464161891));
#70035=CARTESIAN_POINT('Ctrl Pts',(88.3810744688797,58.6358139325587,10.8511001336936));
#70036=CARTESIAN_POINT('Ctrl Pts',(88.3983850683685,58.6340192525014,10.8564636570658));
#70037=CARTESIAN_POINT('Ctrl Pts',(88.4098506962277,58.6328342100168,10.8601959043312));
#70038=CARTESIAN_POINT('Ctrl Pts',(88.4976553892865,58.6237738875421,10.8901673495209));
#70039=CARTESIAN_POINT('Ctrl Pts',(88.5714044312577,58.6162440517771,10.9234729705172));
#70040=CARTESIAN_POINT('Ctrl Pts',(88.7119240501686,58.6010799772221,11.003838706996));
#70041=CARTESIAN_POINT('Ctrl Pts',(88.778312033937,58.5934762488734,11.0507611068985));
#70042=CARTESIAN_POINT('Ctrl Pts',(88.8523737681701,58.5840088797201,11.1145447861536));
#70043=CARTESIAN_POINT('Ctrl Pts',(88.8647659290384,58.5823882705203,11.1256487259842));
#70044=CARTESIAN_POINT('Ctrl Pts',(88.8841393004861,58.5797923868578,11.1437068045899));
#70045=CARTESIAN_POINT('Ctrl Pts',(88.8912642844276,58.5788237398503,11.1505046409948));
#70046=CARTESIAN_POINT('Ctrl Pts',(88.9046403991701,58.5769778010686,11.1635670961257));
#70047=CARTESIAN_POINT('Ctrl Pts',(88.9109065443432,58.5761012503558,11.169815582375));
#70048=CARTESIAN_POINT('Ctrl Pts',(88.9251025132104,58.5740876090394,11.1842705538872));
#70049=CARTESIAN_POINT('Ctrl Pts',(88.9329879016964,58.5729486773214,11.1925193144278));
#70050=CARTESIAN_POINT('Ctrl Pts',(88.9536019177779,58.5699153258734,11.2146734028036));
#70051=CARTESIAN_POINT('Ctrl Pts',(88.9661333172046,58.568012881167,11.2287571442493));
#70052=CARTESIAN_POINT('Ctrl Pts',(89.0496665149654,58.5549133065949,11.3269547691037));
#70053=CARTESIAN_POINT('Ctrl Pts',(89.1097694970408,58.5432873123365,11.4196953926493));
#70054=CARTESIAN_POINT('Ctrl Pts',(89.1781065003179,58.526600131987,11.562881542631));
#70055=CARTESIAN_POINT('Ctrl Pts',(89.196520648374,58.5215176853357,11.6079519533705));
#70056=CARTESIAN_POINT('Ctrl Pts',(89.2154232907968,58.5155731287881,11.6630646562695));
#70057=CARTESIAN_POINT('Ctrl Pts',(89.2184379953646,58.514597477717,11.6721905761405));
#70058=CARTESIAN_POINT('Ctrl Pts',(89.2230324687728,58.5130663936297,11.6866476696338));
#70059=CARTESIAN_POINT('Ctrl Pts',(89.2246812294648,58.5125072593936,11.6919561876885));
#70060=CARTESIAN_POINT('Ctrl Pts',(89.2277664843263,58.5114422578257,11.7021250148485));
#70061=CARTESIAN_POINT('Ctrl Pts',(89.2292087646248,58.5109361094244,11.7069831620253));
#70062=CARTESIAN_POINT('Ctrl Pts',(89.232645388408,58.5097092492029,11.7188182120293));
#70063=CARTESIAN_POINT('Ctrl Pts',(89.2346091063273,58.5089902815678,11.725803860849));
#70064=CARTESIAN_POINT('Ctrl Pts',(89.2411970534292,58.5065130044844,11.7500348515875));
#70065=CARTESIAN_POINT('Ctrl Pts',(89.2455177807447,58.5047705156264,11.7673618739297));
#70066=CARTESIAN_POINT('Ctrl Pts',(89.2669603556061,58.4953996100657,11.8617919774794));
#70067=CARTESIAN_POINT('Ctrl Pts',(89.2772293546733,58.4880534419646,11.9402840041561));
#70068=CARTESIAN_POINT('Ctrl Pts',(89.2819951784243,58.4759241693202,12.0696144020795));
#70069=CARTESIAN_POINT('Ctrl Pts',(89.2808499059722,58.4711883895201,12.1200579776393));
#70070=CARTESIAN_POINT('Ctrl Pts',(89.2740808794595,58.4633221547994,12.2022047800746));
#70071=CARTESIAN_POINT('Ctrl Pts',(89.27024621205,58.4602399467561,12.2339989251376));
#70072=CARTESIAN_POINT('Ctrl Pts',(89.2632418669668,58.4558975424663,12.2780092113431));
#70073=CARTESIAN_POINT('Ctrl Pts',(89.2610850943507,58.4546689023842,12.2903765331183));
#70074=CARTESIAN_POINT('Ctrl Pts',(89.2570641707339,58.452547453924,12.311571680849));
#70075=CARTESIAN_POINT('Ctrl Pts',(89.2552885801581,58.4516574985606,12.3204155788569));
#70076=CARTESIAN_POINT('Ctrl Pts',(89.2514730509701,58.4498350906204,12.3384238389548));
#70077=CARTESIAN_POINT('Ctrl Pts',(89.2494253994663,58.4489024444644,12.3475859656692));
#70078=CARTESIAN_POINT('Ctrl Pts',(89.2439695450625,58.4465262794236,12.3707864536412));
#70079=CARTESIAN_POINT('Ctrl Pts',(89.2404231516483,58.445078433943,12.384790450371));
#70080=CARTESIAN_POINT('Ctrl Pts',(89.2247991316418,58.4390690122588,12.4423428064532));
#70081=CARTESIAN_POINT('Ctrl Pts',(89.2106420066052,58.4344424531357,12.4852851696894));
#70082=CARTESIAN_POINT('Ctrl Pts',(89.1609531959061,58.4202532957062,12.6127154717471));
#70083=CARTESIAN_POINT('Ctrl Pts',(89.1185428065423,58.4105211119895,12.6942006333123));
#70084=CARTESIAN_POINT('Ctrl Pts',(89.048390739255,58.3972908421033,12.7994428383259));
#70085=CARTESIAN_POINT('Ctrl Pts',(89.0278425470015,58.3936709820817,12.8276756806663));
#70086=CARTESIAN_POINT('Ctrl Pts',(89.0006440106737,58.3892109097503,12.8619795218085));
#70087=CARTESIAN_POINT('Ctrl Pts',(88.9950606346836,58.3883115206806,12.8688719390346));
#70088=CARTESIAN_POINT('Ctrl Pts',(88.9859638161077,58.3868725669035,12.8798640506232));
#70089=CARTESIAN_POINT('Ctrl Pts',(88.9824958172821,58.3863299902342,12.8840006214246));
#70090=CARTESIAN_POINT('Ctrl Pts',(88.9757055829966,58.3852794046092,12.8919957993825));
#70091=CARTESIAN_POINT('Ctrl Pts',(88.9723864299962,58.3847712259424,12.8958566484953));
#70092=CARTESIAN_POINT('Ctrl Pts',(88.9640132241627,58.3835022689435,12.9054787218968));
#70093=CARTESIAN_POINT('Ctrl Pts',(88.9589299964689,58.3827435975447,12.9112144476724));
#70094=CARTESIAN_POINT('Ctrl Pts',(88.9399992934022,58.3799592000895,12.9321895157328));
#70095=CARTESIAN_POINT('Ctrl Pts',(88.9258325639842,58.3779549763666,12.9471387610327));
#70096=CARTESIAN_POINT('Ctrl Pts',(88.857241230216,58.3685757050472,13.0160799497583));
#70097=CARTESIAN_POINT('Ctrl Pts',(88.7983586355497,58.3614463243779,13.0654227539293));
#70098=CARTESIAN_POINT('Ctrl Pts',(88.6946773653598,58.3496142310001,13.1374198284483));
#70099=CARTESIAN_POINT('Ctrl Pts',(88.6523624066709,58.3449575386355,13.1632733072907));
#70100=CARTESIAN_POINT('Ctrl Pts',(88.5896220205865,58.3381697481612,13.196734955352));
#70101=CARTESIAN_POINT('Ctrl Pts',(88.5703413516156,58.3360990337979,13.206395597784));
#70102=CARTESIAN_POINT('Ctrl Pts',(88.535046751526,58.3323259332403,13.2229696904649));
#70103=CARTESIAN_POINT('Ctrl Pts',(88.5191182975175,58.3306293947817,13.2300530863234));
#70104=CARTESIAN_POINT('Ctrl Pts',(88.4938186334599,58.3279408297784,13.2406856759083));
#70105=CARTESIAN_POINT('Ctrl Pts',(88.4845420248605,58.3269562918225,13.2444558568179));
#70106=CARTESIAN_POINT('Ctrl Pts',(88.4670121477407,58.3250975134683,13.2513399173737));
#70107=CARTESIAN_POINT('Ctrl Pts',(88.458769069066,58.324224154033,13.2544782915241));
#70108=CARTESIAN_POINT('Ctrl Pts',(88.4400500964841,58.3222419319001,13.2613827566492));
#70109=CARTESIAN_POINT('Ctrl Pts',(88.4295562022615,58.3211314386496,13.2650974128277));
#70110=CARTESIAN_POINT('Ctrl Pts',(88.4020967793693,58.3182265664748,13.2744132109398));
#70111=CARTESIAN_POINT('Ctrl Pts',(88.3850602172566,58.3164252240534,13.2797948961812));
#70112=CARTESIAN_POINT('Ctrl Pts',(88.2706129929587,58.3043230017434,13.3133095345537));
#70113=CARTESIAN_POINT('Ctrl Pts',(88.1702692631488,58.2936613478557,13.330042398711));
#70114=CARTESIAN_POINT('Ctrl Pts',(88.0290736568651,58.2787665736703,13.336501306081));
#70115=CARTESIAN_POINT('Ctrl Pts',(87.9890452397125,58.2745619939403,13.3364403701319));
#70116=CARTESIAN_POINT('Ctrl Pts',(87.9263363182777,58.2680498841345,13.3333794727661));
#70117=CARTESIAN_POINT('Ctrl Pts',(87.903620648719,58.2657066236617,13.3316573634987));
#70118=CARTESIAN_POINT('Ctrl Pts',(87.8732694413172,58.2626059193666,13.3285332013652));
#70119=CARTESIAN_POINT('Ctrl Pts',(87.8655846306259,58.2618234450197,13.3276711824862));
#70120=CARTESIAN_POINT('Ctrl Pts',(87.8527895999044,58.2605254806098,13.3261174753903));
#70121=CARTESIAN_POINT('Ctrl Pts',(87.8476749955015,58.2600079337665,13.3254647791904));
#70122=CARTESIAN_POINT('Ctrl Pts',(87.8378775906762,58.2590191728347,13.3241538020797));
#70123=CARTESIAN_POINT('Ctrl Pts',(87.8331943014986,58.2585476764829,13.3235004948725));
#70124=CARTESIAN_POINT('Ctrl Pts',(87.8204206684261,58.2572645136297,13.3216458145816));
#70125=CARTESIAN_POINT('Ctrl Pts',(87.8123378573726,58.2564556772551,13.3203923865316));
#70126=CARTESIAN_POINT('Ctrl Pts',(87.7801305916342,58.2532430094398,13.3150787628242));
#70127=CARTESIAN_POINT('Ctrl Pts',(87.7561111497571,58.2508701164471,13.3103996097835));
#70128=CARTESIAN_POINT('Ctrl Pts',(87.6604818668318,58.2414573869847,13.2888846184787));
#70129=CARTESIAN_POINT('Ctrl Pts',(87.5902540031261,58.2346174625761,13.2665353614745));
#70130=CARTESIAN_POINT('Ctrl Pts',(87.4777213102011,58.2231863794653,13.2196253976678));
#70131=CARTESIAN_POINT('Ctrl Pts',(87.4341963076196,58.2186392853675,13.1984903992423));
#70132=CARTESIAN_POINT('Ctrl Pts',(87.3647690740798,58.2110461799235,13.1597353874689));
#70133=CARTESIAN_POINT('Ctrl Pts',(87.3381244210555,58.2080439466192,13.1435479578421));
#70134=CARTESIAN_POINT('Ctrl Pts',(87.301722704792,58.2037948979502,13.1195560341631));
#70135=CARTESIAN_POINT('Ctrl Pts',(87.2914425164443,58.2025777995275,13.1125617993605));
#70136=CARTESIAN_POINT('Ctrl Pts',(87.2739014351877,58.2004699301109,13.1002469238456));
#70137=CARTESIAN_POINT('Ctrl Pts',(87.2665911833855,58.1995819160712,13.094997811952));
#70138=CARTESIAN_POINT('Ctrl Pts',(87.2526467505545,58.1978690179649,13.0847586824416));
#70139=CARTESIAN_POINT('Ctrl Pts',(87.2460044687283,58.1970446245268,13.0797804164424));
#70140=CARTESIAN_POINT('Ctrl Pts',(87.2285883359835,58.1948600599779,13.066458730388));
#70141=CARTESIAN_POINT('Ctrl Pts',(87.2178995121185,58.1934956773863,13.0580066845039));
#70142=CARTESIAN_POINT('Ctrl Pts',(87.1983434524692,58.1909539173572,13.0420249009918));
#70143=CARTESIAN_POINT('Ctrl Pts',(87.189440499867,58.1897786506171,13.0345428123893));
#70144=CARTESIAN_POINT('Ctrl Pts',(87.1806428261678,58.1885986874538,13.0269406661524));
#70145=CARTESIAN_POINT('Origin',(88.011,66.41344859951,12.066));
#70146=CARTESIAN_POINT('',(87.1806428354228,57.224088141927,13.0269406741497));
#70147=CARTESIAN_POINT('',(87.1806427720391,57.39301128552,13.0269406193793));
#70148=CARTESIAN_POINT('',(87.1806428354228,66.41344859951,13.0269406741497));
#70149=CARTESIAN_POINT('',(86.7410005228783,57.90950140049,12.0648475632288));
#70150=CARTESIAN_POINT('Ctrl Pts',(86.7410005228783,57.90950140049,12.0648475632288));
#70151=CARTESIAN_POINT('Ctrl Pts',(86.7410619857771,57.9027591545593,11.9971146937284));
#70152=CARTESIAN_POINT('Ctrl Pts',(86.7465456957433,57.8960169086286,11.929620021689));
#70153=CARTESIAN_POINT('Ctrl Pts',(86.7573167636289,57.8892746626979,11.8630755242906));
#70154=CARTESIAN_POINT('Ctrl Pts',(86.7614355253459,57.8866964870962,11.8376294931931));
#70155=CARTESIAN_POINT('Ctrl Pts',(86.7663269456463,57.8841183114945,11.8123221050166));
#70156=CARTESIAN_POINT('Ctrl Pts',(86.7719817452547,57.8815401358928,11.7871922447137));
#70157=CARTESIAN_POINT('Ctrl Pts',(86.7828344623163,57.8765920895821,11.7389629028177));
#70158=CARTESIAN_POINT('Ctrl Pts',(86.7965314004248,57.8716440432713,11.691261574028));
#70159=CARTESIAN_POINT('Ctrl Pts',(86.8130042208988,57.8666959969606,11.6444479708794));
#70160=CARTESIAN_POINT('Ctrl Pts',(86.8294467317454,57.8617570549463,11.5977205037312));
#70161=CARTESIAN_POINT('Ctrl Pts',(86.8486548145271,57.8568181129319,11.55187803535));
#70162=CARTESIAN_POINT('Ctrl Pts',(86.8705096968997,57.8518791709176,11.5072676235135));
#70163=CARTESIAN_POINT('Ctrl Pts',(86.8923423888668,57.8469452436695,11.4627025069625));
#70164=CARTESIAN_POINT('Ctrl Pts',(86.9168163203082,57.8420113164214,11.4193674601876));
#70165=CARTESIAN_POINT('Ctrl Pts',(86.9437645123884,57.8370773891734,11.3775899376226));
#70166=CARTESIAN_POINT('Ctrl Pts',(86.9706968097254,57.8321463720837,11.3358370565249));
#70167=CARTESIAN_POINT('Ctrl Pts',(87.0001001801263,57.827215354994,11.2956403393399));
#70168=CARTESIAN_POINT('Ctrl Pts',(87.0317628358655,57.8222843379043,11.2573006885264));
#70169=CARTESIAN_POINT('Ctrl Pts',(87.0634202885994,57.8173541311101,11.2189673379237));
#70170=CARTESIAN_POINT('Ctrl Pts',(87.0973359401222,57.8124239243159,11.1824908695214));
#70171=CARTESIAN_POINT('Ctrl Pts',(87.133257610372,57.8074937175218,11.1481392821075));
#70172=CARTESIAN_POINT('Ctrl Pts',(87.1692143770386,57.8025586937859,11.1137541322891));
#70173=CARTESIAN_POINT('Ctrl Pts',(87.2071806781485,57.79762367005,11.0814983872616));
#70174=CARTESIAN_POINT('Ctrl Pts',(87.2468686439494,57.7926886463141,11.0516020156269));
#70175=CARTESIAN_POINT('Ctrl Pts',(87.2865779685748,57.7877509667024,11.021689554698));
#70176=CARTESIAN_POINT('Ctrl Pts',(87.3280103461592,57.7828132870908,10.9941392993314));
#70177=CARTESIAN_POINT('Ctrl Pts',(87.3708490295984,57.7778756074791,10.9691377775245));
#70178=CARTESIAN_POINT('Ctrl Pts',(87.4137677090518,57.7729287073532,10.9440895684263));
#70179=CARTESIAN_POINT('Ctrl Pts',(87.4580974467746,57.7679818072274,10.9215998401677));
#70180=CARTESIAN_POINT('Ctrl Pts',(87.5034984997004,57.7630349071015,10.9018083374317));
#70181=CARTESIAN_POINT('Ctrl Pts',(87.5264702739549,57.7605319018709,10.8917943420789));
#70182=CARTESIAN_POINT('Ctrl Pts',(87.5497160264354,57.7580288966402,10.8824703397855));
#70183=CARTESIAN_POINT('Ctrl Pts',(87.573190329049,57.7555258914096,10.8738495514316));
#70184=CARTESIAN_POINT('Ctrl Pts',(87.6195953205454,57.7505778450988,10.8568076134095));
#70185=CARTESIAN_POINT('Ctrl Pts',(87.6670994190304,57.7456297987881,10.8424415593594));
#70186=CARTESIAN_POINT('Ctrl Pts',(87.7153633555719,57.7406817524774,10.8308890841421));
#70187=CARTESIAN_POINT('Ctrl Pts',(87.7635384875313,57.735742810463,10.8193578652253));
#70188=CARTESIAN_POINT('Ctrl Pts',(87.8124701560871,57.7308038684487,10.8106300840773));
#70189=CARTESIAN_POINT('Ctrl Pts',(87.8618023686802,57.7258649264344,10.8047942012469));
#70190=CARTESIAN_POINT('Ctrl Pts',(87.9110844916965,57.7209309991863,10.7989642438936));
#70191=CARTESIAN_POINT('Ctrl Pts',(87.960765812076,57.7159970719382,10.7960204360653));
#70192=CARTESIAN_POINT('Ctrl Pts',(88.0104806593026,57.7110631446902,10.7960001061869));
#70193=CARTESIAN_POINT('Ctrl Pts',(88.0601661834216,57.7061321276005,10.7959797882996));
#70194=CARTESIAN_POINT('Ctrl Pts',(88.1098846482655,57.7012011105108,10.7988795325896));
#70195=CARTESIAN_POINT('Ctrl Pts',(88.1592683859079,57.6962700934211,10.8046846208262));
#70196=CARTESIAN_POINT('Ctrl Pts',(88.208644008506,57.6913398866269,10.8104887551345));
#70197=CARTESIAN_POINT('Ctrl Pts',(88.2576844692856,57.6864096798327,10.8191972206621));
#70198=CARTESIAN_POINT('Ctrl Pts',(88.3060278346373,57.6814794730386,10.8307435178113));
#70199=CARTESIAN_POINT('Ctrl Pts',(88.3544184327286,57.6765444493027,10.8423010959965));
#70200=CARTESIAN_POINT('Ctrl Pts',(88.4021100417701,57.6716094255668,10.856701913136));
#70201=CARTESIAN_POINT('Ctrl Pts',(88.4487533200729,57.6666744018309,10.8738288584414));
#70202=CARTESIAN_POINT('Ctrl Pts',(88.4954217003324,57.6617367222192,10.8909650209343));
#70203=CARTESIAN_POINT('Ctrl Pts',(88.5410401234826,57.6567990426076,10.9108300140715));
#70204=CARTESIAN_POINT('Ctrl Pts',(88.5852800801664,57.6518613629959,10.9332589044605));
#70205=CARTESIAN_POINT('Ctrl Pts',(88.6296026495712,57.6469144628701,10.9557296780655));
#70206=CARTESIAN_POINT('Ctrl Pts',(88.6725411413171,57.6419675627442,10.9807736284387));
#70207=CARTESIAN_POINT('Ctrl Pts',(88.7137938767186,57.6370206626184,11.0081811275806));
#70208=CARTESIAN_POINT('Ctrl Pts',(88.7346667081612,57.6345176573877,11.0220486227729));
#70209=CARTESIAN_POINT('Ctrl Pts',(88.7551084672777,57.632014652157,11.0365205442552));
#70210=CARTESIAN_POINT('Ctrl Pts',(88.7750834067852,57.6295116469264,11.0515658979138));
#70211=CARTESIAN_POINT('Ctrl Pts',(88.8145707096986,57.6245636006156,11.081308187603));
#70212=CARTESIAN_POINT('Ctrl Pts',(88.8524061001075,57.6196155543049,11.113425256499));
#70213=CARTESIAN_POINT('Ctrl Pts',(88.8882898785945,57.6146675079941,11.1477067631113));
#70214=CARTESIAN_POINT('Ctrl Pts',(88.9241076317183,57.6097285659798,11.1819251925053));
#70215=CARTESIAN_POINT('Ctrl Pts',(88.957980501935,57.6047896239655,11.2182997854886));
#70216=CARTESIAN_POINT('Ctrl Pts',(88.9896410817415,57.5998506819511,11.2565794460678));
#70217=CARTESIAN_POINT('Ctrl Pts',(89.0212695149046,57.5949167547031,11.2948202393047));
#70218=CARTESIAN_POINT('Ctrl Pts',(89.0506897569054,57.589982827455,11.3349618506302));
#70219=CARTESIAN_POINT('Ctrl Pts',(89.0776721081081,57.5850489002069,11.3767173193934));
#70220=CARTESIAN_POINT('Ctrl Pts',(89.1046385444195,57.5801178831172,11.4184481596971));
#70221=CARTESIAN_POINT('Ctrl Pts',(89.1291696416839,57.5751868660275,11.4617905123143));
#70222=CARTESIAN_POINT('Ctrl Pts',(89.1510783423698,57.5702558489378,11.5064275084859));
#70223=CARTESIAN_POINT('Ctrl Pts',(89.1729834428811,57.5653256421437,11.5510571696275));
#70224=CARTESIAN_POINT('Ctrl Pts',(89.1922667618919,57.5603954353495,11.5969805598905));
#70225=CARTESIAN_POINT('Ctrl Pts',(89.2087878547802,57.5554652285553,11.6438575418877));
#70226=CARTESIAN_POINT('Ctrl Pts',(89.2253250892107,57.5505302048195,11.6907803239294));
#70227=CARTESIAN_POINT('Ctrl Pts',(89.2390945276057,57.5455951810836,11.738658039764));
#70228=CARTESIAN_POINT('Ctrl Pts',(89.250005074718,57.5406601573477,11.787133679296));
#70229=CARTESIAN_POINT('Ctrl Pts',(89.2609214935463,57.535722477736,11.8356354069045));
#70230=CARTESIAN_POINT('Ctrl Pts',(89.2689758685409,57.5307847981243,11.8847351576829));
#70231=CARTESIAN_POINT('Ctrl Pts',(89.274128580668,57.5258471185127,11.9340674842974));
#70232=CARTESIAN_POINT('Ctrl Pts',(89.2792909148563,57.5209002183868,11.9834919330123));
#70233=CARTESIAN_POINT('Ctrl Pts',(89.281540746755,57.515953318261,12.0331492766801));
#70234=CARTESIAN_POINT('Ctrl Pts',(89.2808905591385,57.5110064181352,12.0826723666826));
#70235=CARTESIAN_POINT('Ctrl Pts',(89.2805615807958,57.5085034129045,12.1077297865134));
#70236=CARTESIAN_POINT('Ctrl Pts',(89.2794909980342,57.5060004076738,12.1327528934289));
#70237=CARTESIAN_POINT('Ctrl Pts',(89.2776854603828,57.5034974024432,12.1576948442112));
#70238=CARTESIAN_POINT('Ctrl Pts',(89.2741161974,57.4985493561325,12.2070011445093));
#70239=CARTESIAN_POINT('Ctrl Pts',(89.2676558368303,57.4936013098217,12.2562077154442));
#70240=CARTESIAN_POINT('Ctrl Pts',(89.2583185344195,57.488653263511,12.3049486842262));
#70241=CARTESIAN_POINT('Ctrl Pts',(89.2489984124399,57.4837143214966,12.3535999706975));
#70242=CARTESIAN_POINT('Ctrl Pts',(89.2368119496979,57.4787753794823,12.4017868203275));
#70243=CARTESIAN_POINT('Ctrl Pts',(89.2218250557544,57.473836437468,12.4491483842551));
#70244=CARTESIAN_POINT('Ctrl Pts',(89.2068533787886,57.4689025102199,12.4964618595086));
#70245=CARTESIAN_POINT('Ctrl Pts',(89.1890870641493,57.4639685829718,12.5429511879973));
#70246=CARTESIAN_POINT('Ctrl Pts',(89.1686426047564,57.4590346557237,12.5882677470921));
#70247=CARTESIAN_POINT('Ctrl Pts',(89.1482102040365,57.454103638634,12.6335575773039));
#70248=CARTESIAN_POINT('Ctrl Pts',(89.1251030128179,57.4491726215443,12.6776755099094));
#70249=CARTESIAN_POINT('Ctrl Pts',(89.0994857794802,57.4442416044546,12.7202925246932));
#70250=CARTESIAN_POINT('Ctrl Pts',(89.0738727557262,57.4393113976605,12.762902536383));
#70251=CARTESIAN_POINT('Ctrl Pts',(89.0457507917049,57.4343811908663,12.8040116510038));
#70252=CARTESIAN_POINT('Ctrl Pts',(89.0153294670472,57.4294509840721,12.8433173879573));
#70253=CARTESIAN_POINT('Ctrl Pts',(88.984878419955,57.4245159603362,12.8826615276497));
#70254=CARTESIAN_POINT('Ctrl Pts',(88.9521238636205,57.4195809366003,12.9201983382039));
#70255=CARTESIAN_POINT('Ctrl Pts',(88.9173163198337,57.4146459128644,12.95565764674));
#70256=CARTESIAN_POINT('Ctrl Pts',(88.8824900437131,57.4097082332528,12.9911360383694));
#70257=CARTESIAN_POINT('Ctrl Pts',(88.8456089866316,57.4047705536411,13.0245343334098));
#70258=CARTESIAN_POINT('Ctrl Pts',(88.8069586793161,57.3998328740294,13.05562102889));
#70259=CARTESIAN_POINT('Ctrl Pts',(88.7682361972678,57.3948859739036,13.0867657749809));
#70260=CARTESIAN_POINT('Ctrl Pts',(88.7277383175997,57.3899390737777,13.1155899881723));
#70261=CARTESIAN_POINT('Ctrl Pts',(88.6857802602803,57.3849921736519,13.141905014551));
#70262=CARTESIAN_POINT('Ctrl Pts',(88.6645505539457,57.3824891684212,13.1552197464022));
#70263=CARTESIAN_POINT('Ctrl Pts',(88.6429474292981,57.3799861631906,13.1678928293979));
#70264=CARTESIAN_POINT('Ctrl Pts',(88.6210138470131,57.3774831579599,13.1799044422446));
#70265=CARTESIAN_POINT('Ctrl Pts',(88.5776546164459,57.3725351116492,13.2036495051411));
#70266=CARTESIAN_POINT('Ctrl Pts',(88.5328110428732,57.3675870653385,13.2249116026642));
#70267=CARTESIAN_POINT('Ctrl Pts',(88.4867981818304,57.3626390190277,13.2435041784074));
#70268=CARTESIAN_POINT('Ctrl Pts',(88.44086998344,57.3577000770134,13.2620625442201));
#70269=CARTESIAN_POINT('Ctrl Pts',(88.3937772685885,57.3527611349991,13.277960926507));
#70270=CARTESIAN_POINT('Ctrl Pts',(88.345858943308,57.3478221929847,13.2910589733097));
#70271=CARTESIAN_POINT('Ctrl Pts',(88.2979892720104,57.3428882657367,13.3041437209802));
#70272=CARTESIAN_POINT('Ctrl Pts',(88.2492961758408,57.3379543384886,13.3144336181903));
#70273=CARTESIAN_POINT('Ctrl Pts',(88.2001357256658,57.3330204112405,13.3218374406255));
#70274=CARTESIAN_POINT('Ctrl Pts',(88.1510042716006,57.3280893941508,13.3292368960941));
#70275=CARTESIAN_POINT('Ctrl Pts',(88.1014065504667,57.3231583770611,13.3337535676249));
#70276=CARTESIAN_POINT('Ctrl Pts',(88.0517083384299,57.3182273599714,13.3353474036615));
#70277=CARTESIAN_POINT('Ctrl Pts',(88.0020182931138,57.3132971531773,13.3369409777891));
#70278=CARTESIAN_POINT('Ctrl Pts',(87.9522283371031,57.3083669463831,13.3356126533678));
#70279=CARTESIAN_POINT('Ctrl Pts',(87.9027062664847,57.3034367395889,13.3313744375802));
#70280=CARTESIAN_POINT('Ctrl Pts',(87.8531358115008,57.298501715853,13.3271320809442));
#70281=CARTESIAN_POINT('Ctrl Pts',(87.8038343114249,57.2935666921171,13.3199742043374));
#70282=CARTESIAN_POINT('Ctrl Pts',(87.7551646269224,57.2886316683812,13.3099647349834));
#70283=CARTESIAN_POINT('Ctrl Pts',(87.7064687499145,57.2836939887696,13.2999498788453));
#70284=CARTESIAN_POINT('Ctrl Pts',(87.658405895437,57.2787563091579,13.2870805159034));
#70285=CARTESIAN_POINT('Ctrl Pts',(87.6113254255502,57.2738186295463,13.2714709596412));
#70286=CARTESIAN_POINT('Ctrl Pts',(87.5641570386307,57.2688717294204,13.2558322544374));
#70287=CARTESIAN_POINT('Ctrl Pts',(87.5179752070549,57.2639248292946,13.2374433459321));
#70288=CARTESIAN_POINT('Ctrl Pts',(87.4731093978903,57.2589779291688,13.2164667314452));
#70289=CARTESIAN_POINT('Ctrl Pts',(87.4504084433207,57.2564749239381,13.2058530997875));
#70290=CARTESIAN_POINT('Ctrl Pts',(87.4280440099079,57.2539719187074,13.1945777219539));
#70291=CARTESIAN_POINT('Ctrl Pts',(87.4060560517573,57.2514689134767,13.1826659390725));
#70292=CARTESIAN_POINT('Ctrl Pts',(87.3626043588745,57.2465225781316,13.1591263667343));
#70293=CARTESIAN_POINT('Ctrl Pts',(87.3204326650643,57.2415762427864,13.1329948052886));
#70294=CARTESIAN_POINT('Ctrl Pts',(87.2798682499743,57.2366299074413,13.1044345738198));
#70295=CARTESIAN_POINT('Ctrl Pts',(87.2455836502466,57.2324493189365,13.080295778724));
#70296=CARTESIAN_POINT('Ctrl Pts',(87.2124470760778,57.2282687304318,13.0544229941328));
#70297=CARTESIAN_POINT('Ctrl Pts',(87.1806428354228,57.224088141927,13.0269406741497));
#70298=CARTESIAN_POINT('Ctrl Pts',(87.1795113209163,58.0179748583214,13.028265366586));
#70299=CARTESIAN_POINT('Ctrl Pts',(87.1530435317638,58.014501365673,13.0056897999309));
#70300=CARTESIAN_POINT('Ctrl Pts',(86.8879207557325,57.9783435977464,12.7588929134556));
#70301=CARTESIAN_POINT('Ctrl Pts',(86.743865944262,57.9421858298198,12.3932421316416));
#70302=CARTESIAN_POINT('Ctrl Pts',(86.7408356874277,57.9095015545417,12.0648489614637));
#70303=CARTESIAN_POINT('Ctrl Pts',(87.1806428261678,58.1885986874538,13.0269406661524));
#70304=CARTESIAN_POINT('Ctrl Pts',(87.1609641663325,58.1859593427242,13.0099361653115));
#70305=CARTESIAN_POINT('Ctrl Pts',(87.1418122557908,58.1832963391464,12.9923309966038));
#70306=CARTESIAN_POINT('Ctrl Pts',(87.0519099702601,58.1703207988888,12.9044446282297));
#70307=CARTESIAN_POINT('Ctrl Pts',(86.9890694800532,58.1597250790729,12.8265891326154));
#70308=CARTESIAN_POINT('Ctrl Pts',(86.9168429676078,58.1455276365694,12.7117659337051));
#70309=CARTESIAN_POINT('Ctrl Pts',(86.8989940863025,58.1417952157628,12.6805216162562));
#70310=CARTESIAN_POINT('Ctrl Pts',(86.8783909365337,58.1372185375922,12.6406100448996));
#70311=CARTESIAN_POINT('Ctrl Pts',(86.8743721386058,58.1363114800545,12.6326190216156));
#70312=CARTESIAN_POINT('Ctrl Pts',(86.8680566715997,58.1348632524529,12.6197236304901));
#70313=CARTESIAN_POINT('Ctrl Pts',(86.8657064771589,58.1343190035126,12.6148461182345));
#70314=CARTESIAN_POINT('Ctrl Pts',(86.8612110354625,58.133267718598,12.6053618062651));
#70315=CARTESIAN_POINT('Ctrl Pts',(86.8590621872782,58.1327604973651,12.6007570466441));
#70316=CARTESIAN_POINT('Ctrl Pts',(86.8542796468877,58.1316205956781,12.5903459450481));
#70317=CARTESIAN_POINT('Ctrl Pts',(86.8516619172355,58.1309888755473,12.5845324112614));
#70318=CARTESIAN_POINT('Ctrl Pts',(86.8424647967122,58.1287401517919,12.5636893024982));
#70319=CARTESIAN_POINT('Ctrl Pts',(86.8361325237269,58.1271367843992,12.5485512075589));
#70320=CARTESIAN_POINT('Ctrl Pts',(86.7886810831452,58.1146339648853,12.4286358554004));
#70321=CARTESIAN_POINT('Ctrl Pts',(86.7613571608766,58.1043366032532,12.3189217790707));
#70322=CARTESIAN_POINT('Ctrl Pts',(86.743632010035,58.0892456771226,12.1602880143216));
#70323=CARTESIAN_POINT('Ctrl Pts',(86.7410104748876,58.0847568795635,12.1133009844547));
#70324=CARTESIAN_POINT('Ctrl Pts',(86.740996868144,58.0788036501029,12.052040829192));
#70325=CARTESIAN_POINT('Ctrl Pts',(86.7412332481562,58.0774129161942,12.0378012425294));
#70326=CARTESIAN_POINT('Ctrl Pts',(86.7420212575764,58.0750971481515,12.0142283650332));
#70327=CARTESIAN_POINT('Ctrl Pts',(86.7424366055087,58.074176399149,12.0048914621107));
#70328=CARTESIAN_POINT('Ctrl Pts',(86.7434567202418,58.0723579862332,11.9865275074311));
#70329=CARTESIAN_POINT('Ctrl Pts',(86.7440549754702,58.071460579516,11.9775006375718));
#70330=CARTESIAN_POINT('Ctrl Pts',(86.7457249556406,58.0692957366276,11.9558164744029));
#70331=CARTESIAN_POINT('Ctrl Pts',(86.7468902189997,58.0680254580803,11.9431676809069));
#70332=CARTESIAN_POINT('Ctrl Pts',(86.7517749053325,58.0634236855104,11.8976330572363));
#70333=CARTESIAN_POINT('Ctrl Pts',(86.756589305555,58.0600588922583,11.8648817128486));
#70334=CARTESIAN_POINT('Ctrl Pts',(86.772453910004,58.0511944786744,11.7801183743937));
#70335=CARTESIAN_POINT('Ctrl Pts',(86.7854998204982,58.0456438345551,11.7285499263457));
#70336=CARTESIAN_POINT('Ctrl Pts',(86.8274903724479,58.0311843007983,11.5976941116045));
#70337=CARTESIAN_POINT('Ctrl Pts',(86.8611751512743,58.0222383138625,11.5201875718347));
#70338=CARTESIAN_POINT('Ctrl Pts',(86.9079437883526,58.0124193633623,11.4364755161873));
#70339=CARTESIAN_POINT('Ctrl Pts',(86.9137297331258,58.0112402871914,11.4264438434461));
#70340=CARTESIAN_POINT('Ctrl Pts',(86.9227432303269,58.009457928551,11.4112987498286));
#70341=CARTESIAN_POINT('Ctrl Pts',(86.9258711589752,58.0088489188173,11.406127339856));
#70342=CARTESIAN_POINT('Ctrl Pts',(86.9313757794217,58.0077937671844,11.3971715406549));
#70343=CARTESIAN_POINT('Ctrl Pts',(86.9337356165596,58.0073465974539,11.3933772111385));
#70344=CARTESIAN_POINT('Ctrl Pts',(86.9393909518938,58.0062871022269,11.3843902380527));
#70345=CARTESIAN_POINT('Ctrl Pts',(86.942704216949,58.0056759464112,11.37920895078));
#70346=CARTESIAN_POINT('Ctrl Pts',(86.952858197018,58.0038309301573,11.3635814397178));
#70347=CARTESIAN_POINT('Ctrl Pts',(86.9598157884563,58.0026043134095,11.3532113178333));
#70348=CARTESIAN_POINT('Ctrl Pts',(86.9958487821804,57.996428302522,11.3011805417272));
#70349=CARTESIAN_POINT('Ctrl Pts',(87.0272567431343,57.9916084654011,11.261182180699));
#70350=CARTESIAN_POINT('Ctrl Pts',(87.1222147346365,57.978141883981,11.1541481154597));
#70351=CARTESIAN_POINT('Ctrl Pts',(87.1907809981661,57.9696041795622,11.0920120775261));
#70352=CARTESIAN_POINT('Ctrl Pts',(87.2876959135263,57.9581433880395,11.0217371494635));
#70353=CARTESIAN_POINT('Ctrl Pts',(87.3104361379208,57.9554941484458,11.006347356427));
#70354=CARTESIAN_POINT('Ctrl Pts',(87.3429568488521,57.9517457394591,10.9858429456714));
#70355=CARTESIAN_POINT('Ctrl Pts',(87.3523338410237,57.9506694754437,10.9800995504004));
#70356=CARTESIAN_POINT('Ctrl Pts',(87.3688360722683,57.948782343433,10.9702843355352));
#70357=CARTESIAN_POINT('Ctrl Pts',(87.375928543253,57.9479734752513,10.9661583912467));
#70358=CARTESIAN_POINT('Ctrl Pts',(87.390958198284,57.9462636010808,10.9576089476924));
#70359=CARTESIAN_POINT('Ctrl Pts',(87.3989038260318,57.9453620824566,10.953201355333));
#70360=CARTESIAN_POINT('Ctrl Pts',(87.4182599298711,57.9431712081381,10.9427341729519));
#70361=CARTESIAN_POINT('Ctrl Pts',(87.4297166114248,57.941878834594,10.9367628683981));
#70362=CARTESIAN_POINT('Ctrl Pts',(87.4723077139112,57.9370883796243,10.9153839396885));
#70363=CARTESIAN_POINT('Ctrl Pts',(87.5039758057764,57.9335532532777,10.9010825882101));
#70364=CARTESIAN_POINT('Ctrl Pts',(87.5895634271671,57.92405495113,10.8665821096539));
#70365=CARTESIAN_POINT('Ctrl Pts',(87.644333837879,57.9180304225882,10.8487217945282));
#70366=CARTESIAN_POINT('Ctrl Pts',(87.7745554703628,57.9038826152027,10.8158448090695));
#70367=CARTESIAN_POINT('Ctrl Pts',(87.8505511980966,57.8957537821757,10.8038379996809));
#70368=CARTESIAN_POINT('Ctrl Pts',(87.9394594854289,57.8866215687176,10.7979568027595));
#70369=CARTESIAN_POINT('Ctrl Pts',(87.9517570443401,57.8853670215096,10.7973227722495));
#70370=CARTESIAN_POINT('Ctrl Pts',(87.9701744362412,57.883502703665,10.7966416274773));
#70371=CARTESIAN_POINT('Ctrl Pts',(87.9762879710333,57.8828862528051,10.7964597346695));
#70372=CARTESIAN_POINT('Ctrl Pts',(87.9873637270242,57.8817740447275,10.7962102734071));
#70373=CARTESIAN_POINT('Ctrl Pts',(87.9923252151887,57.8812775196486,10.7961276132986));
#70374=CARTESIAN_POINT('Ctrl Pts',(88.0036217064928,57.8801508037054,10.7960056342756));
#70375=CARTESIAN_POINT('Ctrl Pts',(88.0099566904224,57.8795216258223,10.7959846276501));
#70376=CARTESIAN_POINT('Ctrl Pts',(88.029754002933,57.8775629671159,10.7960671194802));
#70377=CARTESIAN_POINT('Ctrl Pts',(88.0432154353562,57.8762420915072,10.7963372682181));
#70378=CARTESIAN_POINT('Ctrl Pts',(88.0753857551097,57.873105788758,10.7974949073793));
#70379=CARTESIAN_POINT('Ctrl Pts',(88.0940848225632,57.8712992662735,10.7985822633269));
#70380=CARTESIAN_POINT('Ctrl Pts',(88.1682107234434,57.8641775894275,10.8045405053188));
#70381=CARTESIAN_POINT('Ctrl Pts',(88.2233200250708,57.8589694229288,10.8126378192746));
#70382=CARTESIAN_POINT('Ctrl Pts',(88.3565005736143,57.846208996109,10.841246474797));
#70383=CARTESIAN_POINT('Ctrl Pts',(88.4334745726621,57.8386726683573,10.8656233351135));
#70384=CARTESIAN_POINT('Ctrl Pts',(88.5236148066165,57.829216322951,10.9039207038179));
#70385=CARTESIAN_POINT('Ctrl Pts',(88.539473121397,57.8275282550573,10.9110461818542));
#70386=CARTESIAN_POINT('Ctrl Pts',(88.5651124000053,57.8247549217802,10.9232050474758));
#70387=CARTESIAN_POINT('Ctrl Pts',(88.5749835067088,57.8236762862583,10.9280441832448));
#70388=CARTESIAN_POINT('Ctrl Pts',(88.5926487836561,57.8217252859572,10.9369905714201));
#70389=CARTESIAN_POINT('Ctrl Pts',(88.6004655141809,57.8208545660127,10.9410520033975));
#70390=CARTESIAN_POINT('Ctrl Pts',(88.6171589828715,57.818978545179,10.9499473832506));
#70391=CARTESIAN_POINT('Ctrl Pts',(88.6260214504087,57.8179723996883,10.9548066071781));
#70392=CARTESIAN_POINT('Ctrl Pts',(88.6504021131356,57.8151753175194,10.9685553493259));
#70393=CARTESIAN_POINT('Ctrl Pts',(88.6657912235772,57.8133765580079,10.9776672414249));
#70394=CARTESIAN_POINT('Ctrl Pts',(88.6999225936818,57.8093088324409,10.9988623542658));
#70395=CARTESIAN_POINT('Ctrl Pts',(88.7185487882275,57.8070340833539,11.0111200760454));
#70396=CARTESIAN_POINT('Ctrl Pts',(88.7798653177869,57.799354787376,11.0538265292159));
#70397=CARTESIAN_POINT('Ctrl Pts',(88.8209863768143,57.7938812109666,11.0864237412434));
#70398=CARTESIAN_POINT('Ctrl Pts',(88.9236575888081,57.7793597596115,11.1787069624114));
#70399=CARTESIAN_POINT('Ctrl Pts',(88.9813974752437,57.7702681986845,11.2422497155887));
#70400=CARTESIAN_POINT('Ctrl Pts',(89.0390994169243,57.760330080863,11.3203176261556));
#70401=CARTESIAN_POINT('Ctrl Pts',(89.0457685290178,57.7591665785606,11.3296001507021));
#70402=CARTESIAN_POINT('Ctrl Pts',(89.0557532165843,57.7574029020035,11.3439010765878));
#70403=CARTESIAN_POINT('Ctrl Pts',(89.0591596966055,57.7567971728477,11.3488546907348));
#70404=CARTESIAN_POINT('Ctrl Pts',(89.0652903250764,57.7556999152783,11.3579066986006));
#70405=CARTESIAN_POINT('Ctrl Pts',(89.0680259161355,57.7552076742686,11.3619968549412));
#70406=CARTESIAN_POINT('Ctrl Pts',(89.0742824271566,57.7540756656837,11.371470052077));
#70407=CARTESIAN_POINT('Ctrl Pts',(89.077786328161,57.7534370185408,11.3768640880782));
#70408=CARTESIAN_POINT('Ctrl Pts',(89.0887826794301,57.7514168741067,11.3940771546875));
#70409=CARTESIAN_POINT('Ctrl Pts',(89.0961212788388,57.7500447680257,11.4059941791689));
#70410=CARTESIAN_POINT('Ctrl Pts',(89.1133297238051,57.7467614707615,11.4350019380987));
#70411=CARTESIAN_POINT('Ctrl Pts',(89.1230014481502,57.7448603427926,11.4522066463369));
#70412=CARTESIAN_POINT('Ctrl Pts',(89.1611440219771,57.7370923930166,11.5239208000006));
#70413=CARTESIAN_POINT('Ctrl Pts',(89.1860408894176,57.7313535011974,11.5802412803928));
#70414=CARTESIAN_POINT('Ctrl Pts',(89.2312269251569,57.7187869905285,11.7065275287635));
#70415=CARTESIAN_POINT('Ctrl Pts',(89.2497794423937,57.7119699055572,11.7768681740403));
#70416=CARTESIAN_POINT('Ctrl Pts',(89.265223803704,57.7032681522485,11.865675099231));
#70417=CARTESIAN_POINT('Ctrl Pts',(89.2678696946986,57.7015659162922,11.8830084263556));
#70418=CARTESIAN_POINT('Ctrl Pts',(89.2715949578838,57.6987741367308,11.9113321195205));
#70419=CARTESIAN_POINT('Ctrl Pts',(89.2728913664648,57.6976913750341,11.9222920966106));
#70420=CARTESIAN_POINT('Ctrl Pts',(89.274965734422,57.6957359435524,11.9420311416621));
#70421=CARTESIAN_POINT('Ctrl Pts',(89.2757954658817,57.6948649511802,11.9508041874718));
#70422=CARTESIAN_POINT('Ctrl Pts',(89.2773781971878,57.6929916887311,11.969626700734));
#70423=CARTESIAN_POINT('Ctrl Pts',(89.278103002836,57.6919885982722,11.979677834198));
#70424=CARTESIAN_POINT('Ctrl Pts',(89.2797733202122,57.689209211698,12.0074429575954));
#70425=CARTESIAN_POINT('Ctrl Pts',(89.280467371488,57.687425256254,12.0251689296196));
#70426=CARTESIAN_POINT('Ctrl Pts',(89.2811911548917,57.6833967562893,12.064959075668));
#70427=CARTESIAN_POINT('Ctrl Pts',(89.2810175744667,57.6811465977044,12.0870205909266));
#70428=CARTESIAN_POINT('Ctrl Pts',(89.2777098867373,57.6711249530162,12.184509763801));
#70429=CARTESIAN_POINT('Ctrl Pts',(89.2684289989737,57.6631891741562,12.2595644022451));
#70430=CARTESIAN_POINT('Ctrl Pts',(89.2518891570939,57.6549048247147,12.3363770794827));
#70431=CARTESIAN_POINT('Ctrl Pts',(89.2512235670153,57.6545770516432,12.3394139154327));
#70432=CARTESIAN_POINT('Ctrl Pts',(89.2369247911865,57.6476521657259,12.4035271822922));
#70433=CARTESIAN_POINT('Ctrl Pts',(89.2188047109582,57.6410708765688,12.4635253162702));
#70434=CARTESIAN_POINT('Ctrl Pts',(89.192775188052,57.6336680440243,12.5311940318788));
#70435=CARTESIAN_POINT('Ctrl Pts',(89.189111412272,57.6326619193675,12.5403960420601));
#70436=CARTESIAN_POINT('Ctrl Pts',(89.1831781482921,57.6310882645186,12.5548053101634));
#70437=CARTESIAN_POINT('Ctrl Pts',(89.1809808755076,57.6305167961573,12.5600414943702));
#70438=CARTESIAN_POINT('Ctrl Pts',(89.176772710023,57.6294435239744,12.5698841610954));
#70439=CARTESIAN_POINT('Ctrl Pts',(89.1747695724333,57.6289413293989,12.5744935038689));
#70440=CARTESIAN_POINT('Ctrl Pts',(89.1699147192715,57.6277444870236,12.5854858445216));
#70441=CARTESIAN_POINT('Ctrl Pts',(89.1670375636543,57.6270513722783,12.5918574226533));
#70442=CARTESIAN_POINT('Ctrl Pts',(89.1568422197554,57.624649370946,12.613947268851));
#70443=CARTESIAN_POINT('Ctrl Pts',(89.1492543679954,57.6229555565382,12.6295403298904));
#70444=CARTESIAN_POINT('Ctrl Pts',(89.1292329327532,57.6187008204597,12.6686287660051));
#70445=CARTESIAN_POINT('Ctrl Pts',(89.1163763078725,57.6161596508093,12.6918991995914));
#70446=CARTESIAN_POINT('Ctrl Pts',(89.0735902903707,57.6082124201461,12.763904737886));
#70447=CARTESIAN_POINT('Ctrl Pts',(89.0410952260603,57.602882921433,12.8110327169208));
#70448=CARTESIAN_POINT('Ctrl Pts',(88.9609866886082,57.5908046467616,12.9119054658519));
#70449=CARTESIAN_POINT('Ctrl Pts',(88.9117825183258,57.5840554810671,12.9641196130535));
#70450=CARTESIAN_POINT('Ctrl Pts',(88.8465890670682,57.5755692650659,13.0225272521232));
#70451=CARTESIAN_POINT('Ctrl Pts',(88.8345330716084,57.5740174217952,13.0329264184839));
#70452=CARTESIAN_POINT('Ctrl Pts',(88.8148251008043,57.5715054941576,13.0492900047145));
#70453=CARTESIAN_POINT('Ctrl Pts',(88.8072943459043,57.5705512955222,13.0553984676414));
#70454=CARTESIAN_POINT('Ctrl Pts',(88.7927285468054,57.5687158012079,13.0669392935383));
#70455=CARTESIAN_POINT('Ctrl Pts',(88.7857049368417,57.5678351130327,13.0723852348146));
#70456=CARTESIAN_POINT('Ctrl Pts',(88.7692927481366,57.5657867585359,13.0848372444535));
#70457=CARTESIAN_POINT('Ctrl Pts',(88.7598634212971,57.5646170214461,13.0917878801957));
#70458=CARTESIAN_POINT('Ctrl Pts',(88.7287948848014,57.5607844395237,13.1140327487044));
#70459=CARTESIAN_POINT('Ctrl Pts',(88.7067747408981,57.5581013777191,13.1287790841729));
#70460=CARTESIAN_POINT('Ctrl Pts',(88.6520895745806,57.5515102232162,13.1629723535767));
#70461=CARTESIAN_POINT('Ctrl Pts',(88.6189833787897,57.5475791426713,13.1816611231888));
#70462=CARTESIAN_POINT('Ctrl Pts',(88.5415196299343,57.5385138527237,13.2209178205029));
#70463=CARTESIAN_POINT('Ctrl Pts',(88.496711051912,57.5333630607269,13.2404660268192));
#70464=CARTESIAN_POINT('Ctrl Pts',(88.3922444390325,57.5216235072372,13.2790379285733));
#70465=CARTESIAN_POINT('Ctrl Pts',(88.3320695773349,57.5150490037439,13.2963353467067));
#70466=CARTESIAN_POINT('Ctrl Pts',(88.2611647219359,57.5076528329458,13.3111568782726));
#70467=CARTESIAN_POINT('Ctrl Pts',(88.2514487980308,57.5066469309627,13.3130695398332));
#70468=CARTESIAN_POINT('Ctrl Pts',(88.2361276606362,57.5050735464429,13.3158999053919));
#70469=CARTESIAN_POINT('Ctrl Pts',(88.2305373063819,57.5045021278631,13.3168939254882));
#70470=CARTESIAN_POINT('Ctrl Pts',(88.2199861028671,57.5034288918468,13.3186971180063));
#70471=CARTESIAN_POINT('Ctrl Pts',(88.2150270555444,57.5029266840923,13.3195143490282));
#70472=CARTESIAN_POINT('Ctrl Pts',(88.2031577874327,57.5017297331929,13.3213980514166));
#70473=CARTESIAN_POINT('Ctrl Pts',(88.1962433597143,57.5010365238713,13.3224369418294));
#70474=CARTESIAN_POINT('Ctrl Pts',(88.1721480599071,57.4986338122654,13.3258540086255));
#70475=CARTESIAN_POINT('Ctrl Pts',(88.1549260805346,57.4969393940372,13.3279374831467));
#70476=CARTESIAN_POINT('Ctrl Pts',(88.1112074005929,57.492682749731,13.3323196794481));
#70477=CARTESIAN_POINT('Ctrl Pts',(88.0846701814,57.4901402982706,13.3341403814033));
#70478=CARTESIAN_POINT('Ctrl Pts',(88.0012457782746,57.4822193999283,13.3372359749553));
#70479=CARTESIAN_POINT('Ctrl Pts',(87.9443178354556,57.4769164838844,13.3355236530341));
#70480=CARTESIAN_POINT('Ctrl Pts',(87.8161855663503,57.4648454525446,13.3230240240987));
#70481=CARTESIAN_POINT('Ctrl Pts',(87.7454105763784,57.4580766105689,13.3099941814995));
#70482=CARTESIAN_POINT('Ctrl Pts',(87.6607421340787,57.4495670288067,13.2868495923758));
#70483=CARTESIAN_POINT('Ctrl Pts',(87.6454411304861,57.4480126989241,13.2823556051771));
#70484=CARTESIAN_POINT('Ctrl Pts',(87.6209737679506,57.4454977360607,13.2746660706407));
#70485=CARTESIAN_POINT('Ctrl Pts',(87.6117519052563,57.4445430150088,13.2716513085726));
#70486=CARTESIAN_POINT('Ctrl Pts',(87.5941518556165,57.4427071675272,13.2656735330011));
#70487=CARTESIAN_POINT('Ctrl Pts',(87.5857684126008,57.4418266535634,13.2627276415808));
#70488=CARTESIAN_POINT('Ctrl Pts',(87.5772575048634,57.4409263455922,13.259636241344));
#70489=CARTESIAN_POINT('Ctrl Pts',(87.5770981816909,57.440909489639,13.259578334591));
#70490=CARTESIAN_POINT('Ctrl Pts',(87.5767956332609,57.4408774764845,13.2594683033642));
#70491=CARTESIAN_POINT('Ctrl Pts',(87.5766524056898,57.4408623194786,13.2594161849696));
#70492=CARTESIAN_POINT('Ctrl Pts',(87.57638033461,57.4408335241245,13.2593171268612));
#70493=CARTESIAN_POINT('Ctrl Pts',(87.5762514893518,57.4408198859451,13.2592701920743));
#70494=CARTESIAN_POINT('Ctrl Pts',(87.5760066664193,57.4407939687505,13.2591809648917));
#70495=CARTESIAN_POINT('Ctrl Pts',(87.5758906873032,57.440781689868,13.2591386764513));
#70496=CARTESIAN_POINT('Ctrl Pts',(87.5756702524212,57.4407583497771,13.2590582648125));
#70497=CARTESIAN_POINT('Ctrl Pts',(87.5755657954311,57.4407472886694,13.2590201447821));
#70498=CARTESIAN_POINT('Ctrl Pts',(87.5753672109313,57.4407262583743,13.2589476447566));
#70499=CARTESIAN_POINT('Ctrl Pts',(87.5752730825234,57.440716289278,13.2589132673536));
#70500=CARTESIAN_POINT('Ctrl Pts',(87.575094093768,57.4406973311302,13.2588478734002));
#70501=CARTESIAN_POINT('Ctrl Pts',(87.5750092326021,57.4406883421427,13.258816858913));
#70502=CARTESIAN_POINT('Ctrl Pts',(87.5748478326266,57.4406712444747,13.2587578520124));
#70503=CARTESIAN_POINT('Ctrl Pts',(87.574771293269,57.4406631358582,13.2587298613121));
#70504=CARTESIAN_POINT('Ctrl Pts',(87.574496330622,57.4406340042679,13.2586292765404));
#70505=CARTESIAN_POINT('Ctrl Pts',(87.5742979228688,57.4406129798909,13.2585566403617));
#70506=CARTESIAN_POINT('Ctrl Pts',(87.5636491170005,57.4394843814052,13.2546551469838));
#70507=CARTESIAN_POINT('Ctrl Pts',(87.5532499223203,57.4383722819139,13.2506892913613));
#70508=CARTESIAN_POINT('Ctrl Pts',(87.517424244737,57.4345051807202,13.2364846386856));
#70509=CARTESIAN_POINT('Ctrl Pts',(87.4922802822394,57.4317277149054,13.22556063883));
#70510=CARTESIAN_POINT('Ctrl Pts',(87.431207635568,57.4248152953361,13.1966433054023));
#70511=CARTESIAN_POINT('Ctrl Pts',(87.3957440674988,57.4206537988001,13.1777431587578));
#70512=CARTESIAN_POINT('Ctrl Pts',(87.320714236362,57.4115244271141,13.1330661438628));
#70513=CARTESIAN_POINT('Ctrl Pts',(87.2815667956405,57.4065487390504,13.1066975254403));
#70514=CARTESIAN_POINT('Ctrl Pts',(87.2223183995014,57.3987132783415,13.0618011373154));
#70515=CARTESIAN_POINT('Ctrl Pts',(87.2011957666037,57.3958534395397,13.0447006424742));
#70516=CARTESIAN_POINT('Ctrl Pts',(87.1806427720391,57.39301128552,13.0269406193793));
#70517=CARTESIAN_POINT('Origin',(88.011,66.41344859951,12.066));
#70518=CARTESIAN_POINT('',(87.1806428354357,56.4292380444866,13.0269406741609));
#70519=CARTESIAN_POINT('',(87.1801902653375,56.5998778161658,13.027459163232));
#70520=CARTESIAN_POINT('',(87.1806428354228,66.41344859951,13.0269406741497));
#70521=CARTESIAN_POINT('',(86.7410001292204,57.11575140049,12.0665729046198));
#70522=CARTESIAN_POINT('Ctrl Pts',(87.1806428354357,56.4292380444866,13.0269406741609));
#70523=CARTESIAN_POINT('Ctrl Pts',(87.1815511872673,56.4293562257376,13.0277255888508));
#70524=CARTESIAN_POINT('Ctrl Pts',(87.1824606515523,56.4294744595993,13.02850921516));
#70525=CARTESIAN_POINT('Ctrl Pts',(87.1900528136169,56.4304607079242,13.0350321539109));
#70526=CARTESIAN_POINT('Ctrl Pts',(87.1967937305493,56.4313314643143,13.0407028978344));
#70527=CARTESIAN_POINT('Ctrl Pts',(87.2114100591946,56.4332095500112,13.0527413484288));
#70528=CARTESIAN_POINT('Ctrl Pts',(87.2193036744075,56.4342177386951,13.0590858346253));
#70529=CARTESIAN_POINT('Ctrl Pts',(87.2414157120846,56.4370260473583,13.0764271888448));
#70530=CARTESIAN_POINT('Ctrl Pts',(87.2557923142829,56.4388340924591,13.0872170908351));
#70531=CARTESIAN_POINT('Ctrl Pts',(87.28862355028,56.4429263515667,13.1107851134188));
#70532=CARTESIAN_POINT('Ctrl Pts',(87.3071972126167,56.4452164544235,13.1233859979102));
#70533=CARTESIAN_POINT('Ctrl Pts',(87.3707427042797,56.452972877426,13.1640809353309));
#70534=CARTESIAN_POINT('Ctrl Pts',(87.417132463637,56.4585097847843,13.1898465303408));
#70535=CARTESIAN_POINT('Ctrl Pts',(87.5413048325652,56.4729796596785,13.2489754893543));
#70536=CARTESIAN_POINT('Ctrl Pts',(87.6210640173552,56.4819508507898,13.2776094421537));
#70537=CARTESIAN_POINT('Ctrl Pts',(87.7142942650251,56.4917905927181,13.3009085854228));
#70538=CARTESIAN_POINT('Ctrl Pts',(87.7255424902289,56.4929671037451,13.3035570902417));
#70539=CARTESIAN_POINT('Ctrl Pts',(87.7427225727965,56.4947464615107,13.3073555861693));
#70540=CARTESIAN_POINT('Ctrl Pts',(87.7486285925255,56.4953550064515,13.3086172859344));
#70541=CARTESIAN_POINT('Ctrl Pts',(87.7589211146403,56.4964098185702,13.3107394155931));
#70542=CARTESIAN_POINT('Ctrl Pts',(87.763303331121,56.4968571092307,13.3116188580882));
#70543=CARTESIAN_POINT('Ctrl Pts',(87.7737338532045,56.4979174911731,13.3136548765408));
#70544=CARTESIAN_POINT('Ctrl Pts',(87.7797860715061,56.4985294073228,13.3147906311591));
#70545=CARTESIAN_POINT('Ctrl Pts',(87.798170789801,56.5003787364104,13.3181024491282));
#70546=CARTESIAN_POINT('Ctrl Pts',(87.8105280501107,56.5016088575653,13.3201402857987));
#70547=CARTESIAN_POINT('Ctrl Pts',(87.8734755865306,56.5078195991908,13.3295667018586));
#70548=CARTESIAN_POINT('Ctrl Pts',(87.9244566752159,56.5126690358122,13.3340795605586));
#70549=CARTESIAN_POINT('Ctrl Pts',(88.068776159048,56.5262552720969,13.338106285534));
#70550=CARTESIAN_POINT('Ctrl Pts',(88.161968475598,56.5348821836411,13.3304364123718));
#70551=CARTESIAN_POINT('Ctrl Pts',(88.2795181168433,56.5463561243396,13.3075722809627));
#70552=CARTESIAN_POINT('Ctrl Pts',(88.3053902625239,56.5489176527014,13.3016932675965));
#70553=CARTESIAN_POINT('Ctrl Pts',(88.3415556306588,56.5525624846962,13.2922751172882));
#70554=CARTESIAN_POINT('Ctrl Pts',(88.3520180386733,56.5536245666161,13.2894068693012));
#70555=CARTESIAN_POINT('Ctrl Pts',(88.3710805309575,56.5555746554578,13.2839174123201));
#70556=CARTESIAN_POINT('Ctrl Pts',(88.3796920879425,56.5564612599687,13.2813382022595));
#70557=CARTESIAN_POINT('Ctrl Pts',(88.3971399866615,56.5582696339004,13.2759099553706));
#70558=CARTESIAN_POINT('Ctrl Pts',(88.4059738930652,56.5591915467965,13.273055011795));
#70559=CARTESIAN_POINT('Ctrl Pts',(88.427980633579,56.5615046675162,13.2656754300987));
#70560=CARTESIAN_POINT('Ctrl Pts',(88.4411114200283,56.5628997414632,13.2610305908167));
#70561=CARTESIAN_POINT('Ctrl Pts',(88.4950705603822,56.5686972339007,13.2409387988065));
#70562=CARTESIAN_POINT('Ctrl Pts',(88.5351594801019,56.5731604493787,13.2236101231282));
#70563=CARTESIAN_POINT('Ctrl Pts',(88.6550509179425,56.5870181018942,13.1642812294383));
#70564=CARTESIAN_POINT('Ctrl Pts',(88.7313401164117,56.5965839800609,13.1158237683423));
#70565=CARTESIAN_POINT('Ctrl Pts',(88.8316699345391,56.6100211258957,13.0359760959231));
#70566=CARTESIAN_POINT('Ctrl Pts',(88.8604138833674,56.6139832281062,13.0109072124338));
#70567=CARTESIAN_POINT('Ctrl Pts',(88.8947441243965,56.6188233342398,12.9781313070374));
#70568=CARTESIAN_POINT('Ctrl Pts',(88.9014272748383,56.619770959051,12.9716083511424));
#70569=CARTESIAN_POINT('Ctrl Pts',(88.9119317794159,56.6212682881089,12.9611269083194));
#70570=CARTESIAN_POINT('Ctrl Pts',(88.9158001990069,56.6218214336459,12.9572165041569));
#70571=CARTESIAN_POINT('Ctrl Pts',(88.9232033273231,56.6228831691662,12.949635137332));
#70572=CARTESIAN_POINT('Ctrl Pts',(88.9267414104244,56.6233919845579,12.9459679753269));
#70573=CARTESIAN_POINT('Ctrl Pts',(88.9353709620412,56.6246367395389,12.936915177881));
#70574=CARTESIAN_POINT('Ctrl Pts',(88.94043759056,56.625370810856,12.9315060355751));
#70575=CARTESIAN_POINT('Ctrl Pts',(88.9591665802194,56.6280980695201,12.9111567782944));
#70576=CARTESIAN_POINT('Ctrl Pts',(88.9725196154335,56.6300702256156,12.8959337553049));
#70577=CARTESIAN_POINT('Ctrl Pts',(89.0068866129423,56.6352432759506,12.854810312601));
#70578=CARTESIAN_POINT('Ctrl Pts',(89.0272552931815,56.6384118770012,12.8283893311679));
#70579=CARTESIAN_POINT('Ctrl Pts',(89.1129641916995,56.6523823990047,12.7076636042831));
#70580=CARTESIAN_POINT('Ctrl Pts',(89.1663826697847,56.6629334106132,12.6055791584121));
#70581=CARTESIAN_POINT('Ctrl Pts',(89.2113684280754,56.6757324723813,12.4811227602697));
#70582=CARTESIAN_POINT('Ctrl Pts',(89.2170190434689,56.6774487608568,12.4644084126889));
#70583=CARTESIAN_POINT('Ctrl Pts',(89.2253718145597,56.680171217308,12.4378928704803));
#70584=CARTESIAN_POINT('Ctrl Pts',(89.2283077698893,56.6811697417268,12.4281670742206));
#70585=CARTESIAN_POINT('Ctrl Pts',(89.2335701637644,56.6830409375251,12.4099472921285));
#70586=CARTESIAN_POINT('Ctrl Pts',(89.2359255607343,56.6839126104301,12.4014622271366));
#70587=CARTESIAN_POINT('Ctrl Pts',(89.2410055301142,56.6858724356546,12.3823949965554));
#70588=CARTESIAN_POINT('Ctrl Pts',(89.243682101606,56.686962063142,12.3718009404115));
#70589=CARTESIAN_POINT('Ctrl Pts',(89.2513401418302,56.6902613880028,12.3397541697793));
#70590=CARTESIAN_POINT('Ctrl Pts',(89.2559002857052,56.6924842041352,12.3182065353659));
#70591=CARTESIAN_POINT('Ctrl Pts',(89.277099381309,56.7043641161924,12.2033717274388));
#70592=CARTESIAN_POINT('Ctrl Pts',(89.283814830232,56.7143213038455,12.1085783189939));
#70593=CARTESIAN_POINT('Ctrl Pts',(89.2774131806424,56.7307848237239,11.9525263008568));
#70594=CARTESIAN_POINT('Ctrl Pts',(89.2704373403079,56.7372463275319,11.8913616833031));
#70595=CARTESIAN_POINT('Ctrl Pts',(89.2572077847251,56.7445439320123,11.8211206657119));
#70596=CARTESIAN_POINT('Ctrl Pts',(89.2552435678475,56.7455583684757,11.8113282552207));
#70597=CARTESIAN_POINT('Ctrl Pts',(89.2519895677624,56.7471362590663,11.7960431482084));
#70598=CARTESIAN_POINT('Ctrl Pts',(89.2507784352414,56.747703784987,11.7905344936574));
#70599=CARTESIAN_POINT('Ctrl Pts',(89.2484157682736,56.7487744064457,11.7801195884816));
#70600=CARTESIAN_POINT('Ctrl Pts',(89.2472717218303,56.749277857102,11.7752120617999));
#70601=CARTESIAN_POINT('Ctrl Pts',(89.2444513814456,56.7504841602544,11.7634314403725));
#70602=CARTESIAN_POINT('Ctrl Pts',(89.2427468109817,56.7511854139932,11.7565652800296));
#70603=CARTESIAN_POINT('Ctrl Pts',(89.2365318593605,56.7536486317145,11.7323963864265));
#70604=CARTESIAN_POINT('Ctrl Pts',(89.2317132139794,56.7553944840277,11.7151737242088));
#70605=CARTESIAN_POINT('Ctrl Pts',(89.2221507136994,56.7585898176861,11.683583163453));
#70606=CARTESIAN_POINT('Ctrl Pts',(89.2175110253315,56.7600431603729,11.669187842766));
#70607=CARTESIAN_POINT('Ctrl Pts',(89.1916654882579,56.7676732158,11.5936472835332));
#70608=CARTESIAN_POINT('Ctrl Pts',(89.1660643855557,56.7737036474884,11.5341015580417));
#70609=CARTESIAN_POINT('Ctrl Pts',(89.1041244740852,56.7862162170744,11.4158395538987));
#70610=CARTESIAN_POINT('Ctrl Pts',(89.0673251822746,56.7926839817483,11.3576183468105));
#70611=CARTESIAN_POINT('Ctrl Pts',(89.0155538552522,56.8010007094916,11.2887783067108));
#70612=CARTESIAN_POINT('Ctrl Pts',(89.0048252187677,56.80268816811,11.2751059649097));
#70613=CARTESIAN_POINT('Ctrl Pts',(88.9868578765319,56.8054608260815,11.2531517693297));
#70614=CARTESIAN_POINT('Ctrl Pts',(88.979785829117,56.8065394030033,11.2447358281463));
#70615=CARTESIAN_POINT('Ctrl Pts',(88.9668504630952,56.8084905100742,11.2297419545109));
#70616=CARTESIAN_POINT('Ctrl Pts',(88.9610261505693,56.8093613969358,11.2231311313195));
#70617=CARTESIAN_POINT('Ctrl Pts',(88.9483707781329,56.8112380190129,11.2090646071677));
#70618=CARTESIAN_POINT('Ctrl Pts',(88.9415185688234,56.8122446009229,11.2016288869434));
#70619=CARTESIAN_POINT('Ctrl Pts',(88.922293351752,56.8150435859577,11.1812600555145));
#70620=CARTESIAN_POINT('Ctrl Pts',(88.9097352072485,56.8168438273645,11.1685061082928));
#70621=CARTESIAN_POINT('Ctrl Pts',(88.8809212502997,56.8209153706759,11.1404541520472));
#70622=CARTESIAN_POINT('Ctrl Pts',(88.8645236180995,56.82319247096,11.1253112215245));
#70623=CARTESIAN_POINT('Ctrl Pts',(88.808229237616,56.8308831827854,11.0760082731423));
#70624=CARTESIAN_POINT('Ctrl Pts',(88.7666189437846,56.8363660484672,11.0438959697772));
#70625=CARTESIAN_POINT('Ctrl Pts',(88.6523829906287,56.8508794034788,10.9665310282105));
#70626=CARTESIAN_POINT('Ctrl Pts',(88.576956394807,56.8599527445137,10.9258682105593));
#70627=CARTESIAN_POINT('Ctrl Pts',(88.4874361105472,56.8698760798227,10.8886981260928));
#70628=CARTESIAN_POINT('Ctrl Pts',(88.47680319907,56.8710416412169,10.8844508124563));
#70629=CARTESIAN_POINT('Ctrl Pts',(88.4604967090254,56.872807863575,10.87819155285));
#70630=CARTESIAN_POINT('Ctrl Pts',(88.4548643135275,56.8734141015865,10.8760753489535));
#70631=CARTESIAN_POINT('Ctrl Pts',(88.4445976881036,56.8745119476096,10.8723010155149));
#70632=CARTESIAN_POINT('Ctrl Pts',(88.4399687211188,56.8750042716023,10.8706297395365));
#70633=CARTESIAN_POINT('Ctrl Pts',(88.4292705109998,56.8761360654688,10.8668373300499));
#70634=CARTESIAN_POINT('Ctrl Pts',(88.4231947097598,56.8767744179401,10.8647353092673));
#70635=CARTESIAN_POINT('Ctrl Pts',(88.4038644024565,56.8787921894322,10.8582116152764));
#70636=CARTESIAN_POINT('Ctrl Pts',(88.3905520089413,56.8801622498778,10.853962231432));
#70637=CARTESIAN_POINT('Ctrl Pts',(88.3583164420102,56.8834395398326,10.8442557455046));
#70638=CARTESIAN_POINT('Ctrl Pts',(88.3393306429984,56.8853367562984,10.8390171761421));
#70639=CARTESIAN_POINT('Ctrl Pts',(88.2608402413683,56.8930763748795,10.8193127169733));
#70640=CARTESIAN_POINT('Ctrl Pts',(88.2004448760899,56.8987918110998,10.8087166378623));
#70641=CARTESIAN_POINT('Ctrl Pts',(88.0668823765914,56.9113697479765,10.7951312845081));
#70642=CARTESIAN_POINT('Ctrl Pts',(87.9937585890848,56.9182218578444,10.7940210878684));
#70643=CARTESIAN_POINT('Ctrl Pts',(87.9034902106471,56.9269583025082,10.8004376383025));
#70644=CARTESIAN_POINT('Ctrl Pts',(87.8860572339359,56.9286578986099,10.8020396835717));
#70645=CARTESIAN_POINT('Ctrl Pts',(87.8577038196236,56.9314463602381,10.8052375590161));
#70646=CARTESIAN_POINT('Ctrl Pts',(87.8467607381644,56.9325284732268,10.8066163818838));
#70647=CARTESIAN_POINT('Ctrl Pts',(87.8271082537827,56.9344833750762,10.809353072017));
#70648=CARTESIAN_POINT('Ctrl Pts',(87.8183922627767,56.9353544927229,10.8106594383987));
#70649=CARTESIAN_POINT('Ctrl Pts',(87.7997326026262,56.937228737766,10.8136550757421));
#70650=CARTESIAN_POINT('Ctrl Pts',(87.7897941322235,56.93823269103,10.8153722890039));
#70651=CARTESIAN_POINT('Ctrl Pts',(87.7624008597505,56.9410164452931,10.820442147622));
#70652=CARTESIAN_POINT('Ctrl Pts',(87.7449951996424,56.9428039436267,10.8240429716981));
#70653=CARTESIAN_POINT('Ctrl Pts',(87.7159670845498,56.9458184727898,10.8306863726074));
#70654=CARTESIAN_POINT('Ctrl Pts',(87.7043013317597,56.9470390898627,10.8335309003409));
#70655=CARTESIAN_POINT('Ctrl Pts',(87.6738372558035,56.9502512670543,10.8414184145493));
#70656=CARTESIAN_POINT('Ctrl Pts',(87.6551122308213,56.9522504976668,10.846728670482));
#70657=CARTESIAN_POINT('Ctrl Pts',(87.5661396781767,56.9618711431419,10.87418456361));
#70658=CARTESIAN_POINT('Ctrl Pts',(87.497792659662,56.9696388136903,10.9019810114289));
#70659=CARTESIAN_POINT('Ctrl Pts',(87.380654283355,56.9835060490229,10.9619510911352));
#70660=CARTESIAN_POINT('Ctrl Pts',(87.3309203679017,56.9895902603073,10.9918708256271));
#70661=CARTESIAN_POINT('Ctrl Pts',(87.2752451129141,56.9965266414844,11.0307880888301));
#70662=CARTESIAN_POINT('Ctrl Pts',(87.2671586809928,56.9975372967341,11.0365831411089));
#70663=CARTESIAN_POINT('Ctrl Pts',(87.2545559664893,56.9991165231332,11.0458408032338));
#70664=CARTESIAN_POINT('Ctrl Pts',(87.2499937151712,56.9996890753513,11.0492395554058));
#70665=CARTESIAN_POINT('Ctrl Pts',(87.241573299093,57.0007472135728,11.0556009646502));
#70666=CARTESIAN_POINT('Ctrl Pts',(87.2377092603258,57.0012333071786,11.0585551665479));
#70667=CARTESIAN_POINT('Ctrl Pts',(87.2337880173248,57.0017272171201,11.0615889572738));
#70668=CARTESIAN_POINT('Ctrl Pts',(87.2337139793801,57.0017365429841,11.0616462521038));
#70669=CARTESIAN_POINT('Ctrl Pts',(87.2335669763132,57.0017550600373,11.0617600375427));
#70670=CARTESIAN_POINT('Ctrl Pts',(87.233494010923,57.0017642512537,11.0618165279868));
#70671=CARTESIAN_POINT('Ctrl Pts',(87.2333490519652,57.0017825117164,11.0619287817524));
#70672=CARTESIAN_POINT('Ctrl Pts',(87.23327705826,57.0017915809741,11.0619845448481));
#70673=CARTESIAN_POINT('Ctrl Pts',(87.2331339478638,57.0018096094471,11.0620954163724));
#70674=CARTESIAN_POINT('Ctrl Pts',(87.2330628309948,57.0018185686795,11.0621505246429));
#70675=CARTESIAN_POINT('Ctrl Pts',(87.2329213841737,57.001836388438,11.0622601554622));
#70676=CARTESIAN_POINT('Ctrl Pts',(87.2328510542875,57.0018452489512,11.0623146776975));
#70677=CARTESIAN_POINT('Ctrl Pts',(87.2327110965624,57.0018628819512,11.0624232014688));
#70678=CARTESIAN_POINT('Ctrl Pts',(87.2326414686106,57.0018716544482,11.0624772028611));
#70679=CARTESIAN_POINT('Ctrl Pts',(87.2325028341706,57.0018891215579,11.0625847467652));
#70680=CARTESIAN_POINT('Ctrl Pts',(87.2324338274016,57.0018978162023,11.0626382892923));
#70681=CARTESIAN_POINT('Ctrl Pts',(87.2322963576771,57.0019151373814,11.0627449751213));
#70682=CARTESIAN_POINT('Ctrl Pts',(87.2322278947359,57.0019237639109,11.0627981182365));
#70683=CARTESIAN_POINT('Ctrl Pts',(87.2320914388658,57.0019409581515,11.0629040620147));
#70684=CARTESIAN_POINT('Ctrl Pts',(87.2320234458504,57.0019495258705,11.0629568625945));
#70685=CARTESIAN_POINT('Ctrl Pts',(87.2318878586206,57.0019666114566,11.0630621761636));
#70686=CARTESIAN_POINT('Ctrl Pts',(87.2318202644013,57.001975129322,11.0631146890302));
#70687=CARTESIAN_POINT('Ctrl Pts',(87.231685406248,57.0019921238291,11.0632194800344));
#70688=CARTESIAN_POINT('Ctrl Pts',(87.2316181422467,57.0020006004775,11.0632717581207));
#70689=CARTESIAN_POINT('Ctrl Pts',(87.2262199904002,57.0026808945831,11.0674681135403));
#70690=CARTESIAN_POINT('Ctrl Pts',(87.2209220133654,57.0033498074512,11.0716548012747));
#70691=CARTESIAN_POINT('Ctrl Pts',(87.2091727749076,57.0048367223819,11.0810927524063));
#70692=CARTESIAN_POINT('Ctrl Pts',(87.2027391198258,57.0056533074955,11.0863656052262));
#70693=CARTESIAN_POINT('Ctrl Pts',(87.1845444142284,57.0079711291973,11.1015787887414));
#70694=CARTESIAN_POINT('Ctrl Pts',(87.1729111597567,57.0094633622371,11.1116707744877));
#70695=CARTESIAN_POINT('Ctrl Pts',(87.132071215514,57.0147521969192,11.1484229071398));
#70696=CARTESIAN_POINT('Ctrl Pts',(87.1039270099763,57.0184914708578,11.1762344201138));
#70697=CARTESIAN_POINT('Ctrl Pts',(87.0096790725315,57.0315680303241,11.2784972559531));
#70698=CARTESIAN_POINT('Ctrl Pts',(86.9510769971634,57.0407763206326,11.3593425295514));
#70699=CARTESIAN_POINT('Ctrl Pts',(86.8922110294999,57.0523963269993,11.4646208053566));
#70700=CARTESIAN_POINT('Ctrl Pts',(86.8823696485452,57.054443771096,11.4833001588955));
#70701=CARTESIAN_POINT('Ctrl Pts',(86.8681652021713,57.0575717417811,11.5119718515118));
#70702=CARTESIAN_POINT('Ctrl Pts',(86.8634572903073,57.0586403185192,11.5217902281683));
#70703=CARTESIAN_POINT('Ctrl Pts',(86.8551724281082,57.0605807851163,11.5396539860567));
#70704=CARTESIAN_POINT('Ctrl Pts',(86.8515517395434,57.0614511107281,11.5476784552092));
#70705=CARTESIAN_POINT('Ctrl Pts',(86.8439215543373,57.0633349035371,11.5650691697909));
#70706=CARTESIAN_POINT('Ctrl Pts',(86.8399407961342,57.0643492786296,11.5744472352828));
#70707=CARTESIAN_POINT('Ctrl Pts',(86.8291378979728,57.0671935874465,11.6007734547568));
#70708=CARTESIAN_POINT('Ctrl Pts',(86.8225683495071,57.0690317855879,11.6178215873962));
#70709=CARTESIAN_POINT('Ctrl Pts',(86.8085890649151,57.0732043169257,11.6565692746366));
#70710=CARTESIAN_POINT('Ctrl Pts',(86.8013949242058,57.0755448968069,11.6783391039054));
#70711=CARTESIAN_POINT('Ctrl Pts',(86.7590701631882,57.0906623334501,11.8190943868847));
#70712=CARTESIAN_POINT('Ctrl Pts',(86.7409544477374,57.1039345767614,11.9424578425332));
#70713=CARTESIAN_POINT('Ctrl Pts',(86.7410000860046,57.1167707803686,12.0664673881771));
#70714=CARTESIAN_POINT('Ctrl Pts',(87.1806428354228,57.224088141927,13.0269406741497));
#70715=CARTESIAN_POINT('Ctrl Pts',(87.1431026657818,57.219153579792,12.994501888219));
#70716=CARTESIAN_POINT('Ctrl Pts',(87.1074198120016,57.214219017657,12.9598198990021));
#70717=CARTESIAN_POINT('Ctrl Pts',(87.073869362273,57.209284455522,12.9231383597958));
#70718=CARTESIAN_POINT('Ctrl Pts',(87.04034089956,57.2043531272124,12.886480859539));
#70719=CARTESIAN_POINT('Ctrl Pts',(87.0089424419052,57.1994217989027,12.8478268082961));
#70720=CARTESIAN_POINT('Ctrl Pts',(86.9799121855865,57.1944904705931,12.8074566197479));
#70721=CARTESIAN_POINT('Ctrl Pts',(86.9508886015368,57.1895602756922,12.7670957098211));
#70722=CARTESIAN_POINT('Ctrl Pts',(86.924232458129,57.1846300807914,12.725019890116));
#70723=CARTESIAN_POINT('Ctrl Pts',(86.900140007665,57.1796998858906,12.6815404758661));
#70724=CARTESIAN_POINT('Ctrl Pts',(86.8760251392384,57.1747651034563,12.6380206041341));
#70725=CARTESIAN_POINT('Ctrl Pts',(86.8544789949268,57.1698303210219,12.593095009375));
#70726=CARTESIAN_POINT('Ctrl Pts',(86.8356520955675,57.1648955385875,12.547100097221));
#70727=CARTESIAN_POINT('Ctrl Pts',(86.8168161701501,57.1599583903025,12.5010831340251));
#70728=CARTESIAN_POINT('Ctrl Pts',(86.8007022656137,57.1550212420174,12.4539963510136));
#70729=CARTESIAN_POINT('Ctrl Pts',(86.7874116183649,57.1500840937324,12.4061932867174));
#70730=CARTESIAN_POINT('Ctrl Pts',(86.7740954976792,57.1451374826926,12.3582986009734));
#70731=CARTESIAN_POINT('Ctrl Pts',(86.763613555933,57.1401908716528,12.3096854290717));
#70732=CARTESIAN_POINT('Ctrl Pts',(86.7560159808755,57.135244260613,12.2607180313741));
#70733=CARTESIAN_POINT('Ctrl Pts',(86.7510039867034,57.1319810634065,12.2284150518008));
#70734=CARTESIAN_POINT('Ctrl Pts',(86.7472461472918,57.1287178662,12.1959580826879));
#70735=CARTESIAN_POINT('Ctrl Pts',(86.7447444544907,57.1254546689935,12.1634520059662));
#70736=CARTESIAN_POINT('Ctrl Pts',(86.7422648212326,57.122220246159,12.1312325628387));
#70737=CARTESIAN_POINT('Ctrl Pts',(86.741014719967,57.1189858233245,12.0989172875295));
#70738=CARTESIAN_POINT('Ctrl Pts',(86.7410001292204,57.11575140049,12.0665729046198));
#70739=CARTESIAN_POINT('',(86.741302287513,57.2853233247604,12.0648429798974));
#70740=CARTESIAN_POINT('Ctrl Pts',(87.1806427720391,57.39301128552,13.0269406193793));
#70741=CARTESIAN_POINT('Ctrl Pts',(87.1553383036075,57.3895120778282,13.0050748059897));
#70742=CARTESIAN_POINT('Ctrl Pts',(87.130897297411,57.3860395939098,12.9822092877968));
#70743=CARTESIAN_POINT('Ctrl Pts',(87.1003752687152,57.3816048880979,12.951303306484));
#70744=CARTESIAN_POINT('Ctrl Pts',(87.0934548898731,57.380592441693,12.9441288852476));
#70745=CARTESIAN_POINT('Ctrl Pts',(87.0827551723581,57.3790170195409,12.932771766008));
#70746=CARTESIAN_POINT('Ctrl Pts',(87.0789182319904,57.3784499909106,12.9286443859873));
#70747=CARTESIAN_POINT('Ctrl Pts',(87.071702328246,57.3773798609861,12.9207779115088));
#70748=CARTESIAN_POINT('Ctrl Pts',(87.0683181018931,57.3768764080165,12.9170442027784));
#70749=CARTESIAN_POINT('Ctrl Pts',(87.0615779363064,57.3758703508852,12.9095184541659));
#70750=CARTESIAN_POINT('Ctrl Pts',(87.0582223626842,57.375367776353,12.9057263926896));
#70751=CARTESIAN_POINT('Ctrl Pts',(87.0470226873618,57.3736841405164,12.8929163134874));
#70752=CARTESIAN_POINT('Ctrl Pts',(87.0392828130171,57.3725102202813,12.8838071868842));
#70753=CARTESIAN_POINT('Ctrl Pts',(87.0161273608067,57.3689608556031,12.8557623299108));
#70754=CARTESIAN_POINT('Ctrl Pts',(87.0011270807996,57.366609459068,12.8364888286805));
#70755=CARTESIAN_POINT('Ctrl Pts',(86.9453243625591,57.3575976606582,12.7603569668231));
#70756=CARTESIAN_POINT('Ctrl Pts',(86.9086895230378,57.3510928680953,12.7005939910778));
#70757=CARTESIAN_POINT('Ctrl Pts',(86.8463003710983,57.3380992105503,12.5769483952262));
#70758=CARTESIAN_POINT('Ctrl Pts',(86.8204429801723,57.3316335620714,12.5133979409689));
#70759=CARTESIAN_POINT('Ctrl Pts',(86.7950974118727,57.3234639864447,12.433054688005));
#70760=CARTESIAN_POINT('Ctrl Pts',(86.7906375339432,57.3219279546698,12.4179426751307));
#70761=CARTESIAN_POINT('Ctrl Pts',(86.7838981927346,57.3194353245459,12.3934362663027));
#70762=CARTESIAN_POINT('Ctrl Pts',(86.7814427149337,57.3184844464329,12.3840915336714));
#70763=CARTESIAN_POINT('Ctrl Pts',(86.7769310749471,57.3166511485781,12.3660884390914));
#70764=CARTESIAN_POINT('Ctrl Pts',(86.7748588212056,57.3157693045291,12.3574346562902));
#70765=CARTESIAN_POINT('Ctrl Pts',(86.7709385374589,57.3140184255622,12.3402689007293));
#70766=CARTESIAN_POINT('Ctrl Pts',(86.7690868004028,57.3131495617903,12.3317582655975));
#70767=CARTESIAN_POINT('Ctrl Pts',(86.7649972548701,57.31112870839,12.3119857512116));
#70768=CARTESIAN_POINT('Ctrl Pts',(86.7628243923142,57.3099747312008,12.3007114416505));
#70769=CARTESIAN_POINT('Ctrl Pts',(86.7564581425606,57.3063219826306,12.2650860617795));
#70770=CARTESIAN_POINT('Ctrl Pts',(86.7528226881776,57.3038063742123,12.2406429863579));
#70771=CARTESIAN_POINT('Ctrl Pts',(86.7439255923012,57.2960797842203,12.1658978510959));
#70772=CARTESIAN_POINT('Ctrl Pts',(86.7409538637996,57.2908087994244,12.1153800774798));
#70773=CARTESIAN_POINT('Ctrl Pts',(86.7410005413785,57.2854959741782,12.0648273530155));
#70774=CARTESIAN_POINT('Ctrl Pts',(86.741302287513,57.2853233247604,12.0648429798974));
#70775=CARTESIAN_POINT('Ctrl Pts',(86.7403266859258,57.2744592453481,11.9555843196995));
#70776=CARTESIAN_POINT('Ctrl Pts',(86.8032502164186,57.2215904177746,11.4249961153898));
#70777=CARTESIAN_POINT('Ctrl Pts',(87.5455254130428,57.1267168420401,10.6389244339282));
#70778=CARTESIAN_POINT('Ctrl Pts',(88.9574435553591,57.0007025975569,10.9009009231395));
#70779=CARTESIAN_POINT('Ctrl Pts',(89.503174214425,56.8746883530736,12.2291789698061));
#70780=CARTESIAN_POINT('Ctrl Pts',(88.6832633409927,56.7486741085905,13.4081152196214));
#70781=CARTESIAN_POINT('Ctrl Pts',(87.6399969614201,56.6570705962878,13.3722260259654));
#70782=CARTESIAN_POINT('Ctrl Pts',(87.2373685545725,56.6074718321463,13.0778629352728));
#70783=CARTESIAN_POINT('Ctrl Pts',(87.1801902653375,56.5998778161658,13.027459163232));
#70784=CARTESIAN_POINT('Origin',(88.011,66.41344859951,12.066));
#70785=CARTESIAN_POINT('',(87.1806428950462,55.6371283284805,13.0269407256708));
#70786=CARTESIAN_POINT('',(87.1806428354183,55.8074024841729,13.0269406741458));
#70787=CARTESIAN_POINT('',(87.1806428354228,66.41344859951,13.0269406741497));
#70788=CARTESIAN_POINT('Ctrl Pts',(87.1806428950461,55.6371283284805,13.0269407256708));
#70789=CARTESIAN_POINT('Ctrl Pts',(87.1966575417485,55.6391162742572,13.0407791189425));
#70790=CARTESIAN_POINT('Ctrl Pts',(87.2130232902582,55.6410993381051,13.0542216369932));
#70791=CARTESIAN_POINT('Ctrl Pts',(87.2478415693537,55.6452363319383,13.081390173289));
#70792=CARTESIAN_POINT('Ctrl Pts',(87.2663373127494,55.6473886266094,13.0950313153536));
#70793=CARTESIAN_POINT('Ctrl Pts',(87.3191680343155,55.6534388570993,13.1318249117389));
#70794=CARTESIAN_POINT('Ctrl Pts',(87.3542771147909,55.657349514506,13.1538091366578));
#70795=CARTESIAN_POINT('Ctrl Pts',(87.4072461824863,55.6631616021996,13.1834768011556));
#70796=CARTESIAN_POINT('Ctrl Pts',(87.4243101697615,55.665021097995,13.192529196605));
#70797=CARTESIAN_POINT('Ctrl Pts',(87.452084004179,55.668033214733,13.2064609551837));
#70798=CARTESIAN_POINT('Ctrl Pts',(87.4626673270561,55.6691776882719,13.2115869844028));
#70799=CARTESIAN_POINT('Ctrl Pts',(87.4830153913326,55.6713732144237,13.2210960066511));
#70800=CARTESIAN_POINT('Ctrl Pts',(87.4927673989274,55.6724233294133,13.2255039825563));
#70801=CARTESIAN_POINT('Ctrl Pts',(87.5028839742889,55.6735110211033,13.2299236311476));
#70802=CARTESIAN_POINT('Ctrl Pts',(87.5031944163985,55.6735443969063,13.2300591067428));
#70803=CARTESIAN_POINT('Ctrl Pts',(87.5038529905149,55.6736151971493,13.2303461920546));
#70804=CARTESIAN_POINT('Ctrl Pts',(87.504201136306,55.6736526226567,13.2304977698301));
#70805=CARTESIAN_POINT('Ctrl Pts',(87.5047096317478,55.673707282742,13.2307188903608));
#70806=CARTESIAN_POINT('Ctrl Pts',(87.5048699282408,55.6737245131886,13.2307885563523));
#70807=CARTESIAN_POINT('Ctrl Pts',(87.5053328579372,55.6737742727883,13.2309896352733));
#70808=CARTESIAN_POINT('Ctrl Pts',(87.5056355276585,55.6738068047807,13.2311209632269));
#70809=CARTESIAN_POINT('Ctrl Pts',(87.506504456366,55.6739001959589,13.2314975878455));
#70810=CARTESIAN_POINT('Ctrl Pts',(87.5070708421007,55.673961065029,13.2317425893548));
#70811=CARTESIAN_POINT('Ctrl Pts',(87.5129785845904,55.6745959121788,13.2342929918363));
#70812=CARTESIAN_POINT('Ctrl Pts',(87.5183354310073,55.6751711027529,13.2365620293644));
#70813=CARTESIAN_POINT('Ctrl Pts',(87.5326730780846,55.6767095635314,13.2425192785805));
#70814=CARTESIAN_POINT('Ctrl Pts',(87.5416806848059,55.6776750176336,13.2461413576657));
#70815=CARTESIAN_POINT('Ctrl Pts',(87.5656139768747,55.6802380967766,13.255447925763));
#70816=CARTESIAN_POINT('Ctrl Pts',(87.5806062949899,55.6818415006664,13.2609545081679));
#70817=CARTESIAN_POINT('Ctrl Pts',(87.663818240602,55.6907340848988,13.289748704159));
#70818=CARTESIAN_POINT('Ctrl Pts',(87.7338059419043,55.6981998836504,13.3074729191307));
#70819=CARTESIAN_POINT('Ctrl Pts',(87.8708204367117,55.7127831599365,13.3300064403415));
#70820=CARTESIAN_POINT('Ctrl Pts',(87.9374904078203,55.7198626315721,13.3356295588604));
#70821=CARTESIAN_POINT('Ctrl Pts',(88.0196803995132,55.7284374411179,13.3360635381995));
#70822=CARTESIAN_POINT('Ctrl Pts',(88.0350676274304,55.7300358253202,13.3358651668414));
#70823=CARTESIAN_POINT('Ctrl Pts',(88.0685363960555,55.7334930915727,13.3348250704445));
#70824=CARTESIAN_POINT('Ctrl Pts',(88.0866121035431,55.7353479619491,13.3338763441794));
#70825=CARTESIAN_POINT('Ctrl Pts',(88.1117501175129,55.7379054957451,13.3320173445547));
#70826=CARTESIAN_POINT('Ctrl Pts',(88.118833086259,55.7386236675221,13.3314337347683));
#70827=CARTESIAN_POINT('Ctrl Pts',(88.1309343977645,55.7398461000161,13.3303342842001));
#70828=CARTESIAN_POINT('Ctrl Pts',(88.1359551297586,55.7403519211687,13.329847958544));
#70829=CARTESIAN_POINT('Ctrl Pts',(88.1465685640516,55.7414182033296,13.328756035346));
#70830=CARTESIAN_POINT('Ctrl Pts',(88.1521603195523,55.7419782607953,13.3281431808919));
#70831=CARTESIAN_POINT('Ctrl Pts',(88.1675980908674,55.7435202059159,13.3263473230968));
#70832=CARTESIAN_POINT('Ctrl Pts',(88.1774349668264,55.7444979234998,13.3250860817073));
#70833=CARTESIAN_POINT('Ctrl Pts',(88.2404439530875,55.7507359644723,13.316255943038));
#70834=CARTESIAN_POINT('Ctrl Pts',(88.2931151631623,55.7558386964992,13.3054344023733));
#70835=CARTESIAN_POINT('Ctrl Pts',(88.4171547747149,55.7679447184983,13.2716279923893));
#70836=CARTESIAN_POINT('Ctrl Pts',(88.4874753148645,55.7748883283417,13.2456065461113));
#70837=CARTESIAN_POINT('Ctrl Pts',(88.5935032145018,55.7860092315872,13.195334685387));
#70838=CARTESIAN_POINT('Ctrl Pts',(88.6309680579838,55.7900762844767,13.1752094502193));
#70839=CARTESIAN_POINT('Ctrl Pts',(88.679175435972,55.7955520454105,13.1461075863678));
#70840=CARTESIAN_POINT('Ctrl Pts',(88.6908832878241,55.7969017051802,13.1387765332332));
#70841=CARTESIAN_POINT('Ctrl Pts',(88.7102365276172,55.7991679157762,13.1262141487104));
#70842=CARTESIAN_POINT('Ctrl Pts',(88.7179487086796,55.800080561094,13.1210873303257));
#70843=CARTESIAN_POINT('Ctrl Pts',(88.7330497004182,55.8018871510145,13.1108087649444));
#70844=CARTESIAN_POINT('Ctrl Pts',(88.7404411439118,55.8027808713713,13.1056618354437));
#70845=CARTESIAN_POINT('Ctrl Pts',(88.7583433574245,55.8049692612826,13.0929109959384));
#70846=CARTESIAN_POINT('Ctrl Pts',(88.7687932849732,55.8062670525804,13.0852240149216));
#70847=CARTESIAN_POINT('Ctrl Pts',(88.8051932460129,55.8108621234631,13.0575789268829));
#70848=CARTESIAN_POINT('Ctrl Pts',(88.8304848261571,55.8141915632259,13.036781029078));
#70849=CARTESIAN_POINT('Ctrl Pts',(88.9201000927007,55.8265210474135,12.9570891838294));
#70850=CARTESIAN_POINT('Ctrl Pts',(88.9791079843614,55.835727146904,12.8925983979044));
#70851=CARTESIAN_POINT('Ctrl Pts',(89.0602621818186,55.8500705710538,12.7831858671924));
#70852=CARTESIAN_POINT('Ctrl Pts',(89.0871844537959,55.8552105447934,12.7421176125316));
#70853=CARTESIAN_POINT('Ctrl Pts',(89.1177991738759,55.8614998146564,12.6889339773645));
#70854=CARTESIAN_POINT('Ctrl Pts',(89.1237780700906,55.8627524967985,12.6781896427754));
#70855=CARTESIAN_POINT('Ctrl Pts',(89.1324950260401,55.8646146869766,12.6619750643581));
#70856=CARTESIAN_POINT('Ctrl Pts',(89.1353508749676,55.865230852365,12.6565696287676));
#70857=CARTESIAN_POINT('Ctrl Pts',(89.1404545385452,55.8663428950501,12.6467383926541));
#70858=CARTESIAN_POINT('Ctrl Pts',(89.1427155291385,55.8668395371269,12.6423198759139));
#70859=CARTESIAN_POINT('Ctrl Pts',(89.1478060136406,55.8679669742596,12.6322263622838));
#70860=CARTESIAN_POINT('Ctrl Pts',(89.1506189912415,55.8685967520716,12.6265432785495));
#70861=CARTESIAN_POINT('Ctrl Pts',(89.1592834587884,55.8705588432015,12.6087035208388));
#70862=CARTESIAN_POINT('Ctrl Pts',(89.1649842067851,55.8718825099257,12.5964738609668));
#70863=CARTESIAN_POINT('Ctrl Pts',(89.2045111413687,55.8813209205935,12.5080233388288));
#70864=CARTESIAN_POINT('Ctrl Pts',(89.2309587827467,55.8890796517984,12.4287111492942));
#70865=CARTESIAN_POINT('Ctrl Pts',(89.2609388073206,55.9017593893021,12.2967526302879));
#70866=CARTESIAN_POINT('Ctrl Pts',(89.2693231612351,55.9066306403825,12.2454876970344));
#70867=CARTESIAN_POINT('Ctrl Pts',(89.2767790551808,55.9136952953303,12.1718048464141));
#70868=CARTESIAN_POINT('Ctrl Pts',(89.2784326683684,55.9158223993223,12.1496994005669));
#70869=CARTESIAN_POINT('Ctrl Pts',(89.2803700289887,55.9196879732769,12.1097802745085));
#70870=CARTESIAN_POINT('Ctrl Pts',(89.2808589836994,55.9214201406924,12.091982102853));
#70871=CARTESIAN_POINT('Ctrl Pts',(89.2810386596975,55.9241522940594,12.0640886772878));
#70872=CARTESIAN_POINT('Ctrl Pts',(89.280983369067,55.9251443728037,12.0539967493361));
#70873=CARTESIAN_POINT('Ctrl Pts',(89.2806545115811,55.9270098537972,12.0350955565668));
#70874=CARTESIAN_POINT('Ctrl Pts',(89.2804094996243,55.9278823119618,12.0262863282272));
#70875=CARTESIAN_POINT('Ctrl Pts',(89.2796518115364,55.9298523695406,12.0064682308919));
#70876=CARTESIAN_POINT('Ctrl Pts',(89.279087478474,55.9309515145273,11.9954622249726));
#70877=CARTESIAN_POINT('Ctrl Pts',(89.2772581722589,55.9338052960521,11.9670273518823));
#70878=CARTESIAN_POINT('Ctrl Pts',(89.2757766239835,55.9355664915871,11.9496154756622));
#70879=CARTESIAN_POINT('Ctrl Pts',(89.2665586479876,55.9444439554479,11.8625805901143));
#70880=CARTESIAN_POINT('Ctrl Pts',(89.2534318267701,55.9517210931723,11.7936653095985));
#70881=CARTESIAN_POINT('Ctrl Pts',(89.2176838792596,55.9657682810975,11.6649301374377));
#70882=CARTESIAN_POINT('Ctrl Pts',(89.1960937041524,55.9725025550085,11.6050267144622));
#70883=CARTESIAN_POINT('Ctrl Pts',(89.1639874814961,55.9806948586644,11.5333236331117));
#70884=CARTESIAN_POINT('Ctrl Pts',(89.1576261640088,55.9822497517298,11.5197649468844));
#70885=CARTESIAN_POINT('Ctrl Pts',(89.1432001287251,55.9856283311879,11.4903801303504));
#70886=CARTESIAN_POINT('Ctrl Pts',(89.1350398737897,55.9874479744314,11.4746034831961));
#70887=CARTESIAN_POINT('Ctrl Pts',(89.1231783327473,55.9899656742618,11.4528041584942));
#70888=CARTESIAN_POINT('Ctrl Pts',(89.1197542832255,55.9906786321525,11.4466344118229));
#70889=CARTESIAN_POINT('Ctrl Pts',(89.1137983987996,55.9918950603745,11.4361102836849));
#70890=CARTESIAN_POINT('Ctrl Pts',(89.1112918188034,55.9924000511409,11.4317419441958));
#70891=CARTESIAN_POINT('Ctrl Pts',(89.1059187905168,55.9934678258761,11.4225058281628));
#70892=CARTESIAN_POINT('Ctrl Pts',(89.1030457675802,55.9940301837883,11.4176421103241));
#70893=CARTESIAN_POINT('Ctrl Pts',(89.0949829953296,55.9955852846546,11.4041983608931));
#70894=CARTESIAN_POINT('Ctrl Pts',(89.0897237492058,55.9965737403957,11.395660056588));
#70895=CARTESIAN_POINT('Ctrl Pts',(89.0508493751088,56.0037029489873,11.3341907235481));
#70896=CARTESIAN_POINT('Ctrl Pts',(89.0134495705617,56.0096269624183,11.283740743919));
#70897=CARTESIAN_POINT('Ctrl Pts',(88.940356290514,56.0201315394287,11.1990441419156));
#70898=CARTESIAN_POINT('Ctrl Pts',(88.9061129501435,56.0247159314429,11.1637315713122));
#70899=CARTESIAN_POINT('Ctrl Pts',(88.8421375310175,56.03289278576,11.1049943529791));
#70900=CARTESIAN_POINT('Ctrl Pts',(88.8132461906574,56.0364629514657,11.0807477235114));
#70901=CARTESIAN_POINT('Ctrl Pts',(88.7624019205083,56.0426038469785,11.0417980652809));
#70902=CARTESIAN_POINT('Ctrl Pts',(88.7409904372697,56.0451502740243,11.0264288462198));
#70903=CARTESIAN_POINT('Ctrl Pts',(88.7094126116907,56.0488627692712,11.005218911422));
#70904=CARTESIAN_POINT('Ctrl Pts',(88.6996179207254,56.0500085255986,10.9988345812159));
#70905=CARTESIAN_POINT('Ctrl Pts',(88.6822262708745,56.0520339942342,10.9878375557018));
#70906=CARTESIAN_POINT('Ctrl Pts',(88.6746662714523,56.0529115307871,10.9831675877452));
#70907=CARTESIAN_POINT('Ctrl Pts',(88.6587437661365,56.0547541911329,10.9735613041863));
#70908=CARTESIAN_POINT('Ctrl Pts',(88.6503724491952,56.0557198219884,10.9686408297783));
#70909=CARTESIAN_POINT('Ctrl Pts',(88.6280779651335,56.0582839079776,10.9558783286952));
#70910=CARTESIAN_POINT('Ctrl Pts',(88.6140623527833,56.0598881502024,10.9482025769741));
#70911=CARTESIAN_POINT('Ctrl Pts',(88.5359858059523,56.0687879623391,10.9073391511682));
#70912=CARTESIAN_POINT('Ctrl Pts',(88.4693458572225,56.0762604648247,10.8793999772346));
#70913=CARTESIAN_POINT('Ctrl Pts',(88.3371893591119,56.090844114938,10.8367909711677));
#70914=CARTESIAN_POINT('Ctrl Pts',(88.2721526629635,56.0979169553746,10.8213498843952));
#70915=CARTESIAN_POINT('Ctrl Pts',(88.1910068747653,56.1064844368024,10.8087275440985));
#70916=CARTESIAN_POINT('Ctrl Pts',(88.1757684170574,56.1080820065607,10.806639875073));
#70917=CARTESIAN_POINT('Ctrl Pts',(88.1425301929175,56.1115378034208,10.8026999260661));
#70918=CARTESIAN_POINT('Ctrl Pts',(88.1245203002804,56.1133920181771,10.8009543376484));
#70919=CARTESIAN_POINT('Ctrl Pts',(88.0993921900853,56.1159488114788,10.7990598631737));
#70920=CARTESIAN_POINT('Ctrl Pts',(88.0923020320993,56.1166668869841,10.7985851200841));
#70921=CARTESIAN_POINT('Ctrl Pts',(88.0801727221825,56.1178892083945,10.7978751737321));
#70922=CARTESIAN_POINT('Ctrl Pts',(88.0751355902273,56.1183950139965,10.7976104417985));
#70923=CARTESIAN_POINT('Ctrl Pts',(88.064477410663,56.1194613226922,10.7971139484841));
#70924=CARTESIAN_POINT('Ctrl Pts',(88.0588562212764,56.120021421833,10.7968895115888));
#70925=CARTESIAN_POINT('Ctrl Pts',(88.0433205130568,56.1215636050123,10.7963725896781));
#70926=CARTESIAN_POINT('Ctrl Pts',(88.03340341165,56.1225415168726,10.79615887364));
#70927=CARTESIAN_POINT('Ctrl Pts',(87.9696194821342,56.1287954453636,10.7955318392073));
#70928=CARTESIAN_POINT('Ctrl Pts',(87.9157651788213,56.1339128960047,10.7984298078159));
#70929=CARTESIAN_POINT('Ctrl Pts',(87.7880484743806,56.1460217478487,10.8134925729129));
#70930=CARTESIAN_POINT('Ctrl Pts',(87.7147674563245,56.1529543306058,10.8287739572073));
#70931=CARTESIAN_POINT('Ctrl Pts',(87.6026022001417,56.164060615678,10.8627065293705));
#70932=CARTESIAN_POINT('Ctrl Pts',(87.5625967117778,56.1681244943999,10.8770350707131));
#70933=CARTESIAN_POINT('Ctrl Pts',(87.5106366817107,56.1735966453727,10.8986409012261));
#70934=CARTESIAN_POINT('Ctrl Pts',(87.4979731099872,56.1749459728426,10.9041505734897));
#70935=CARTESIAN_POINT('Ctrl Pts',(87.4769726029787,56.1772117823192,10.9136977440502));
#70936=CARTESIAN_POINT('Ctrl Pts',(87.4685851766618,56.1781243618353,10.9176220579012));
#70937=CARTESIAN_POINT('Ctrl Pts',(87.452125281242,56.1799309411882,10.9255438703538));
#70938=CARTESIAN_POINT('Ctrl Pts',(87.4440509356029,56.1808247176085,10.9295362378753));
#70939=CARTESIAN_POINT('Ctrl Pts',(87.4244504827272,56.1830134611015,10.9394885585551));
#70940=CARTESIAN_POINT('Ctrl Pts',(87.4129722426007,56.1843115523338,10.9455397672585));
#70941=CARTESIAN_POINT('Ctrl Pts',(87.372845889215,56.188909461235,10.9674861620631));
#70942=CARTESIAN_POINT('Ctrl Pts',(87.3447251315953,56.192241494459,10.9843112155731));
#70943=CARTESIAN_POINT('Ctrl Pts',(87.2442707878701,56.2045714642783,11.0498182880128));
#70944=CARTESIAN_POINT('Ctrl Pts',(87.1763595116153,56.2137752159159,11.1048188063935));
#70945=CARTESIAN_POINT('Ctrl Pts',(87.0889306919784,56.2267700228069,11.1919268355821));
#70946=CARTESIAN_POINT('Ctrl Pts',(87.0643413274314,56.2305754225416,11.2186196204076));
#70947=CARTESIAN_POINT('Ctrl Pts',(87.0271184295518,56.2365499754805,11.262672679929));
#70948=CARTESIAN_POINT('Ctrl Pts',(87.0137238993618,56.2387489214221,11.2793626675136));
#70949=CARTESIAN_POINT('Ctrl Pts',(86.9961736224313,56.2416908311097,11.3024002298551));
#70950=CARTESIAN_POINT('Ctrl Pts',(86.9916446196991,56.2424557987304,11.3084567308875));
#70951=CARTESIAN_POINT('Ctrl Pts',(86.9841382472343,56.2437330227021,11.3186840084514));
#70952=CARTESIAN_POINT('Ctrl Pts',(86.9811316030901,56.244247199545,11.3228328987715));
#70953=CARTESIAN_POINT('Ctrl Pts',(86.9749800803662,56.2453044264436,11.3314304642347));
#70954=CARTESIAN_POINT('Ctrl Pts',(86.971838584719,56.2458472518691,11.3358813562947));
#70955=CARTESIAN_POINT('Ctrl Pts',(86.9635287614173,56.2472914053428,11.3478170618374));
#70956=CARTESIAN_POINT('Ctrl Pts',(86.9584118687584,56.2481893905372,11.355337652707));
#70957=CARTESIAN_POINT('Ctrl Pts',(86.9344966965585,56.2524320379852,11.3913122335962));
#70958=CARTESIAN_POINT('Ctrl Pts',(86.9167662021825,56.2557149288231,11.4204645551366));
#70959=CARTESIAN_POINT('Ctrl Pts',(86.8547707484135,56.2678895556538,11.5323091523519));
#70960=CARTESIAN_POINT('Ctrl Pts',(86.8185328665949,56.2765287208852,11.6191038169872));
#70961=CARTESIAN_POINT('Ctrl Pts',(86.7797200802849,56.2896047084489,11.7516507588071));
#70962=CARTESIAN_POINT('Ctrl Pts',(86.7694989147304,56.2938425203501,11.7948177423543));
#70963=CARTESIAN_POINT('Ctrl Pts',(86.75904840319,56.2995121402973,11.8521939074152));
#70964=CARTESIAN_POINT('Ctrl Pts',(86.7567685632377,56.3008791851863,11.8660017210296));
#70965=CARTESIAN_POINT('Ctrl Pts',(86.7533546557878,56.3031664025184,11.8890406043635));
#70966=CARTESIAN_POINT('Ctrl Pts',(86.7520929406033,56.3040825105391,11.8982518440248));
#70967=CARTESIAN_POINT('Ctrl Pts',(86.7498116281836,56.3058897896291,11.9163854014396));
#70968=CARTESIAN_POINT('Ctrl Pts',(86.7487853113059,56.3067806936629,11.9253063385142));
#70969=CARTESIAN_POINT('Ctrl Pts',(86.7465233004314,56.3089511861853,11.9469911304842));
#70970=CARTESIAN_POINT('Ctrl Pts',(86.7453861951153,56.3102337745337,11.9597639391091));
#70971=CARTESIAN_POINT('Ctrl Pts',(86.7421265891875,56.314686078039,12.003942964004));
#70972=CARTESIAN_POINT('Ctrl Pts',(86.7409785861381,56.3178852264891,12.0354062694396));
#70973=CARTESIAN_POINT('Ctrl Pts',(86.7410352212291,56.3263148445825,12.1174797443888));
#70974=CARTESIAN_POINT('Ctrl Pts',(86.7440945202449,56.331592165542,12.1680288336347));
#70975=CARTESIAN_POINT('Ctrl Pts',(86.7596908493171,56.3452677324998,12.2971843871384));
#70976=CARTESIAN_POINT('Ctrl Pts',(86.7766131019831,56.3537058707465,12.3750492538448));
#70977=CARTESIAN_POINT('Ctrl Pts',(86.8059324309397,56.36369054287,12.467259981848));
#70978=CARTESIAN_POINT('Ctrl Pts',(86.8114928091901,56.3654576267333,12.4835883390532));
#70979=CARTESIAN_POINT('Ctrl Pts',(86.8195930577662,56.3678641805881,12.5058764624462));
#70980=CARTESIAN_POINT('Ctrl Pts',(86.8218480081806,56.3685179406992,12.5119364877091));
#70981=CARTESIAN_POINT('Ctrl Pts',(86.8258027220988,56.3696369763389,12.5223211572607));
#70982=CARTESIAN_POINT('Ctrl Pts',(86.8274800772679,56.3701035024166,12.5266540797633));
#70983=CARTESIAN_POINT('Ctrl Pts',(86.8311038950971,56.3710942489164,12.5358646177411));
#70984=CARTESIAN_POINT('Ctrl Pts',(86.833056920098,56.3716180587509,12.5407395933306));
#70985=CARTESIAN_POINT('Ctrl Pts',(86.8381333998695,56.3729543940538,12.5531868522906));
#70986=CARTESIAN_POINT('Ctrl Pts',(86.8413000584495,56.3737644051926,12.5607414987031));
#70987=CARTESIAN_POINT('Ctrl Pts',(86.8551894874383,56.3772207984287,12.5929982870824));
#70988=CARTESIAN_POINT('Ctrl Pts',(86.8666245069872,56.3798288481463,12.6173893602901));
#70989=CARTESIAN_POINT('Ctrl Pts',(86.9028290931551,56.3874868679531,12.6886262917061));
#70990=CARTESIAN_POINT('Ctrl Pts',(86.9297640290972,56.3924532625638,12.7343084705616));
#70991=CARTESIAN_POINT('Ctrl Pts',(87.0067403310917,56.4053142286159,12.8479630621663));
#70992=CARTESIAN_POINT('Ctrl Pts',(87.0608259367857,56.413184283837,12.9128588107876));
#70993=CARTESIAN_POINT('Ctrl Pts',(87.1332758337077,56.4229920160226,12.9840412066627));
#70994=CARTESIAN_POINT('Ctrl Pts',(87.1458636762144,56.4246722122169,12.9959131372973));
#70995=CARTESIAN_POINT('Ctrl Pts',(87.1659325664215,56.4273180656943,13.0140804229115));
#70996=CARTESIAN_POINT('Ctrl Pts',(87.1732508658231,56.4282763111732,13.0205532091559));
#70997=CARTESIAN_POINT('Ctrl Pts',(87.1806428354357,56.4292380444866,13.0269406741609));
#70998=CARTESIAN_POINT('',(86.7390851620259,56.4915176496327,12.0663168694075));
#70999=CARTESIAN_POINT('Ctrl Pts',(87.1801902653375,56.5998778161658,13.027459163232));
#71000=CARTESIAN_POINT('Ctrl Pts',(86.9210985275164,56.5654670839852,12.7990647662412));
#71001=CARTESIAN_POINT('Ctrl Pts',(86.7455185357409,56.5293656784333,12.4445437149527));
#71002=CARTESIAN_POINT('Ctrl Pts',(86.7389313495616,56.4932642728814,12.0832340865421));
#71003=CARTESIAN_POINT('Ctrl Pts',(86.7389871696286,56.49157359951,12.0663114291823));
#71004=CARTESIAN_POINT('Ctrl Pts',(86.7410000705041,56.490424310788,12.0664231790162));
#71005=CARTESIAN_POINT('Ctrl Pts',(86.7409944767077,56.4887786996571,12.0496356712115));
#71006=CARTESIAN_POINT('Ctrl Pts',(86.7413217419207,56.4871486528724,12.0328482222298));
#71007=CARTESIAN_POINT('Ctrl Pts',(86.7440792033363,56.4803888779874,11.9627636847443));
#71008=CARTESIAN_POINT('Ctrl Pts',(86.749533632266,56.4753729203867,11.9096347422265));
#71009=CARTESIAN_POINT('Ctrl Pts',(86.768349665406,56.4646530658008,11.7968567378609));
#71010=CARTESIAN_POINT('Ctrl Pts',(86.7827018223532,56.4589658482191,11.7375172852167));
#71011=CARTESIAN_POINT('Ctrl Pts',(86.8094982888892,56.4506112304282,11.6536575793795));
#71012=CARTESIAN_POINT('Ctrl Pts',(86.8185584631519,56.4480261107585,11.6281465907376));
#71013=CARTESIAN_POINT('Ctrl Pts',(86.8359784216655,56.4434202088412,11.5836584749831));
#71014=CARTESIAN_POINT('Ctrl Pts',(86.8440010284607,56.4414101030804,11.5645597327873));
#71015=CARTESIAN_POINT('Ctrl Pts',(86.8568603942884,56.438340381375,11.5359285543681));
#71016=CARTESIAN_POINT('Ctrl Pts',(86.861356725083,56.4372922935868,11.526246083597));
#71017=CARTESIAN_POINT('Ctrl Pts',(86.8694073110944,56.4354577264873,11.5094668830204));
#71018=CARTESIAN_POINT('Ctrl Pts',(86.8729070970506,56.4346731649628,11.5023445070938));
#71019=CARTESIAN_POINT('Ctrl Pts',(86.8809816175717,56.4328914891435,11.4862939613533));
#71020=CARTESIAN_POINT('Ctrl Pts',(86.8855957873334,56.4318930404775,11.4773863923023));
#71021=CARTESIAN_POINT('Ctrl Pts',(86.8983429609311,56.4291858788526,11.4534761008689));
#71022=CARTESIAN_POINT('Ctrl Pts',(86.9066732734729,56.427470320509,11.4385817807309));
#71023=CARTESIAN_POINT('Ctrl Pts',(86.9275529782467,56.4232926603611,11.4029541836966));
#71024=CARTESIAN_POINT('Ctrl Pts',(86.940400105792,56.4208205437462,11.3824044521476));
#71025=CARTESIAN_POINT('Ctrl Pts',(87.0020707037576,56.4093774007473,11.2897646095174));
#71026=CARTESIAN_POINT('Ctrl Pts',(87.0576328732422,56.4001850851353,11.2224563229708));
#71027=CARTESIAN_POINT('Ctrl Pts',(87.1545397847391,56.3858605373558,11.1269695469317));
#71028=CARTESIAN_POINT('Ctrl Pts',(87.1914193126317,56.3807253865876,11.0946138270385));
#71029=CARTESIAN_POINT('Ctrl Pts',(87.2369743565261,56.3748050675469,11.0590935056295));
#71030=CARTESIAN_POINT('Ctrl Pts',(87.2439222965438,56.3739130486739,11.0537904385945));
#71031=CARTESIAN_POINT('Ctrl Pts',(87.2566354155185,56.3723012853771,11.0442931510139));
#71032=CARTESIAN_POINT('Ctrl Pts',(87.2623821426932,56.3715801421382,11.0400749910614));
#71033=CARTESIAN_POINT('Ctrl Pts',(87.2682565773948,56.3708506988579,11.0358387402388));
#71034=CARTESIAN_POINT('Ctrl Pts',(87.2683488382733,56.3708392445173,11.0357722266789));
#71035=CARTESIAN_POINT('Ctrl Pts',(87.2685328322327,56.3708164052009,11.0356396176234));
#71036=CARTESIAN_POINT('Ctrl Pts',(87.2686245651208,56.3708050202265,11.0355735220446));
#71037=CARTESIAN_POINT('Ctrl Pts',(87.2688076081209,56.3707823065441,11.0354416726367));
#71038=CARTESIAN_POINT('Ctrl Pts',(87.2688989181502,56.3707709778283,11.0353759186889));
#71039=CARTESIAN_POINT('Ctrl Pts',(87.2690812213319,56.3707483634739,11.0352446757701));
#71040=CARTESIAN_POINT('Ctrl Pts',(87.269172214486,56.3707370778214,11.0351791866634));
#71041=CARTESIAN_POINT('Ctrl Pts',(87.2693539913903,56.3707145362265,11.0350483956949));
#71042=CARTESIAN_POINT('Ctrl Pts',(87.2694447749949,56.370703280293,11.0349830938468));
#71043=CARTESIAN_POINT('Ctrl Pts',(87.26962624206,56.3706807845657,11.0348525985527));
#71044=CARTESIAN_POINT('Ctrl Pts',(87.2697169255604,56.370669544762,11.0347874050308));
#71045=CARTESIAN_POINT('Ctrl Pts',(87.2698983041798,56.3706470674316,11.0346570459229));
#71046=CARTESIAN_POINT('Ctrl Pts',(87.2699889993472,56.3706358298986,11.0345918802997));
#71047=CARTESIAN_POINT('Ctrl Pts',(87.2701705163076,56.3706133428628,11.0344614943715));
#71048=CARTESIAN_POINT('Ctrl Pts',(87.2702613380428,56.3706020933718,11.0343962741517));
#71049=CARTESIAN_POINT('Ctrl Pts',(87.270443226833,56.3705795677358,11.0342656939495));
#71050=CARTESIAN_POINT('Ctrl Pts',(87.2705342939309,56.370568291595,11.0342003340276));
#71051=CARTESIAN_POINT('Ctrl Pts',(87.2707167966334,56.3705456974386,11.0340693863076));
#71052=CARTESIAN_POINT('Ctrl Pts',(87.2708082323319,56.3705343794258,11.0340037985833));
#71053=CARTESIAN_POINT('Ctrl Pts',(87.2709916007978,56.37051168566,11.0338723034888));
#71054=CARTESIAN_POINT('Ctrl Pts',(87.2710835337144,56.3705003099083,11.0338063962052));
#71055=CARTESIAN_POINT('Ctrl Pts',(87.2712680314927,56.3704774840393,11.0336741659072));
#71056=CARTESIAN_POINT('Ctrl Pts',(87.2713605965202,56.370466033927,11.0336078430233));
#71057=CARTESIAN_POINT('Ctrl Pts',(87.2715465008455,56.3704430418132,11.033474680326));
#71058=CARTESIAN_POINT('Ctrl Pts',(87.2716398401792,56.370431499839,11.033407840796));
#71059=CARTESIAN_POINT('Ctrl Pts',(87.2718274438669,56.3704083054605,11.0332735378152));
#71060=CARTESIAN_POINT('Ctrl Pts',(87.2719217083586,56.3703966530776,11.0332060746395));
#71061=CARTESIAN_POINT('Ctrl Pts',(87.2721113228761,56.3703732181611,11.0330704106469));
#71062=CARTESIAN_POINT('Ctrl Pts',(87.2722066732121,56.3703614356347,11.0330022100524));
#71063=CARTESIAN_POINT('Ctrl Pts',(87.2723461567687,56.3703442025296,11.0329024717763));
#71064=CARTESIAN_POINT('Ctrl Pts',(87.2723902822376,56.3703387512953,11.0328709239552));
#71065=CARTESIAN_POINT('Ctrl Pts',(87.2724821732136,56.370327400054,11.0328052347375));
#71066=CARTESIAN_POINT('Ctrl Pts',(87.272529939278,56.3703215000534,11.0327710936755));
#71067=CARTESIAN_POINT('Ctrl Pts',(87.2726295855147,56.3703091929578,11.0326998814097));
#71068=CARTESIAN_POINT('Ctrl Pts',(87.2726814659998,56.3703027859164,11.0326628108804));
#71069=CARTESIAN_POINT('Ctrl Pts',(87.2727899052278,56.3702893953567,11.0325853393688));
#71070=CARTESIAN_POINT('Ctrl Pts',(87.272846464472,56.3702824118908,11.0325449391393));
#71071=CARTESIAN_POINT('Ctrl Pts',(87.2729649386706,56.3702677851928,11.0324603277878));
#71072=CARTESIAN_POINT('Ctrl Pts',(87.2730268543755,56.3702601420111,11.0324161175187));
#71073=CARTESIAN_POINT('Ctrl Pts',(87.2731568638035,56.3702440948194,11.032323303268));
#71074=CARTESIAN_POINT('Ctrl Pts',(87.2732249584165,56.3702356908805,11.0322747004085));
#71075=CARTESIAN_POINT('Ctrl Pts',(87.273368335546,56.3702179981067,11.032172385672));
#71076=CARTESIAN_POINT('Ctrl Pts',(87.2734436190188,56.370208709386,11.0321186753664));
#71077=CARTESIAN_POINT('Ctrl Pts',(87.2736026302837,56.3701890927586,11.0320052564394));
#71078=CARTESIAN_POINT('Ctrl Pts',(87.2736863595989,56.3701787649665,11.0319455496668));
#71079=CARTESIAN_POINT('Ctrl Pts',(87.2738638502754,56.3701568753092,11.0318190148594));
#71080=CARTESIAN_POINT('Ctrl Pts',(87.2739576133625,56.3701453136324,11.0317521894842));
#71081=CARTESIAN_POINT('Ctrl Pts',(87.2741572134408,56.3701207057009,11.0316099745354));
#71082=CARTESIAN_POINT('Ctrl Pts',(87.2742630530015,56.3701076596722,11.0315345883924));
#71083=CARTESIAN_POINT('Ctrl Pts',(87.2744894875351,56.370079754236,11.0313733586743));
#71084=CARTESIAN_POINT('Ctrl Pts',(87.2746100859724,56.3700648951541,11.0312875199213));
#71085=CARTESIAN_POINT('Ctrl Pts',(87.2786299330166,56.3695697142246,11.0284273586923));
#71086=CARTESIAN_POINT('Ctrl Pts',(87.2825447771138,56.3690909217771,11.0256751027829));
#71087=CARTESIAN_POINT('Ctrl Pts',(87.2916750575344,56.3679821814479,11.019333047508));
#71088=CARTESIAN_POINT('Ctrl Pts',(87.2969019151688,56.3673533567395,11.0157600208355));
#71089=CARTESIAN_POINT('Ctrl Pts',(87.3126171974897,56.3654795160996,11.0051887857053));
#71090=CARTESIAN_POINT('Ctrl Pts',(87.3231838553466,56.3642417509356,10.9983071760737));
#71091=CARTESIAN_POINT('Ctrl Pts',(87.382871782273,56.3573616452187,10.9606890214764));
#71092=CARTESIAN_POINT('Ctrl Pts',(87.4339573578284,56.3518890492376,10.9331798210705));
#71093=CARTESIAN_POINT('Ctrl Pts',(87.5324397445668,56.3417366362891,10.8885467312684));
#71094=CARTESIAN_POINT('Ctrl Pts',(87.5793135195015,56.3370584669608,10.8705658431235));
#71095=CARTESIAN_POINT('Ctrl Pts',(87.6625147283791,56.3288380521041,10.844183242201));
#71096=CARTESIAN_POINT('Ctrl Pts',(87.6983739262747,56.3253211888709,10.834520127424));
#71097=CARTESIAN_POINT('Ctrl Pts',(87.7467028267305,56.3205724667023,10.8237437011638));
#71098=CARTESIAN_POINT('Ctrl Pts',(87.7588419473514,56.3193790292513,10.8212229108515));
#71099=CARTESIAN_POINT('Ctrl Pts',(87.7888890615619,56.3164209155193,10.815440916354));
#71100=CARTESIAN_POINT('Ctrl Pts',(87.8068332884153,56.314650741386,10.8123863574094));
#71101=CARTESIAN_POINT('Ctrl Pts',(87.8348987398724,56.3118723908203,10.8082274329291));
#71102=CARTESIAN_POINT('Ctrl Pts',(87.8449787592737,56.3108725810802,10.8068572689973));
#71103=CARTESIAN_POINT('Ctrl Pts',(87.8638099351451,56.3090004349457,10.8045276170071));
#71104=CARTESIAN_POINT('Ctrl Pts',(87.8725567930655,56.3081291091245,10.8035377404462));
#71105=CARTESIAN_POINT('Ctrl Pts',(87.8921596036967,56.3061719822419,10.8015254650013));
#71106=CARTESIAN_POINT('Ctrl Pts',(87.9030196925874,56.3050847224233,10.8005518091968));
#71107=CARTESIAN_POINT('Ctrl Pts',(87.9309162330448,56.3022832651873,10.7984124609382));
#71108=CARTESIAN_POINT('Ctrl Pts',(87.947965421085,56.3005629077477,10.797450376176));
#71109=CARTESIAN_POINT('Ctrl Pts',(88.0549190890686,56.28971301617,10.7935762647113));
#71110=CARTESIAN_POINT('Ctrl Pts',(88.1448803227444,56.2803039770397,10.7998801562732));
#71111=CARTESIAN_POINT('Ctrl Pts',(88.2817750535413,56.2656445958738,10.8242290174473));
#71112=CARTESIAN_POINT('Ctrl Pts',(88.3296144268799,56.2604609850945,10.8356342849448));
#71113=CARTESIAN_POINT('Ctrl Pts',(88.3934232055733,56.2535324835066,10.8548194445523));
#71114=CARTESIAN_POINT('Ctrl Pts',(88.410066468963,56.2517241749087,10.86020072659));
#71115=CARTESIAN_POINT('Ctrl Pts',(88.4386829933462,56.2486181356404,10.870110826045));
#71116=CARTESIAN_POINT('Ctrl Pts',(88.4507084698018,56.2473138857012,10.8744798927133));
#71117=CARTESIAN_POINT('Ctrl Pts',(88.4684695107905,56.2453909386045,10.8812383382198));
#71118=CARTESIAN_POINT('Ctrl Pts',(88.4742562952742,56.2447649545584,10.883489044718));
#71119=CARTESIAN_POINT('Ctrl Pts',(88.484636201945,56.2436433510208,10.8876140900108));
#71120=CARTESIAN_POINT('Ctrl Pts',(88.489235058203,56.2431468869627,10.8894729765329));
#71121=CARTESIAN_POINT('Ctrl Pts',(88.4995905784515,56.2420299721852,10.8937294983982));
#71122=CARTESIAN_POINT('Ctrl Pts',(88.5053406282151,56.2414104544468,10.8961426447587));
#71123=CARTESIAN_POINT('Ctrl Pts',(88.5229617803364,56.2395132372071,10.903690911402));
#71124=CARTESIAN_POINT('Ctrl Pts',(88.5347730205113,56.2382433922188,10.9089653624906));
#71125=CARTESIAN_POINT('Ctrl Pts',(88.6068219341588,56.2304953922296,10.9424692094042));
#71126=CARTESIAN_POINT('Ctrl Pts',(88.6648559092674,56.2242434915549,10.9752200339329));
#71127=CARTESIAN_POINT('Ctrl Pts',(88.7504030762085,56.2145773851178,11.0327912405865));
#71128=CARTESIAN_POINT('Ctrl Pts',(88.7798447966393,56.2111590048738,11.0545085927455));
#71129=CARTESIAN_POINT('Ctrl Pts',(88.8394849889903,56.2039539411864,11.1026117372673));
#71130=CARTESIAN_POINT('Ctrl Pts',(88.869452131769,56.2001672709245,11.1292162744369));
#71131=CARTESIAN_POINT('Ctrl Pts',(88.9177769762932,56.193698887784,11.1763872560628));
#71132=CARTESIAN_POINT('Ctrl Pts',(88.936813711628,56.1910452735105,11.1962160985985));
#71133=CARTESIAN_POINT('Ctrl Pts',(88.9631322565225,56.1872059674732,11.2254732790846));
#71134=CARTESIAN_POINT('Ctrl Pts',(88.9709491471386,56.1860426371561,11.2344119925652));
#71135=CARTESIAN_POINT('Ctrl Pts',(88.9844102301413,56.1839972484038,11.2502476363671));
#71136=CARTESIAN_POINT('Ctrl Pts',(88.9901094240346,56.1831175077262,11.2570969647151));
#71137=CARTESIAN_POINT('Ctrl Pts',(89.0018150857961,56.1812811146627,11.2714698625218));
#71138=CARTESIAN_POINT('Ctrl Pts',(89.0078089888584,56.1803240301923,11.2790028587972));
#71139=CARTESIAN_POINT('Ctrl Pts',(89.0232829717716,56.1778080089371,11.2989105792398));
#71140=CARTESIAN_POINT('Ctrl Pts',(89.0326214958691,56.1762436714983,11.3113925139936));
#71141=CARTESIAN_POINT('Ctrl Pts',(89.0580231221436,56.1718549449632,11.3466804529686));
#71142=CARTESIAN_POINT('Ctrl Pts',(89.0735669327325,56.169011918626,11.3698468267732));
#71143=CARTESIAN_POINT('Ctrl Pts',(89.1342434680561,56.157226054938,11.4670502190186));
#71144=CARTESIAN_POINT('Ctrl Pts',(89.1724942837361,56.1480712647127,11.5450940886237));
#71145=CARTESIAN_POINT('Ctrl Pts',(89.2194158480375,56.1337985244895,11.6722728495075));
#71146=CARTESIAN_POINT('Ctrl Pts',(89.2336773376462,56.1286769272316,11.719083064245));
#71147=CARTESIAN_POINT('Ctrl Pts',(89.2480988191803,56.1224074729185,11.7785331935176));
#71148=CARTESIAN_POINT('Ctrl Pts',(89.250819484923,56.1211568874318,11.7905034693249));
#71149=CARTESIAN_POINT('Ctrl Pts',(89.2546336632738,56.1192972530635,11.8084876224617));
#71150=CARTESIAN_POINT('Ctrl Pts',(89.2558579061516,56.1186815713323,11.8144724424914));
#71151=CARTESIAN_POINT('Ctrl Pts',(89.257902487706,56.117619898294,11.824848313873));
#71152=CARTESIAN_POINT('Ctrl Pts',(89.2587428879161,56.1171728265193,11.8292350583147));
#71153=CARTESIAN_POINT('Ctrl Pts',(89.2606731197801,56.116120025118,11.8396063344473));
#71154=CARTESIAN_POINT('Ctrl Pts',(89.2617431294994,56.1155154130288,11.8455944017373));
#71155=CARTESIAN_POINT('Ctrl Pts',(89.2648200753046,56.1137106482858,11.8635582632988));
#71156=CARTESIAN_POINT('Ctrl Pts',(89.2666984298799,56.1125172850707,11.8755559638125));
#71157=CARTESIAN_POINT('Ctrl Pts',(89.2795355998673,56.1035953756986,11.9660249481598));
#71158=CARTESIAN_POINT('Ctrl Pts',(89.2833035921784,56.0961986007558,12.0453561360594));
#71159=CARTESIAN_POINT('Ctrl Pts',(89.2770664711368,56.0835222915077,12.1805360965278));
#71160=CARTESIAN_POINT('Ctrl Pts',(89.2707776747942,56.0782724249396,12.236300292316));
#71161=CARTESIAN_POINT('Ctrl Pts',(89.2547558179906,56.06967338265,12.3251153867929));
#71162=CARTESIAN_POINT('Ctrl Pts',(89.2473291266059,56.0663858273598,12.3585049471522));
#71163=CARTESIAN_POINT('Ctrl Pts',(89.2352715835483,56.061804731329,12.4039706853961));
#71164=CARTESIAN_POINT('Ctrl Pts',(89.2317897634942,56.0605477335515,12.4163390052111));
#71165=CARTESIAN_POINT('Ctrl Pts',(89.2255301371041,56.0583927257917,12.4373473727942));
#71166=CARTESIAN_POINT('Ctrl Pts',(89.2228462002056,56.0574978078645,12.4460146070116));
#71167=CARTESIAN_POINT('Ctrl Pts',(89.217554885032,56.0557864982736,12.4624755229777));
#71168=CARTESIAN_POINT('Ctrl Pts',(89.2149642574069,56.0549706963618,12.4702741516469));
#71169=CARTESIAN_POINT('Ctrl Pts',(89.2080310740555,56.0528426303544,12.4904874369771));
#71170=CARTESIAN_POINT('Ctrl Pts',(89.2035711594733,56.0515265653442,12.5028603581536));
#71171=CARTESIAN_POINT('Ctrl Pts',(89.1868779270127,56.0467800386114,12.5470098229965));
#71172=CARTESIAN_POINT('Ctrl Pts',(89.1735613511291,56.0433144859927,12.5783572005425));
#71173=CARTESIAN_POINT('Ctrl Pts',(89.1160653065638,56.0294775439033,12.6998858550423));
#71174=CARTESIAN_POINT('Ctrl Pts',(89.0625202196234,56.0188223565737,12.7852215082493));
#71175=CARTESIAN_POINT('Ctrl Pts',(88.9827458789932,56.0055011559645,12.8841212795644));
#71176=CARTESIAN_POINT('Ctrl Pts',(88.9653353061466,56.0027178139118,12.9043655803217));
#71177=CARTESIAN_POINT('Ctrl Pts',(88.9355485917708,55.9981694145393,12.9368687234744));
#71178=CARTESIAN_POINT('Ctrl Pts',(88.923535876726,55.9963880713386,12.9494482506916));
#71179=CARTESIAN_POINT('Ctrl Pts',(88.9063310241698,55.9939138773543,12.9667393295888));
#71180=CARTESIAN_POINT('Ctrl Pts',(88.901353398134,55.993206772056,12.9716598795706));
#71181=CARTESIAN_POINT('Ctrl Pts',(88.8927310836307,55.9919971384544,12.9800435249064));
#71182=CARTESIAN_POINT('Ctrl Pts',(88.8891061361935,55.9914931340657,12.9835265050985));
#71183=CARTESIAN_POINT('Ctrl Pts',(88.8813455108868,55.9904238334908,12.99089506889));
#71184=CARTESIAN_POINT('Ctrl Pts',(88.8772043515741,55.989858988403,12.9947745812247));
#71185=CARTESIAN_POINT('Ctrl Pts',(88.8657776399523,55.9883155705176,13.0053364212366));
#71186=CARTESIAN_POINT('Ctrl Pts',(88.858439589581,55.9873410869101,13.0119618862341));
#71187=CARTESIAN_POINT('Ctrl Pts',(88.8045545513055,55.9802981323048,13.0594838683586));
#71188=CARTESIAN_POINT('Ctrl Pts',(88.7551381270703,55.9744414043534,13.0970191699342));
#71189=CARTESIAN_POINT('Ctrl Pts',(88.6630723378032,55.9641289183963,13.1568660479542));
#71190=CARTESIAN_POINT('Ctrl Pts',(88.6215361272906,55.9596675673528,13.1806446411991));
#71191=CARTESIAN_POINT('Ctrl Pts',(88.543918809118,55.9515036019351,13.2194359510877));
#71192=CARTESIAN_POINT('Ctrl Pts',(88.5083000618796,55.9478186835245,13.2352344147259));
#71193=CARTESIAN_POINT('Ctrl Pts',(88.4468973566905,55.9415038336806,13.2591555280087));
#71194=CARTESIAN_POINT('Ctrl Pts',(88.4214772632858,55.9389001812605,13.2681375936926));
#71195=CARTESIAN_POINT('Ctrl Pts',(88.3845575805572,55.935119990449,13.2798754967061));
#71196=CARTESIAN_POINT('Ctrl Pts',(88.3732737228104,55.9339648463924,13.2832907271699));
#71197=CARTESIAN_POINT('Ctrl Pts',(88.3533927763155,55.9319288335368,13.2890070985774));
#71198=CARTESIAN_POINT('Ctrl Pts',(88.3448158145241,55.9310502166768,13.2913759293645));
#71199=CARTESIAN_POINT('Ctrl Pts',(88.3268740099108,55.9292112565562,13.2961288493208));
#71200=CARTESIAN_POINT('Ctrl Pts',(88.3175054793968,55.9282504474914,13.2984965533198));
#71201=CARTESIAN_POINT('Ctrl Pts',(88.2927871898879,55.9257132122966,13.3044443468397));
#71202=CARTESIAN_POINT('Ctrl Pts',(88.2773968146136,55.9241312153208,13.3078458440097));
#71203=CARTESIAN_POINT('Ctrl Pts',(88.1945481467689,55.9155984151958,13.3245457455559));
#71204=CARTESIAN_POINT('Ctrl Pts',(88.1261718680012,55.9084877933583,13.3326328507286));
#71205=CARTESIAN_POINT('Ctrl Pts',(87.9877614001459,55.893957779421,13.3377030957457));
#71206=CARTESIAN_POINT('Ctrl Pts',(87.9179401969865,55.8865593934954,13.3345065110059));
#71207=CARTESIAN_POINT('Ctrl Pts',(87.8331161611879,55.8776330889125,13.3235791523053));
#71208=CARTESIAN_POINT('Ctrl Pts',(87.8175355910835,55.8759965277639,13.3212766874952));
#71209=CARTESIAN_POINT('Ctrl Pts',(87.7838623231187,55.8724706459469,13.3156586122435));
#71210=CARTESIAN_POINT('Ctrl Pts',(87.7657897880709,55.8705853008424,13.3122384389581));
#71211=CARTESIAN_POINT('Ctrl Pts',(87.7408026231991,55.8679934735267,13.3069449966079));
#71212=CARTESIAN_POINT('Ctrl Pts',(87.7338212475204,55.8672709481157,13.3054043145988));
#71213=CARTESIAN_POINT('Ctrl Pts',(87.7219310811984,55.8660435663198,13.3026748406931));
#71214=CARTESIAN_POINT('Ctrl Pts',(87.7170158058652,55.8655371155654,13.3015156008071));
#71215=CARTESIAN_POINT('Ctrl Pts',(87.7066607861512,55.8644722731719,13.2990081292537));
#71216=CARTESIAN_POINT('Ctrl Pts',(87.7012228719673,55.8639142658272,13.2976531733077));
#71217=CARTESIAN_POINT('Ctrl Pts',(87.6862795906184,55.8623836775207,13.2938245478341));
#71218=CARTESIAN_POINT('Ctrl Pts',(87.6767933294442,55.8614151677584,13.2912764535884));
#71219=CARTESIAN_POINT('Ctrl Pts',(87.6195498995324,55.8555841546172,13.2751860318623));
#71220=CARTESIAN_POINT('Ctrl Pts',(87.572582548947,55.8508556616082,13.258960999801));
#71221=CARTESIAN_POINT('Ctrl Pts',(87.4545392366518,55.8388110971952,13.2102644351407));
#71222=CARTESIAN_POINT('Ctrl Pts',(87.3852977560678,55.8315797142518,13.1739198630397));
#71223=CARTESIAN_POINT('Ctrl Pts',(87.2834501966439,55.8200797552603,13.1078501448482));
#71224=CARTESIAN_POINT('Ctrl Pts',(87.2483078006617,55.815932636649,13.0824055177643));
#71225=CARTESIAN_POINT('Ctrl Pts',(87.2037137403427,55.8103660620342,13.0465009153038));
#71226=CARTESIAN_POINT('Ctrl Pts',(87.193032891288,55.8090082998732,13.037608420261));
#71227=CARTESIAN_POINT('Ctrl Pts',(87.1818808335678,55.8075631810874,13.028009395259));
#71228=CARTESIAN_POINT('Ctrl Pts',(87.181261574703,55.8074828445688,13.027475332124));
#71229=CARTESIAN_POINT('Ctrl Pts',(87.1806428354183,55.8074024841729,13.0269406741458));
#71230=CARTESIAN_POINT('Origin',(88.011,66.41344859951,12.066));
#71231=CARTESIAN_POINT('',(87.1806429093249,54.843673293217,13.0269407380092));
#71232=CARTESIAN_POINT('',(87.180642810782,55.0125145086225,13.0269406528573));
#71233=CARTESIAN_POINT('',(87.1806428354228,66.41344859951,13.0269406741497));
#71234=CARTESIAN_POINT('',(86.7410003566972,55.527636201329,12.0650481540224));
#71235=CARTESIAN_POINT('Ctrl Pts',(87.1806429093249,54.843673293217,13.0269407380092));
#71236=CARTESIAN_POINT('Ctrl Pts',(87.2040859914023,54.8469114146245,13.0471981052538));
#71237=CARTESIAN_POINT('Ctrl Pts',(87.2282722293485,54.8501250084737,13.0665992097863));
#71238=CARTESIAN_POINT('Ctrl Pts',(87.2611973410103,54.854314497518,13.0910836160516));
#71239=CARTESIAN_POINT('Ctrl Pts',(87.269310677785,54.8553326235955,13.096969165162));
#71240=CARTESIAN_POINT('Ctrl Pts',(87.2821036927062,54.8569149544343,13.1060202251068));
#71241=CARTESIAN_POINT('Ctrl Pts',(87.286735958499,54.8574832670097,13.1092514069836));
#71242=CARTESIAN_POINT('Ctrl Pts',(87.295539915687,54.8585544352337,13.1153055970788));
#71243=CARTESIAN_POINT('Ctrl Pts',(87.2997068940555,54.8590576529505,13.1181347288645));
#71244=CARTESIAN_POINT('Ctrl Pts',(87.3097535865277,54.860262129327,13.1248688691191));
#71245=CARTESIAN_POINT('Ctrl Pts',(87.315649241781,54.8609618021117,13.1287498040497));
#71246=CARTESIAN_POINT('Ctrl Pts',(87.3365033096173,54.8634129124974,13.1422295701707));
#71247=CARTESIAN_POINT('Ctrl Pts',(87.3516316689229,54.8651484473797,13.151564089469));
#71248=CARTESIAN_POINT('Ctrl Pts',(87.3798736032326,54.8683211831377,13.1681815786199));
#71249=CARTESIAN_POINT('Ctrl Pts',(87.3929292084119,54.8697622659677,13.1755554562751));
#71250=CARTESIAN_POINT('Ctrl Pts',(87.4621343540991,54.8772855254863,13.2130421631193));
#71251=CARTESIAN_POINT('Ctrl Pts',(87.5203651361938,54.8832252862192,13.239131800875));
#71252=CARTESIAN_POINT('Ctrl Pts',(87.6461155990688,54.895752141195,13.2844629624941));
#71253=CARTESIAN_POINT('Ctrl Pts',(87.7137551658093,54.9023265285547,13.3027035993879));
#71254=CARTESIAN_POINT('Ctrl Pts',(87.7996961509552,54.9107615380978,13.3184195314639));
#71255=CARTESIAN_POINT('Ctrl Pts',(87.8169090661628,54.9124544530802,13.3212022306194));
#71256=CARTESIAN_POINT('Ctrl Pts',(87.8450749501936,54.9152342164259,13.3251624530921));
#71257=CARTESIAN_POINT('Ctrl Pts',(87.8559960872159,54.9163143840079,13.3265534394645));
#71258=CARTESIAN_POINT('Ctrl Pts',(87.8756884630246,54.9182671961108,13.3288018198912));
#71259=CARTESIAN_POINT('Ctrl Pts',(87.8844532954881,54.9191381847808,13.3297102397482));
#71260=CARTESIAN_POINT('Ctrl Pts',(87.9032829363244,54.9210137277207,13.3314639629091));
#71261=CARTESIAN_POINT('Ctrl Pts',(87.9133497104382,54.9220191192657,13.3322805427928));
#71262=CARTESIAN_POINT('Ctrl Pts',(87.9412239486379,54.9248112037378,13.3342072490425));
#71263=CARTESIAN_POINT('Ctrl Pts',(87.9590458507476,54.9266056709485,13.3350622550181));
#71264=CARTESIAN_POINT('Ctrl Pts',(88.0478320843994,54.9355976370358,13.3374485498738));
#71265=CARTESIAN_POINT('Ctrl Pts',(88.1188044344926,54.9429618308533,13.3334036552168));
#71266=CARTESIAN_POINT('Ctrl Pts',(88.2659077508482,54.9585754415624,13.3125741458312));
#71267=CARTESIAN_POINT('Ctrl Pts',(88.3416059800984,54.966812746604,13.2946684021288));
#71268=CARTESIAN_POINT('Ctrl Pts',(88.4336089358017,54.9768506377623,13.2637807879992));
#71269=CARTESIAN_POINT('Ctrl Pts',(88.4518765132657,54.9788442793576,13.2571780600233));
#71270=CARTESIAN_POINT('Ctrl Pts',(88.4769874971889,54.9815796398335,13.2474448867976));
#71271=CARTESIAN_POINT('Ctrl Pts',(88.4839640122219,54.9823390342727,13.2446693435238));
#71272=CARTESIAN_POINT('Ctrl Pts',(88.4956031690392,54.9836045711307,13.2399188217257));
#71273=CARTESIAN_POINT('Ctrl Pts',(88.5002792391161,54.9841126237765,13.2379775860684));
#71274=CARTESIAN_POINT('Ctrl Pts',(88.5099642874028,54.985163954459,13.2338888378009));
#71275=CARTESIAN_POINT('Ctrl Pts',(88.5149712529474,54.9857069652724,13.2317369677214));
#71276=CARTESIAN_POINT('Ctrl Pts',(88.5283055910584,54.9871521663932,13.2259042260816));
#71277=CARTESIAN_POINT('Ctrl Pts',(88.5366077639636,54.9880510053829,13.2221658117659));
#71278=CARTESIAN_POINT('Ctrl Pts',(88.5797176826314,54.9927171849437,13.2021933176134));
#71279=CARTESIAN_POINT('Ctrl Pts',(88.6138211744567,54.9964047768003,13.1844733402355));
#71280=CARTESIAN_POINT('Ctrl Pts',(88.7479775790189,55.0111206640884,13.1068433184347));
#71281=CARTESIAN_POINT('Ctrl Pts',(88.8403578653001,55.021796356782,13.0348431115575));
#71282=CARTESIAN_POINT('Ctrl Pts',(88.9382898473904,55.0352971196386,12.9341044702504));
#71283=CARTESIAN_POINT('Ctrl Pts',(88.954469432111,55.0376118940403,12.9164922634366));
#71284=CARTESIAN_POINT('Ctrl Pts',(88.9775297832324,55.0410483523088,12.889921869592));
#71285=CARTESIAN_POINT('Ctrl Pts',(88.9848044870047,55.0421538151596,12.8813109039671));
#71286=CARTESIAN_POINT('Ctrl Pts',(88.9975750156283,55.0441341502075,12.865779848812));
#71287=CARTESIAN_POINT('Ctrl Pts',(89.0031151475007,55.0450071667658,12.8588969618853));
#71288=CARTESIAN_POINT('Ctrl Pts',(89.0147282203025,55.0468675605707,12.8441569679154));
#71289=CARTESIAN_POINT('Ctrl Pts',(89.0207816784624,55.0478556355033,12.8362853720696));
#71290=CARTESIAN_POINT('Ctrl Pts',(89.0369620343992,55.0505479179782,12.8147267718992));
#71291=CARTESIAN_POINT('Ctrl Pts',(89.046906550162,55.0522589998692,12.8009064035549));
#71292=CARTESIAN_POINT('Ctrl Pts',(89.063004245015,55.0551271093752,12.7775585499622));
#71293=CARTESIAN_POINT('Ctrl Pts',(89.0693133172775,55.0562781059743,12.7681405865538));
#71294=CARTESIAN_POINT('Ctrl Pts',(89.0934511235522,55.0607896549706,12.7310439898861));
#71295=CARTESIAN_POINT('Ctrl Pts',(89.1103251631192,55.064182084285,12.702763440202));
#71296=CARTESIAN_POINT('Ctrl Pts',(89.1524268988841,55.0733265036068,12.6255308062165));
#71297=CARTESIAN_POINT('Ctrl Pts',(89.1756013966874,55.0791247445234,12.5755415970106));
#71298=CARTESIAN_POINT('Ctrl Pts',(89.2172658428356,55.0913000703415,12.4678407324598));
#71299=CARTESIAN_POINT('Ctrl Pts',(89.2350240401574,55.0976639911057,12.4099772236351));
#71300=CARTESIAN_POINT('Ctrl Pts',(89.2514883187243,55.105188282214,12.3384976405336));
#71301=CARTESIAN_POINT('Ctrl Pts',(89.2541909957703,55.1065029004941,12.3258892597207));
#71302=CARTESIAN_POINT('Ctrl Pts',(89.2579139303162,55.1084381263569,12.3071315949462));
#71303=CARTESIAN_POINT('Ctrl Pts',(89.2590815911228,55.1090661496794,12.3010130711218));
#71304=CARTESIAN_POINT('Ctrl Pts',(89.261098392383,55.1101899056476,12.2900058578985));
#71305=CARTESIAN_POINT('Ctrl Pts',(89.2619639481163,55.1106864984279,12.2851205576061));
#71306=CARTESIAN_POINT('Ctrl Pts',(89.2638498696281,55.1118018617394,12.2741006328399));
#71307=CARTESIAN_POINT('Ctrl Pts',(89.2648538389336,55.1124197138887,12.2679634268865));
#71308=CARTESIAN_POINT('Ctrl Pts',(89.2677924644007,55.1143060562481,12.2491326324625));
#71309=CARTESIAN_POINT('Ctrl Pts',(89.2695798417916,55.1155668227158,12.2364162197954));
#71310=CARTESIAN_POINT('Ctrl Pts',(89.2733559097238,55.1185330416817,12.2062368409889));
#71311=CARTESIAN_POINT('Ctrl Pts',(89.2751756738861,55.120230833799,12.1887549367051));
#71312=CARTESIAN_POINT('Ctrl Pts',(89.2807383164286,55.1266703514273,12.1218574915991));
#71313=CARTESIAN_POINT('Ctrl Pts',(89.2819512812683,55.1313252810911,12.0722719978088));
#71314=CARTESIAN_POINT('Ctrl Pts',(89.2772213003621,55.1443406062693,11.933500151439));
#71315=CARTESIAN_POINT('Ctrl Pts',(89.2647782805744,55.152658992987,11.8448455241119));
#71316=CARTESIAN_POINT('Ctrl Pts',(89.2389976417875,55.1629343391081,11.741631882684));
#71317=CARTESIAN_POINT('Ctrl Pts',(89.2345154236301,55.1645965503466,11.7251146433086));
#71318=CARTESIAN_POINT('Ctrl Pts',(89.226629957002,55.1673363120501,11.6982188610567));
#71319=CARTESIAN_POINT('Ctrl Pts',(89.223424014454,55.1684075071326,11.6877842554212));
#71320=CARTESIAN_POINT('Ctrl Pts',(89.2173897708838,55.170350746179,11.6690097568055));
#71321=CARTESIAN_POINT('Ctrl Pts',(89.2146084302668,55.1712212051891,11.6606553698371));
#71322=CARTESIAN_POINT('Ctrl Pts',(89.2084287552842,55.1731030540761,11.6427178802393));
#71323=CARTESIAN_POINT('Ctrl Pts',(89.2050017838382,55.1741153354815,11.6331454035684));
#71324=CARTESIAN_POINT('Ctrl Pts',(89.195131384984,55.1769474419977,11.6065840806115));
#71325=CARTESIAN_POINT('Ctrl Pts',(89.1884380692579,55.1787754158089,11.5896916658243));
#71326=CARTESIAN_POINT('Ctrl Pts',(89.1765836386218,55.1818680123404,11.5615520411776));
#71327=CARTESIAN_POINT('Ctrl Pts',(89.1716160953457,55.1831260198307,11.5502256168485));
#71328=CARTESIAN_POINT('Ctrl Pts',(89.1511294988949,55.1881688028477,11.5053095428946));
#71329=CARTESIAN_POINT('Ctrl Pts',(89.1343128357946,55.1919934642355,11.472336186666));
#71330=CARTESIAN_POINT('Ctrl Pts',(89.0913196407651,55.2010937002782,11.3964220775805));
#71331=CARTESIAN_POINT('Ctrl Pts',(89.0639845346187,55.2063915789275,11.3542078717234));
#71332=CARTESIAN_POINT('Ctrl Pts',(88.9970197160169,55.2183096331906,11.2631240142454));
#71333=CARTESIAN_POINT('Ctrl Pts',(88.956108102467,55.2249155291813,11.2153427114922));
#71334=CARTESIAN_POINT('Ctrl Pts',(88.9047528117866,55.2323544844298,11.1636660906418));
#71335=CARTESIAN_POINT('Ctrl Pts',(88.8975992649569,55.233373254259,11.1566363000158));
#71336=CARTESIAN_POINT('Ctrl Pts',(88.8862870660021,55.2349563597144,11.1457802096424));
#71337=CARTESIAN_POINT('Ctrl Pts',(88.88218514564,55.2355248094521,11.1418959165428));
#71338=CARTESIAN_POINT('Ctrl Pts',(88.8743774057585,55.2365960735772,11.1346006123904));
#71339=CARTESIAN_POINT('Ctrl Pts',(88.8706771723082,55.2370992512437,11.1311842291833));
#71340=CARTESIAN_POINT('Ctrl Pts',(88.8617445346809,55.2383034116671,11.123034724142));
#71341=CARTESIAN_POINT('Ctrl Pts',(88.8564928188597,55.2390028107782,11.1183230104215));
#71342=CARTESIAN_POINT('Ctrl Pts',(88.8378883669359,55.2414518306441,11.1019093186362));
#71343=CARTESIAN_POINT('Ctrl Pts',(88.8243287911994,55.2431855846127,11.0904429254712));
#71344=CARTESIAN_POINT('Ctrl Pts',(88.7989012496192,55.2463544246719,11.0698395164523));
#71345=CARTESIAN_POINT('Ctrl Pts',(88.787104117171,55.2477933961443,11.0606211956387));
#71346=CARTESIAN_POINT('Ctrl Pts',(88.7243940675556,55.2552984193881,11.0133811955402));
#71347=CARTESIAN_POINT('Ctrl Pts',(88.6708394611965,55.2612227105853,10.9790083287027));
#71348=CARTESIAN_POINT('Ctrl Pts',(88.5476886727734,55.2743416357969,10.9124367230199));
#71349=CARTESIAN_POINT('Ctrl Pts',(88.4773127568304,55.28152812068,10.8822381056674));
#71350=CARTESIAN_POINT('Ctrl Pts',(88.3895815172152,55.2904751576018,10.8536355774732));
#71351=CARTESIAN_POINT('Ctrl Pts',(88.3744152027477,55.2920209245925,10.8490033710182));
#71352=CARTESIAN_POINT('Ctrl Pts',(88.3498532946961,55.2945255657283,10.8420015369077));
#71353=CARTESIAN_POINT('Ctrl Pts',(88.340509922056,55.2954786188591,10.8394532249739));
#71354=CARTESIAN_POINT('Ctrl Pts',(88.3225320028196,55.297313602444,10.8347701629403));
#71355=CARTESIAN_POINT('Ctrl Pts',(88.3139023398703,55.2981949379836,10.8326187683016));
#71356=CARTESIAN_POINT('Ctrl Pts',(88.2938228151596,55.3002473441214,10.8278363318714));
#71357=CARTESIAN_POINT('Ctrl Pts',(88.2823578509034,55.3014205101905,10.8252732344519));
#71358=CARTESIAN_POINT('Ctrl Pts',(88.2447302092167,55.3052763938942,10.8174076884091));
#71359=CARTESIAN_POINT('Ctrl Pts',(88.2184378952367,55.3079796710175,10.8127714422844));
#71360=CARTESIAN_POINT('Ctrl Pts',(88.1540095499799,55.3146331498071,10.8034933107744));
#71361=CARTESIAN_POINT('Ctrl Pts',(88.115773537145,55.3186069334515,10.7997469829524));
#71362=CARTESIAN_POINT('Ctrl Pts',(88.0290696715916,55.3276727565817,10.7952054828988));
#71363=CARTESIAN_POINT('Ctrl Pts',(87.9806059548392,55.33277946252,10.7954407251268));
#71364=CARTESIAN_POINT('Ctrl Pts',(87.8701306723697,55.3444479789913,10.8023018827884));
#71365=CARTESIAN_POINT('Ctrl Pts',(87.8083422543417,55.3509954344047,10.8107273917558));
#71366=CARTESIAN_POINT('Ctrl Pts',(87.7376212181031,55.3583769967046,10.8257321911751));
#71367=CARTESIAN_POINT('Ctrl Pts',(87.7278537306123,55.3593938296147,10.827925523675));
#71368=CARTESIAN_POINT('Ctrl Pts',(87.7126198933929,55.3609746043122,10.8315360770151));
#71369=CARTESIAN_POINT('Ctrl Pts',(87.7071356773418,55.3615426412743,10.8328745630933));
#71370=CARTESIAN_POINT('Ctrl Pts',(87.6967745369339,55.362613617301,10.8354766416908));
#71371=CARTESIAN_POINT('Ctrl Pts',(87.691896145026,55.3631169160003,10.8367326943809));
#71372=CARTESIAN_POINT('Ctrl Pts',(87.6801951740616,55.3643220295458,10.8398197271695));
#71373=CARTESIAN_POINT('Ctrl Pts',(87.6733801378873,55.3650222540222,10.8416786648779));
#71374=CARTESIAN_POINT('Ctrl Pts',(87.6494378289595,55.3674775834151,10.8484245389292));
#71375=CARTESIAN_POINT('Ctrl Pts',(87.6323969113525,55.3692167129644,10.853615150129));
#71376=CARTESIAN_POINT('Ctrl Pts',(87.6011797790079,55.3723973164102,10.8638463035105));
#71377=CARTESIAN_POINT('Ctrl Pts',(87.5869737098363,55.3738426652264,10.868783276847));
#71378=CARTESIAN_POINT('Ctrl Pts',(87.512731499737,55.3814029096302,10.8960717571628));
#71379=CARTESIAN_POINT('Ctrl Pts',(87.4543576003053,55.3873740559487,10.9226914621806));
#71380=CARTESIAN_POINT('Ctrl Pts',(87.3318070338228,55.4004864781314,10.9901984704248));
#71381=CARTESIAN_POINT('Ctrl Pts',(87.2687996584706,55.4076191059062,11.0326619362522));
#71382=CARTESIAN_POINT('Ctrl Pts',(87.1976837476851,55.4165053320255,11.0904657628469));
#71383=CARTESIAN_POINT('Ctrl Pts',(87.1855932716191,55.4180478191361,11.1006741205332));
#71384=CARTESIAN_POINT('Ctrl Pts',(87.1664209338989,55.4205484572738,11.1174854483845));
#71385=CARTESIAN_POINT('Ctrl Pts',(87.1592179998855,55.4215008216204,11.1239484807545));
#71386=CARTESIAN_POINT('Ctrl Pts',(87.1458206712316,55.4232972895803,11.136248870789));
#71387=CARTESIAN_POINT('Ctrl Pts',(87.1396096859145,55.4241405625297,11.1420674566059));
#71388=CARTESIAN_POINT('Ctrl Pts',(87.1255300537694,55.4260767146025,11.1555258105711));
#71389=CARTESIAN_POINT('Ctrl Pts',(87.117701088193,55.4271712929331,11.1632058318453));
#71390=CARTESIAN_POINT('Ctrl Pts',(87.0932318038231,55.4306511313656,11.1878395116583));
#71391=CARTESIAN_POINT('Ctrl Pts',(87.0769684081202,55.4330523134773,11.2051579141156));
#71392=CARTESIAN_POINT('Ctrl Pts',(87.0393535103477,55.438828271075,11.2475342040959));
#71393=CARTESIAN_POINT('Ctrl Pts',(87.0184729813944,55.4422194414489,11.2729849765765));
#71394=CARTESIAN_POINT('Ctrl Pts',(86.9653675261235,55.4513631494686,11.3431006451047));
#71395=CARTESIAN_POINT('Ctrl Pts',(86.9350202891547,55.45716199149,11.3890972209607));
#71396=CARTESIAN_POINT('Ctrl Pts',(86.8778079322664,55.4693395549267,11.4894318498634));
#71397=CARTESIAN_POINT('Ctrl Pts',(86.851645129447,55.4757051118253,11.544029404581));
#71398=CARTESIAN_POINT('Ctrl Pts',(86.8247415664918,55.483230973946,11.6122851503339));
#71399=CARTESIAN_POINT('Ctrl Pts',(86.8201962072513,55.4845456038203,11.6243523923442));
#71400=CARTESIAN_POINT('Ctrl Pts',(86.8137286009386,55.4864808433209,11.642349208719));
#71401=CARTESIAN_POINT('Ctrl Pts',(86.8116651510223,55.4871088688318,11.6482264704523));
#71402=CARTESIAN_POINT('Ctrl Pts',(86.8080359032133,55.488232627002,11.6588120865574));
#71403=CARTESIAN_POINT('Ctrl Pts',(86.8064543751589,55.488729219813,11.6635146512866));
#71404=CARTESIAN_POINT('Ctrl Pts',(86.8029526811489,55.4898445810724,11.6741322361196));
#71405=CARTESIAN_POINT('Ctrl Pts',(86.8010483461148,55.490462431156,11.6800522442026));
#71406=CARTESIAN_POINT('Ctrl Pts',(86.7971388503017,55.491755591094,11.6925190974547));
#71407=CARTESIAN_POINT('Ctrl Pts',(86.7951429817796,55.4924303833304,11.6990686795843));
#71408=CARTESIAN_POINT('Ctrl Pts',(86.7899388940344,55.4942308947352,11.7166550875056));
#71409=CARTESIAN_POINT('Ctrl Pts',(86.7868272490698,55.4953518070467,11.727720235947));
#71410=CARTESIAN_POINT('Ctrl Pts',(86.7554955425682,55.5071464108204,11.8452365619051));
#71411=CARTESIAN_POINT('Ctrl Pts',(86.7410829143962,55.5172338869301,11.9548956180338));
#71412=CARTESIAN_POINT('Ctrl Pts',(86.7410003566972,55.527636201329,12.0650481540224));
#71413=CARTESIAN_POINT('Ctrl Pts',(86.7410003556522,55.5276363331034,12.0650495494126));
#71414=CARTESIAN_POINT('Ctrl Pts',(86.7409762743704,55.5306750427983,12.0972271498695));
#71415=CARTESIAN_POINT('Ctrl Pts',(86.7421751037416,55.5337325688994,12.1293919897642));
#71416=CARTESIAN_POINT('Ctrl Pts',(86.7461044628181,55.5387526504158,12.1815121376383));
#71417=CARTESIAN_POINT('Ctrl Pts',(86.7480903153629,55.5406944456528,12.201509414993));
#71418=CARTESIAN_POINT('Ctrl Pts',(86.7517745285109,55.5436247217039,12.2313824890764));
#71419=CARTESIAN_POINT('Ctrl Pts',(86.7531168155513,55.544602413178,12.2412998468796));
#71420=CARTESIAN_POINT('Ctrl Pts',(86.7557867378001,55.5463977939441,12.2594129926097));
#71421=CARTESIAN_POINT('Ctrl Pts',(86.7570778223769,55.5472143111321,12.2676136990852));
#71422=CARTESIAN_POINT('Ctrl Pts',(86.7599037053006,55.5489020927059,12.2844847499268));
#71423=CARTESIAN_POINT('Ctrl Pts',(86.7614484569822,55.5497736266679,12.2931529352528));
#71424=CARTESIAN_POINT('Ctrl Pts',(86.7651086574365,55.5517314974193,12.3125233620957));
#71425=CARTESIAN_POINT('Ctrl Pts',(86.7672720985356,55.552819295837,12.3232156557579));
#71426=CARTESIAN_POINT('Ctrl Pts',(86.7740470906868,55.5560354678659,12.3546129645832));
#71427=CARTESIAN_POINT('Ctrl Pts',(86.7790396688936,55.5581757116014,12.3752305726424));
#71428=CARTESIAN_POINT('Ctrl Pts',(86.8029216734197,55.5675285441556,12.4640662498715));
#71429=CARTESIAN_POINT('Ctrl Pts',(86.8269758864899,55.5748982163994,12.5307504349586));
#71430=CARTESIAN_POINT('Ctrl Pts',(86.891365947548,55.5911638822733,12.6712633640904));
#71431=CARTESIAN_POINT('Ctrl Pts',(86.933740207904,55.6000562040281,12.7438189421686));
#71432=CARTESIAN_POINT('Ctrl Pts',(86.9893733214197,55.6097541951035,12.8205185549781));
#71433=CARTESIAN_POINT('Ctrl Pts',(86.9959011505201,55.6108662837773,12.8292782420139));
#71434=CARTESIAN_POINT('Ctrl Pts',(87.0062550229444,55.6125893391099,12.8428042573247));
#71435=CARTESIAN_POINT('Ctrl Pts',(87.0100035587952,55.6132051040285,12.8476287184431));
#71436=CARTESIAN_POINT('Ctrl Pts',(87.0165532918571,55.6142669539492,12.8559339862698));
#71437=CARTESIAN_POINT('Ctrl Pts',(87.0193381633471,55.6147141194907,12.859427225468));
#71438=CARTESIAN_POINT('Ctrl Pts',(87.0259595389537,55.6157672058953,12.8676435066403));
#71439=CARTESIAN_POINT('Ctrl Pts',(87.029811639287,55.6163720082429,12.8723537859249));
#71440=CARTESIAN_POINT('Ctrl Pts',(87.0414556854975,55.6181775484707,12.8863849129415));
#71441=CARTESIAN_POINT('Ctrl Pts',(87.0493480404108,55.6193714896878,12.8956222824675));
#71442=CARTESIAN_POINT('Ctrl Pts',(87.0956383874749,55.6262151565257,12.9482529719988));
#71443=CARTESIAN_POINT('Ctrl Pts',(87.1368265374621,55.6316892735561,12.9890786360942));
#71444=CARTESIAN_POINT('Ctrl Pts',(87.1806428950461,55.6371283284805,13.0269407256708));
#71445=CARTESIAN_POINT('Ctrl Pts',(87.1806428354183,55.8074024841729,13.0269406741458));
#71446=CARTESIAN_POINT('Ctrl Pts',(87.1742426907308,55.806571248508,13.0214102536541));
#71447=CARTESIAN_POINT('Ctrl Pts',(87.1678981387326,55.8057374559431,13.015816187997));
#71448=CARTESIAN_POINT('Ctrl Pts',(87.1549254284368,55.8040118150213,13.0041456057867));
#71449=CARTESIAN_POINT('Ctrl Pts',(87.1483050232558,55.8031196747329,12.9980612727825));
#71450=CARTESIAN_POINT('Ctrl Pts',(87.1323477367404,55.8009405552997,12.9830804311961));
#71451=CARTESIAN_POINT('Ctrl Pts',(87.1230809352282,55.7996505157731,12.974111237607));
#71452=CARTESIAN_POINT('Ctrl Pts',(87.0912541366452,55.7951311148999,12.9423536738375));
#71453=CARTESIAN_POINT('Ctrl Pts',(87.0694241995254,55.7918710630158,12.9188556513527));
#71454=CARTESIAN_POINT('Ctrl Pts',(86.9912294539478,55.7795550695985,12.8280212070575));
#71455=CARTESIAN_POINT('Ctrl Pts',(86.9410128016627,55.7702866727908,12.7557322484035));
#71456=CARTESIAN_POINT('Ctrl Pts',(86.8810716336288,55.7572073513683,12.6469390278745));
#71457=CARTESIAN_POINT('Ctrl Pts',(86.8648649784342,55.7533834806886,12.614272950054));
#71458=CARTESIAN_POINT('Ctrl Pts',(86.8413834412009,55.7473839179663,12.5613358715389));
#71459=CARTESIAN_POINT('Ctrl Pts',(86.833179765032,55.7451781626739,12.5414999493231));
#71460=CARTESIAN_POINT('Ctrl Pts',(86.8227673631107,55.7422288238544,12.5143977006385));
#71461=CARTESIAN_POINT('Ctrl Pts',(86.8201157952495,55.741463096499,12.5073072836044));
#71462=CARTESIAN_POINT('Ctrl Pts',(86.8157757990795,55.7401850495687,12.495377883066));
#71463=CARTESIAN_POINT('Ctrl Pts',(86.8140530169991,55.7396708031507,12.4905517419504));
#71464=CARTESIAN_POINT('Ctrl Pts',(86.8105604530218,55.7386139239542,12.4805775255028));
#71465=CARTESIAN_POINT('Ctrl Pts',(86.8087944811187,55.73807151245,12.4754282905537));
#71466=CARTESIAN_POINT('Ctrl Pts',(86.804171467344,55.7366293603664,12.4616606212));
#71467=CARTESIAN_POINT('Ctrl Pts',(86.8013735518153,55.7357329475437,12.4530223607614));
#71468=CARTESIAN_POINT('Ctrl Pts',(86.7885731014044,55.7315129327186,12.4120068692531));
#71469=CARTESIAN_POINT('Ctrl Pts',(86.7797750485167,55.7282502967681,12.379263553727));
#71470=CARTESIAN_POINT('Ctrl Pts',(86.7515634702555,55.7160746554525,12.2545475702932));
#71471=CARTESIAN_POINT('Ctrl Pts',(86.7410660618885,55.7074172420535,12.1608707216829));
#71472=CARTESIAN_POINT('Ctrl Pts',(86.7409697010484,55.6943772943106,12.0231361436092));
#71473=CARTESIAN_POINT('Ctrl Pts',(86.7432000208007,55.6901959042556,11.9794171160793));
#71474=CARTESIAN_POINT('Ctrl Pts',(86.7491444094718,55.6845569953527,11.921692688553));
#71475=CARTESIAN_POINT('Ctrl Pts',(86.750847627602,55.6831618261989,11.9075068137284));
#71476=CARTESIAN_POINT('Ctrl Pts',(86.7540615337585,55.6808406807999,11.884084580041));
#71477=CARTESIAN_POINT('Ctrl Pts',(86.7554356972621,55.6799190312747,11.8748304471702));
#71478=CARTESIAN_POINT('Ctrl Pts',(86.7583385394581,55.6781003474421,11.8566653464927));
#71479=CARTESIAN_POINT('Ctrl Pts',(86.7598603862993,55.6772035809256,11.8477538359257));
#71480=CARTESIAN_POINT('Ctrl Pts',(86.7637428491864,55.6750428498231,11.8263960044005));
#71481=CARTESIAN_POINT('Ctrl Pts',(86.7661947521036,55.6737760704334,11.8139675817289));
#71482=CARTESIAN_POINT('Ctrl Pts',(86.7756699159317,55.6692034389198,11.7694562837635));
#71483=CARTESIAN_POINT('Ctrl Pts',(86.7837503728528,55.6658648468416,11.7376154001105));
#71484=CARTESIAN_POINT('Ctrl Pts',(86.8079302954473,55.6570951543037,11.6557814773996));
#71485=CARTESIAN_POINT('Ctrl Pts',(86.8259113657069,55.6516144725774,11.6064138376836));
#71486=CARTESIAN_POINT('Ctrl Pts',(86.8810744508484,55.6370988190487,11.4799285130019));
#71487=CARTESIAN_POINT('Ctrl Pts',(86.9230879715157,55.6280207865556,11.4051959960656));
#71488=CARTESIAN_POINT('Ctrl Pts',(86.9788828632682,55.618093704215,11.3258884163083));
#71489=CARTESIAN_POINT('Ctrl Pts',(86.9855936752824,55.6169287270587,11.3166183598834));
#71490=CARTESIAN_POINT('Ctrl Pts',(86.9960217540745,55.6151632803129,11.3026158663387));
#71491=CARTESIAN_POINT('Ctrl Pts',(86.9996485730698,55.614557239594,11.2978174227993));
#71492=CARTESIAN_POINT('Ctrl Pts',(87.0063041866729,55.6134596926859,11.2891405961505));
#71493=CARTESIAN_POINT('Ctrl Pts',(87.0093215168426,55.6129674713452,11.2852539275462));
#71494=CARTESIAN_POINT('Ctrl Pts',(87.0163328431421,55.6118358563024,11.2763300901002));
#71495=CARTESIAN_POINT('Ctrl Pts',(87.0203426012824,55.6111975800186,11.2713055653412));
#71496=CARTESIAN_POINT('Ctrl Pts',(87.0331885262414,55.6091798680469,11.255457004686));
#71497=CARTESIAN_POINT('Ctrl Pts',(87.0421657495625,55.6078097918092,11.2447476151732));
#71498=CARTESIAN_POINT('Ctrl Pts',(87.0642164520096,55.6045323564112,11.2193071985131));
#71499=CARTESIAN_POINT('Ctrl Pts',(87.0774597481987,55.6026350127563,11.2047273880955));
#71500=CARTESIAN_POINT('Ctrl Pts',(87.1332602744334,55.5948940046685,11.1460956961943));
#71501=CARTESIAN_POINT('Ctrl Pts',(87.1786407943541,55.5891773623421,11.1048389347805));
#71502=CARTESIAN_POINT('Ctrl Pts',(87.2842425587871,55.5765995191281,11.0219446131959));
#71503=CARTESIAN_POINT('Ctrl Pts',(87.3454292036532,55.5697487153235,10.9819146564514));
#71504=CARTESIAN_POINT('Ctrl Pts',(87.4251268937649,55.5610136695561,10.9390753592568));
#71505=CARTESIAN_POINT('Ctrl Pts',(87.4407148192381,55.5593140832851,10.9311074124511));
#71506=CARTESIAN_POINT('Ctrl Pts',(87.4663830358684,55.556525752762,10.9186491441039));
#71507=CARTESIAN_POINT('Ctrl Pts',(87.4763664114891,55.5554437618659,10.9139633116163));
#71508=CARTESIAN_POINT('Ctrl Pts',(87.494433914038,55.5534891598212,10.9057685044401));
#71509=CARTESIAN_POINT('Ctrl Pts',(87.5024960676586,55.5526182200004,10.9022124827278));
#71510=CARTESIAN_POINT('Ctrl Pts',(87.5198614278259,55.5507444504161,10.8947679283834));
#71511=CARTESIAN_POINT('Ctrl Pts',(87.5291751701245,55.5497407957872,10.8909057565745));
#71512=CARTESIAN_POINT('Ctrl Pts',(87.555023959982,55.5469581441455,10.8805458825034));
#71513=CARTESIAN_POINT('Ctrl Pts',(87.5716500965028,55.5451714577499,10.8742839289602));
#71514=CARTESIAN_POINT('Ctrl Pts',(87.6092450208936,55.5411357282,10.8610180476422));
#71515=CARTESIAN_POINT('Ctrl Pts',(87.6302757887951,55.5388810400453,10.854208972585));
#71516=CARTESIAN_POINT('Ctrl Pts',(87.7240536883532,55.5288349419768,10.8265287804316));
#71517=CARTESIAN_POINT('Ctrl Pts',(87.7983936782144,55.5208784789874,10.8116388117117));
#71518=CARTESIAN_POINT('Ctrl Pts',(87.93391375377,55.5065057028491,10.7968907971071));
#71519=CARTESIAN_POINT('Ctrl Pts',(87.9946253038751,55.5001175917607,10.7946565124833));
#71520=CARTESIAN_POINT('Ctrl Pts',(88.068156867777,55.4925702114449,10.7972213210792));
#71521=CARTESIAN_POINT('Ctrl Pts',(88.0810358988616,55.4912555506162,10.7978670169152));
#71522=CARTESIAN_POINT('Ctrl Pts',(88.1001183802775,55.4893203529465,10.7991153559433));
#71523=CARTESIAN_POINT('Ctrl Pts',(88.1063301887382,55.4886923992545,10.7995676298504));
#71524=CARTESIAN_POINT('Ctrl Pts',(88.1174830587634,55.4875688192735,10.8004621844496));
#71525=CARTESIAN_POINT('Ctrl Pts',(88.1224250866354,55.4870723326713,10.800887729211));
#71526=CARTESIAN_POINT('Ctrl Pts',(88.1335549875207,55.4859572877434,10.8019118236752));
#71527=CARTESIAN_POINT('Ctrl Pts',(88.1397411212455,55.4853396467555,10.8025268613153));
#71528=CARTESIAN_POINT('Ctrl Pts',(88.158682648607,55.4834542227593,10.8045506314272));
#71529=CARTESIAN_POINT('Ctrl Pts',(88.1714220728153,55.4821941541104,10.8061073541215));
#71530=CARTESIAN_POINT('Ctrl Pts',(88.2015334496605,55.479229805268,10.8102510655707));
#71531=CARTESIAN_POINT('Ctrl Pts',(88.2188801142066,55.4775331734065,10.8130058522676));
#71532=CARTESIAN_POINT('Ctrl Pts',(88.2848761166757,55.4711002424619,10.8248950022527));
#71533=CARTESIAN_POINT('Ctrl Pts',(88.3330375722939,55.4664505605265,10.8365112492117));
#71534=CARTESIAN_POINT('Ctrl Pts',(88.4659205023589,55.453431763719,10.8769093455519));
#71535=CARTESIAN_POINT('Ctrl Pts',(88.5484422552698,55.4451050334358,10.9118588672234));
#71536=CARTESIAN_POINT('Ctrl Pts',(88.641569196846,55.4348212070188,10.9634687499155));
#71537=CARTESIAN_POINT('Ctrl Pts',(88.6563626355999,55.4331595936727,10.9720623086464));
#71538=CARTESIAN_POINT('Ctrl Pts',(88.6803008697219,55.4304207292695,10.9866226618151));
#71539=CARTESIAN_POINT('Ctrl Pts',(88.6895507011338,55.4293498282405,10.9924134780315));
#71540=CARTESIAN_POINT('Ctrl Pts',(88.7061252976115,55.4274070730296,11.0030896936527));
#71541=CARTESIAN_POINT('Ctrl Pts',(88.7134761742902,55.4265368025766,11.0079335023704));
#71542=CARTESIAN_POINT('Ctrl Pts',(88.7292058128093,55.4246553110747,11.0185346053922));
#71543=CARTESIAN_POINT('Ctrl Pts',(88.7375669132263,55.4236431984878,11.024316819932));
#71544=CARTESIAN_POINT('Ctrl Pts',(88.7606746721042,55.4208114428163,11.0407107994589));
#71545=CARTESIAN_POINT('Ctrl Pts',(88.7752636493158,55.4189836520927,11.0515390370486));
#71546=CARTESIAN_POINT('Ctrl Pts',(88.7993845043506,55.4158913333416,11.0702576572477));
#71547=CARTESIAN_POINT('Ctrl Pts',(88.8090428748285,55.4146334189762,11.0779815370658));
#71548=CARTESIAN_POINT('Ctrl Pts',(88.8471412925432,55.4095909467583,11.1093722502589));
#71549=CARTESIAN_POINT('Ctrl Pts',(88.8746509048974,55.405766506366,11.1341333708096));
#71550=CARTESIAN_POINT('Ctrl Pts',(88.9368848617311,55.3966663165167,11.1952747129193));
#71551=CARTESIAN_POINT('Ctrl Pts',(88.9706077975009,55.3913682524108,11.2325868244853));
#71552=CARTESIAN_POINT('Ctrl Pts',(89.0413098159751,55.3794494169718,11.3208106873007));
#71553=CARTESIAN_POINT('Ctrl Pts',(89.0769058912529,55.3728429243946,11.3726801033294));
#71554=CARTESIAN_POINT('Ctrl Pts',(89.1135662794786,55.3654035246424,11.4356444259484));
#71555=CARTESIAN_POINT('Ctrl Pts',(89.1185092522852,55.3643848682818,11.4443700221243));
#71556=CARTESIAN_POINT('Ctrl Pts',(89.1260740897032,55.3628019725235,11.4581006053044));
#71557=CARTESIAN_POINT('Ctrl Pts',(89.1287666216006,55.362233619658,11.463065771579));
#71558=CARTESIAN_POINT('Ctrl Pts',(89.1337966887918,55.3611625705363,11.4724909877047));
#71559=CARTESIAN_POINT('Ctrl Pts',(89.1361408579918,55.3606595109032,11.4769470281411));
#71560=CARTESIAN_POINT('Ctrl Pts',(89.1417050304948,55.3594556943809,11.4876783970367));
#71561=CARTESIAN_POINT('Ctrl Pts',(89.1448993854837,55.3587565198449,11.4939668413559));
#71562=CARTESIAN_POINT('Ctrl Pts',(89.1559457301189,55.3563086390901,11.5161689752502));
#71563=CARTESIAN_POINT('Ctrl Pts',(89.1635170235174,55.3545757823827,11.532221482241));
#71564=CARTESIAN_POINT('Ctrl Pts',(89.176846448266,55.3514088117629,11.5620894551549));
#71565=CARTESIAN_POINT('Ctrl Pts',(89.1827013978177,55.3499708120719,11.5758575051926));
#71566=CARTESIAN_POINT('Ctrl Pts',(89.2121126492015,55.3424738820711,11.6485599062844));
#71567=CARTESIAN_POINT('Ctrl Pts',(89.2314720252821,55.3365564301679,11.7091002578572));
#71568=CARTESIAN_POINT('Ctrl Pts',(89.2639912469591,55.3234442438341,11.8451908335917));
#71569=CARTESIAN_POINT('Ctrl Pts',(89.2750056182029,55.3162576590329,11.9209813796044));
#71570=CARTESIAN_POINT('Ctrl Pts',(89.2800006411937,55.3073059920968,12.0131760118662));
#71571=CARTESIAN_POINT('Ctrl Pts',(89.2805626469994,55.3057555702018,12.0290726077536));
#71572=CARTESIAN_POINT('Ctrl Pts',(89.2809864284081,55.3032453774918,12.0546669871657));
#71573=CARTESIAN_POINT('Ctrl Pts',(89.2810359303341,55.3022914774543,12.0643604180708));
#71574=CARTESIAN_POINT('Ctrl Pts',(89.2809181040722,55.3004561840916,12.08294154406));
#71575=CARTESIAN_POINT('Ctrl Pts',(89.2807684311442,55.2995753954288,12.091828821345));
#71576=CARTESIAN_POINT('Ctrl Pts',(89.28020511378,55.2975262485786,12.112430187171));
#71577=CARTESIAN_POINT('Ctrl Pts',(89.2797225635363,55.2963558143991,12.1241413468149));
#71578=CARTESIAN_POINT('Ctrl Pts',(89.277618482419,55.2925183263846,12.1623429421642));
#71579=CARTESIAN_POINT('Ctrl Pts',(89.2753288161302,55.2898309829731,12.188787290903));
#71580=CARTESIAN_POINT('Ctrl Pts',(89.2677401360237,55.2832266061911,12.2529623153027));
#71581=CARTESIAN_POINT('Ctrl Pts',(89.2615687161592,55.2792864589947,12.2905615789233));
#71582=CARTESIAN_POINT('Ctrl Pts',(89.2436656760791,55.2702208523047,12.3755367917411));
#71583=CARTESIAN_POINT('Ctrl Pts',(89.230873951759,55.2650792159383,12.4226295924784));
#71584=CARTESIAN_POINT('Ctrl Pts',(89.1955935016051,55.2533546611971,12.5281036600316));
#71585=CARTESIAN_POINT('Ctrl Pts',(89.1714329956013,55.2467860221635,12.5858069028569));
#71586=CARTESIAN_POINT('Ctrl Pts',(89.1385808577845,55.2393838216216,12.6504328111946));
#71587=CARTESIAN_POINT('Ctrl Pts',(89.1339367853736,55.238366444452,12.6593070878795));
#71588=CARTESIAN_POINT('Ctrl Pts',(89.1265114177256,55.2367850879517,12.6730964887112));
#71589=CARTESIAN_POINT('Ctrl Pts',(89.1238016768983,55.2362170076618,12.678049264468));
#71590=CARTESIAN_POINT('Ctrl Pts',(89.1186123770424,55.2351461490309,12.6873856956811));
#71591=CARTESIAN_POINT('Ctrl Pts',(89.1161397446226,55.2346430097185,12.6917727282085));
#71592=CARTESIAN_POINT('Ctrl Pts',(89.1101387096611,55.2334385649127,12.7022734617776));
#71593=CARTESIAN_POINT('Ctrl Pts',(89.1065853045363,55.2327388462045,12.7083726880008));
#71594=CARTESIAN_POINT('Ctrl Pts',(89.0939019621382,55.2302868082073,12.7297315218877));
#71595=CARTESIAN_POINT('Ctrl Pts',(89.0845019083017,55.2285504098872,12.7448298469503));
#71596=CARTESIAN_POINT('Ctrl Pts',(89.0665912226597,55.2253756918107,12.7722947592354));
#71597=CARTESIAN_POINT('Ctrl Pts',(89.0581729216091,55.2239334930981,12.7847169412609));
#71598=CARTESIAN_POINT('Ctrl Pts',(89.0128106847907,55.2164002903223,12.8491644170682));
#71599=CARTESIAN_POINT('Ctrl Pts',(88.9722019895771,55.2104520684762,12.8985043311548));
#71600=CARTESIAN_POINT('Ctrl Pts',(88.8797238794693,55.197924516813,12.9950313099526));
#71601=CARTESIAN_POINT('Ctrl Pts',(88.8273225951367,55.191358018066,13.0413950201957));
#71602=CARTESIAN_POINT('Ctrl Pts',(88.757429170904,55.1829328304002,13.0936414471728));
#71603=CARTESIAN_POINT('Ctrl Pts',(88.7432643871098,55.181241416312,13.1037823710239));
#71604=CARTESIAN_POINT('Ctrl Pts',(88.7198194208111,55.1784637255298,13.1198482373213));
#71605=CARTESIAN_POINT('Ctrl Pts',(88.7106624332172,55.1773841144651,13.1259497815893));
#71606=CARTESIAN_POINT('Ctrl Pts',(88.6940335493441,55.1754320684973,13.1367206831172));
#71607=CARTESIAN_POINT('Ctrl Pts',(88.6865900351724,55.174561286132,13.1414327990515));
#71608=CARTESIAN_POINT('Ctrl Pts',(88.6705087778154,55.172685927221,13.1513802021207));
#71609=CARTESIAN_POINT('Ctrl Pts',(88.6618564685076,55.1716805118497,13.1565905984606));
#71610=CARTESIAN_POINT('Ctrl Pts',(88.6377439880494,55.1688876621025,13.1707219375318));
#71611=CARTESIAN_POINT('Ctrl Pts',(88.6221572253211,55.1670924441391,13.1794205622875));
#71612=CARTESIAN_POINT('Ctrl Pts',(88.5414031664841,55.1578366459231,13.2222811190804));
#71613=CARTESIAN_POINT('Ctrl Pts',(88.4735533902345,55.1501956800951,13.2510541277681));
#71614=CARTESIAN_POINT('Ctrl Pts',(88.3251768370904,55.1337886744991,13.2992861847797));
#71615=CARTESIAN_POINT('Ctrl Pts',(88.2444405521378,55.1250339102652,13.317083399324));
#71616=CARTESIAN_POINT('Ctrl Pts',(88.1496223296431,55.1152170520254,13.3284789871405));
#71617=CARTESIAN_POINT('Ctrl Pts',(88.1366781178288,55.1138871386668,13.3298332168037));
#71618=CARTESIAN_POINT('Ctrl Pts',(88.1173784652334,55.1119214474161,13.3315528777645));
#71619=CARTESIAN_POINT('Ctrl Pts',(88.111038016509,55.1112784213846,13.3320698502638));
#71620=CARTESIAN_POINT('Ctrl Pts',(88.0996299317929,55.1101266946505,13.3329137766099));
#71621=CARTESIAN_POINT('Ctrl Pts',(88.0945637425395,55.1096170851142,13.3332580193756));
#71622=CARTESIAN_POINT('Ctrl Pts',(88.0840856217954,55.1085670854476,13.333906885253));
#71623=CARTESIAN_POINT('Ctrl Pts',(88.078673579823,55.108026932576,13.3342072655776));
#71624=CARTESIAN_POINT('Ctrl Pts',(88.0642980489005,55.1065975417128,13.3349128499314));
#71625=CARTESIAN_POINT('Ctrl Pts',(88.0553316254386,55.10571152923,13.3352577463317));
#71626=CARTESIAN_POINT('Ctrl Pts',(88.0099968123367,55.1012561373778,13.3365205367272));
#71627=CARTESIAN_POINT('Ctrl Pts',(87.973599452576,55.0977581144267,13.3359706459247));
#71628=CARTESIAN_POINT('Ctrl Pts',(87.8341536538382,55.0844775103858,13.3278615020794));
#71629=CARTESIAN_POINT('Ctrl Pts',(87.7321525664578,55.0749877735975,13.3093080343236));
#71630=CARTESIAN_POINT('Ctrl Pts',(87.600567667142,55.0618650497292,13.2683462474039));
#71631=CARTESIAN_POINT('Ctrl Pts',(87.5680491518291,55.058549161303,13.2567498776087));
#71632=CARTESIAN_POINT('Ctrl Pts',(87.5237892189435,55.0539041175254,13.238902517896));
#71633=CARTESIAN_POINT('Ctrl Pts',(87.5116107164062,55.0526118503887,13.2337692295014));
#71634=CARTESIAN_POINT('Ctrl Pts',(87.4919832333254,55.0505045495865,13.2251329982411));
#71635=CARTESIAN_POINT('Ctrl Pts',(87.48448400245,55.0496934762607,13.221745909812));
#71636=CARTESIAN_POINT('Ctrl Pts',(87.4707144379843,55.0481929128675,13.2153649490223));
#71637=CARTESIAN_POINT('Ctrl Pts',(87.4644346847937,55.0475041670229,13.2123920035873));
#71638=CARTESIAN_POINT('Ctrl Pts',(87.4500943428532,55.0459209956294,13.2054584245364));
#71639=CARTESIAN_POINT('Ctrl Pts',(87.4420508550704,55.0450254120678,13.2014635693395));
#71640=CARTESIAN_POINT('Ctrl Pts',(87.4239617918976,55.0429936471862,13.1922390496625));
#71641=CARTESIAN_POINT('Ctrl Pts',(87.4139426093247,55.0418557866997,13.1869597252703));
#71642=CARTESIAN_POINT('Ctrl Pts',(87.3879970054156,55.0388755238957,13.1728419100577));
#71643=CARTESIAN_POINT('Ctrl Pts',(87.3721884418009,55.0370259961618,13.1637939024786));
#71644=CARTESIAN_POINT('Ctrl Pts',(87.3242346711514,55.0313083839228,13.1349611345074));
#71645=CARTESIAN_POINT('Ctrl Pts',(87.2927754174569,55.0274048953664,13.1140826914261));
#71646=CARTESIAN_POINT('Ctrl Pts',(87.2341947981403,55.0198358239701,13.0713277928951));
#71647=CARTESIAN_POINT('Ctrl Pts',(87.2069545388486,55.0161792082546,13.0496768462902));
#71648=CARTESIAN_POINT('Ctrl Pts',(87.180642810782,55.0125145086225,13.0269406528573));
#71649=CARTESIAN_POINT('Origin',(88.011,66.41344859951,12.066));
#71650=CARTESIAN_POINT('',(87.1806428502938,54.0480645842206,13.0269406869999));
#71651=CARTESIAN_POINT('',(87.1806428209146,54.2176482202995,13.026940661613));
#71652=CARTESIAN_POINT('',(87.1806428354228,66.41344859951,13.0269406741497));
#71653=CARTESIAN_POINT('Ctrl Pts',(87.1806428502938,54.0480645842206,13.0269406869999));
#71654=CARTESIAN_POINT('Ctrl Pts',(87.2477090573159,54.0570744662908,13.0848931759078));
#71655=CARTESIAN_POINT('Ctrl Pts',(87.3206512326996,54.0663624465791,13.1356597057593));
#71656=CARTESIAN_POINT('Ctrl Pts',(87.4397015010786,54.0806929260796,13.2012334320204));
#71657=CARTESIAN_POINT('Ctrl Pts',(87.4823742143646,54.0856792126345,13.2217215612789));
#71658=CARTESIAN_POINT('Ctrl Pts',(87.5419104595419,54.0923744890811,13.2463168583588));
#71659=CARTESIAN_POINT('Ctrl Pts',(87.5578593301287,54.0941433137765,13.2525312891203));
#71660=CARTESIAN_POINT('Ctrl Pts',(87.5857486242469,54.0971889307359,13.2627538226797));
#71661=CARTESIAN_POINT('Ctrl Pts',(87.5976317664102,54.0984719261204,13.2669101512775));
#71662=CARTESIAN_POINT('Ctrl Pts',(87.6154292872799,54.1003699080812,13.2728396252423));
#71663=CARTESIAN_POINT('Ctrl Pts',(87.6212973935762,54.1009919187595,13.2747472664732));
#71664=CARTESIAN_POINT('Ctrl Pts',(87.6314405749286,54.1020603194275,13.2779631288489));
#71665=CARTESIAN_POINT('Ctrl Pts',(87.6357088691582,54.102507837008,13.2792916188988));
#71666=CARTESIAN_POINT('Ctrl Pts',(87.645748951861,54.1035556761566,13.2823585010867));
#71667=CARTESIAN_POINT('Ctrl Pts',(87.6515262348226,54.1041549256366,13.2840783837553));
#71668=CARTESIAN_POINT('Ctrl Pts',(87.6683613237701,54.105891043989,13.288959933899));
#71669=CARTESIAN_POINT('Ctrl Pts',(87.6794505902244,54.1070220041077,13.2920127590006));
#71670=CARTESIAN_POINT('Ctrl Pts',(87.7728223244483,54.1164519402811,13.3163579178208));
#71671=CARTESIAN_POINT('Ctrl Pts',(87.8570265830251,54.1243628567864,13.3294958211391));
#71672=CARTESIAN_POINT('Ctrl Pts',(88.0172320519737,54.1393950326146,13.3382219947221));
#71673=CARTESIAN_POINT('Ctrl Pts',(88.0927404322202,54.1464753687877,13.3356075382403));
#71674=CARTESIAN_POINT('Ctrl Pts',(88.185228383494,54.1554897126628,13.3241181799552));
#71675=CARTESIAN_POINT('Ctrl Pts',(88.2028446655056,54.1572216152083,13.3215526408394));
#71676=CARTESIAN_POINT('Ctrl Pts',(88.2303535972828,54.159953445597,13.3169539712056));
#71677=CARTESIAN_POINT('Ctrl Pts',(88.240286444847,54.1609454693887,13.3151715456174));
#71678=CARTESIAN_POINT('Ctrl Pts',(88.2588516753012,54.1628109023192,13.3116111799338));
#71679=CARTESIAN_POINT('Ctrl Pts',(88.2674889089172,54.1636833678406,13.3098613645371));
#71680=CARTESIAN_POINT('Ctrl Pts',(88.286885439905,54.1656535159112,13.3057212156918));
#71681=CARTESIAN_POINT('Ctrl Pts',(88.2976330668623,54.1667527446516,13.3032804588634));
#71682=CARTESIAN_POINT('Ctrl Pts',(88.3253383064679,54.1696068989774,13.2966083343203));
#71683=CARTESIAN_POINT('Ctrl Pts',(88.342242070599,54.1713683864569,13.2921664064197));
#71684=CARTESIAN_POINT('Ctrl Pts',(88.4258372616374,54.1801851679883,13.2683448435993));
#71685=CARTESIAN_POINT('Ctrl Pts',(88.4909387049016,54.1873983060972,13.2438701369153));
#71686=CARTESIAN_POINT('Ctrl Pts',(88.611610003777,54.2014292398099,13.1868345685225));
#71687=CARTESIAN_POINT('Ctrl Pts',(88.6673656328176,54.2082135193037,13.1551221611906));
#71688=CARTESIAN_POINT('Ctrl Pts',(88.7329627406893,54.2164613650735,13.1109382157457));
#71689=CARTESIAN_POINT('Ctrl Pts',(88.7452839299954,54.218022698036,13.1023171489562));
#71690=CARTESIAN_POINT('Ctrl Pts',(88.7718578539834,54.2214129576133,13.0830115454234));
#71691=CARTESIAN_POINT('Ctrl Pts',(88.7860454957718,54.2232378451739,13.0722413974713));
#71692=CARTESIAN_POINT('Ctrl Pts',(88.805537979194,54.2257614811753,13.0567872076999));
#71693=CARTESIAN_POINT('Ctrl Pts',(88.8110363952888,54.2264752206026,13.0523527087603));
#71694=CARTESIAN_POINT('Ctrl Pts',(88.8203922634826,54.2276925472771,13.0446774435839));
#71695=CARTESIAN_POINT('Ctrl Pts',(88.8242678630225,54.2281976609557,13.0414592572267));
#71696=CARTESIAN_POINT('Ctrl Pts',(88.8324458507645,54.2292652046441,13.0345858663922));
#71697=CARTESIAN_POINT('Ctrl Pts',(88.8367431547146,54.2298272120113,13.0309249262644));
#71698=CARTESIAN_POINT('Ctrl Pts',(88.8485926096838,54.231380306168,13.0206930530893));
#71699=CARTESIAN_POINT('Ctrl Pts',(88.8560919817911,54.2323671237043,13.0140610585623));
#71700=CARTESIAN_POINT('Ctrl Pts',(88.9096270001363,54.2394471597219,12.9655777873724));
#71701=CARTESIAN_POINT('Ctrl Pts',(88.9526197939588,54.2453270079938,12.9204740678232));
#71702=CARTESIAN_POINT('Ctrl Pts',(89.0228343171692,54.2557114919477,12.8350437681715));
#71703=CARTESIAN_POINT('Ctrl Pts',(89.0513718490613,54.2602210338976,12.7959749153529));
#71704=CARTESIAN_POINT('Ctrl Pts',(89.0984998871026,54.2683917568101,12.7230575812023));
#71705=CARTESIAN_POINT('Ctrl Pts',(89.1179057383543,54.2720335301538,12.6898107771316));
#71706=CARTESIAN_POINT('Ctrl Pts',(89.1481839480766,54.2782831438371,12.6320628993527));
#71707=CARTESIAN_POINT('Ctrl Pts',(89.1598450576781,54.2808654590492,12.608004921635));
#71708=CARTESIAN_POINT('Ctrl Pts',(89.1755280676174,54.2846205137263,12.5728654024179));
#71709=CARTESIAN_POINT('Ctrl Pts',(89.180169063428,54.2857722665396,12.5620663614418));
#71710=CARTESIAN_POINT('Ctrl Pts',(89.1880575489933,54.2878045607757,12.542984949286));
#71711=CARTESIAN_POINT('Ctrl Pts',(89.1913692147343,54.2886828784394,12.5347297966354));
#71712=CARTESIAN_POINT('Ctrl Pts',(89.19810400506,54.2905234442968,12.5174175688706));
#71713=CARTESIAN_POINT('Ctrl Pts',(89.201510790377,54.2914861738261,12.5083548180015));
#71714=CARTESIAN_POINT('Ctrl Pts',(89.2102187977816,54.2940337345027,12.4843602808558));
#71715=CARTESIAN_POINT('Ctrl Pts',(89.2153445605503,54.2956242180375,12.4693672899858));
#71716=CARTESIAN_POINT('Ctrl Pts',(89.2418364409257,54.3043735642727,12.3868665002708));
#71717=CARTESIAN_POINT('Ctrl Pts',(89.2578037375673,54.3117025925848,12.3177732913356));
#71718=CARTESIAN_POINT('Ctrl Pts',(89.2762633668814,54.3252455634622,12.1900940851957));
#71719=CARTESIAN_POINT('Ctrl Pts',(89.2806219968887,54.3314088549626,12.1319594085346));
#71720=CARTESIAN_POINT('Ctrl Pts',(89.2811379697643,54.3402940178449,12.0472015834006));
#71721=CARTESIAN_POINT('Ctrl Pts',(89.2804681481531,54.3430600981869,12.0206711824044));
#71722=CARTESIAN_POINT('Ctrl Pts',(89.2779882561083,54.3475837970607,11.9768897239188));
#71723=CARTESIAN_POINT('Ctrl Pts',(89.2766553304923,54.3493574972562,11.9596206247205));
#71724=CARTESIAN_POINT('Ctrl Pts',(89.2742892334432,54.3518231016048,11.9354276097054));
#71725=CARTESIAN_POINT('Ctrl Pts',(89.2735515921043,54.3525291317395,11.9284779217565));
#71726=CARTESIAN_POINT('Ctrl Pts',(89.2721848463212,54.3537376210803,11.9165408217073));
#71727=CARTESIAN_POINT('Ctrl Pts',(89.2715834478049,54.3542415475622,11.9115505312625));
#71728=CARTESIAN_POINT('Ctrl Pts',(89.2702391389431,54.3553114882047,11.9009270749086));
#71729=CARTESIAN_POINT('Ctrl Pts',(89.2694880371334,54.3558770454214,11.895295153289));
#71730=CARTESIAN_POINT('Ctrl Pts',(89.267322496146,54.3574240559171,11.8798492725788));
#71731=CARTESIAN_POINT('Ctrl Pts',(89.2658308382263,54.358401389945,11.8700461854474));
#71732=CARTESIAN_POINT('Ctrl Pts',(89.2540512127098,54.3655289610195,11.7982925755796));
#71733=CARTESIAN_POINT('Ctrl Pts',(89.2392936034383,54.3714616685136,11.7371511551096));
#71734=CARTESIAN_POINT('Ctrl Pts',(89.2046897822339,54.3820784468765,11.629502809415));
#71735=CARTESIAN_POINT('Ctrl Pts',(89.1864861846156,54.3867649475019,11.5826189477322));
#71736=CARTESIAN_POINT('Ctrl Pts',(89.1501395232306,54.3949826696573,11.5033010402599));
#71737=CARTESIAN_POINT('Ctrl Pts',(89.1332648476761,54.3984880830722,11.4703573622825));
#71738=CARTESIAN_POINT('Ctrl Pts',(89.1088639433914,54.4032222577977,11.427448732369));
#71739=CARTESIAN_POINT('Ctrl Pts',(89.1025937278335,54.4044128434394,11.4167881158779));
#71740=CARTESIAN_POINT('Ctrl Pts',(89.0867299602863,54.4073650364963,11.3906962371979));
#71741=CARTESIAN_POINT('Ctrl Pts',(89.0769593875125,54.4091321316522,11.3753766406835));
#71742=CARTESIAN_POINT('Ctrl Pts',(89.0612142031055,54.4119068604515,11.3518196977023));
#71743=CARTESIAN_POINT('Ctrl Pts',(89.0554631582905,54.412906165915,11.3434350737097));
#71744=CARTESIAN_POINT('Ctrl Pts',(89.0445448853187,54.414778064243,11.3279197180957));
#71745=CARTESIAN_POINT('Ctrl Pts',(89.0394029138504,54.415649652086,11.3207718675617));
#71746=CARTESIAN_POINT('Ctrl Pts',(89.0277207864666,54.4176082869813,11.3048837136517));
#71747=CARTESIAN_POINT('Ctrl Pts',(89.0211415235751,54.4186968009592,11.2961732388358));
#71748=CARTESIAN_POINT('Ctrl Pts',(89.0039609977495,54.421503398391,11.274026929334));
#71749=CARTESIAN_POINT('Ctrl Pts',(88.9931993615528,54.4232276788463,11.2607191615827));
#71750=CARTESIAN_POINT('Ctrl Pts',(88.9246385638887,54.4340146355097,11.1793565966288));
#71751=CARTESIAN_POINT('Ctrl Pts',(88.8600784429745,54.4433521928657,11.1173534650959));
#71752=CARTESIAN_POINT('Ctrl Pts',(88.7504133965323,54.4579864547707,11.0322570435867));
#71753=CARTESIAN_POINT('Ctrl Pts',(88.7095071795635,54.4632161236954,11.0041878525694));
#71754=CARTESIAN_POINT('Ctrl Pts',(88.6520138762113,54.4701989999536,10.9695009808637));
#71755=CARTESIAN_POINT('Ctrl Pts',(88.636777377736,54.4720164575826,10.9607345787409));
#71756=CARTESIAN_POINT('Ctrl Pts',(88.6101020486744,54.4751365349092,10.9461153524475));
#71757=CARTESIAN_POINT('Ctrl Pts',(88.5987476183028,54.476445747223,10.940114716542));
#71758=CARTESIAN_POINT('Ctrl Pts',(88.5817618113023,54.4783746130096,10.9314650174533));
#71759=CARTESIAN_POINT('Ctrl Pts',(88.5761994081254,54.4790016146174,10.9286837260942));
#71760=CARTESIAN_POINT('Ctrl Pts',(88.5661628659973,54.4801243441433,10.9237571154769));
#71761=CARTESIAN_POINT('Ctrl Pts',(88.5616963848108,54.4806209240297,10.9215970508617));
#71762=CARTESIAN_POINT('Ctrl Pts',(88.5515941464856,54.4817372519929,10.9167842840366));
#71763=CARTESIAN_POINT('Ctrl Pts',(88.5459513877859,54.482356073601,10.9141467924438));
#71764=CARTESIAN_POINT('Ctrl Pts',(88.5285702088604,54.4842485033881,10.9061779090582));
#71765=CARTESIAN_POINT('Ctrl Pts',(88.516769221134,54.4855143155939,10.9009833710567));
#71766=CARTESIAN_POINT('Ctrl Pts',(88.4493852184585,54.4926468783066,10.8725394146499));
#71767=CARTESIAN_POINT('Ctrl Pts',(88.3922729607955,54.4983296620278,10.8530847994365));
#71768=CARTESIAN_POINT('Ctrl Pts',(88.2389483893888,54.5132076613164,10.8127657149742));
#71769=CARTESIAN_POINT('Ctrl Pts',(88.1413461511993,54.5223294742203,10.7988919380768));
#71770=CARTESIAN_POINT('Ctrl Pts',(88.0253755463014,54.5335505100894,10.7959572057265));
#71771=CARTESIAN_POINT('Ctrl Pts',(88.0076165950491,54.5352782998689,10.7958803859647));
#71772=CARTESIAN_POINT('Ctrl Pts',(87.979781669207,54.5380051150081,10.7963437177765));
#71773=CARTESIAN_POINT('Ctrl Pts',(87.9697031728523,54.5389962852452,10.7966315677761));
#71774=CARTESIAN_POINT('Ctrl Pts',(87.9508229866988,54.540860973131,10.7973958815655));
#71775=CARTESIAN_POINT('Ctrl Pts',(87.9420206846636,54.5417335544161,10.7978440449414));
#71776=CARTESIAN_POINT('Ctrl Pts',(87.9222106291433,54.5437051153804,10.7990595122792));
#71777=CARTESIAN_POINT('Ctrl Pts',(87.9112069527115,54.5448056509134,10.7998787262813));
#71778=CARTESIAN_POINT('Ctrl Pts',(87.8827611864052,54.5476656242003,10.802369592879));
#71779=CARTESIAN_POINT('Ctrl Pts',(87.8653412464594,54.5494316691465,10.8042589615149));
#71780=CARTESIAN_POINT('Ctrl Pts',(87.7756934509989,54.5586012203498,10.8158632782155));
#71781=CARTESIAN_POINT('Ctrl Pts',(87.7043752054558,54.5661800643612,10.8314199710698));
#71782=CARTESIAN_POINT('Ctrl Pts',(87.5762308265137,54.5802955222117,10.871162843861));
#71783=CARTESIAN_POINT('Ctrl Pts',(87.5190543661515,54.586786710843,10.8935452778004));
#71784=CARTESIAN_POINT('Ctrl Pts',(87.4459356331277,54.5952329774468,10.9284629505517));
#71785=CARTESIAN_POINT('Ctrl Pts',(87.4283530001038,54.5972752479509,10.9373676994321));
#71786=CARTESIAN_POINT('Ctrl Pts',(87.3986626946154,54.6007360908112,10.9532833038118));
#71787=CARTESIAN_POINT('Ctrl Pts',(87.3864509019732,54.6021631879937,10.9600913673934));
#71788=CARTESIAN_POINT('Ctrl Pts',(87.3687893437143,54.6042301136872,10.9703235792519));
#71789=CARTESIAN_POINT('Ctrl Pts',(87.3632498850711,54.6048788254373,10.973589298295));
#71790=CARTESIAN_POINT('Ctrl Pts',(87.3535147989339,54.6060193467266,10.9794285890256));
#71791=CARTESIAN_POINT('Ctrl Pts',(87.3493090530997,54.6065122107802,10.9819846332971));
#71792=CARTESIAN_POINT('Ctrl Pts',(87.3399956660237,54.6076039313844,10.9877192527519));
#71793=CARTESIAN_POINT('Ctrl Pts',(87.3348956173438,54.6082020059995,10.9909097455034));
#71794=CARTESIAN_POINT('Ctrl Pts',(87.3201599119126,54.6099313795194,11.0002744580347));
#71795=CARTESIAN_POINT('Ctrl Pts',(87.3105843686005,54.6110568386429,11.0065430943592));
#71796=CARTESIAN_POINT('Ctrl Pts',(87.2302069682482,54.6205309982767,11.0607284363416));
#71797=CARTESIAN_POINT('Ctrl Pts',(87.1643108997441,54.6284864121256,11.1155620438226));
#71798=CARTESIAN_POINT('Ctrl Pts',(87.0676533366749,54.6414183348221,11.2140886685929));
#71799=CARTESIAN_POINT('Ctrl Pts',(87.0332521205014,54.6463437503981,11.2538028991818));
#71800=CARTESIAN_POINT('Ctrl Pts',(86.9814839304115,54.6544823065815,11.3216376320076));
#71801=CARTESIAN_POINT('Ctrl Pts',(86.9625813372398,54.657642476021,11.3485067503935));
#71802=CARTESIAN_POINT('Ctrl Pts',(86.937860065441,54.6620758210487,11.3867127256944));
#71803=CARTESIAN_POINT('Ctrl Pts',(86.9311371766234,54.6633155937145,11.3974517408704));
#71804=CARTESIAN_POINT('Ctrl Pts',(86.9198934952538,54.6654503273698,11.4160243397901));
#71805=CARTESIAN_POINT('Ctrl Pts',(86.9152935351916,54.6663423429489,11.4238091436931));
#71806=CARTESIAN_POINT('Ctrl Pts',(86.9061030147647,54.6681637309044,11.4397490737935));
#71807=CARTESIAN_POINT('Ctrl Pts',(86.9015186985972,54.6690932614997,11.4479071263924));
#71808=CARTESIAN_POINT('Ctrl Pts',(86.8901617304365,54.6714507760458,11.4686509938695));
#71809=CARTESIAN_POINT('Ctrl Pts',(86.8835108308186,54.6728829474553,11.4813014519466));
#71810=CARTESIAN_POINT('Ctrl Pts',(86.8573580728529,54.6787335095887,11.5331518263962));
#71811=CARTESIAN_POINT('Ctrl Pts',(86.8396787641963,54.6832126176885,11.5732299737906));
#71812=CARTESIAN_POINT('Ctrl Pts',(86.7909831271674,54.6973977977161,11.7011366842082));
#71813=CARTESIAN_POINT('Ctrl Pts',(86.767529211037,54.7072893198655,11.7915124924679));
#71814=CARTESIAN_POINT('Ctrl Pts',(86.749121452133,54.720699356509,11.9183681160973));
#71815=CARTESIAN_POINT('Ctrl Pts',(86.7455219099128,54.7243414510373,11.9533122849575));
#71816=CARTESIAN_POINT('Ctrl Pts',(86.7428319437241,54.7288247137774,11.997234203389));
#71817=CARTESIAN_POINT('Ctrl Pts',(86.7423818345657,54.7297257640732,12.0061090960341));
#71818=CARTESIAN_POINT('Ctrl Pts',(86.7418079148009,54.7311667993958,12.0203860522273));
#71819=CARTESIAN_POINT('Ctrl Pts',(86.7416253688206,54.731709810395,12.0257851877751));
#71820=CARTESIAN_POINT('Ctrl Pts',(86.7413377252564,54.7327607548558,12.0362742121381));
#71821=CARTESIAN_POINT('Ctrl Pts',(86.7412287726824,54.7332688610319,12.041363705589));
#71822=CARTESIAN_POINT('Ctrl Pts',(86.7410518012606,54.7344128290737,12.0528610200948));
#71823=CARTESIAN_POINT('Ctrl Pts',(86.7410016692145,54.7350477107754,12.0592689933539));
#71824=CARTESIAN_POINT('Ctrl Pts',(86.7409954393869,54.737467659951,12.0837882439003));
#71825=CARTESIAN_POINT('Ctrl Pts',(86.7413782462323,54.7392356099123,12.1018988784228));
#71826=CARTESIAN_POINT('Ctrl Pts',(86.7428033295998,54.7424795095499,12.1353864192012));
#71827=CARTESIAN_POINT('Ctrl Pts',(86.7437382177276,54.7439592720158,12.1507638011839));
#71828=CARTESIAN_POINT('Ctrl Pts',(86.7502296530399,54.7518249398589,12.2328488985241));
#71829=CARTESIAN_POINT('Ctrl Pts',(86.7607741707956,54.7580558745846,12.2990610896158));
#71830=CARTESIAN_POINT('Ctrl Pts',(86.7933757143798,54.7710769329224,12.4340550311957));
#71831=CARTESIAN_POINT('Ctrl Pts',(86.816166671103,54.7778528761339,12.5023988119153));
#71832=CARTESIAN_POINT('Ctrl Pts',(86.8509282599534,54.7863711478374,12.5830959713173));
#71833=CARTESIAN_POINT('Ctrl Pts',(86.857517285119,54.7879266373817,12.5976316934127));
#71834=CARTESIAN_POINT('Ctrl Pts',(86.8685512176222,54.7904431456659,12.6208017543951));
#71835=CARTESIAN_POINT('Ctrl Pts',(86.8728245161467,54.7913982411413,12.6295164256622));
#71836=CARTESIAN_POINT('Ctrl Pts',(86.8812012190041,54.7932345964088,12.6461152471569));
#71837=CARTESIAN_POINT('Ctrl Pts',(86.8852883481446,54.7941152418322,12.6540070171199));
#71838=CARTESIAN_POINT('Ctrl Pts',(86.8949476552359,54.7961622143243,12.6721881523995));
#71839=CARTESIAN_POINT('Ctrl Pts',(86.9005797756989,54.7973306010337,12.6824444940606));
#71840=CARTESIAN_POINT('Ctrl Pts',(86.9193827947974,54.8011528229406,12.7155916481902));
#71841=CARTESIAN_POINT('Ctrl Pts',(86.9331250331379,54.8038267187554,12.7381478433711));
#71842=CARTESIAN_POINT('Ctrl Pts',(86.9682326824704,54.8103894049703,12.7919246111992));
#71843=CARTESIAN_POINT('Ctrl Pts',(86.9903080281129,54.8143009102124,12.8226488418689));
#71844=CARTESIAN_POINT('Ctrl Pts',(87.0440791960149,54.8233651467671,12.8908445856383));
#71845=CARTESIAN_POINT('Ctrl Pts',(87.0766427135866,54.8285353338819,12.9275569074693));
#71846=CARTESIAN_POINT('Ctrl Pts',(87.1335701734923,54.8370389051246,12.984704319067));
#71847=CARTESIAN_POINT('Ctrl Pts',(87.1567195825001,54.8403688370676,13.0062683871806));
#71848=CARTESIAN_POINT('Ctrl Pts',(87.1806429093249,54.843673293217,13.0269407380092));
#71849=CARTESIAN_POINT('',(86.7410003619504,54.90489047952,12.0650595732259));
#71850=CARTESIAN_POINT('Ctrl Pts',(87.180642810782,55.0125145086225,13.0269406528573));
#71851=CARTESIAN_POINT('Ctrl Pts',(87.1698106884351,55.0110058097381,13.0175805215751));
#71852=CARTESIAN_POINT('Ctrl Pts',(87.1591359293049,55.0094958279517,13.0080364534887));
#71853=CARTESIAN_POINT('Ctrl Pts',(87.102604711212,55.0013776670237,12.9557458148336));
#71854=CARTESIAN_POINT('Ctrl Pts',(87.0597937052197,54.9947847952294,12.9098238037927));
#71855=CARTESIAN_POINT('Ctrl Pts',(87.0142711780043,54.9873587895733,12.8531036237434));
#71856=CARTESIAN_POINT('Ctrl Pts',(87.0080900050372,54.9863406024284,12.8452124382936));
#71857=CARTESIAN_POINT('Ctrl Pts',(86.9985732413489,54.9847582712658,12.8327619884891));
#71858=CARTESIAN_POINT('Ctrl Pts',(86.9951737557381,54.9841900183706,12.828252539949));
#71859=CARTESIAN_POINT('Ctrl Pts',(86.9888000763443,54.9831190391899,12.8196794220616));
#71860=CARTESIAN_POINT('Ctrl Pts',(86.985819930942,54.9826159504102,12.8156206928221));
#71861=CARTESIAN_POINT('Ctrl Pts',(86.9787223153728,54.9814119038054,12.8058327872665));
#71862=CARTESIAN_POINT('Ctrl Pts',(86.9746282856707,54.9807125299567,12.8000868133862));
#71863=CARTESIAN_POINT('Ctrl Pts',(86.9612526646347,54.9784101933249,12.7809791584609));
#71864=CARTESIAN_POINT('Ctrl Pts',(86.9521793093724,54.9768200701466,12.7674723798383));
#71865=CARTESIAN_POINT('Ctrl Pts',(86.890023481675,54.9656912590456,12.670990567327));
#71866=CARTESIAN_POINT('Ctrl Pts',(86.8464848539477,54.9566150649677,12.5822489567285));
#71867=CARTESIAN_POINT('Ctrl Pts',(86.7940489582253,54.9418198833297,12.4339455362181));
#71868=CARTESIAN_POINT('Ctrl Pts',(86.7783309794268,54.9362472325153,12.3772539443391));
#71869=CARTESIAN_POINT('Ctrl Pts',(86.7635088573466,54.9290486303741,12.3045467181843));
#71870=CARTESIAN_POINT('Ctrl Pts',(86.7606994424445,54.9275419707352,12.2893543233547));
#71871=CARTESIAN_POINT('Ctrl Pts',(86.7565952360157,54.9250851736239,12.2646474290017));
#71872=CARTESIAN_POINT('Ctrl Pts',(86.7551299125376,54.924140453901,12.255162426993));
#71873=CARTESIAN_POINT('Ctrl Pts',(86.7525739206633,54.9223554465787,12.2372762686541));
#71874=CARTESIAN_POINT('Ctrl Pts',(86.7514595327371,54.9215159572235,12.2288789729665));
#71875=CARTESIAN_POINT('Ctrl Pts',(86.7493741882523,54.9198113628102,12.2118614279721));
#71876=CARTESIAN_POINT('Ctrl Pts',(86.748407387461,54.9189461736336,12.2032411388734));
#71877=CARTESIAN_POINT('Ctrl Pts',(86.7463769813185,54.9169398262956,12.1832946222166));
#71878=CARTESIAN_POINT('Ctrl Pts',(86.7453771269305,54.9157967451473,12.1719628677395));
#71879=CARTESIAN_POINT('Ctrl Pts',(86.7421536702233,54.9114308722007,12.1288173779079));
#71880=CARTESIAN_POINT('Ctrl Pts',(86.7409767013054,54.9081768245373,12.0969410458204));
#71881=CARTESIAN_POINT('Ctrl Pts',(86.741000349337,54.904890341317,12.0650580255078));
#71882=CARTESIAN_POINT('Ctrl Pts',(86.7410003481916,54.9048905006295,12.0650595710399));
#71883=CARTESIAN_POINT('Ctrl Pts',(86.7410934640266,54.8919284719138,11.9393115527867));
#71884=CARTESIAN_POINT('Ctrl Pts',(86.7598596542112,54.8784526712305,11.8142941249287));
#71885=CARTESIAN_POINT('Ctrl Pts',(86.8000461907814,54.8643085503561,11.6830861840034));
#71886=CARTESIAN_POINT('Ctrl Pts',(86.8035615683117,54.8631294965894,11.672141418893));
#71887=CARTESIAN_POINT('Ctrl Pts',(86.8094072797689,54.8612592606878,11.65475577855));
#71888=CARTESIAN_POINT('Ctrl Pts',(86.8116418267275,54.8605636417918,11.648283763229));
#71889=CARTESIAN_POINT('Ctrl Pts',(86.816005498673,54.8592415412436,11.6359688302902));
#71890=CARTESIAN_POINT('Ctrl Pts',(86.8181254029523,54.8586145936132,11.6301228764736));
#71891=CARTESIAN_POINT('Ctrl Pts',(86.8220134337675,54.8574920245916,11.619641904184));
#71892=CARTESIAN_POINT('Ctrl Pts',(86.8237658511113,54.8569955509263,11.6150014597488));
#71893=CARTESIAN_POINT('Ctrl Pts',(86.8277792241609,54.8558795571868,11.6045594730795));
#71894=CARTESIAN_POINT('Ctrl Pts',(86.8300557092215,54.8552609624051,11.598764136273));
#71895=CARTESIAN_POINT('Ctrl Pts',(86.8371734589993,54.8533695505927,11.581028612118));
#71896=CARTESIAN_POINT('Ctrl Pts',(86.8421541185608,54.8521045189239,11.5691445403283));
#71897=CARTESIAN_POINT('Ctrl Pts',(86.8711897508726,54.845034940732,11.5027187163825));
#71898=CARTESIAN_POINT('Ctrl Pts',(86.898884545489,54.8394103086718,11.4498385398354));
#71899=CARTESIAN_POINT('Ctrl Pts',(86.957438505406,54.828944563975,11.3549450153583));
#71900=CARTESIAN_POINT('Ctrl Pts',(86.9873580027247,54.8241067814038,11.3125095054062));
#71901=CARTESIAN_POINT('Ctrl Pts',(87.0417871436568,54.8158976085815,11.2445594063387));
#71902=CARTESIAN_POINT('Ctrl Pts',(87.0649160702189,54.8125593532128,11.2180241628412));
#71903=CARTESIAN_POINT('Ctrl Pts',(87.1010909933119,54.807510928794,11.1798460780079));
#71904=CARTESIAN_POINT('Ctrl Pts',(87.1133250067429,54.8058307642166,11.1674552232407));
#71905=CARTESIAN_POINT('Ctrl Pts',(87.1361804189124,54.8027357380138,11.1452395062453));
#71906=CARTESIAN_POINT('Ctrl Pts',(87.1467225318601,54.8013243501708,11.1353370087123));
#71907=CARTESIAN_POINT('Ctrl Pts',(87.1577545313864,54.7998624769916,11.1253234555548));
#71908=CARTESIAN_POINT('Ctrl Pts',(87.1580782715222,54.7998195907075,11.1250299069215));
#71909=CARTESIAN_POINT('Ctrl Pts',(87.1587262028293,54.7997337847073,11.1244430097918));
#71910=CARTESIAN_POINT('Ctrl Pts',(87.1590503940878,54.7996908649918,11.1241496614968));
#71911=CARTESIAN_POINT('Ctrl Pts',(87.1597029878005,54.7996044944453,11.1235597669833));
#71912=CARTESIAN_POINT('Ctrl Pts',(87.1600313938301,54.7995610434592,11.1232632249135));
#71913=CARTESIAN_POINT('Ctrl Pts',(87.1606965707766,54.79947306186,11.1226632182742));
#71914=CARTESIAN_POINT('Ctrl Pts',(87.1610333493052,54.7994285309049,11.1223597622975));
#71915=CARTESIAN_POINT('Ctrl Pts',(87.1678875392284,54.7985225122609,11.1161904064832));
#71916=CARTESIAN_POINT('Ctrl Pts',(87.1744651567851,54.7976582896785,11.1103921662719));
#71917=CARTESIAN_POINT('Ctrl Pts',(87.1879067299265,54.7959022483479,11.0987884000115));
#71918=CARTESIAN_POINT('Ctrl Pts',(87.1947733284507,54.7950103352439,11.0929867316224));
#71919=CARTESIAN_POINT('Ctrl Pts',(87.2100650496211,54.7930348550631,11.0803423503396));
#71920=CARTESIAN_POINT('Ctrl Pts',(87.2185173591802,54.7919499913962,11.0735338583841));
#71921=CARTESIAN_POINT('Ctrl Pts',(87.2481870943528,54.7881649774426,11.0502550012664));
#71922=CARTESIAN_POINT('Ctrl Pts',(87.2698371283267,54.7854432180522,11.034351439843));
#71923=CARTESIAN_POINT('Ctrl Pts',(87.3686244663003,54.7731854466729,10.9664996947126));
#71924=CARTESIAN_POINT('Ctrl Pts',(87.4508128749438,54.763381774003,10.9224393986443));
#71925=CARTESIAN_POINT('Ctrl Pts',(87.5721714171492,54.749603050082,10.8736231944838));
#71926=CARTESIAN_POINT('Ctrl Pts',(87.6079083186902,54.7456284260851,10.8610723900173));
#71927=CARTESIAN_POINT('Ctrl Pts',(87.6652083914254,54.7394248306864,10.8437840851159));
#71928=CARTESIAN_POINT('Ctrl Pts',(87.6864251036473,54.7371635848832,10.8379792689086));
#71929=CARTESIAN_POINT('Ctrl Pts',(87.7151996095432,54.7341530222537,10.8309046820618));
#71930=CARTESIAN_POINT('Ctrl Pts',(87.7226318520593,54.7333804158651,10.8291482961644));
#71931=CARTESIAN_POINT('Ctrl Pts',(87.7350895739684,54.7320942028469,10.8263226929633));
#71932=CARTESIAN_POINT('Ctrl Pts',(87.7401063850147,54.7315786160972,10.825216762339));
#71933=CARTESIAN_POINT('Ctrl Pts',(87.7504317359373,54.7305225095385,10.8230062041882));
#71934=CARTESIAN_POINT('Ctrl Pts',(87.7557408629402,54.7299821877035,10.8219050785012));
#71935=CARTESIAN_POINT('Ctrl Pts',(87.7698617672608,54.7285518422606,10.8190705717059));
#71936=CARTESIAN_POINT('Ctrl Pts',(87.7786854314441,54.7276650517673,10.8173965382823));
#71937=CARTESIAN_POINT('Ctrl Pts',(87.81957034491,54.7235849506805,10.8100882597403));
#71938=CARTESIAN_POINT('Ctrl Pts',(87.8518270409986,54.7204477333111,10.8055936472637));
#71939=CARTESIAN_POINT('Ctrl Pts',(87.9514931432954,54.7108998143063,10.7955947677734));
#71940=CARTESIAN_POINT('Ctrl Pts',(88.0191979091881,54.704612275786,10.7942276895338));
#71941=CARTESIAN_POINT('Ctrl Pts',(88.1514390326683,54.6921835303043,10.802123545547));
#71942=CARTESIAN_POINT('Ctrl Pts',(88.2157824777618,54.686064924414,10.8109426972517));
#71943=CARTESIAN_POINT('Ctrl Pts',(88.2965679504061,54.6780710247587,10.8283942569459));
#71944=CARTESIAN_POINT('Ctrl Pts',(88.3138897576757,54.6763387324865,10.8325192545325));
#71945=CARTESIAN_POINT('Ctrl Pts',(88.3408833471298,54.6736065565357,10.8395503245772));
#71946=CARTESIAN_POINT('Ctrl Pts',(88.350617538802,54.672614582483,10.8422100908025));
#71947=CARTESIAN_POINT('Ctrl Pts',(88.3687895050635,54.6707494059505,10.8474088880152));
#71948=CARTESIAN_POINT('Ctrl Pts',(88.377234624666,54.6698771480351,10.8499203077494));
#71949=CARTESIAN_POINT('Ctrl Pts',(88.3961788519711,54.6679076927656,10.8557691896448));
#71950=CARTESIAN_POINT('Ctrl Pts',(88.4066618709041,54.6668089517301,10.8591557571115));
#71951=CARTESIAN_POINT('Ctrl Pts',(88.4336466123747,54.6639565542522,10.8682626131104));
#71952=CARTESIAN_POINT('Ctrl Pts',(88.4500760831121,54.6621963476232,10.8741874633724));
#71953=CARTESIAN_POINT('Ctrl Pts',(88.5354174710193,54.65292354661,10.9069675898494));
#71954=CARTESIAN_POINT('Ctrl Pts',(88.6019939977865,54.6452297135823,10.9394604562044));
#71955=CARTESIAN_POINT('Ctrl Pts',(88.7172631204084,54.6310766496725,11.0087578628638));
#71956=CARTESIAN_POINT('Ctrl Pts',(88.7668756677696,54.624666052473,11.0436394730726));
#71957=CARTESIAN_POINT('Ctrl Pts',(88.8289828577866,54.616312114149,11.0943069292513));
#71958=CARTESIAN_POINT('Ctrl Pts',(88.8438675644932,54.6142830231231,11.1070343507949));
#71959=CARTESIAN_POINT('Ctrl Pts',(88.8688158653228,54.61084206221,11.1293861378105));
#71960=CARTESIAN_POINT('Ctrl Pts',(88.8790261743421,54.6094217857296,11.1388407884696));
#71961=CARTESIAN_POINT('Ctrl Pts',(88.8937161291832,54.6073628928174,11.1528990099708));
#71962=CARTESIAN_POINT('Ctrl Pts',(88.898318983797,54.6067154848059,11.1573712473022));
#71963=CARTESIAN_POINT('Ctrl Pts',(88.9063902915822,54.6055764465913,11.1653333417676));
#71964=CARTESIAN_POINT('Ctrl Pts',(88.9098725923055,54.6050837713722,11.1688086770513));
#71965=CARTESIAN_POINT('Ctrl Pts',(88.9175733017625,54.6039914894095,11.1765838281908));
#71966=CARTESIAN_POINT('Ctrl Pts',(88.9217814276838,54.6033926717779,11.1808935235751));
#71967=CARTESIAN_POINT('Ctrl Pts',(88.9339226836329,54.6016586842055,11.1935061124505));
#71968=CARTESIAN_POINT('Ctrl Pts',(88.9417744173397,54.6005294024667,11.2018872286319));
#71969=CARTESIAN_POINT('Ctrl Pts',(89.0068712655435,54.5910865180717,11.2732901338863));
#71970=CARTESIAN_POINT('Ctrl Pts',(89.0577709229527,54.5831625132236,11.3418279581042));
#71971=CARTESIAN_POINT('Ctrl Pts',(89.1284424505854,54.5702460281034,11.4601961620565));
#71972=CARTESIAN_POINT('Ctrl Pts',(89.1526079268061,54.5653032155488,11.5070666754943));
#71973=CARTESIAN_POINT('Ctrl Pts',(89.187028315973,54.557139897787,11.585436898572));
#71974=CARTESIAN_POINT('Ctrl Pts',(89.1990868389286,54.5539728128097,11.6160747414578));
#71975=CARTESIAN_POINT('Ctrl Pts',(89.2141222022973,54.5495315761257,11.6591121774551));
#71976=CARTESIAN_POINT('Ctrl Pts',(89.2181238957757,54.5482909954441,11.6711422966348));
#71977=CARTESIAN_POINT('Ctrl Pts',(89.2246699800244,54.5461554480458,11.6918517079031));
#71978=CARTESIAN_POINT('Ctrl Pts',(89.2273030520984,54.5452634344613,11.7005022028386));
#71979=CARTESIAN_POINT('Ctrl Pts',(89.2321612988465,54.5435517554946,11.7170972335822));
#71980=CARTESIAN_POINT('Ctrl Pts',(89.2344018803436,54.5427326399951,11.7250368213773));
#71981=CARTESIAN_POINT('Ctrl Pts',(89.2394974019756,54.5407970350535,11.7437901076697));
#71982=CARTESIAN_POINT('Ctrl Pts',(89.2422870999899,54.5396785065264,11.7546205880538));
#71983=CARTESIAN_POINT('Ctrl Pts',(89.2517401826652,54.535666199873,11.7934356705659));
#71984=CARTESIAN_POINT('Ctrl Pts',(89.2575947509803,54.5327473167474,11.8216054367845));
#71985=CARTESIAN_POINT('Ctrl Pts',(89.2779626443844,54.5204791434414,11.9395864339998));
#71986=CARTESIAN_POINT('Ctrl Pts',(89.2837593992223,54.5108837227244,12.0306143038151));
#71987=CARTESIAN_POINT('Ctrl Pts',(89.2775894085617,54.4960029016111,12.1717695457315));
#71988=CARTESIAN_POINT('Ctrl Pts',(89.2723996171966,54.4907233301621,12.2219112243757));
#71989=CARTESIAN_POINT('Ctrl Pts',(89.2622305298388,54.4842847338275,12.2838918446784));
#71990=CARTESIAN_POINT('Ctrl Pts',(89.2600364952113,54.4830172366291,12.2961359821706));
#71991=CARTESIAN_POINT('Ctrl Pts',(89.2564910524735,54.481137620085,12.3143741967708));
#71992=CARTESIAN_POINT('Ctrl Pts',(89.2552755897611,54.4805186646489,12.3203933291233));
#71993=CARTESIAN_POINT('Ctrl Pts',(89.2531003768096,54.4794535699923,12.3307765386684));
#71994=CARTESIAN_POINT('Ctrl Pts',(89.2521612141287,54.4790063256276,12.3351445791839));
#71995=CARTESIAN_POINT('Ctrl Pts',(89.2498955399249,54.4779563316691,12.3454180938682));
#71996=CARTESIAN_POINT('Ctrl Pts',(89.248549837746,54.4773546749522,12.3513191803497));
#71997=CARTESIAN_POINT('Ctrl Pts',(89.2444972534445,54.4756043450149,12.3685220216944));
#71998=CARTESIAN_POINT('Ctrl Pts',(89.2416772565029,54.4744617284442,12.3797970254614));
#71999=CARTESIAN_POINT('Ctrl Pts',(89.2172317356977,54.4651293178242,12.4721319029169));
#72000=CARTESIAN_POINT('Ctrl Pts',(89.1877731304621,54.4573162747194,12.5509215426156));
#72001=CARTESIAN_POINT('Ctrl Pts',(89.1272113055187,54.4444544097837,12.6741278069826));
#72002=CARTESIAN_POINT('Ctrl Pts',(89.1006806900123,54.4394504502596,12.7204786401932));
#72003=CARTESIAN_POINT('Ctrl Pts',(89.0589178918515,54.4322155310729,12.7838269091795));
#72004=CARTESIAN_POINT('Ctrl Pts',(89.0460225595952,54.4300546750574,12.802298548022));
#72005=CARTESIAN_POINT('Ctrl Pts',(89.0219367227628,54.4261339902829,12.8349160033659));
#72006=CARTESIAN_POINT('Ctrl Pts',(89.0109229389182,54.4243807461337,12.8491851099382));
#72007=CARTESIAN_POINT('Ctrl Pts',(88.9932470705487,54.421623027223,12.8711046122149));
#72008=CARTESIAN_POINT('Ctrl Pts',(88.9867902432503,54.4206267134841,12.8789182804297));
#72009=CARTESIAN_POINT('Ctrl Pts',(88.974550504583,54.4187577041039,12.8933741421176));
#72010=CARTESIAN_POINT('Ctrl Pts',(88.9687906385924,54.417885989702,12.9000351483223));
#72011=CARTESIAN_POINT('Ctrl Pts',(88.9557122213166,54.4159234963693,12.9148455603578));
#72012=CARTESIAN_POINT('Ctrl Pts',(88.9483566833082,54.4148312215729,12.9229611399494));
#72013=CARTESIAN_POINT('Ctrl Pts',(88.9291519674401,54.4120075519794,12.9436071780924));
#72014=CARTESIAN_POINT('Ctrl Pts',(88.9171513393755,54.4102698283627,12.9559927357421));
#72015=CARTESIAN_POINT('Ctrl Pts',(88.8436968601303,54.3997841687521,13.0287773962269));
#72016=CARTESIAN_POINT('Ctrl Pts',(88.7764921301597,54.3907823443872,13.0830247520019));
#72017=CARTESIAN_POINT('Ctrl Pts',(88.6610408754983,54.3762572511149,13.1582531509457));
#72018=CARTESIAN_POINT('Ctrl Pts',(88.6160639346775,54.3708013832918,13.1837962122567));
#72019=CARTESIAN_POINT('Ctrl Pts',(88.5534992295892,54.363552929103,13.2144416161539));
#72020=CARTESIAN_POINT('Ctrl Pts',(88.5371777433677,54.3616919650728,13.2220106560987));
#72021=CARTESIAN_POINT('Ctrl Pts',(88.5087332694371,54.3585055580064,13.2344743403046));
#72022=CARTESIAN_POINT('Ctrl Pts',(88.4966856901262,54.3571731644325,13.2395331907957));
#72023=CARTESIAN_POINT('Ctrl Pts',(88.4787524777634,54.3552171244259,13.2467399425524));
#72024=CARTESIAN_POINT('Ctrl Pts',(88.472926195591,54.3545858374817,13.2490314401169));
#72025=CARTESIAN_POINT('Ctrl Pts',(88.4624533947451,54.3534588873235,13.2530612616414));
#72026=CARTESIAN_POINT('Ctrl Pts',(88.4578134106997,54.3529623372208,13.2548155390403));
#72027=CARTESIAN_POINT('Ctrl Pts',(88.4473652911451,54.3518503447489,13.25869593022));
#72028=CARTESIAN_POINT('Ctrl Pts',(88.4415517546531,54.3512357938772,13.2608068637843));
#72029=CARTESIAN_POINT('Ctrl Pts',(88.4237852353928,54.3493696895176,13.267111485281));
#72030=CARTESIAN_POINT('Ctrl Pts',(88.4117841241153,54.3481256235145,13.271169108979));
#72031=CARTESIAN_POINT('Ctrl Pts',(88.3096035819413,54.3376549887867,13.3040214162474));
#72032=CARTESIAN_POINT('Ctrl Pts',(88.2165082314341,54.3288988436078,13.3228351911097));
#72033=CARTESIAN_POINT('Ctrl Pts',(88.0583346645404,54.3139999131475,13.3367343967961));
#72034=CARTESIAN_POINT('Ctrl Pts',(87.9941756024205,54.3079526973779,13.3375035803119));
#72035=CARTESIAN_POINT('Ctrl Pts',(87.9124589523599,54.3000330499152,13.3322966064627));
#72036=CARTESIAN_POINT('Ctrl Pts',(87.894705251123,54.298299672508,13.3307896623789));
#72037=CARTESIAN_POINT('Ctrl Pts',(87.8669531057224,54.2955661733847,13.327844827497));
#72038=CARTESIAN_POINT('Ctrl Pts',(87.8569294897768,54.2945739742299,13.3266601999583));
#72039=CARTESIAN_POINT('Ctrl Pts',(87.8381848255181,54.2927086006077,13.3242180013995));
#72040=CARTESIAN_POINT('Ctrl Pts',(87.8294606070769,54.2918363726147,13.3229888871672));
#72041=CARTESIAN_POINT('Ctrl Pts',(87.8098613366899,54.2898672869698,13.320019348486));
#72042=CARTESIAN_POINT('Ctrl Pts',(87.7989948880798,54.2887688881668,13.3182280547628));
#72043=CARTESIAN_POINT('Ctrl Pts',(87.7709715095677,54.2859180136631,13.313233307976));
#72044=CARTESIAN_POINT('Ctrl Pts',(87.753855569142,54.2841589995986,13.3098172152271));
#72045=CARTESIAN_POINT('Ctrl Pts',(87.6687843221247,54.2753219228958,13.2910073802815));
#72046=CARTESIAN_POINT('Ctrl Pts',(87.6021200901101,54.2680848228393,13.2703952751904));
#72047=CARTESIAN_POINT('Ctrl Pts',(87.4781922404125,54.254044161759,13.2205996898477));
#72048=CARTESIAN_POINT('Ctrl Pts',(87.420772204561,54.247274937073,13.1923286053936));
#72049=CARTESIAN_POINT('Ctrl Pts',(87.3527888283091,54.2390438609256,13.1522244542174));
#72050=CARTESIAN_POINT('Ctrl Pts',(87.33999023972,54.2374845061477,13.1443651804191));
#72051=CARTESIAN_POINT('Ctrl Pts',(87.3123387923966,54.234097917353,13.1267021711953));
#72052=CARTESIAN_POINT('Ctrl Pts',(87.2975457726233,54.2322747226001,13.1168090964369));
#72053=CARTESIAN_POINT('Ctrl Pts',(87.2771794563364,54.2297530917471,13.1025602992714));
#72054=CARTESIAN_POINT('Ctrl Pts',(87.2714282191832,54.2290396927658,13.0984647373534));
#72055=CARTESIAN_POINT('Ctrl Pts',(87.2616335438753,54.2278228412966,13.0913659227947));
#72056=CARTESIAN_POINT('Ctrl Pts',(87.2575733652529,54.2273178644425,13.0883862636069));
#72057=CARTESIAN_POINT('Ctrl Pts',(87.2490001081318,54.2262505054806,13.082015760578));
#72058=CARTESIAN_POINT('Ctrl Pts',(87.2444917672516,54.2256885465556,13.0786188792675));
#72059=CARTESIAN_POINT('Ctrl Pts',(87.2320505764725,54.2241353851996,13.0691141632968));
#72060=CARTESIAN_POINT('Ctrl Pts',(87.2241667767994,54.223148453758,13.0629421903661));
#72061=CARTESIAN_POINT('Ctrl Pts',(87.2042690256248,54.2206480225701,13.046981774004));
#72062=CARTESIAN_POINT('Ctrl Pts',(87.1923625943332,54.2191427597545,13.0370678197031));
#72063=CARTESIAN_POINT('Ctrl Pts',(87.1806428209146,54.2176482202995,13.026940661613));
#72064=CARTESIAN_POINT('Origin',(88.011,66.41344859951,12.066));
#72065=CARTESIAN_POINT('',(87.180642873398,53.2551312395179,13.0269407069644));
#72066=CARTESIAN_POINT('',(87.1806428308131,53.4258009314892,13.0269406701664));
#72067=CARTESIAN_POINT('',(87.1806428354228,66.41344859951,13.0269406741497));
#72068=CARTESIAN_POINT('',(86.7410006142678,53.9404808773293,12.0671672720113));
#72069=CARTESIAN_POINT('Ctrl Pts',(87.180642873398,53.2551312395179,13.0269407069644));
#72070=CARTESIAN_POINT('Ctrl Pts',(87.227200822058,53.2609129875801,13.0671718306847));
#72071=CARTESIAN_POINT('Ctrl Pts',(87.2766258799977,53.2667392828233,13.1039705488038));
#72072=CARTESIAN_POINT('Ctrl Pts',(87.3419097202082,53.2742449419896,13.1455692719022));
#72073=CARTESIAN_POINT('Ctrl Pts',(87.3554449324859,53.2757911838897,13.1538414935601));
#72074=CARTESIAN_POINT('Ctrl Pts',(87.3774884242731,53.2782964046547,13.1667528771713));
#72075=CARTESIAN_POINT('Ctrl Pts',(87.3859014717742,53.2792495575271,13.1715521834217));
#72076=CARTESIAN_POINT('Ctrl Pts',(87.4021431627526,53.2810846073721,13.1805727640856));
#72077=CARTESIAN_POINT('Ctrl Pts',(87.4099629095553,53.281965908476,13.1848089650934));
#72078=CARTESIAN_POINT('Ctrl Pts',(87.4282119803334,53.2840180455739,13.1944485293537));
#72079=CARTESIAN_POINT('Ctrl Pts',(87.438672854058,53.2851909752648,13.1997899159215));
#72080=CARTESIAN_POINT('Ctrl Pts',(87.4731334037261,53.2890451883397,13.2167872697744));
#72081=CARTESIAN_POINT('Ctrl Pts',(87.4974244754101,53.2917470063026,13.2278311941146));
#72082=CARTESIAN_POINT('Ctrl Pts',(87.5574596915302,53.2983959634044,13.2528756537902));
#72083=CARTESIAN_POINT('Ctrl Pts',(87.5935234971836,53.3023666408844,13.2660355517333));
#72084=CARTESIAN_POINT('Ctrl Pts',(87.6763517669119,53.3114324930981,13.2920745537359));
#72085=CARTESIAN_POINT('Ctrl Pts',(87.7233712346569,53.3165424736692,13.3039488656055));
#72086=CARTESIAN_POINT('Ctrl Pts',(87.8321118113701,53.3282161234439,13.3248797660017));
#72087=CARTESIAN_POINT('Ctrl Pts',(87.8940655349541,53.3347654443521,13.3321389991874));
#72088=CARTESIAN_POINT('Ctrl Pts',(87.9663115815308,53.3421488353369,13.3352529899925));
#72089=CARTESIAN_POINT('Ctrl Pts',(87.9763179798554,53.343165726688,13.3355658264261));
#72090=CARTESIAN_POINT('Ctrl Pts',(87.9919715713423,53.3447465717136,13.3358699876128));
#72091=CARTESIAN_POINT('Ctrl Pts',(87.9976164228162,53.3453146211337,13.3359420266138));
#72092=CARTESIAN_POINT('Ctrl Pts',(88.0082991920578,53.3463856058333,13.3360071189668));
#72093=CARTESIAN_POINT('Ctrl Pts',(88.0133366499035,53.3468889008576,13.3360078419431));
#72094=CARTESIAN_POINT('Ctrl Pts',(88.0254374930207,53.3480939855365,13.3359375770154));
#72095=CARTESIAN_POINT('Ctrl Pts',(88.0325005487673,53.3487941850249,13.3358376375378));
#72096=CARTESIAN_POINT('Ctrl Pts',(88.0573668062436,53.3512493231859,13.3352782459652));
#72097=CARTESIAN_POINT('Ctrl Pts',(88.0751621460975,53.3529882897881,13.3345032445289));
#72098=CARTESIAN_POINT('Ctrl Pts',(88.1079409181058,53.3561685364609,13.3323840333867));
#72099=CARTESIAN_POINT('Ctrl Pts',(88.1229274231113,53.3576136917733,13.331147567277));
#72100=CARTESIAN_POINT('Ctrl Pts',(88.2016123289715,53.3651722545157,13.3232463992466));
#72101=CARTESIAN_POINT('Ctrl Pts',(88.2647662196606,53.3711419734209,13.3120360571269));
#72102=CARTESIAN_POINT('Ctrl Pts',(88.3940981054705,53.3836557428268,13.2788322085525));
#72103=CARTESIAN_POINT('Ctrl Pts',(88.4598453548579,53.3901865239372,13.2560679273938));
#72104=CARTESIAN_POINT('Ctrl Pts',(88.539374841443,53.3985779470414,13.2210000080367));
#72105=CARTESIAN_POINT('Ctrl Pts',(88.5552063716418,53.4002735747,13.2136255257334));
#72106=CARTESIAN_POINT('Ctrl Pts',(88.5807690891419,53.4030568699978,13.2010702936736));
#72107=CARTESIAN_POINT('Ctrl Pts',(88.5905942179696,53.4041378277624,13.196084912859));
#72108=CARTESIAN_POINT('Ctrl Pts',(88.608158994077,53.4060914880882,13.186883042628));
#72109=CARTESIAN_POINT('Ctrl Pts',(88.6159220864767,53.4069625285583,13.1827125497895));
#72110=CARTESIAN_POINT('Ctrl Pts',(88.6324828838084,53.4088375414358,13.173592396239));
#72111=CARTESIAN_POINT('Ctrl Pts',(88.641266159136,53.4098423464701,13.1686179957836));
#72112=CARTESIAN_POINT('Ctrl Pts',(88.6653836757304,53.4126310330154,13.1545767484904));
#72113=CARTESIAN_POINT('Ctrl Pts',(88.6805871360927,53.4144226573814,13.1452915810143));
#72114=CARTESIAN_POINT('Ctrl Pts',(88.7057337470706,53.417445128256,13.1291980435367));
#72115=CARTESIAN_POINT('Ctrl Pts',(88.7157848461693,53.418669540422,13.1225620450246));
#72116=CARTESIAN_POINT('Ctrl Pts',(88.7418933031712,53.4218938618913,13.1047862530261));
#72117=CARTESIAN_POINT('Ctrl Pts',(88.7577898985557,53.4239015101202,13.0934174663456));
#72118=CARTESIAN_POINT('Ctrl Pts',(88.8327674971458,53.4335891531515,13.0371361729708));
#72119=CARTESIAN_POINT('Ctrl Pts',(88.8880919137604,53.441417514281,12.9874739654833));
#72120=CARTESIAN_POINT('Ctrl Pts',(88.977981698057,53.4552869895173,12.8913154341149));
#72121=CARTESIAN_POINT('Ctrl Pts',(89.014320546775,53.4613141201742,12.8467362553351));
#72122=CARTESIAN_POINT('Ctrl Pts',(89.0532635774611,53.4681945067787,12.7917309572362));
#72123=CARTESIAN_POINT('Ctrl Pts',(89.0589116240661,53.4692040610727,12.7835514181491));
#72124=CARTESIAN_POINT('Ctrl Pts',(89.067607674981,53.470776074706,12.770636016785));
#72125=CARTESIAN_POINT('Ctrl Pts',(89.0707210090841,53.4713425583696,12.7659450567098));
#72126=CARTESIAN_POINT('Ctrl Pts',(89.0765635827895,53.4724124640642,12.7570135152552));
#72127=CARTESIAN_POINT('Ctrl Pts',(89.0792987988567,53.4729162319831,12.7527773332959));
#72128=CARTESIAN_POINT('Ctrl Pts',(89.0858223890336,53.4741249947116,12.7425406009205));
#72129=CARTESIAN_POINT('Ctrl Pts',(89.0895858520266,53.4748283734369,12.7365243628437));
#72130=CARTESIAN_POINT('Ctrl Pts',(89.1027301802048,53.4773079483199,12.7151148948363));
#72131=CARTESIAN_POINT('Ctrl Pts',(89.1118342568701,53.4790677482175,12.6995526749275));
#72132=CARTESIAN_POINT('Ctrl Pts',(89.1280472963119,53.4822937092311,12.6704331355535));
#72133=CARTESIAN_POINT('Ctrl Pts',(89.1352481784326,53.4837637017494,12.6569316091449));
#72134=CARTESIAN_POINT('Ctrl Pts',(89.1722531185891,53.4915413443748,12.5844217391698));
#72135=CARTESIAN_POINT('Ctrl Pts',(89.1976622421734,53.4976972963418,12.5232792095373));
#72136=CARTESIAN_POINT('Ctrl Pts',(89.2409203861896,53.510754763041,12.3908832282285));
#72137=CARTESIAN_POINT('Ctrl Pts',(89.2575877956678,53.5176441922671,12.3195137660679));
#72138=CARTESIAN_POINT('Ctrl Pts',(89.2702811037403,53.5262742114309,12.2314166371873));
#72139=CARTESIAN_POINT('Ctrl Pts',(89.272248599468,53.5278202924326,12.2156779167385));
#72140=CARTESIAN_POINT('Ctrl Pts',(89.2749419691799,53.5303253168196,12.1902759223732));
#72141=CARTESIAN_POINT('Ctrl Pts',(89.2758529362929,53.5312784358993,12.1806335158943));
#72142=CARTESIAN_POINT('Ctrl Pts',(89.2773886760471,53.533113463287,12.1621187693856));
#72143=CARTESIAN_POINT('Ctrl Pts',(89.278030703806,53.5339947760492,12.1532483926499));
#72144=CARTESIAN_POINT('Ctrl Pts',(89.2793043736349,53.5360470042544,12.1326482825649));
#72145=CARTESIAN_POINT('Ctrl Pts',(89.2798665269275,53.5372200139954,12.1209153052308));
#72146=CARTESIAN_POINT('Ctrl Pts',(89.2811730491244,53.5410747927666,12.082507475488));
#72147=CARTESIAN_POINT('Ctrl Pts',(89.2812394047926,53.5437771048086,12.0558189759272));
#72148=CARTESIAN_POINT('Ctrl Pts',(89.279351549044,53.5504275928278,11.9907820758287));
#72149=CARTESIAN_POINT('Ctrl Pts',(89.2764990454405,53.554399321915,11.9524884125613));
#72150=CARTESIAN_POINT('Ctrl Pts',(89.2661339457825,53.5634651656053,11.8662851949888));
#72151=CARTESIAN_POINT('Ctrl Pts',(89.2576027577796,53.5685740388597,11.8185565934819));
#72152=CARTESIAN_POINT('Ctrl Pts',(89.2319222088054,53.5802459506783,11.7108556917915));
#72153=CARTESIAN_POINT('Ctrl Pts',(89.2130387189582,53.5867946386327,11.651411261068));
#72154=CARTESIAN_POINT('Ctrl Pts',(89.1861418964584,53.5941774091248,11.5842929036424));
#72155=CARTESIAN_POINT('Ctrl Pts',(89.182308366679,53.595194280619,11.5750448732928));
#72156=CARTESIAN_POINT('Ctrl Pts',(89.1761425240416,53.5967751017487,11.5606538169309));
#72157=CARTESIAN_POINT('Ctrl Pts',(89.1738847311767,53.5973431469358,11.5554797039982));
#72158=CARTESIAN_POINT('Ctrl Pts',(89.1695469582974,53.5984141286884,11.545717074907));
#72159=CARTESIAN_POINT('Ctrl Pts',(89.1674741567402,53.5989174249613,11.54112582131));
#72160=CARTESIAN_POINT('Ctrl Pts',(89.1624292812693,53.6001225194474,11.5301264121205));
#72161=CARTESIAN_POINT('Ctrl Pts',(89.159430956467,53.6008227274255,11.523730474059));
#72162=CARTESIAN_POINT('Ctrl Pts',(89.1486857207714,53.6032779305565,11.5012979832534));
#72163=CARTESIAN_POINT('Ctrl Pts',(89.1406544459258,53.6050169525187,11.4853984879923));
#72164=CARTESIAN_POINT('Ctrl Pts',(89.1252304480136,53.6081973204011,11.4563963653593));
#72165=CARTESIAN_POINT('Ctrl Pts',(89.1179346531099,53.6096425414535,11.4432465898851));
#72166=CARTESIAN_POINT('Ctrl Pts',(89.0783432864674,53.6172016754727,11.3747832724085));
#72167=CARTESIAN_POINT('Ctrl Pts',(89.0421284568892,53.6231718792804,11.3218374218185));
#72168=CARTESIAN_POINT('Ctrl Pts',(88.9586340692464,53.6356853680847,11.217640040739));
#72169=CARTESIAN_POINT('Ctrl Pts',(88.9108310694222,53.6422153736724,11.1670969481297));
#72170=CARTESIAN_POINT('Ctrl Pts',(88.8461424890644,53.6506060544648,11.1090558822231));
#72171=CARTESIAN_POINT('Ctrl Pts',(88.8329046808739,53.6523017639449,11.0976624308889));
#72172=CARTESIAN_POINT('Ctrl Pts',(88.8109397090098,53.6550851657703,11.0795326391947));
#72173=CARTESIAN_POINT('Ctrl Pts',(88.8023519489175,53.6561661473626,11.0726302469969));
#72174=CARTESIAN_POINT('Ctrl Pts',(88.7867357361356,53.6581198332789,11.0604097616439));
#72175=CARTESIAN_POINT('Ctrl Pts',(88.779739556562,53.6589908753236,11.0550513642729));
#72176=CARTESIAN_POINT('Ctrl Pts',(88.7646113938964,53.6608658722791,11.0437124892815));
#72177=CARTESIAN_POINT('Ctrl Pts',(88.7564628059474,53.6618706596769,11.0377553416448));
#72178=CARTESIAN_POINT('Ctrl Pts',(88.7337400591966,53.6646592440665,11.0215555977138));
#72179=CARTESIAN_POINT('Ctrl Pts',(88.7190207791399,53.6664507829694,11.0115220266858));
#72180=CARTESIAN_POINT('Ctrl Pts',(88.6855108820365,53.6704992528545,10.9896975309784));
#72181=CARTESIAN_POINT('Ctrl Pts',(88.6666130533864,53.67276188235,10.9780830417959));
#72182=CARTESIAN_POINT('Ctrl Pts',(88.602455349279,53.6803799305159,10.9409308300515));
#72183=CARTESIAN_POINT('Ctrl Pts',(88.5559389544959,53.6858031451973,10.9176794012558));
#72184=CARTESIAN_POINT('Ctrl Pts',(88.4312121177589,53.7000586730948,10.8646217120435));
#72185=CARTESIAN_POINT('Ctrl Pts',(88.3512396705861,53.7089328416846,10.8395712402414));
#72186=CARTESIAN_POINT('Ctrl Pts',(88.2576175200656,53.7187474075095,10.8201171399385));
#72187=CARTESIAN_POINT('Ctrl Pts',(88.2458213257682,53.7199735538201,10.8178400407036));
#72188=CARTESIAN_POINT('Ctrl Pts',(88.2279678130038,53.7218119895713,10.8146557482068));
#72189=CARTESIAN_POINT('Ctrl Pts',(88.2219338513308,53.7224303527924,10.8136245034682));
#72190=CARTESIAN_POINT('Ctrl Pts',(88.2109382800165,53.7235515169876,10.8118270119901));
#72191=CARTESIAN_POINT('Ctrl Pts',(88.2059791600429,53.7240550771237,10.8110464823259));
#72192=CARTESIAN_POINT('Ctrl Pts',(88.1955383257625,53.7251107239863,10.8094665582754));
#72193=CARTESIAN_POINT('Ctrl Pts',(88.1900558198364,53.7256624524202,10.8086735898869));
#72194=CARTESIAN_POINT('Ctrl Pts',(88.1751391518321,53.7271569958738,10.8066156519063));
#72195=CARTESIAN_POINT('Ctrl Pts',(88.165695350603,53.7280960512637,10.8054207815989));
#72196=CARTESIAN_POINT('Ctrl Pts',(88.110183777952,53.7335790675027,10.7990304967894));
#72197=CARTESIAN_POINT('Ctrl Pts',(88.0638650818169,53.738005843388,10.7962535985385));
#72198=CARTESIAN_POINT('Ctrl Pts',(87.9203700546664,53.7515648895685,10.7955202181334));
#72199=CARTESIAN_POINT('Ctrl Pts',(87.8235171925083,53.7605208532554,10.8061656460052));
#72200=CARTESIAN_POINT('Ctrl Pts',(87.6987427862446,53.7727394791197,10.8345994491986));
#72201=CARTESIAN_POINT('Ctrl Pts',(87.668924110744,53.7757102978226,10.8425476629295));
#72202=CARTESIAN_POINT('Ctrl Pts',(87.6272754210389,53.7799532090743,10.8552907325108));
#72203=CARTESIAN_POINT('Ctrl Pts',(87.6151809256083,53.7811966276637,10.8591906882591));
#72204=CARTESIAN_POINT('Ctrl Pts',(87.5946628477819,53.7833268368108,10.8661484911236));
#72205=CARTESIAN_POINT('Ctrl Pts',(87.5862091529078,53.7842105935675,10.8691152964586));
#72206=CARTESIAN_POINT('Ctrl Pts',(87.5701273551783,53.7859039369664,10.8749509997062));
#72207=CARTESIAN_POINT('Ctrl Pts',(87.5624940540122,53.7867129697123,10.8778043853999));
#72208=CARTESIAN_POINT('Ctrl Pts',(87.5429750969172,53.7887957477423,10.885315601271));
#72209=CARTESIAN_POINT('Ctrl Pts',(87.5311316064293,53.7900729717251,10.8900794016814));
#72210=CARTESIAN_POINT('Ctrl Pts',(87.505759343155,53.7928394602801,10.9007319866757));
#72211=CARTESIAN_POINT('Ctrl Pts',(87.4922575138148,53.7943305434619,10.9066795737546));
#72212=CARTESIAN_POINT('Ctrl Pts',(87.4540644936607,53.7986043003359,10.9243044321128));
#72213=CARTESIAN_POINT('Ctrl Pts',(87.4296439162768,53.8014048315963,10.9365440420089));
#72214=CARTESIAN_POINT('Ctrl Pts',(87.338102664363,53.8121704423523,10.9861799518255));
#72215=CARTESIAN_POINT('Ctrl Pts',(87.274036090704,53.8202832533066,11.0288484074807));
#72216=CARTESIAN_POINT('Ctrl Pts',(87.1721700492341,53.8340593509287,11.1109182916318));
#72217=CARTESIAN_POINT('Ctrl Pts',(87.1323115452117,53.8397179275001,11.1474548667143));
#72218=CARTESIAN_POINT('Ctrl Pts',(87.088025414481,53.8462457087994,11.193580191624));
#72219=CARTESIAN_POINT('Ctrl Pts',(87.0812386734784,53.8472532929789,11.2008166058618));
#72220=CARTESIAN_POINT('Ctrl Pts',(87.0707369416348,53.84882293458,11.212280473454));
#72221=CARTESIAN_POINT('Ctrl Pts',(87.0669643006591,53.849388997233,11.2164540908107));
#72222=CARTESIAN_POINT('Ctrl Pts',(87.059862004756,53.8504586166493,11.2244169944347));
#72223=CARTESIAN_POINT('Ctrl Pts',(87.0565271452581,53.8509625155647,11.2282010905067));
#72224=CARTESIAN_POINT('Ctrl Pts',(87.0498840262776,53.8519698519427,11.2358302524024));
#72225=CARTESIAN_POINT('Ctrl Pts',(87.0465761672355,53.8524732570309,11.2396753671932));
#72226=CARTESIAN_POINT('Ctrl Pts',(87.0355052617916,53.8541646747381,11.2527014296199));
#72227=CARTESIAN_POINT('Ctrl Pts',(87.0278491601786,53.8553454513114,11.2619732509114));
#72228=CARTESIAN_POINT('Ctrl Pts',(86.9931989627852,53.8607493197772,11.3051711380689));
#72229=CARTESIAN_POINT('Ctrl Pts',(86.9678177390817,53.8648799917736,11.3403613686492));
#72230=CARTESIAN_POINT('Ctrl Pts',(86.8978245348265,53.8770552709313,11.4486919645222));
#72231=CARTESIAN_POINT('Ctrl Pts',(86.858756279572,53.8849730260875,11.5251088653218));
#72232=CARTESIAN_POINT('Ctrl Pts',(86.8138425110357,53.8967233255252,11.6403654185521));
#72233=CARTESIAN_POINT('Ctrl Pts',(86.8016176322635,53.9003750519474,11.6764560070783));
#72234=CARTESIAN_POINT('Ctrl Pts',(86.787231252252,53.9054097134905,11.7261805659641));
#72235=CARTESIAN_POINT('Ctrl Pts',(86.7836415410765,53.9067467444399,11.7393834450648));
#72236=CARTESIAN_POINT('Ctrl Pts',(86.7782150904638,53.9089070967039,11.7606961253094));
#72237=CARTESIAN_POINT('Ctrl Pts',(86.7762433873895,53.9097260516932,11.7687708148808));
#72238=CARTESIAN_POINT('Ctrl Pts',(86.7723033992911,53.9114365702296,11.7856223395694));
#72239=CARTESIAN_POINT('Ctrl Pts',(86.7703488253289,53.912328520507,11.7944018533713));
#72240=CARTESIAN_POINT('Ctrl Pts',(86.7666474487188,53.9141084381533,11.8119019490776));
#72241=CARTESIAN_POINT('Ctrl Pts',(86.7648986721547,53.914996287898,11.8206215947707));
#72242=CARTESIAN_POINT('Ctrl Pts',(86.7610045829513,53.9170897039602,11.8411542756627));
#72243=CARTESIAN_POINT('Ctrl Pts',(86.7589349747071,53.9182975815157,11.8529805420042));
#72244=CARTESIAN_POINT('Ctrl Pts',(86.7462970460061,53.9263601260066,11.9317589099448));
#72245=CARTESIAN_POINT('Ctrl Pts',(86.7409382294059,53.9333728463356,11.999419128777));
#72246=CARTESIAN_POINT('Ctrl Pts',(86.7410005370969,53.9404808185598,12.0671680007619));
#72247=CARTESIAN_POINT('Ctrl Pts',(86.7410005364398,53.9404807435815,12.0671672861144));
#72248=CARTESIAN_POINT('Ctrl Pts',(86.7410774089203,53.9492556144373,12.1508040292818));
#72249=CARTESIAN_POINT('Ctrl Pts',(86.7494157570709,53.9581444962025,12.2342329466652));
#72250=CARTESIAN_POINT('Ctrl Pts',(86.7688445984371,53.968341402801,12.330902980819));
#72251=CARTESIAN_POINT('Ctrl Pts',(86.7720501381706,53.969878990606,12.345511955724));
#72252=CARTESIAN_POINT('Ctrl Pts',(86.7771489511873,53.9721258255758,12.3669343715233));
#72253=CARTESIAN_POINT('Ctrl Pts',(86.7788420704812,53.9728440139614,12.3737933580615));
#72254=CARTESIAN_POINT('Ctrl Pts',(86.7818560468689,53.9740756904126,12.3855796582954));
#72255=CARTESIAN_POINT('Ctrl Pts',(86.7831494855596,53.9745905597395,12.3905136868546));
#72256=CARTESIAN_POINT('Ctrl Pts',(86.785784663883,53.9756126975312,12.4003246352557));
#72257=CARTESIAN_POINT('Ctrl Pts',(86.7871258895036,53.9761199808866,12.4052016333851));
#72258=CARTESIAN_POINT('Ctrl Pts',(86.7900098943165,53.9771839811387,12.4154486725062));
#72259=CARTESIAN_POINT('Ctrl Pts',(86.7915590183176,53.9777403313606,12.420816726675));
#72260=CARTESIAN_POINT('Ctrl Pts',(86.7959055217669,53.9792611371941,12.4355135363661));
#72261=CARTESIAN_POINT('Ctrl Pts',(86.7987749560635,53.9802216080124,12.4448209455089));
#72262=CARTESIAN_POINT('Ctrl Pts',(86.8161707011016,53.9858048695619,12.4990236134905));
#72263=CARTESIAN_POINT('Ctrl Pts',(86.8330853920197,53.9903068880614,12.5431218244563));
#72264=CARTESIAN_POINT('Ctrl Pts',(86.8820836768189,54.0016038173732,12.6522535615841));
#72265=CARTESIAN_POINT('Ctrl Pts',(86.9173456295729,54.0083221859697,12.7156659144132));
#72266=CARTESIAN_POINT('Ctrl Pts',(86.9854956949888,54.0198335403661,12.8167951369301));
#72267=CARTESIAN_POINT('Ctrl Pts',(87.0155449349726,54.0245513528329,12.8562027721401));
#72268=CARTESIAN_POINT('Ctrl Pts',(87.0573017404777,54.0307715628485,12.9047917088545));
#72269=CARTESIAN_POINT('Ctrl Pts',(87.0669781102026,54.032191910796,12.9156673059788));
#72270=CARTESIAN_POINT('Ctrl Pts',(87.0771017205844,54.0336580390481,12.926659139456));
#72271=CARTESIAN_POINT('Ctrl Pts',(87.077364775672,54.0336961218725,12.9269444921234));
#72272=CARTESIAN_POINT('Ctrl Pts',(87.0778940974583,54.033772725348,12.927518153414));
#72273=CARTESIAN_POINT('Ctrl Pts',(87.0781603670495,54.0338112461138,12.9278064592564));
#72274=CARTESIAN_POINT('Ctrl Pts',(87.0786989203184,54.0338891298909,12.9283890407244));
#72275=CARTESIAN_POINT('Ctrl Pts',(87.0789712097866,54.0339284931401,12.9286833109255));
#72276=CARTESIAN_POINT('Ctrl Pts',(87.0795249682822,54.0340085175775,12.9292812037212));
#72277=CARTESIAN_POINT('Ctrl Pts',(87.0798064465256,54.0340491791475,12.9295848177096));
#72278=CARTESIAN_POINT('Ctrl Pts',(87.0803822894288,54.0341323327005,12.9302053366248));
#72279=CARTESIAN_POINT('Ctrl Pts',(87.0806766675609,54.0341748252385,12.9305222288629));
#72280=CARTESIAN_POINT('Ctrl Pts',(87.0812828050402,54.0342622851492,12.9311740557667));
#72281=CARTESIAN_POINT('Ctrl Pts',(87.081594583547,54.0343072533134,12.9315089723637));
#72282=CARTESIAN_POINT('Ctrl Pts',(87.0822411605697,54.0344004715382,12.9322027817289));
#72283=CARTESIAN_POINT('Ctrl Pts',(87.0825759862102,54.0344487227287,12.9325616489964));
#72284=CARTESIAN_POINT('Ctrl Pts',(87.0832759761026,54.0345495528775,12.9333110291756));
#72285=CARTESIAN_POINT('Ctrl Pts',(87.0836411789779,54.0346021334467,12.9337015056552));
#72286=CARTESIAN_POINT('Ctrl Pts',(87.0844117616438,54.0347130262685,12.9345243737721));
#72287=CARTESIAN_POINT('Ctrl Pts',(87.0848171976186,54.0347713408721,12.9349567123087));
#72288=CARTESIAN_POINT('Ctrl Pts',(87.0856819839576,54.0348956592984,12.9358775884344));
#72289=CARTESIAN_POINT('Ctrl Pts',(87.08614141865,54.0349616666589,12.9363660460818));
#72290=CARTESIAN_POINT('Ctrl Pts',(87.0871342276459,54.0351042199292,12.9374198981166));
#72291=CARTESIAN_POINT('Ctrl Pts',(87.0876677342188,54.0351807714096,12.9379851668015));
#72292=CARTESIAN_POINT('Ctrl Pts',(87.088720540459,54.0353317328197,12.9390986019172));
#72293=CARTESIAN_POINT('Ctrl Pts',(87.0892398107883,54.0354061414805,12.9396467957585));
#72294=CARTESIAN_POINT('Ctrl Pts',(87.0905308512817,54.0355910187751,12.941007315263));
#72295=CARTESIAN_POINT('Ctrl Pts',(87.0913032064837,54.0357015122499,12.9418190814783));
#72296=CARTESIAN_POINT('Ctrl Pts',(87.0981508446169,54.0366801881847,12.9489970881405));
#72297=CARTESIAN_POINT('Ctrl Pts',(87.1042908739419,54.037551123617,12.9553008427873));
#72298=CARTESIAN_POINT('Ctrl Pts',(87.118128539811,54.039499851941,12.969215214179));
#72299=CARTESIAN_POINT('Ctrl Pts',(87.1258588598495,54.0405790426804,12.9767921337576));
#72300=CARTESIAN_POINT('Ctrl Pts',(87.1458321042446,54.043344475069,12.9958745931005));
#72301=CARTESIAN_POINT('Ctrl Pts',(87.1582077453494,54.0450366054679,13.0072372431507));
#72302=CARTESIAN_POINT('Ctrl Pts',(87.174069591308,54.0471802137722,13.0212310982307));
#72303=CARTESIAN_POINT('Ctrl Pts',(87.1773491320214,54.0476220959016,13.0240945565846));
#72304=CARTESIAN_POINT('Ctrl Pts',(87.1806428502938,54.0480645842206,13.0269406869999));
#72305=CARTESIAN_POINT('Ctrl Pts',(87.1806428209146,54.2176482202995,13.026940661613));
#72306=CARTESIAN_POINT('Ctrl Pts',(87.1452504011479,54.2131348764096,12.996357764029));
#72307=CARTESIAN_POINT('Ctrl Pts',(87.1115603032837,54.2087186693022,12.9638305417161));
#72308=CARTESIAN_POINT('Ctrl Pts',(87.0467713246626,54.1997705438192,12.8939570940156));
#72309=CARTESIAN_POINT('Ctrl Pts',(87.0158741148475,54.1952486465662,12.8565531707686));
#72310=CARTESIAN_POINT('Ctrl Pts',(86.9644944811698,54.1870763956072,12.7865535725928));
#72311=CARTESIAN_POINT('Ctrl Pts',(86.9432127007455,54.1834459049798,12.7546225877747));
#72312=CARTESIAN_POINT('Ctrl Pts',(86.9096381452467,54.1772134858484,12.6989402662999));
#72313=CARTESIAN_POINT('Ctrl Pts',(86.8965905957655,54.174636889643,12.6756743072217));
#72314=CARTESIAN_POINT('Ctrl Pts',(86.8788676274429,54.1708887549885,12.6415989755517));
#72315=CARTESIAN_POINT('Ctrl Pts',(86.8735941890102,54.1697380961456,12.6311069706101));
#72316=CARTESIAN_POINT('Ctrl Pts',(86.8645847070452,54.1677072020006,12.612544633227));
#72317=CARTESIAN_POINT('Ctrl Pts',(86.8607864545929,54.1668291826751,12.6045051994745));
#72318=CARTESIAN_POINT('Ctrl Pts',(86.8530285148853,54.1649887233119,12.587628043773));
#72319=CARTESIAN_POINT('Ctrl Pts',(86.8490848963894,54.1640257985537,12.5787836337886));
#72320=CARTESIAN_POINT('Ctrl Pts',(86.8389503302454,54.1614765140877,12.5553374099452));
#72321=CARTESIAN_POINT('Ctrl Pts',(86.8329313494374,54.1598844859821,12.5406638022288));
#72322=CARTESIAN_POINT('Ctrl Pts',(86.8006921590715,54.1508945143421,12.4576749218825));
#72323=CARTESIAN_POINT('Ctrl Pts',(86.7801458233677,54.1433138737863,12.3873216522661));
#72324=CARTESIAN_POINT('Ctrl Pts',(86.7527767831557,54.1286851747907,12.2507841957157));
#72325=CARTESIAN_POINT('Ctrl Pts',(86.744864362002,54.121679725967,12.1850450812428));
#72326=CARTESIAN_POINT('Ctrl Pts',(86.7414675389801,54.113186815787,12.1037015291466));
#72327=CARTESIAN_POINT('Ctrl Pts',(86.7411054460214,54.1115976140026,12.0884042004117));
#72328=CARTESIAN_POINT('Ctrl Pts',(86.7409190489905,54.1081570085854,12.0550785338904));
#72329=CARTESIAN_POINT('Ctrl Pts',(86.741201971086,54.1063096229264,12.0370520622072));
#72330=CARTESIAN_POINT('Ctrl Pts',(86.7421310113146,54.1037606345058,12.011946066198));
#72331=CARTESIAN_POINT('Ctrl Pts',(86.7424527987386,54.1030436523913,12.0048579929283));
#72332=CARTESIAN_POINT('Ctrl Pts',(86.7431048214481,54.1018226752449,11.9927386083271));
#72333=CARTESIAN_POINT('Ctrl Pts',(86.7434056364446,54.1013171283638,11.987706005492));
#72334=CARTESIAN_POINT('Ctrl Pts',(86.7441057043148,54.1002507981529,11.9770588902709));
#72335=CARTESIAN_POINT('Ctrl Pts',(86.7445123191759,54.0996904225213,11.9714450620343));
#72336=CARTESIAN_POINT('Ctrl Pts',(86.7457398629063,54.0981463162111,11.9559295892261));
#72337=CARTESIAN_POINT('Ctrl Pts',(86.7466397088983,54.0971667758778,11.9460342270354));
#72338=CARTESIAN_POINT('Ctrl Pts',(86.753462231243,54.0906247524847,11.8796561964146));
#72339=CARTESIAN_POINT('Ctrl Pts',(86.7630528461093,54.0852392204285,11.8236043980689));
#72340=CARTESIAN_POINT('Ctrl Pts',(86.7938720768371,54.0728695065694,11.6957581542139));
#72341=CARTESIAN_POINT('Ctrl Pts',(86.8177483610913,54.0659350576208,11.6248317152101));
#72342=CARTESIAN_POINT('Ctrl Pts',(86.8585329065731,54.0562880486032,11.5317285163744));
#72343=CARTESIAN_POINT('Ctrl Pts',(86.8701297135073,54.0537136447811,11.5073935156067));
#72344=CARTESIAN_POINT('Ctrl Pts',(86.8919621904196,54.0491248629058,11.4651000828709));
#72345=CARTESIAN_POINT('Ctrl Pts',(86.9018787347758,54.0471210451209,11.4469876943142));
#72346=CARTESIAN_POINT('Ctrl Pts',(86.9175787775237,54.0440589315388,11.4199011502146));
#72347=CARTESIAN_POINT('Ctrl Pts',(86.9230416266576,54.0430120750963,11.410744130681));
#72348=CARTESIAN_POINT('Ctrl Pts',(86.9327696084529,54.041178843936,11.3948948051827));
#72349=CARTESIAN_POINT('Ctrl Pts',(86.93698345927,54.0403943776376,11.3881715388263));
#72350=CARTESIAN_POINT('Ctrl Pts',(86.946672078271,54.0386118204885,11.3730303725156));
#72351=CARTESIAN_POINT('Ctrl Pts',(86.9521841608399,54.0376123875257,11.3646371598997));
#72352=CARTESIAN_POINT('Ctrl Pts',(86.9673556778885,54.0348997894766,11.3421220773424));
#72353=CARTESIAN_POINT('Ctrl Pts',(86.9772014826095,54.033179731932,11.3281292321384));
#72354=CARTESIAN_POINT('Ctrl Pts',(87.049229071842,54.020867390024,11.2300359650397));
#72355=CARTESIAN_POINT('Ctrl Pts',(87.1212936806378,54.0098816986994,11.1537224746171));
#72356=CARTESIAN_POINT('Ctrl Pts',(87.233316938063,53.9945638770265,11.0611248684566));
#72357=CARTESIAN_POINT('Ctrl Pts',(87.2660047324878,53.9902734837296,11.036656733222));
#72358=CARTESIAN_POINT('Ctrl Pts',(87.3189208879931,53.983647056243,11.000890510969));
#72359=CARTESIAN_POINT('Ctrl Pts',(87.3383755947283,53.9812739783418,10.9884990219838));
#72360=CARTESIAN_POINT('Ctrl Pts',(87.3648208636924,53.978140601786,10.9726506307202));
#72361=CARTESIAN_POINT('Ctrl Pts',(87.3715195148245,53.9773546256594,10.9687192520859));
#72362=CARTESIAN_POINT('Ctrl Pts',(87.3827303395892,53.9760524813875,10.9622772602455));
#72363=CARTESIAN_POINT('Ctrl Pts',(87.3872223883075,53.9755342291853,10.9597323342925));
#72364=CARTESIAN_POINT('Ctrl Pts',(87.3958519078256,53.9745454739766,10.954912643268));
#72365=CARTESIAN_POINT('Ctrl Pts',(87.3999867131435,53.974074679926,10.9526334585611));
#72366=CARTESIAN_POINT('Ctrl Pts',(87.411285725228,53.9727959279774,10.9464871301954));
#72367=CARTESIAN_POINT('Ctrl Pts',(87.4184747782267,53.9719907666679,10.9426656101503));
#72368=CARTESIAN_POINT('Ctrl Pts',(87.4471279635553,53.9688128720373,10.9277859233527));
#72369=CARTESIAN_POINT('Ctrl Pts',(87.4688709215971,53.9664702359408,10.9172705776264));
#72370=CARTESIAN_POINT('Ctrl Pts',(87.5582283065022,53.9570613150049,10.8771586054341));
#72371=CARTESIAN_POINT('Ctrl Pts',(87.6280679556381,53.9501984395087,10.8528587190258));
#72372=CARTESIAN_POINT('Ctrl Pts',(87.770028122764,53.9364695387322,10.816958237326));
#72373=CARTESIAN_POINT('Ctrl Pts',(87.8418107444953,53.9296293366728,10.8052284554274));
#72374=CARTESIAN_POINT('Ctrl Pts',(87.9298719804741,53.9210645337955,10.7984963534869));
#72375=CARTESIAN_POINT('Ctrl Pts',(87.9455704471089,53.9195315420915,10.7975891159698));
#72376=CARTESIAN_POINT('Ctrl Pts',(87.9709288032017,53.9170426217436,10.7965956025956));
#72377=CARTESIAN_POINT('Ctrl Pts',(87.980580366757,53.9160923817299,10.7963276572004));
#72378=CARTESIAN_POINT('Ctrl Pts',(87.9991331974031,53.9142594960961,10.7960242518575));
#72379=CARTESIAN_POINT('Ctrl Pts',(88.0080336641173,53.9133774200005,10.7959722788624));
#72380=CARTESIAN_POINT('Ctrl Pts',(88.0285381315914,53.9113384330585,10.7960680802873));
#72381=CARTESIAN_POINT('Ctrl Pts',(88.0401408087626,53.9101795529397,10.7962813472911));
#72382=CARTESIAN_POINT('Ctrl Pts',(88.0783240644833,53.9063476655699,10.7975068019968));
#72383=CARTESIAN_POINT('Ctrl Pts',(88.1048736211317,53.9036541536336,10.7991949652328));
#72384=CARTESIAN_POINT('Ctrl Pts',(88.2247184448708,53.891349956566,10.8106030784746));
#72385=CARTESIAN_POINT('Ctrl Pts',(88.3167996224409,53.8814639459333,10.8298056266883));
#72386=CARTESIAN_POINT('Ctrl Pts',(88.4546734630524,53.8661827805205,10.8749136740534));
#72387=CARTESIAN_POINT('Ctrl Pts',(88.5024354813102,53.8608008338611,10.8938117165615));
#72388=CARTESIAN_POINT('Ctrl Pts',(88.5602894635928,53.8542529043565,10.9208631636009));
#72389=CARTESIAN_POINT('Ctrl Pts',(88.5715718353867,53.8529746664114,10.9263436706061));
#72390=CARTESIAN_POINT('Ctrl Pts',(88.5882726868535,53.8510823733531,10.9347643057762));
#72391=CARTESIAN_POINT('Ctrl Pts',(88.5937534190231,53.8504613516962,10.9375779117248));
#72392=CARTESIAN_POINT('Ctrl Pts',(88.6036103921725,53.8493446754645,10.9427290915909));
#72393=CARTESIAN_POINT('Ctrl Pts',(88.6079935926367,53.848848216146,10.9450525150588));
#72394=CARTESIAN_POINT('Ctrl Pts',(88.6178998857648,53.8477263606179,10.9503781818722));
#72395=CARTESIAN_POINT('Ctrl Pts',(88.6234144524948,53.8471019381096,10.9533958219668));
#72396=CARTESIAN_POINT('Ctrl Pts',(88.6404393225424,53.845173682006,10.9628769821767));
#72397=CARTESIAN_POINT('Ctrl Pts',(88.6518720409121,53.8438780778468,10.9694794435844));
#72398=CARTESIAN_POINT('Ctrl Pts',(88.7350119539368,53.8344341155836,11.0192379815106));
#72399=CARTESIAN_POINT('Ctrl Pts',(88.8024136019785,53.8266470684094,11.069218188806));
#72400=CARTESIAN_POINT('Ctrl Pts',(88.9029230042319,53.8139301878386,11.1604189644734));
#72401=CARTESIAN_POINT('Ctrl Pts',(88.9392446499283,53.8090502815021,11.1976885705281));
#72402=CARTESIAN_POINT('Ctrl Pts',(88.9876594990274,53.8019745890153,11.2538863906094));
#72403=CARTESIAN_POINT('Ctrl Pts',(89.0016973148835,53.7998453505486,11.271071702612));
#72404=CARTESIAN_POINT('Ctrl Pts',(89.0261832243833,53.795976350256,11.3027042000749));
#72405=CARTESIAN_POINT('Ctrl Pts',(89.0367910905204,53.7942429093751,11.3170206805782));
#72406=CARTESIAN_POINT('Ctrl Pts',(89.0529308143438,53.7915093328552,11.3397892473091));
#72407=CARTESIAN_POINT('Ctrl Pts',(89.0586693440849,53.7905171205344,11.3480927566082));
#72408=CARTESIAN_POINT('Ctrl Pts',(89.0692303822464,53.7886517353787,11.3637706347628));
#72409=CARTESIAN_POINT('Ctrl Pts',(89.0740763391676,53.7877795091298,11.3711285655024));
#72410=CARTESIAN_POINT('Ctrl Pts',(89.0848065919618,53.7858104450746,11.3877959842441));
#72411=CARTESIAN_POINT('Ctrl Pts',(89.0906470392867,53.7847120662646,11.3971326477929));
#72412=CARTESIAN_POINT('Ctrl Pts',(89.1054272420102,53.7818612807239,11.4214586212093));
#72413=CARTESIAN_POINT('Ctrl Pts',(89.1141803847152,53.7801023363195,11.4365577561931));
#72414=CARTESIAN_POINT('Ctrl Pts',(89.1563168367608,53.7712647232938,11.512822959893));
#72415=CARTESIAN_POINT('Ctrl Pts',(89.1849305820884,53.7640269853221,11.5764710535249));
#72416=CARTESIAN_POINT('Ctrl Pts',(89.2295070319227,53.7499860653472,11.7023728720982));
#72417=CARTESIAN_POINT('Ctrl Pts',(89.2462591447343,53.7432172414619,11.7641401883981));
#72418=CARTESIAN_POINT('Ctrl Pts',(89.2611180185048,53.7349866104183,11.8416555402151));
#72419=CARTESIAN_POINT('Ctrl Pts',(89.2636834239061,53.7334273071814,11.8564533809709));
#72420=CARTESIAN_POINT('Ctrl Pts',(89.2687136535559,53.7300408118499,11.8888759465607));
#72421=CARTESIAN_POINT('Ctrl Pts',(89.2710718879255,53.7282176590526,11.9065148451159));
#72422=CARTESIAN_POINT('Ctrl Pts',(89.2738471033515,53.7256960756864,11.9312148486454));
#72423=CARTESIAN_POINT('Ctrl Pts',(89.2745768999791,53.7249826829541,11.9382374474331));
#72424=CARTESIAN_POINT('Ctrl Pts',(89.2757268741141,53.7237658386703,11.9502792369806));
#72425=CARTESIAN_POINT('Ctrl Pts',(89.2761758197216,53.7232608628,11.9552953882759));
#72426=CARTESIAN_POINT('Ctrl Pts',(89.277064663548,53.7221935019962,11.9659393734273));
#72427=CARTESIAN_POINT('Ctrl Pts',(89.2774968993691,53.7216315402728,11.9715676446691));
#72428=CARTESIAN_POINT('Ctrl Pts',(89.2785916406405,53.7200783628997,11.9871858877048));
#72429=CARTESIAN_POINT('Ctrl Pts',(89.2791735938267,53.7190914183823,11.9971814655512));
#72430=CARTESIAN_POINT('Ctrl Pts',(89.282522263607,53.7120035476859,12.0694102439732));
#72431=CARTESIAN_POINT('Ctrl Pts',(89.2808255258396,53.7061165425557,12.13177786816));
#72432=CARTESIAN_POINT('Ctrl Pts',(89.2696773275139,53.6957116902284,12.2420169720675));
#72433=CARTESIAN_POINT('Ctrl Pts',(89.2620411319101,53.6911891213685,12.289934433655));
#72434=CARTESIAN_POINT('Ctrl Pts',(89.2434919432652,53.6830167976973,12.3747625981709));
#72435=CARTESIAN_POINT('Ctrl Pts',(89.2336075385662,53.6793869309998,12.4118338791707));
#72436=CARTESIAN_POINT('Ctrl Pts',(89.2140325740849,53.6731554580471,12.473828108739));
#72437=CARTESIAN_POINT('Ctrl Pts',(89.2052047983294,53.670579173345,12.4989963113444));
#72438=CARTESIAN_POINT('Ctrl Pts',(89.1913588844973,53.6668314079365,12.5348184944832));
#72439=CARTESIAN_POINT('Ctrl Pts',(89.1869740556626,53.6656808009468,12.5457112411131));
#72440=CARTESIAN_POINT('Ctrl Pts',(89.1790046389428,53.6636499659003,12.564742641155));
#72441=CARTESIAN_POINT('Ctrl Pts',(89.17548435024,53.6627719534045,12.5729075326067));
#72442=CARTESIAN_POINT('Ctrl Pts',(89.1679514675653,53.6609314763122,12.5898865170836));
#72443=CARTESIAN_POINT('Ctrl Pts',(89.1639232254399,53.6599685267739,12.5986929734983));
#72444=CARTESIAN_POINT('Ctrl Pts',(89.153032704143,53.6574191011774,12.6217993058069));
#72445=CARTESIAN_POINT('Ctrl Pts',(89.1460028308883,53.6558269555751,12.6360176146151));
#72446=CARTESIAN_POINT('Ctrl Pts',(89.1051197283574,53.6468510496238,12.7149497508105));
#72447=CARTESIAN_POINT('Ctrl Pts',(89.0660073902115,53.6392853545012,12.7767661248979));
#72448=CARTESIAN_POINT('Ctrl Pts',(88.9880434050264,53.6257575059081,12.8792634541353));
#72449=CARTESIAN_POINT('Ctrl Pts',(88.9513868087343,53.6198554004453,12.9213852368911));
#72450=CARTESIAN_POINT('Ctrl Pts',(88.8932991622785,53.6112137878877,12.9798700489183));
#72451=CARTESIAN_POINT('Ctrl Pts',(88.873926140145,53.6084348393591,12.9981850649468));
#72452=CARTESIAN_POINT('Ctrl Pts',(88.8409965628351,53.6038927425522,13.0274091130975));
#72453=CARTESIAN_POINT('Ctrl Pts',(88.8277672466565,53.6021133600738,13.0386731966241));
#72454=CARTESIAN_POINT('Ctrl Pts',(88.8088912648143,53.5996413918402,13.0540882914258));
#72455=CARTESIAN_POINT('Ctrl Pts',(88.8034359992838,53.5989345843782,13.0584687085611));
#72456=CARTESIAN_POINT('Ctrl Pts',(88.7939994124706,53.5977252914003,13.0659185892293));
#72457=CARTESIAN_POINT('Ctrl Pts',(88.7900356548054,53.5972213320852,13.0690098295977));
#72458=CARTESIAN_POINT('Ctrl Pts',(88.7815572245223,53.5961519352171,13.0755413695585));
#72459=CARTESIAN_POINT('Ctrl Pts',(88.7770377095485,53.5955869501071,13.0789750467331));
#72460=CARTESIAN_POINT('Ctrl Pts',(88.7645785600711,53.5940427624159,13.0883097411461));
#72461=CARTESIAN_POINT('Ctrl Pts',(88.7565924790065,53.5930676556945,13.0941486908534));
#72462=CARTESIAN_POINT('Ctrl Pts',(88.6979295637554,53.5860039232337,13.1359964606998));
#72463=CARTESIAN_POINT('Ctrl Pts',(88.6447275843761,53.5801284639822,13.1683416361379));
#72464=CARTESIAN_POINT('Ctrl Pts',(88.5464070672245,53.5697574741116,13.2186347797761));
#72465=CARTESIAN_POINT('Ctrl Pts',(88.5022377493295,53.5652569076127,13.2381403916589));
#72466=CARTESIAN_POINT('Ctrl Pts',(88.4209541155103,53.5570872098767,13.2686326186366));
#72467=CARTESIAN_POINT('Ctrl Pts',(88.384246949572,53.5534371585868,13.280526176888));
#72468=CARTESIAN_POINT('Ctrl Pts',(88.3212393590593,53.5471750903146,13.2978150639335));
#72469=CARTESIAN_POINT('Ctrl Pts',(88.2952050747479,53.5445887437386,13.3040807929702));
#72470=CARTESIAN_POINT('Ctrl Pts',(88.2574800375832,53.5408290533537,13.3119076518311));
#72471=CARTESIAN_POINT('Ctrl Pts',(88.2459336004037,53.5396767739187,13.3141363974276));
#72472=CARTESIAN_POINT('Ctrl Pts',(88.2256030552416,53.5376440318289,13.317768601019));
#72473=CARTESIAN_POINT('Ctrl Pts',(88.2168318620694,53.5367657981367,13.3192407335524));
#72474=CARTESIAN_POINT('Ctrl Pts',(88.1984871034593,53.5349258882757,13.3221218955505));
#72475=CARTESIAN_POINT('Ctrl Pts',(88.1889114993275,53.5339637342582,13.323513862975));
#72476=CARTESIAN_POINT('Ctrl Pts',(88.1636369979451,53.5314188393498,13.3268934694608));
#72477=CARTESIAN_POINT('Ctrl Pts',(88.1479158546044,53.5298304656738,13.3286972658015));
#72478=CARTESIAN_POINT('Ctrl Pts',(88.0619889765172,53.5211146086696,13.3369327989064));
#72479=CARTESIAN_POINT('Ctrl Pts',(87.9913901625712,53.5138185211745,13.3378023642957));
#72480=CARTESIAN_POINT('Ctrl Pts',(87.8626381848231,53.5002697111586,13.3286652738885));
#72481=CARTESIAN_POINT('Ctrl Pts',(87.8045361113477,53.4940661992991,13.3204749509714));
#72482=CARTESIAN_POINT('Ctrl Pts',(87.7212732943293,53.4851434214448,13.3027947902325));
#72483=CARTESIAN_POINT('Ctrl Pts',(87.6955154855073,53.4823791994417,13.296476605255));
#72484=CARTESIAN_POINT('Ctrl Pts',(87.6532995552846,53.4778582397883,13.2847083222531));
#72485=CARTESIAN_POINT('Ctrl Pts',(87.6367220638024,53.4760854407113,13.2797197839208));
#72486=CARTESIAN_POINT('Ctrl Pts',(87.6136031291482,53.4736209479673,13.2722439772814));
#72487=CARTESIAN_POINT('Ctrl Pts',(87.6069734770703,53.4729151425032,13.2700396101214));
#72488=CARTESIAN_POINT('Ctrl Pts',(87.5956069833166,53.4717069948256,13.2661557784235));
#72489=CARTESIAN_POINT('Ctrl Pts',(87.5908614189479,53.4712031865013,13.264502744347));
#72490=CARTESIAN_POINT('Ctrl Pts',(87.580772298154,53.4701334626688,13.2609210823057));
#72491=CARTESIAN_POINT('Ctrl Pts',(87.5754317070703,53.4695680041429,13.2589847170942));
#72492=CARTESIAN_POINT('Ctrl Pts',(87.5608068928572,53.4680212129953,13.2535708187436));
#72493=CARTESIAN_POINT('Ctrl Pts',(87.5515497785602,53.4670439988229,13.2500201854786));
#72494=CARTESIAN_POINT('Ctrl Pts',(87.4839673931964,53.4599163535982,13.2231864349197));
#72495=CARTESIAN_POINT('Ctrl Pts',(87.4273873336932,53.4539834716108,13.1957093548275));
#72496=CARTESIAN_POINT('Ctrl Pts',(87.3296137954752,53.4433666361083,13.1389109049242));
#72497=CARTESIAN_POINT('Ctrl Pts',(87.2877010223443,53.4386802496924,13.1111140975397));
#72498=CARTESIAN_POINT('Ctrl Pts',(87.2246387717377,53.431247716195,13.0636761329904));
#72499=CARTESIAN_POINT('Ctrl Pts',(87.202325301845,53.4285357509339,13.0456766814791));
#72500=CARTESIAN_POINT('Ctrl Pts',(87.1806428308131,53.4258009314892,13.0269406701664));
#72501=CARTESIAN_POINT('Origin',(88.011,66.41344859951,12.066));
#72502=CARTESIAN_POINT('',(87.1806428354249,52.4628656574377,13.0269406741515));
#72503=CARTESIAN_POINT('',(87.1806428293121,52.6319631729084,13.0269406688694));
#72504=CARTESIAN_POINT('',(87.1806428354228,66.41344859951,13.0269406741497));
#72505=CARTESIAN_POINT('Ctrl Pts',(87.1806428354249,52.4628656574377,13.0269406741515));
#72506=CARTESIAN_POINT('Ctrl Pts',(87.1823742791358,52.4630959657415,13.0284368296678));
#72507=CARTESIAN_POINT('Ctrl Pts',(87.1841097925396,52.463325945256,13.0299283280082));
#72508=CARTESIAN_POINT('Ctrl Pts',(87.1894085350898,52.464025434346,13.0344572198663));
#72509=CARTESIAN_POINT('Ctrl Pts',(87.1929844642713,52.4644938131071,13.0374795455676));
#72510=CARTESIAN_POINT('Ctrl Pts',(87.201458071945,52.4655951445308,13.0445613565417));
#72511=CARTESIAN_POINT('Ctrl Pts',(87.2063696616142,52.4662268852427,13.0486039317712));
#72512=CARTESIAN_POINT('Ctrl Pts',(87.2218771673402,52.468201630086,13.0611734145365));
#72513=CARTESIAN_POINT('Ctrl Pts',(87.2325803858327,52.4695358283367,13.0695676005866));
#72514=CARTESIAN_POINT('Ctrl Pts',(87.3096735956759,52.4789615863688,13.1280535433542));
#72515=CARTESIAN_POINT('Ctrl Pts',(87.3807201693157,52.4867000534846,13.1716984530809));
#72516=CARTESIAN_POINT('Ctrl Pts',(87.5022452525584,52.4993623578523,13.2308030983649));
#72517=CARTESIAN_POINT('Ctrl Pts',(87.5502984157015,52.5042369908387,13.2506311297707));
#72518=CARTESIAN_POINT('Ctrl Pts',(87.6204046098024,52.5113059949499,13.2746467373196));
#72519=CARTESIAN_POINT('Ctrl Pts',(87.6415653099816,52.5134339706799,13.2812816877559));
#72520=CARTESIAN_POINT('Ctrl Pts',(87.6800151641187,52.5173009710025,13.2922406880998));
#72521=CARTESIAN_POINT('Ctrl Pts',(87.6972425256221,52.519033685865,13.2967612925169));
#72522=CARTESIAN_POINT('Ctrl Pts',(87.724372709713,52.5217665067826,13.3032738866751));
#72523=CARTESIAN_POINT('Ctrl Pts',(87.7342145487322,52.5227586991067,13.3055126758526));
#72524=CARTESIAN_POINT('Ctrl Pts',(87.7526973989221,52.524624279486,13.3094859980572));
#72525=CARTESIAN_POINT('Ctrl Pts',(87.7613318818579,52.525496722493,13.3112483615455));
#72526=CARTESIAN_POINT('Ctrl Pts',(87.7808022491705,52.5274665932623,13.3150117727668));
#72527=CARTESIAN_POINT('Ctrl Pts',(87.7916470715518,52.5285655653177,13.3169619043391));
#72528=CARTESIAN_POINT('Ctrl Pts',(87.8197466933412,52.5314185771291,13.3216382087006));
#72529=CARTESIAN_POINT('Ctrl Pts',(87.8370341115358,52.533179169902,13.3241498044262));
#72530=CARTESIAN_POINT('Ctrl Pts',(87.9233754684778,52.542004222068,13.3348804914783));
#72531=CARTESIAN_POINT('Ctrl Pts',(87.9929571080323,52.5492270024747,13.3377729134239));
#72532=CARTESIAN_POINT('Ctrl Pts',(88.1263516045711,52.5632616172065,13.3323684303559));
#72533=CARTESIAN_POINT('Ctrl Pts',(88.1900050836201,52.5700396018162,13.3249490044845));
#72534=CARTESIAN_POINT('Ctrl Pts',(88.2675827476387,52.5782804582478,13.3099015786419));
#72535=CARTESIAN_POINT('Ctrl Pts',(88.2822847477183,52.5798409831681,13.3067781746664));
#72536=CARTESIAN_POINT('Ctrl Pts',(88.3142741597248,52.5832297777446,13.2993862803844));
#72537=CARTESIAN_POINT('Ctrl Pts',(88.3315350822376,52.5850540078219,13.2950135501902));
#72538=CARTESIAN_POINT('Ctrl Pts',(88.3555080030124,52.587576899724,13.2884009627456));
#72539=CARTESIAN_POINT('Ctrl Pts',(88.3623006858114,52.5882905412783,13.2864661873842));
#72540=CARTESIAN_POINT('Ctrl Pts',(88.3739099895328,52.5895077554112,13.2830545233475));
#72541=CARTESIAN_POINT('Ctrl Pts',(88.3787344945672,52.5900128536705,13.2816054950424));
#72542=CARTESIAN_POINT('Ctrl Pts',(88.3889476423061,52.5910804261593,13.278471628976));
#72543=CARTESIAN_POINT('Ctrl Pts',(88.3943338421549,52.5916424773191,13.2767795180905));
#72544=CARTESIAN_POINT('Ctrl Pts',(88.409240642247,52.5931958221268,13.2719869976482));
#72545=CARTESIAN_POINT('Ctrl Pts',(88.4187364879145,52.5941828442802,13.268809721904));
#72546=CARTESIAN_POINT('Ctrl Pts',(88.4870166062117,52.6012693017236,13.2450618313528));
#72547=CARTESIAN_POINT('Ctrl Pts',(88.5442665422542,52.6071549270674,13.2203000051829));
#72548=CARTESIAN_POINT('Ctrl Pts',(88.6424211426496,52.6175562367526,13.1689758392418));
#72549=CARTESIAN_POINT('Ctrl Pts',(88.6840438071263,52.6220766717097,13.1440817922037));
#72550=CARTESIAN_POINT('Ctrl Pts',(88.7558918978885,52.630248660336,13.09532422512));
#72551=CARTESIAN_POINT('Ctrl Pts',(88.7866463255951,52.633880404465,13.0723521302925));
#72552=CARTESIAN_POINT('Ctrl Pts',(88.8369403570209,52.640114813673,13.0311084119627));
#72553=CARTESIAN_POINT('Ctrl Pts',(88.857029163468,52.6426921267512,13.0135474341148));
#72554=CARTESIAN_POINT('Ctrl Pts',(88.8851436743173,52.6464412526736,12.9873635491724));
#72555=CARTESIAN_POINT('Ctrl Pts',(88.8936269322807,52.647592173582,12.9792401814132));
#72556=CARTESIAN_POINT('Ctrl Pts',(88.9083334550585,52.6496235194173,12.9647612388746));
#72557=CARTESIAN_POINT('Ctrl Pts',(88.9146050211638,52.6505017272515,12.958455628959));
#72558=CARTESIAN_POINT('Ctrl Pts',(88.9275675017931,52.6523425762586,12.9451460800595));
#72559=CARTESIAN_POINT('Ctrl Pts',(88.9342455087131,52.6533057023011,12.9381304562682));
#72560=CARTESIAN_POINT('Ctrl Pts',(88.9516471836922,52.6558555212838,12.9194251634223));
#72561=CARTESIAN_POINT('Ctrl Pts',(88.9622327786363,52.657447884948,12.9076102280764));
#72562=CARTESIAN_POINT('Ctrl Pts',(89.0202758209102,52.6664201791749,12.8403322986654));
#72563=CARTESIAN_POINT('Ctrl Pts',(89.0630929910157,52.6739818345908,12.7810691260865));
#72564=CARTESIAN_POINT('Ctrl Pts',(89.1346129647296,52.6886052203436,12.6616362905329));
#72565=CARTESIAN_POINT('Ctrl Pts',(89.1641489655427,52.6956251131005,12.6022242664629));
#72566=CARTESIAN_POINT('Ctrl Pts',(89.1946418421869,52.7041340548743,12.5265720308245));
#72567=CARTESIAN_POINT('Ctrl Pts',(89.2001107648329,52.7057250924005,12.5122625312404));
#72568=CARTESIAN_POINT('Ctrl Pts',(89.2114541684645,52.7091690983356,12.4808918312051));
#72569=CARTESIAN_POINT('Ctrl Pts',(89.2172269717008,52.7110180491254,12.4637964956962));
#72570=CARTESIAN_POINT('Ctrl Pts',(89.2247611033712,52.7135688958206,12.4398106023941));
#72571=CARTESIAN_POINT('Ctrl Pts',(89.2268314715854,52.7142861973132,12.4330207403978));
#72572=CARTESIAN_POINT('Ctrl Pts',(89.2302751574187,52.7155076259154,12.4213779947144));
#72573=CARTESIAN_POINT('Ctrl Pts',(89.2316766654725,52.716013306784,12.4165337527103));
#72574=CARTESIAN_POINT('Ctrl Pts',(89.2345814793649,52.7170798301912,12.4062646726259));
#72575=CARTESIAN_POINT('Ctrl Pts',(89.2360776264963,52.7176402654713,12.4008380170699));
#72576=CARTESIAN_POINT('Ctrl Pts',(89.2401144566424,52.7191843691226,12.3858067380316));
#72577=CARTESIAN_POINT('Ctrl Pts',(89.2425786941156,52.7201638482998,12.3761816241583));
#72578=CARTESIAN_POINT('Ctrl Pts',(89.2582601139588,52.7266608149601,12.3117957102351));
#72579=CARTESIAN_POINT('Ctrl Pts',(89.2679366369789,52.7320043117928,12.2562262810163));
#72580=CARTESIAN_POINT('Ctrl Pts',(89.2818195819148,52.7443650466693,12.1255689132522));
#72581=CARTESIAN_POINT('Ctrl Pts',(89.2831190812652,52.751330386456,12.0503969934082));
#72582=CARTESIAN_POINT('Ctrl Pts',(89.2758512804784,52.7610151567976,11.9486079547546));
#72583=CARTESIAN_POINT('Ctrl Pts',(89.2730685294822,52.7635951417093,11.9217347057547));
#72584=CARTESIAN_POINT('Ctrl Pts',(89.2666460818684,52.7681929154307,11.8744779410276));
#72585=CARTESIAN_POINT('Ctrl Pts',(89.2633607333884,52.770200084597,11.8540559961083));
#72586=CARTESIAN_POINT('Ctrl Pts',(89.2576268216648,52.7732663856689,11.8232337839553));
#72587=CARTESIAN_POINT('Ctrl Pts',(89.2555431097102,52.7743140319397,11.8127682896456));
#72588=CARTESIAN_POINT('Ctrl Pts',(89.251680037624,52.7761482684735,11.794566695118));
#72589=CARTESIAN_POINT('Ctrl Pts',(89.2499595264022,52.776932945165,11.7868185545899));
#72590=CARTESIAN_POINT('Ctrl Pts',(89.2458985632029,52.7787154791357,11.7693076974282));
#72591=CARTESIAN_POINT('Ctrl Pts',(89.2435147782696,52.7797146755448,11.7595557305063));
#72592=CARTESIAN_POINT('Ctrl Pts',(89.2367605029523,52.7824253855073,11.7332788724281));
#72593=CARTESIAN_POINT('Ctrl Pts',(89.2321717875719,52.7841437730606,11.7168130136821));
#72594=CARTESIAN_POINT('Ctrl Pts',(89.1971120622441,52.7964665985134,11.6001641702151));
#72595=CARTESIAN_POINT('Ctrl Pts',(89.1546922661271,52.807465525127,11.5040202504589));
#72596=CARTESIAN_POINT('Ctrl Pts',(89.0800702195963,52.8227892616701,11.3792332701759));
#72597=CARTESIAN_POINT('Ctrl Pts',(89.0574896753962,52.8270726976908,11.3452923142248));
#72598=CARTESIAN_POINT('Ctrl Pts',(89.0196466282889,52.8336899689284,11.2939490414931));
#72599=CARTESIAN_POINT('Ctrl Pts',(89.0054749532874,52.8360607374529,11.2757781974143));
#72600=CARTESIAN_POINT('Ctrl Pts',(88.9858750436903,52.8391916859008,11.2520104772819));
#72601=CARTESIAN_POINT('Ctrl Pts',(88.9808797849678,52.839977491618,11.2460649368586));
#72602=CARTESIAN_POINT('Ctrl Pts',(88.972472747039,52.8412795081493,11.2362429189353));
#72603=CARTESIAN_POINT('Ctrl Pts',(88.9690913900066,52.8417978012411,11.2323408670968));
#72604=CARTESIAN_POINT('Ctrl Pts',(88.9625714739324,52.8427867725853,11.2249090201569));
#72605=CARTESIAN_POINT('Ctrl Pts',(88.9594368952985,52.8432577411085,11.2213759624957));
#72606=CARTESIAN_POINT('Ctrl Pts',(88.9508418827735,52.8445372385156,11.2117965072618));
#72607=CARTESIAN_POINT('Ctrl Pts',(88.9453426962689,52.8453429660223,11.2057848464429));
#72608=CARTESIAN_POINT('Ctrl Pts',(88.9232910610307,52.8485253607497,11.1821391926004));
#72609=CARTESIAN_POINT('Ctrl Pts',(88.9062925921666,52.8508718261795,11.1649248931283));
#72610=CARTESIAN_POINT('Ctrl Pts',(88.8355028162124,52.860281101975,11.0972191223858));
#72611=CARTESIAN_POINT('Ctrl Pts',(88.7778475790417,52.8671409590051,11.0509686130264));
#72612=CARTESIAN_POINT('Ctrl Pts',(88.6593817268734,52.8804987430598,10.9718249073616));
#72613=CARTESIAN_POINT('Ctrl Pts',(88.5992748881181,52.8869671663661,10.9383705084544));
#72614=CARTESIAN_POINT('Ctrl Pts',(88.5205318119235,52.8953336506621,10.9025588223497));
#72615=CARTESIAN_POINT('Ctrl Pts',(88.5041453972314,52.8970686588304,10.8955190803493));
#72616=CARTESIAN_POINT('Ctrl Pts',(88.4782570129851,52.8998042760683,10.8850373172108));
#72617=CARTESIAN_POINT('Ctrl Pts',(88.4688523560557,52.9007969440513,10.8813594723269));
#72618=CARTESIAN_POINT('Ctrl Pts',(88.451160703031,52.9026629411226,10.8746829947548));
#72619=CARTESIAN_POINT('Ctrl Pts',(88.4428843429044,52.903535321127,10.8716576889786));
#72620=CARTESIAN_POINT('Ctrl Pts',(88.4241962894727,52.9055044119707,10.86504617782));
#72621=CARTESIAN_POINT('Ctrl Pts',(88.4137682499115,52.9066026617624,10.8615088319652));
#72622=CARTESIAN_POINT('Ctrl Pts',(88.3867053417737,52.9094524596944,10.8527194151114));
#72623=CARTESIAN_POINT('Ctrl Pts',(88.3700065812749,52.9112105359099,10.8476739029728));
#72624=CARTESIAN_POINT('Ctrl Pts',(88.2800974423266,52.9206800557911,10.8225167652175));
#72625=CARTESIAN_POINT('Ctrl Pts',(88.2053140600595,52.9285834933689,10.808661086677));
#72626=CARTESIAN_POINT('Ctrl Pts',(88.0579048758485,52.9441695733533,10.7948161707603));
#72627=CARTESIAN_POINT('Ctrl Pts',(87.9856023694152,52.9518147146446,10.7942040359902));
#72628=CARTESIAN_POINT('Ctrl Pts',(87.8954880800442,52.9611473823246,10.8011331170657));
#72629=CARTESIAN_POINT('Ctrl Pts',(87.8773721915217,52.9630129813771,10.802918465057));
#72630=CARTESIAN_POINT('Ctrl Pts',(87.8522285098102,52.965582628126,10.805943519324));
#72631=CARTESIAN_POINT('Ctrl Pts',(87.845164635058,52.9663023712236,10.8068537173674));
#72632=CARTESIAN_POINT('Ctrl Pts',(87.8331090616176,52.9675266179231,10.8085103259716));
#72633=CARTESIAN_POINT('Ctrl Pts',(87.8281135894133,52.9680326940156,10.8092271359246));
#72634=CARTESIAN_POINT('Ctrl Pts',(87.8175660245862,52.9690985484034,10.8108048520815));
#72635=CARTESIAN_POINT('Ctrl Pts',(87.8120151923191,52.9696579298235,10.8116728444997));
#72636=CARTESIAN_POINT('Ctrl Pts',(87.7967150855748,52.9711960145643,10.8141694724645));
#72637=CARTESIAN_POINT('Ctrl Pts',(87.7869784265711,52.9721705819194,10.8158751857984));
#72638=CARTESIAN_POINT('Ctrl Pts',(87.7262729961519,52.9782262386956,10.82724192125));
#72639=CARTESIAN_POINT('Ctrl Pts',(87.6759070930623,52.9831606259344,10.8399062997474));
#72640=CARTESIAN_POINT('Ctrl Pts',(87.553773073519,52.9952364751671,10.8787096118044));
#72641=CARTESIAN_POINT('Ctrl Pts',(87.4833261242387,53.0023077546989,10.908297493803));
#72642=CARTESIAN_POINT('Ctrl Pts',(87.3780644970398,53.0135974124284,10.9641231634466));
#72643=CARTESIAN_POINT('Ctrl Pts',(87.3412172364548,53.0177006555736,10.9861249541763));
#72644=CARTESIAN_POINT('Ctrl Pts',(87.2940382427846,53.0232175586522,11.0176404554194));
#72645=CARTESIAN_POINT('Ctrl Pts',(87.2826464542447,53.0245709832951,11.0255227191019));
#72646=CARTESIAN_POINT('Ctrl Pts',(87.2638516843255,53.0268417395692,11.0389871944164));
#72647=CARTESIAN_POINT('Ctrl Pts',(87.2563765442531,53.0277551314488,11.0444671629876));
#72648=CARTESIAN_POINT('Ctrl Pts',(87.241761787677,53.0295618480941,11.0554290778574));
#72649=CARTESIAN_POINT('Ctrl Pts',(87.2346191387781,53.0304549392476,11.0609060921191));
#72650=CARTESIAN_POINT('Ctrl Pts',(87.2173516827805,53.0326393539961,11.0744407342887));
#72651=CARTESIAN_POINT('Ctrl Pts',(87.2072909123284,53.0339337721917,11.0825778630921));
#72652=CARTESIAN_POINT('Ctrl Pts',(87.1723812219749,53.0385042600995,11.1117062314311));
#72653=CARTESIAN_POINT('Ctrl Pts',(87.1482186488439,53.0418120395344,11.1334948218912));
#72654=CARTESIAN_POINT('Ctrl Pts',(87.0623102930519,53.0541387940927,11.2171618134637));
#72655=CARTESIAN_POINT('Ctrl Pts',(87.0061700679373,53.0633659433336,11.2844309088616));
#72656=CARTESIAN_POINT('Ctrl Pts',(86.9299582166029,53.0777384268249,11.3976720114085));
#72657=CARTESIAN_POINT('Ctrl Pts',(86.9049121616993,53.0828859921942,11.4399930945454));
#72658=CARTESIAN_POINT('Ctrl Pts',(86.8767379270176,53.0891833996016,11.4945974306205));
#72659=CARTESIAN_POINT('Ctrl Pts',(86.8712557038719,53.0904369016935,11.505612342601));
#72660=CARTESIAN_POINT('Ctrl Pts',(86.8632893563129,53.092300061176,11.522219099191));
#72661=CARTESIAN_POINT('Ctrl Pts',(86.8606844009173,53.0929163857274,11.5277515277105));
#72662=CARTESIAN_POINT('Ctrl Pts',(86.8562454710126,53.0939788184756,11.5373584034222));
#72663=CARTESIAN_POINT('Ctrl Pts',(86.8543929468679,53.094426011435,11.5414238978997));
#72664=CARTESIAN_POINT('Ctrl Pts',(86.850070254946,53.095478607935,11.5510445799515));
#72665=CARTESIAN_POINT('Ctrl Pts',(86.8476184599334,53.0960828972349,11.5566078569078));
#72666=CARTESIAN_POINT('Ctrl Pts',(86.8403979450442,53.097885302517,11.5733157574695));
#72667=CARTESIAN_POINT('Ctrl Pts',(86.8357485000002,53.0990766566255,11.5845118016098));
#72668=CARTESIAN_POINT('Ctrl Pts',(86.8017584495209,53.1080404802805,11.6697886326248));
#72669=CARTESIAN_POINT('Ctrl Pts',(86.7792818949578,53.1154771514103,11.746431270888));
#72670=CARTESIAN_POINT('Ctrl Pts',(86.7487691137389,53.1305199686773,11.9040920530442));
#72671=CARTESIAN_POINT('Ctrl Pts',(86.7410239596817,53.1380967716393,11.9847682564807));
#72672=CARTESIAN_POINT('Ctrl Pts',(86.7409950052116,53.1475755416504,12.0827072230892));
#72673=CARTESIAN_POINT('Ctrl Pts',(86.7413346216635,53.149238241815,12.0997872587707));
#72674=CARTESIAN_POINT('Ctrl Pts',(86.7424204882589,53.1518947598353,12.1268831867411));
#72675=CARTESIAN_POINT('Ctrl Pts',(86.742941254752,53.1528815493602,12.1369065886768));
#72676=CARTESIAN_POINT('Ctrl Pts',(86.7440864916012,53.1546553940199,12.1548434636506));
#72677=CARTESIAN_POINT('Ctrl Pts',(86.7446664669981,53.1554410169951,12.1627593650907));
#72678=CARTESIAN_POINT('Ctrl Pts',(86.7462002829072,53.1572886816428,12.1813065724569));
#72679=CARTESIAN_POINT('Ctrl Pts',(86.7472140159564,53.1583525422592,12.1919321193083));
#72680=CARTESIAN_POINT('Ctrl Pts',(86.7505868315951,53.1614919958295,12.2231211225857));
#72681=CARTESIAN_POINT('Ctrl Pts',(86.7533146938287,53.1635788800465,12.2436399273561));
#72682=CARTESIAN_POINT('Ctrl Pts',(86.7607596324566,53.1684278405857,12.2907890205622));
#72683=CARTESIAN_POINT('Ctrl Pts',(86.7658282467243,53.1711996524057,12.3173525847148));
#72684=CARTESIAN_POINT('Ctrl Pts',(86.7881848887099,53.1817656008263,12.4171095530073));
#72685=CARTESIAN_POINT('Ctrl Pts',(86.811112449967,53.1897012770843,12.4888731918023));
#72686=CARTESIAN_POINT('Ctrl Pts',(86.8620017324087,53.2035347978097,12.6099246723796));
#72687=CARTESIAN_POINT('Ctrl Pts',(86.8871665725444,53.2094217686278,12.6601813295732));
#72688=CARTESIAN_POINT('Ctrl Pts',(86.9206056157081,53.2161683758425,12.7171825919518));
#72689=CARTESIAN_POINT('Ctrl Pts',(86.9257327438217,53.2171773812698,12.7256921148064));
#72690=CARTESIAN_POINT('Ctrl Pts',(86.9339207137207,53.2187487340921,12.738927851421));
#72691=CARTESIAN_POINT('Ctrl Pts',(86.9369138375728,53.219315100488,12.7436950659087));
#72692=CARTESIAN_POINT('Ctrl Pts',(86.9426485136075,53.2203849262764,12.7526953710659));
#72693=CARTESIAN_POINT('Ctrl Pts',(86.9453836131954,53.2208887305173,12.7569320872768));
#72694=CARTESIAN_POINT('Ctrl Pts',(86.9520294677,53.2220977728255,12.7670932887489));
#72695=CARTESIAN_POINT('Ctrl Pts',(86.9559648042419,53.2228013928399,12.7730015079374));
#72696=CARTESIAN_POINT('Ctrl Pts',(86.9700772545258,53.2252828311546,12.7938086074734));
#72697=CARTESIAN_POINT('Ctrl Pts',(86.9805228532394,53.2270442206058,12.80852441132));
#72698=CARTESIAN_POINT('Ctrl Pts',(87.0004112541684,53.2302736778544,12.8353146849463));
#72699=CARTESIAN_POINT('Ctrl Pts',(87.0097653911286,53.2317455734891,12.847449941906));
#72700=CARTESIAN_POINT('Ctrl Pts',(87.0607361913128,53.2395402786966,12.9111567310743));
#72701=CARTESIAN_POINT('Ctrl Pts',(87.1061251458202,53.2457107582171,12.9595851144826));
#72702=CARTESIAN_POINT('Ctrl Pts',(87.163508176764,53.2529925397285,13.011932042438));
#72703=CARTESIAN_POINT('Ctrl Pts',(87.1720264167175,53.2540612142451,13.0194951526666));
#72704=CARTESIAN_POINT('Ctrl Pts',(87.180642873398,53.2551312395179,13.0269407069644));
#72705=CARTESIAN_POINT('Ctrl Pts',(87.1806428308131,53.4258009314892,13.0269406701664));
#72706=CARTESIAN_POINT('Ctrl Pts',(87.1743362995706,53.4250054859773,13.021491141811));
#72707=CARTESIAN_POINT('Ctrl Pts',(87.1680831488515,53.4242081263248,13.0159792999802));
#72708=CARTESIAN_POINT('Ctrl Pts',(87.1526872726662,53.4222224618141,13.0021368621377));
#72709=CARTESIAN_POINT('Ctrl Pts',(87.1436118734228,53.4210318639093,12.9937342173096));
#72710=CARTESIAN_POINT('Ctrl Pts',(87.1215109639658,53.4180797241952,12.9726638567472));
#72711=CARTESIAN_POINT('Ctrl Pts',(87.1086323299979,53.4163126955017,12.9598470804606));
#72712=CARTESIAN_POINT('Ctrl Pts',(87.0889835770527,53.4135381775367,12.9394352080008));
#72713=CARTESIAN_POINT('Ctrl Pts',(87.0820218227003,53.4125390165741,12.9320270653993));
#72714=CARTESIAN_POINT('Ctrl Pts',(87.0691988395837,53.4106674557414,12.918049336971));
#72715=CARTESIAN_POINT('Ctrl Pts',(87.0633154884272,53.4097960610142,12.9115007717413));
#72716=CARTESIAN_POINT('Ctrl Pts',(87.0502925727587,53.4078379539761,12.8966986971728));
#72717=CARTESIAN_POINT('Ctrl Pts',(87.0431904664282,53.4067497761132,12.8884133838061));
#72718=CARTESIAN_POINT('Ctrl Pts',(87.0252313496684,53.4039442570272,12.8669074889071));
#72719=CARTESIAN_POINT('Ctrl Pts',(87.0145335404841,53.4022207250683,12.8535577183681));
#72720=CARTESIAN_POINT('Ctrl Pts',(86.9496254954417,53.3914231563109,12.7691189825988));
#72721=CARTESIAN_POINT('Ctrl Pts',(86.9027909286916,53.3820734526397,12.692703495933));
#72722=CARTESIAN_POINT('Ctrl Pts',(86.8430929950701,53.3674346628164,12.5673411062292));
#72723=CARTESIAN_POINT('Ctrl Pts',(86.824442372871,53.3622125720084,12.521446286182));
#72724=CARTESIAN_POINT('Ctrl Pts',(86.8028678730855,53.3552387132727,12.4579504163095));
#72725=CARTESIAN_POINT('Ctrl Pts',(86.7975635046663,53.3534228278343,12.4412070441592));
#72726=CARTESIAN_POINT('Ctrl Pts',(86.7889868668633,53.3503052046175,12.4120470621341));
#72727=CARTESIAN_POINT('Ctrl Pts',(86.785552508179,53.3489968862542,12.3996812210068));
#72728=CARTESIAN_POINT('Ctrl Pts',(86.7807334664907,53.3470691505736,12.3812505326128));
#72729=CARTESIAN_POINT('Ctrl Pts',(86.7792050926382,53.3464423956993,12.3752247628335));
#72730=CARTESIAN_POINT('Ctrl Pts',(86.7765367977728,53.3453200200336,12.3643709214399));
#72731=CARTESIAN_POINT('Ctrl Pts',(86.7753808583461,53.3448235485095,12.3595471757687));
#72732=CARTESIAN_POINT('Ctrl Pts',(86.772837291566,53.343707371493,12.3486515437848));
#72733=CARTESIAN_POINT('Ctrl Pts',(86.7714660254179,53.3430885928258,12.3425760648276));
#72734=CARTESIAN_POINT('Ctrl Pts',(86.76739326784,53.3411960252479,12.323892510249));
#72735=CARTESIAN_POINT('Ctrl Pts',(86.7648388967869,53.3399300354423,12.3112525290357));
#72736=CARTESIAN_POINT('Ctrl Pts',(86.7513700162843,53.3327578184018,12.2389480823466));
#72737=CARTESIAN_POINT('Ctrl Pts',(86.7445464424472,53.3270381670947,12.1785910719884));
#72738=CARTESIAN_POINT('Ctrl Pts',(86.7389670051514,53.3142432876107,12.0423534299551));
#72739=CARTESIAN_POINT('Ctrl Pts',(86.742635134136,53.3072033728407,11.9666197628864));
#72740=CARTESIAN_POINT('Ctrl Pts',(86.7560566600149,53.2978758065233,11.8697709449612));
#72741=CARTESIAN_POINT('Ctrl Pts',(86.7596619502016,53.2957543189757,11.8479596572584));
#72742=CARTESIAN_POINT('Ctrl Pts',(86.7671881734674,53.2918980023108,11.8088078804139));
#72743=CARTESIAN_POINT('Ctrl Pts',(86.7709075752303,53.2901694303619,11.7914342521375));
#72744=CARTESIAN_POINT('Ctrl Pts',(86.7773070816809,53.2874417910367,11.7643322192337));
#72745=CARTESIAN_POINT('Ctrl Pts',(86.7797409192025,53.2864505890083,11.7545473902702));
#72746=CARTESIAN_POINT('Ctrl Pts',(86.7845195335236,53.2845860869579,11.7362678217));
#72747=CARTESIAN_POINT('Ctrl Pts',(86.7868367415506,53.2837137249435,11.7277664257047));
#72748=CARTESIAN_POINT('Ctrl Pts',(86.7922528064276,53.2817429947288,11.7086809604643));
#72749=CARTESIAN_POINT('Ctrl Pts',(86.7954013963993,53.2806430741272,11.6981119286266));
#72750=CARTESIAN_POINT('Ctrl Pts',(86.8039028215265,53.277785425259,11.6708762075711));
#72751=CARTESIAN_POINT('Ctrl Pts',(86.8094631084701,53.2760211059665,11.6542774845786));
#72752=CARTESIAN_POINT('Ctrl Pts',(86.8400105828043,53.2668309478734,11.568981708683));
#72753=CARTESIAN_POINT('Ctrl Pts',(86.8705468156836,53.2592285556787,11.5024349977368));
#72754=CARTESIAN_POINT('Ctrl Pts',(86.9368333641795,53.2451044765989,11.3856998462628));
#72755=CARTESIAN_POINT('Ctrl Pts',(86.9708449156313,53.2386288866275,11.33475436133));
#72756=CARTESIAN_POINT('Ctrl Pts',(87.0204768562574,53.2302005573834,11.2709206285754));
#72757=CARTESIAN_POINT('Ctrl Pts',(87.0329171919717,53.2281608980847,11.255665844093));
#72758=CARTESIAN_POINT('Ctrl Pts',(87.0547835720146,53.224704037964,11.2300902031486));
#72759=CARTESIAN_POINT('Ctrl Pts',(87.0640342951544,53.2232783350877,11.2196247538526));
#72760=CARTESIAN_POINT('Ctrl Pts',(87.0777917420912,53.2212131152558,11.204568835072));
#72761=CARTESIAN_POINT('Ctrl Pts',(87.0821631471431,53.2205647333298,11.1998571642833));
#72762=CARTESIAN_POINT('Ctrl Pts',(87.0899440778987,53.2194246594765,11.19159723377));
#72763=CARTESIAN_POINT('Ctrl Pts',(87.0933386676946,53.2189319149457,11.188035369674));
#72764=CARTESIAN_POINT('Ctrl Pts',(87.100929468367,53.2178403121735,11.1801626481716));
#72765=CARTESIAN_POINT('Ctrl Pts',(87.1051357102015,53.2172422366549,11.1758617633376));
#72766=CARTESIAN_POINT('Ctrl Pts',(87.1174343768849,53.2155125088264,11.1634638412944));
#72767=CARTESIAN_POINT('Ctrl Pts',(87.1256062680018,53.2143867011865,11.1554457657749));
#72768=CARTESIAN_POINT('Ctrl Pts',(87.1956854808461,53.2049159360581,11.088521372613));
#72769=CARTESIAN_POINT('Ctrl Pts',(87.2632970299013,53.1969638755544,11.0358793469521));
#72770=CARTESIAN_POINT('Ctrl Pts',(87.3801771608586,53.1840333805324,10.9624961337654));
#72771=CARTESIAN_POINT('Ctrl Pts',(87.4263416165389,53.1791058824947,10.9373583323227));
#72772=CARTESIAN_POINT('Ctrl Pts',(87.4941503445692,53.1719690393177,10.9057136033897));
#72773=CARTESIAN_POINT('Ctrl Pts',(87.5146182916453,53.1698275950103,10.896810895419));
#72774=CARTESIAN_POINT('Ctrl Pts',(87.5519033764804,53.1659386317299,10.88174892614));
#72775=CARTESIAN_POINT('Ctrl Pts',(87.5686366863371,53.1641975348209,10.8753972373276));
#72776=CARTESIAN_POINT('Ctrl Pts',(87.5950233905697,53.1614546236232,10.8660143026159));
#72777=CARTESIAN_POINT('Ctrl Pts',(87.6045888929747,53.160460824184,10.8627410041958));
#72778=CARTESIAN_POINT('Ctrl Pts',(87.6225597507285,53.1585940439212,10.8568301340054));
#72779=CARTESIAN_POINT('Ctrl Pts',(87.6309555187496,53.1577220231255,10.8541651208067));
#72780=CARTESIAN_POINT('Ctrl Pts',(87.6498864610458,53.1557555380268,10.8483720687597));
#72781=CARTESIAN_POINT('Ctrl Pts',(87.6604357180292,53.1546595503998,10.8452930607038));
#72782=CARTESIAN_POINT('Ctrl Pts',(87.6877601302789,53.151819397866,10.8377012838283));
#72783=CARTESIAN_POINT('Ctrl Pts',(87.7045896201895,53.15006877755,10.8333952976683));
#72784=CARTESIAN_POINT('Ctrl Pts',(87.8006196166402,53.1400662759991,10.8109131766325));
#72785=CARTESIAN_POINT('Ctrl Pts',(87.8813147875154,53.1315914198,10.8000305166795));
#72786=CARTESIAN_POINT('Ctrl Pts',(88.0175852036541,53.1172239105759,10.7948202513751));
#72787=CARTESIAN_POINT('Ctrl Pts',(88.0727745163799,53.1113950628162,10.7963048142722));
#72788=CARTESIAN_POINT('Ctrl Pts',(88.146254503647,53.1037117947099,10.8030852748142));
#72789=CARTESIAN_POINT('Ctrl Pts',(88.1647753570916,53.1017821873963,10.8052063503584));
#72790=CARTESIAN_POINT('Ctrl Pts',(88.1965351239592,53.0984914775908,10.8095539492406));
#72791=CARTESIAN_POINT('Ctrl Pts',(88.2097974223791,53.0971228444555,10.8115839616569));
#72792=CARTESIAN_POINT('Ctrl Pts',(88.2292631079569,53.0951243033126,10.8148800086814));
#72793=CARTESIAN_POINT('Ctrl Pts',(88.2354924915123,53.0944862887158,10.8159827423222));
#72794=CARTESIAN_POINT('Ctrl Pts',(88.2465929146709,53.0933524448222,10.8180334144628));
#72795=CARTESIAN_POINT('Ctrl Pts',(88.2514669066145,53.092855675258,10.8189633965339));
#72796=CARTESIAN_POINT('Ctrl Pts',(88.2623440776884,53.0917494404576,10.8211049621593));
#72797=CARTESIAN_POINT('Ctrl Pts',(88.2683440995254,53.0911408168332,10.8223314264609));
#72798=CARTESIAN_POINT('Ctrl Pts',(88.2864194141755,53.0893114371129,10.8261626179787));
#72799=CARTESIAN_POINT('Ctrl Pts',(88.298466398465,53.0880977465207,10.8289002873616));
#72800=CARTESIAN_POINT('Ctrl Pts',(88.3847382968194,53.0794328010571,10.849833952263));
#72801=CARTESIAN_POINT('Ctrl Pts',(88.4572412975141,53.0722879195457,10.8745246671426));
#72802=CARTESIAN_POINT('Ctrl Pts',(88.6031961230309,53.0573242846725,10.9394385622575));
#72803=CARTESIAN_POINT('Ctrl Pts',(88.6757708175089,53.0495325654057,10.9806828417891));
#72804=CARTESIAN_POINT('Ctrl Pts',(88.758114356599,53.0397782748239,11.0388543638781));
#72805=CARTESIAN_POINT('Ctrl Pts',(88.7722363912794,53.0380703642393,11.0492762890238));
#72806=CARTESIAN_POINT('Ctrl Pts',(88.7940887735301,53.0353679252044,11.06611363734));
#72807=CARTESIAN_POINT('Ctrl Pts',(88.8019671879608,53.0343810181749,11.0723342318931));
#72808=CARTESIAN_POINT('Ctrl Pts',(88.8166255014765,53.0325202257917,11.0841928440842));
#72809=CARTESIAN_POINT('Ctrl Pts',(88.8234220811331,53.0316472417752,11.0898093976243));
#72810=CARTESIAN_POINT('Ctrl Pts',(88.8386373397229,53.0296692076657,11.1026519242035));
#72811=CARTESIAN_POINT('Ctrl Pts',(88.8470207791278,53.0285625554123,11.1099182472026));
#72812=CARTESIAN_POINT('Ctrl Pts',(88.8685552350983,53.0256748717389,11.1290829718841));
#72813=CARTESIAN_POINT('Ctrl Pts',(88.8815535628568,53.0238870134857,11.1411481676868));
#72814=CARTESIAN_POINT('Ctrl Pts',(88.9124633002674,53.0195220834512,11.1710679673297));
#72815=CARTESIAN_POINT('Ctrl Pts',(88.9301014311276,53.0169341977256,11.1891922870389));
#72816=CARTESIAN_POINT('Ctrl Pts',(88.9916209429204,53.0075433220139,11.2563044355828));
#72817=CARTESIAN_POINT('Ctrl Pts',(89.0322184093449,53.0006319543569,11.3081510593211));
#72818=CARTESIAN_POINT('Ctrl Pts',(89.1041642543375,52.9869299370977,11.4163730820691));
#72819=CARTESIAN_POINT('Ctrl Pts',(89.1356115581439,52.9801598257506,11.4724730876544));
#72820=CARTESIAN_POINT('Ctrl Pts',(89.1680855505055,52.9722572636082,11.5423423466759));
#72821=CARTESIAN_POINT('Ctrl Pts',(89.1733123175282,52.9709503881399,11.5540484093683));
#72822=CARTESIAN_POINT('Ctrl Pts',(89.1808084034402,52.9690243505817,11.5715438260489));
#72823=CARTESIAN_POINT('Ctrl Pts',(89.1832136657773,52.9683978689227,11.5772733520239));
#72824=CARTESIAN_POINT('Ctrl Pts',(89.1874632619129,52.9672757671348,11.5876081126859));
#72825=CARTESIAN_POINT('Ctrl Pts',(89.1893227576895,52.966779298458,11.592206704995));
#72826=CARTESIAN_POINT('Ctrl Pts',(89.1934572169716,52.9656628608343,11.6026062676374));
#72827=CARTESIAN_POINT('Ctrl Pts',(89.1957164976753,52.9650438208894,11.6084132351972));
#72828=CARTESIAN_POINT('Ctrl Pts',(89.2025246358033,52.9631496103649,11.6263004921114));
#72829=CARTESIAN_POINT('Ctrl Pts',(89.2069323771307,52.9618822584453,11.6384343191065));
#72830=CARTESIAN_POINT('Ctrl Pts',(89.2169432469068,52.9588974548337,11.6673596396495));
#72831=CARTESIAN_POINT('Ctrl Pts',(89.2223820315127,52.9571877953838,11.684205655217));
#72832=CARTESIAN_POINT('Ctrl Pts',(89.2418856285817,52.9506762649702,11.7492356995046));
#72833=CARTESIAN_POINT('Ctrl Pts',(89.2534430343471,52.9459632329482,11.7981279600959));
#72834=CARTESIAN_POINT('Ctrl Pts',(89.2772681025976,52.9329794250132,11.9345948434656));
#72835=CARTESIAN_POINT('Ctrl Pts',(89.2833384199377,52.9247468114159,12.0229431818811));
#72836=CARTESIAN_POINT('Ctrl Pts',(89.2795847020413,52.9145602018262,12.1283485130167));
#72837=CARTESIAN_POINT('Ctrl Pts',(89.2786264699751,52.9128935361273,12.1454830166634));
#72838=CARTESIAN_POINT('Ctrl Pts',(89.2764902721414,52.9101480862054,12.173488603561));
#72839=CARTESIAN_POINT('Ctrl Pts',(89.2755185174059,52.9090757050422,12.1843736862948));
#72840=CARTESIAN_POINT('Ctrl Pts',(89.273510459982,52.9071313783768,12.2040030975057));
#72841=CARTESIAN_POINT('Ctrl Pts',(89.2725234395056,52.9062610283024,12.2127518933196));
#72842=CARTESIAN_POINT('Ctrl Pts',(89.2702023512373,52.9043806150649,12.2315673532507));
#72843=CARTESIAN_POINT('Ctrl Pts',(89.2688383586928,52.9033696695075,12.2416296041543));
#72844=CARTESIAN_POINT('Ctrl Pts',(89.2647059530782,52.9005447071138,12.2695913144076));
#72845=CARTESIAN_POINT('Ctrl Pts',(89.2616751975165,52.8987226067386,12.2874486474905));
#72846=CARTESIAN_POINT('Ctrl Pts',(89.2539937456106,52.8945928600967,12.3274964690376));
#72847=CARTESIAN_POINT('Ctrl Pts',(89.2491287026293,52.892279158034,12.3496388724209));
#72848=CARTESIAN_POINT('Ctrl Pts',(89.2306913532324,52.8844019954083,12.4239989880257));
#72849=CARTESIAN_POINT('Ctrl Pts',(89.2143872341998,52.8787654563511,12.4754727203919));
#72850=CARTESIAN_POINT('Ctrl Pts',(89.1648757976314,52.8643716092896,12.6029661035577));
#72851=CARTESIAN_POINT('Ctrl Pts',(89.1274025669483,52.8555840413405,12.6770729622982));
#72852=CARTESIAN_POINT('Ctrl Pts',(89.0766828758596,52.8458963161823,12.7569107348018));
#72853=CARTESIAN_POINT('Ctrl Pts',(89.0702546409967,52.8447014861323,12.7667262492174));
#72854=CARTESIAN_POINT('Ctrl Pts',(89.0602921451754,52.8429002529548,12.7814878802534));
#72855=CARTESIAN_POINT('Ctrl Pts',(89.0568571737377,52.8422879459457,12.7864996116957));
#72856=CARTESIAN_POINT('Ctrl Pts',(89.0508345918231,52.8412296338958,12.7951529152225));
#72857=CARTESIAN_POINT('Ctrl Pts',(89.0482636307569,52.8407825747008,12.7988056459588));
#72858=CARTESIAN_POINT('Ctrl Pts',(89.0421269240648,52.8397265336142,12.8074274532702));
#72859=CARTESIAN_POINT('Ctrl Pts',(89.0385444757098,52.8391186952639,12.8123844573347));
#72860=CARTESIAN_POINT('Ctrl Pts',(89.0276429985925,52.8372941490059,12.8272414742837));
#72861=CARTESIAN_POINT('Ctrl Pts',(89.0202153337361,52.8360844519654,12.8370616189461));
#72862=CARTESIAN_POINT('Ctrl Pts',(88.9823875275384,52.8300783294306,12.8855905255051));
#72863=CARTESIAN_POINT('Ctrl Pts',(88.9498934610293,52.8254036125229,12.9226230338728));
#72864=CARTESIAN_POINT('Ctrl Pts',(88.853791285557,52.8125125897115,13.0200880685693));
#72865=CARTESIAN_POINT('Ctrl Pts',(88.7859656525664,52.804400662786,13.0759547566736));
#72866=CARTESIAN_POINT('Ctrl Pts',(88.686067098715,52.7929676115575,13.1422078952438));
#72867=CARTESIAN_POINT('Ctrl Pts',(88.6585382890826,52.789866493102,13.1589925856943));
#72868=CARTESIAN_POINT('Ctrl Pts',(88.6191324948814,52.7854708056106,13.1810074223256));
#72869=CARTESIAN_POINT('Ctrl Pts',(88.607766703452,52.7842078810806,13.1871316404283));
#72870=CARTESIAN_POINT('Ctrl Pts',(88.5883279549346,52.7820547193353,13.1972264709698));
#72871=CARTESIAN_POINT('Ctrl Pts',(88.5803023389341,52.7811676829258,13.2012866301586));
#72872=CARTESIAN_POINT('Ctrl Pts',(88.563916170857,52.7793599788299,13.2093589531419));
#72873=CARTESIAN_POINT('Ctrl Pts',(88.5555534662902,52.7784391781227,13.2133654598325));
#72874=CARTESIAN_POINT('Ctrl Pts',(88.5345647854469,52.7761319350997,13.223139831433));
#72875=CARTESIAN_POINT('Ctrl Pts',(88.5218870900371,52.7747416667695,13.2287927656928));
#72876=CARTESIAN_POINT('Ctrl Pts',(88.4693883834337,52.768995601822,13.2511774899006));
#72877=CARTESIAN_POINT('Ctrl Pts',(88.4288248404821,52.764580372948,13.2660778717099));
#72878=CARTESIAN_POINT('Ctrl Pts',(88.313684937213,52.7520945759315,13.3018276019312));
#72879=CARTESIAN_POINT('Ctrl Pts',(88.2378473576537,52.7439134533325,13.3179686969941));
#72880=CARTESIAN_POINT('Ctrl Pts',(88.110910077758,52.7304611387984,13.3330694253974));
#72881=CARTESIAN_POINT('Ctrl Pts',(88.0604773065984,52.7251820375424,13.3360395713598));
#72882=CARTESIAN_POINT('Ctrl Pts',(88.0001483484465,52.7190241107554,13.335991806336));
#72883=CARTESIAN_POINT('Ctrl Pts',(87.9903020752933,52.7180241434539,13.3358695067524));
#72884=CARTESIAN_POINT('Ctrl Pts',(87.9748501246574,52.7164637481889,13.3354977941489));
#72885=CARTESIAN_POINT('Ctrl Pts',(87.969243327152,52.7158993880113,13.3353257452641));
#72886=CARTESIAN_POINT('Ctrl Pts',(87.9585929779854,52.7148310610893,13.3349282833395));
#72887=CARTESIAN_POINT('Ctrl Pts',(87.9535495675135,52.7143267663684,13.3347099487096));
#72888=CARTESIAN_POINT('Ctrl Pts',(87.9413788672194,52.7131134379033,13.3341103405441));
#72889=CARTESIAN_POINT('Ctrl Pts',(87.9342532101594,52.7124060534704,13.3336990482815));
#72890=CARTESIAN_POINT('Ctrl Pts',(87.9088621077425,52.7098947822123,13.3320185893685));
#72891=CARTESIAN_POINT('Ctrl Pts',(87.8906196938915,52.708107853037,13.3304144592637));
#72892=CARTESIAN_POINT('Ctrl Pts',(87.8568620913763,52.7048219610243,13.3267086760515));
#72893=CARTESIAN_POINT('Ctrl Pts',(87.8413394460499,52.703319233422,13.3247137149969));
#72894=CARTESIAN_POINT('Ctrl Pts',(87.7576549415357,52.6952419761042,13.3123822712204));
#72895=CARTESIAN_POINT('Ctrl Pts',(87.6903785885725,52.6888304194108,13.2967949164672));
#72896=CARTESIAN_POINT('Ctrl Pts',(87.5586013782521,52.6758550212628,13.2547174752188));
#72897=CARTESIAN_POINT('Ctrl Pts',(87.4943593346212,52.6693112279041,13.2282364520719));
#72898=CARTESIAN_POINT('Ctrl Pts',(87.4186656291913,52.6610687245653,13.1895146846946));
#72899=CARTESIAN_POINT('Ctrl Pts',(87.4048573173293,52.6595424937634,13.1821255530731));
#72900=CARTESIAN_POINT('Ctrl Pts',(87.3826525252733,52.6570484483686,13.1697097105431));
#72901=CARTESIAN_POINT('Ctrl Pts',(87.3741709190312,52.6560861534063,13.1648377416535));
#72902=CARTESIAN_POINT('Ctrl Pts',(87.3585851005065,52.6542992563279,13.1556439483817));
#72903=CARTESIAN_POINT('Ctrl Pts',(87.3514653592732,52.6534756785054,13.1513493376085));
#72904=CARTESIAN_POINT('Ctrl Pts',(87.3371111111189,52.6517999688757,13.1424974992895));
#72905=CARTESIAN_POINT('Ctrl Pts',(87.329879447325,52.6509477332218,13.1379365112114));
#72906=CARTESIAN_POINT('Ctrl Pts',(87.3134618915067,52.6489941427409,13.1273488035069));
#72907=CARTESIAN_POINT('Ctrl Pts',(87.3043072047548,52.6478911000812,13.1212753049212));
#72908=CARTESIAN_POINT('Ctrl Pts',(87.255383607329,52.6419203044738,13.0878958009803));
#72909=CARTESIAN_POINT('Ctrl Pts',(87.2171260935039,52.6369746254133,13.0584661740469));
#72910=CARTESIAN_POINT('Ctrl Pts',(87.1806428293121,52.6319631729084,13.0269406688694));
#72911=CARTESIAN_POINT('Origin',(88.011,66.41344859951,12.066));
#72912=CARTESIAN_POINT('',(87.1806428357067,51.6672833294972,13.026940674395));
#72913=CARTESIAN_POINT('',(87.1792973239246,51.8375066538898,13.0285052387874));
#72914=CARTESIAN_POINT('',(87.1806428354228,66.41344859951,13.0269406741497));
#72915=CARTESIAN_POINT('',(86.7410001453939,52.3539891800374,12.0650476267737));
#72916=CARTESIAN_POINT('Ctrl Pts',(87.1806428357067,51.6672833294972,13.026940674395));
#72917=CARTESIAN_POINT('Ctrl Pts',(87.1817392149757,51.6674344362791,13.0278880652227));
#72918=CARTESIAN_POINT('Ctrl Pts',(87.1828372304032,51.6675855942185,13.0288335924603));
#72919=CARTESIAN_POINT('Ctrl Pts',(87.2213438210188,51.6728804841237,13.0618779302639));
#72920=CARTESIAN_POINT('Ctrl Pts',(87.2605856494101,51.6780774533418,13.0917716257743));
#72921=CARTESIAN_POINT('Ctrl Pts',(87.3535931839974,51.6898996608408,13.1544241286476));
#72922=CARTESIAN_POINT('Ctrl Pts',(87.4082672543514,51.6965107849232,13.1856278242971));
#72923=CARTESIAN_POINT('Ctrl Pts',(87.4739873489515,51.7039430767255,13.2169195082281));
#72924=CARTESIAN_POINT('Ctrl Pts',(87.4829892692356,51.7049503422229,13.2210770503001));
#72925=CARTESIAN_POINT('Ctrl Pts',(87.4972249153891,51.7065254537571,13.2274505763393));
#72926=CARTESIAN_POINT('Ctrl Pts',(87.5024260803381,51.7070972484085,13.2297374496546));
#72927=CARTESIAN_POINT('Ctrl Pts',(87.5122573403788,51.7081709014651,13.2339816026196));
#72928=CARTESIAN_POINT('Ctrl Pts',(87.5168837642477,51.7086731525451,13.2359463287323));
#72929=CARTESIAN_POINT('Ctrl Pts',(87.5279705418267,51.7098698347381,13.2405771072161));
#72930=CARTESIAN_POINT('Ctrl Pts',(87.5344414706581,51.7105627350852,13.2432174033289));
#72931=CARTESIAN_POINT('Ctrl Pts',(87.5570221378625,51.712962567406,13.2522141505839));
#72932=CARTESIAN_POINT('Ctrl Pts',(87.573241005222,51.7146544656587,13.2582948797009));
#72933=CARTESIAN_POINT('Ctrl Pts',(87.6146089505715,51.7189030076769,13.2728463288263));
#72934=CARTESIAN_POINT('Ctrl Pts',(87.6399094313916,51.7214399748708,13.2808645944262));
#72935=CARTESIAN_POINT('Ctrl Pts',(87.7214345733798,51.7294789526008,13.3039165351732));
#72936=CARTESIAN_POINT('Ctrl Pts',(87.7784492768445,51.7349007854946,13.3158825738163));
#72937=CARTESIAN_POINT('Ctrl Pts',(87.9062412190162,51.7470004134378,13.3336523343811));
#72938=CARTESIAN_POINT('Ctrl Pts',(87.9770770967976,51.7536772256821,13.3375200956158));
#72939=CARTESIAN_POINT('Ctrl Pts',(88.0637009184863,51.7620798466425,13.3350050560877));
#72940=CARTESIAN_POINT('Ctrl Pts',(88.0795332609607,51.7636248911654,13.334248539426));
#72941=CARTESIAN_POINT('Ctrl Pts',(88.1050081914213,51.7661286509612,13.3325528896491));
#72942=CARTESIAN_POINT('Ctrl Pts',(88.1146618962562,51.7670815527957,13.3317993366585));
#72943=CARTESIAN_POINT('Ctrl Pts',(88.1331645870808,51.7689164368705,13.3301419710605));
#72944=CARTESIAN_POINT('Ctrl Pts',(88.1420145876308,51.7697978256503,13.3292554282161));
#72945=CARTESIAN_POINT('Ctrl Pts',(88.1625342767225,51.7718506439428,13.3269819429118));
#72946=CARTESIAN_POINT('Ctrl Pts',(88.1741952464939,51.7730241716353,13.3255258572246));
#72947=CARTESIAN_POINT('Ctrl Pts',(88.2122951475645,51.7768826095321,13.3202304376413));
#72948=CARTESIAN_POINT('Ctrl Pts',(88.2386311296509,51.7795881173133,13.315718977328));
#72949=CARTESIAN_POINT('Ctrl Pts',(88.3024759949519,51.7862485109085,13.3026972344534));
#72950=CARTESIAN_POINT('Ctrl Pts',(88.3397761485748,51.7902270454978,13.2933075706572));
#72951=CARTESIAN_POINT('Ctrl Pts',(88.4229203949389,51.7992927949267,13.2683153262318));
#72952=CARTESIAN_POINT('Ctrl Pts',(88.4684155811112,51.804394462812,13.2517533452652));
#72953=CARTESIAN_POINT('Ctrl Pts',(88.5700267689911,51.8160551147531,13.2080433012511));
#72954=CARTESIAN_POINT('Ctrl Pts',(88.6253249693706,51.8225997333426,13.1792749187157));
#72955=CARTESIAN_POINT('Ctrl Pts',(88.6868133522788,51.8299785158323,13.1413029767386));
#72956=CARTESIAN_POINT('Ctrl Pts',(88.6952673438125,51.8309952606904,13.1359431778764));
#72957=CARTESIAN_POINT('Ctrl Pts',(88.7083888441128,51.8325759297479,13.1274050420334));
#72958=CARTESIAN_POINT('Ctrl Pts',(88.713099726916,51.8331439482561,13.1242947799039));
#72959=CARTESIAN_POINT('Ctrl Pts',(88.7219752823662,51.8342149117723,13.118349526282));
#72960=CARTESIAN_POINT('Ctrl Pts',(88.7261438787201,51.8347182162491,13.1155211347422));
#72961=CARTESIAN_POINT('Ctrl Pts',(88.7361175492315,51.8359233741614,13.1086669840792));
#72962=CARTESIAN_POINT('Ctrl Pts',(88.7419060867106,51.8366236369168,13.1046174468439));
#72963=CARTESIAN_POINT('Ctrl Pts',(88.7621708584317,51.8390792589787,13.0901873075785));
#72964=CARTESIAN_POINT('Ctrl Pts',(88.7764632817917,51.8408186378754,13.0795498901577));
#72965=CARTESIAN_POINT('Ctrl Pts',(88.8024023463741,51.843999787252,13.0593823757239));
#72966=CARTESIAN_POINT('Ctrl Pts',(88.8141120330593,51.8454454321576,13.0499397004182));
#72967=CARTESIAN_POINT('Ctrl Pts',(88.8748140165075,51.8530082505001,12.9991838161022));
#72968=CARTESIAN_POINT('Ctrl Pts',(88.9207990569598,51.8589815816981,12.9544109119908));
#72969=CARTESIAN_POINT('Ctrl Pts',(89.0091377830331,51.8714932992909,12.854313642337));
#72970=CARTESIAN_POINT('Ctrl Pts',(89.0507144980876,51.8780183416019,12.798604190185));
#72971=CARTESIAN_POINT('Ctrl Pts',(89.0967978004155,51.8864042547085,12.7249752222019));
#72972=CARTESIAN_POINT('Ctrl Pts',(89.1057592992095,51.8881004701978,12.7099776503915));
#72973=CARTESIAN_POINT('Ctrl Pts',(89.1198640045623,51.8908845307619,12.6852269738495));
#72974=CARTESIAN_POINT('Ctrl Pts',(89.1251948337624,51.8919656596498,12.6755828732984));
#72975=CARTESIAN_POINT('Ctrl Pts',(89.1345618343001,51.8939195037024,12.6581034254008));
#72976=CARTESIAN_POINT('Ctrl Pts',(89.1386432734137,51.8947905554241,12.6502929914847));
#72977=CARTESIAN_POINT('Ctrl Pts',(89.1472240298164,51.8966654537922,12.6334476363894));
#72978=CARTESIAN_POINT('Ctrl Pts',(89.1516975435629,51.8976701320607,12.6244003626394));
#72979=CARTESIAN_POINT('Ctrl Pts',(89.1637648405395,51.9004580846247,12.5992451039592));
#72980=CARTESIAN_POINT('Ctrl Pts',(89.1711280119999,51.9022490949957,12.5830300103371));
#72981=CARTESIAN_POINT('Ctrl Pts',(89.2068749783876,51.9114287868335,12.4996971376571));
#72982=CARTESIAN_POINT('Ctrl Pts',(89.2297789064264,51.9189941700965,12.4303948988274));
#72983=CARTESIAN_POINT('Ctrl Pts',(89.2653190483963,51.935161767403,12.2807872587821));
#72984=CARTESIAN_POINT('Ctrl Pts',(89.276456050109,51.9437521262372,12.2004349617768));
#72985=CARTESIAN_POINT('Ctrl Pts',(89.2805289953162,51.9536989766017,12.1039514713849));
#72986=CARTESIAN_POINT('Ctrl Pts',(89.2808999066288,51.9552978033713,12.0883268779407));
#72987=CARTESIAN_POINT('Ctrl Pts',(89.2810153078521,51.9575168102198,12.0664467473331));
#72988=CARTESIAN_POINT('Ctrl Pts',(89.2810021214388,51.9581485716723,12.0601948973341));
#72989=CARTESIAN_POINT('Ctrl Pts',(89.2808948176609,51.959286291433,12.048892622697));
#72990=CARTESIAN_POINT('Ctrl Pts',(89.2808167375596,51.959793090378,12.0438422031532));
#72991=CARTESIAN_POINT('Ctrl Pts',(89.2805912850935,51.9608454063165,12.0333210223533));
#72992=CARTESIAN_POINT('Ctrl Pts',(89.2804386828509,51.9613906324065,12.0278505381235));
#72993=CARTESIAN_POINT('Ctrl Pts',(89.2799344176376,51.962848356043,12.0131771325673));
#72994=CARTESIAN_POINT('Ctrl Pts',(89.2795179978313,51.9637574004397,12.0039764644561));
#72995=CARTESIAN_POINT('Ctrl Pts',(89.2767486519361,51.9686063171211,11.9546705563998));
#72996=CARTESIAN_POINT('Ctrl Pts',(89.2725935187751,51.972458744986,11.9146833579683));
#72997=CARTESIAN_POINT('Ctrl Pts',(89.2581369648283,51.9815722209583,11.8196751289201));
#72998=CARTESIAN_POINT('Ctrl Pts',(89.2460835817811,51.9867853967364,11.7650086279144));
#72999=CARTESIAN_POINT('Ctrl Pts',(89.2103850981192,51.998770218907,11.6422724191995));
#73000=CARTESIAN_POINT('Ctrl Pts',(89.1844816080507,52.0055438242668,11.5750745540258));
#73001=CARTESIAN_POINT('Ctrl Pts',(89.146057339155,52.0140592987613,11.4960882375117));
#73002=CARTESIAN_POINT('Ctrl Pts',(89.1388081664462,52.0156144717272,11.4818739303158));
#73003=CARTESIAN_POINT('Ctrl Pts',(89.12672209458,52.0181305935031,11.4592394202074));
#73004=CARTESIAN_POINT('Ctrl Pts',(89.1220528317171,52.0190856223875,11.4507311273435));
#73005=CARTESIAN_POINT('Ctrl Pts',(89.1129218042035,52.0209219322914,11.4345355698235));
#73006=CARTESIAN_POINT('Ctrl Pts',(89.1084759294346,52.0218025995724,11.4268399549019));
#73007=CARTESIAN_POINT('Ctrl Pts',(89.0979897575588,52.023849746178,11.4091208523541));
#73008=CARTESIAN_POINT('Ctrl Pts',(89.0918910682549,52.0250182862934,11.3991331297484));
#73009=CARTESIAN_POINT('Ctrl Pts',(89.0715776151549,52.0288415853856,11.3668769521485));
#73010=CARTESIAN_POINT('Ctrl Pts',(89.0568070661922,52.031516420849,11.3449693284727));
#73011=CARTESIAN_POINT('Ctrl Pts',(89.0192456406346,52.0380820025928,11.2928426036675));
#73012=CARTESIAN_POINT('Ctrl Pts',(88.9957675525294,52.04199549108,11.2631526609964));
#73013=CARTESIAN_POINT('Ctrl Pts',(88.938912261982,52.0510598404315,11.1975062318521));
#73014=CARTESIAN_POINT('Ctrl Pts',(88.9047061400356,52.0562280683231,11.1623455640425));
#73015=CARTESIAN_POINT('Ctrl Pts',(88.8223671330295,52.0679963130974,11.0869674223922));
#73016=CARTESIAN_POINT('Ctrl Pts',(88.7731064762636,52.0745821144528,11.0481505325354));
#73017=CARTESIAN_POINT('Ctrl Pts',(88.7128667057587,52.0820013128468,11.0075182732179));
#73018=CARTESIAN_POINT('Ctrl Pts',(88.7044916479797,52.0830193939742,11.0020123141498));
#73019=CARTESIAN_POINT('Ctrl Pts',(88.6912963709355,52.0846016706885,10.9935594459112));
#73020=CARTESIAN_POINT('Ctrl Pts',(88.6865204887862,52.0851699736504,10.9905447623639));
#73021=CARTESIAN_POINT('Ctrl Pts',(88.6774474793814,52.0862411351503,10.9849018888959));
#73022=CARTESIAN_POINT('Ctrl Pts',(88.6731547776891,52.0867443556721,10.9822673664916));
#73023=CARTESIAN_POINT('Ctrl Pts',(88.6628088303405,52.087948854134,10.9760022633703));
#73024=CARTESIAN_POINT('Ctrl Pts',(88.6567407659716,52.0886485460433,10.9723964663112));
#73025=CARTESIAN_POINT('Ctrl Pts',(88.6352875561016,52.09109980242,10.9598892612214));
#73026=CARTESIAN_POINT('Ctrl Pts',(88.6197447734738,52.09283546166,10.9512597453841));
#73027=CARTESIAN_POINT('Ctrl Pts',(88.5907659230636,52.0960084694772,10.9359573979586));
#73028=CARTESIAN_POINT('Ctrl Pts',(88.5773835830163,52.0974496997681,10.929191089982));
#73029=CARTESIAN_POINT('Ctrl Pts',(88.5065152751818,52.1049742345317,10.8949212841805));
#73030=CARTESIAN_POINT('Ctrl Pts',(88.4471346030256,52.1109150771811,10.8715340416709));
#73031=CARTESIAN_POINT('Ctrl Pts',(88.3194247811908,52.1234425699354,10.8320364591742));
#73032=CARTESIAN_POINT('Ctrl Pts',(88.2510227557726,52.1300165013664,10.8169289013674));
#73033=CARTESIAN_POINT('Ctrl Pts',(88.1644602816992,52.1384505340385,10.8051852809591));
#73034=CARTESIAN_POINT('Ctrl Pts',(88.1471428636284,52.1401429410943,10.8031980101817));
#73035=CARTESIAN_POINT('Ctrl Pts',(88.1188314603923,52.1429220431208,10.8005382077332));
#73036=CARTESIAN_POINT('Ctrl Pts',(88.1078594361391,52.1440020627525,10.7996511529323));
#73037=CARTESIAN_POINT('Ctrl Pts',(88.0880861390598,52.1459547162005,10.7983110107467));
#73038=CARTESIAN_POINT('Ctrl Pts',(88.0792889162113,52.1468256953351,10.7978066944111));
#73039=CARTESIAN_POINT('Ctrl Pts',(88.0603975765138,52.1487013382048,10.7969208422943));
#73040=CARTESIAN_POINT('Ctrl Pts',(88.0503028159967,52.1497068400885,10.7965681181659));
#73041=CARTESIAN_POINT('Ctrl Pts',(88.0223631474586,52.15249956369,10.7959254394335));
#73042=CARTESIAN_POINT('Ctrl Pts',(88.0045155495054,52.1542945656077,10.7958911939459));
#73043=CARTESIAN_POINT('Ctrl Pts',(87.9142136112086,52.1634384733453,10.7976211637886));
#73044=CARTESIAN_POINT('Ctrl Pts',(87.8420212708799,52.1709618813644,10.8052088877695));
#73045=CARTESIAN_POINT('Ctrl Pts',(87.6920222529483,52.1870212600025,10.8340896915308));
#73046=CARTESIAN_POINT('Ctrl Pts',(87.6147735663741,52.1955454771024,10.8567207812351));
#73047=CARTESIAN_POINT('Ctrl Pts',(87.5250498300873,52.205504249235,10.8925360407141));
#73048=CARTESIAN_POINT('Ctrl Pts',(87.5100406801162,52.207171636112,10.8988645841986));
#73049=CARTESIAN_POINT('Ctrl Pts',(87.4893461591826,52.2094691105509,10.9080631723716));
#73050=CARTESIAN_POINT('Ctrl Pts',(87.4835553417364,52.2101118295174,10.9106894075234));
#73051=CARTESIAN_POINT('Ctrl Pts',(87.4731759129027,52.2112632429076,10.9154909678409));
#73052=CARTESIAN_POINT('Ctrl Pts',(87.4685801877,52.2117728438773,10.9176505176821));
#73053=CARTESIAN_POINT('Ctrl Pts',(87.459201349554,52.2128122315539,10.9221265412529));
#73054=CARTESIAN_POINT('Ctrl Pts',(87.4544196264119,52.2133418568133,10.9244455633442));
#73055=CARTESIAN_POINT('Ctrl Pts',(87.4419250183301,52.2147253718586,10.9306023265188));
#73056=CARTESIAN_POINT('Ctrl Pts',(87.4342361501195,52.2155763581498,10.9344887591395));
#73057=CARTESIAN_POINT('Ctrl Pts',(87.4171542118176,52.2174674879111,10.9433424114163));
#73058=CARTESIAN_POINT('Ctrl Pts',(87.4077825917064,52.2185053836489,10.9483499365597));
#73059=CARTESIAN_POINT('Ctrl Pts',(87.3790508385487,52.2216922329338,10.9641688441136));
#73060=CARTESIAN_POINT('Ctrl Pts',(87.3599089406063,52.2238222973051,10.9753707125273));
#73061=CARTESIAN_POINT('Ctrl Pts',(87.2741762101353,52.2334431137692,11.0286040078826));
#73062=CARTESIAN_POINT('Ctrl Pts',(87.2112866374828,52.2407364630698,11.0762726531749));
#73063=CARTESIAN_POINT('Ctrl Pts',(87.1101825432368,52.2536335600202,11.1688751991031));
#73064=CARTESIAN_POINT('Ctrl Pts',(87.0699257814049,52.2591677577206,11.2112003035933));
#73065=CARTESIAN_POINT('Ctrl Pts',(87.0228737148715,52.2663259016114,11.2680369056587));
#73066=CARTESIAN_POINT('Ctrl Pts',(87.013240899309,52.2678324615083,11.2801149050149));
#73067=CARTESIAN_POINT('Ctrl Pts',(86.9979841374338,52.2702892673875,11.2999771567767));
#73068=CARTESIAN_POINT('Ctrl Pts',(86.992223699199,52.2712340975289,11.307655111123));
#73069=CARTESIAN_POINT('Ctrl Pts',(86.9812771966769,52.2730638955885,11.3225952839969));
#73070=CARTESIAN_POINT('Ctrl Pts',(86.9760795392654,52.2739483488278,11.3298483491408));
#73071=CARTESIAN_POINT('Ctrl Pts',(86.9641005325154,52.2760243390254,11.3469420593605));
#73072=CARTESIAN_POINT('Ctrl Pts',(86.9573809473203,52.2772181268517,11.3568246452856));
#73073=CARTESIAN_POINT('Ctrl Pts',(86.9357029531295,52.2811692641687,11.3896950240199));
#73074=CARTESIAN_POINT('Ctrl Pts',(86.921350949421,52.2839483983011,11.4130705927901));
#73075=CARTESIAN_POINT('Ctrl Pts',(86.8698084939175,52.2945927301042,11.5034574774526));
#73076=CARTESIAN_POINT('Ctrl Pts',(86.8379586335781,52.3026265416557,11.5733116096807));
#73077=CARTESIAN_POINT('Ctrl Pts',(86.7942977908676,52.316532262508,11.6977704280845));
#73078=CARTESIAN_POINT('Ctrl Pts',(86.7794197358012,52.3223659474705,11.7510898798021));
#73079=CARTESIAN_POINT('Ctrl Pts',(86.7638460209407,52.3302189440268,11.8253158809965));
#73080=CARTESIAN_POINT('Ctrl Pts',(86.7601161365846,52.3323294997758,11.845519574348));
#73081=CARTESIAN_POINT('Ctrl Pts',(86.7556706550292,52.335194929833,11.8733685560581));
#73082=CARTESIAN_POINT('Ctrl Pts',(86.7545319422459,52.3359696994726,11.8809414468146));
#73083=CARTESIAN_POINT('Ctrl Pts',(86.7527503274679,52.3372534279904,11.8935654368501));
#73084=CARTESIAN_POINT('Ctrl Pts',(86.7520691931819,52.3377644162333,11.8986107973947));
#73085=CARTESIAN_POINT('Ctrl Pts',(86.7508275297589,52.3387360334251,11.9082447740154));
#73086=CARTESIAN_POINT('Ctrl Pts',(86.7502616868218,52.3391969666742,11.9128325285457));
#73087=CARTESIAN_POINT('Ctrl Pts',(86.7490890935347,52.3401934796134,11.9227867709244));
#73088=CARTESIAN_POINT('Ctrl Pts',(86.7484914940307,52.3407285578998,11.9281542854903));
#73089=CARTESIAN_POINT('Ctrl Pts',(86.7471097786466,52.3420366875703,11.9413281979347));
#73090=CARTESIAN_POINT('Ctrl Pts',(86.7463637057939,52.3428077976718,11.9491385266829));
#73091=CARTESIAN_POINT('Ctrl Pts',(86.7425923982012,52.3471061903767,11.992899355873));
#73092=CARTESIAN_POINT('Ctrl Pts',(86.7410273681016,52.3505653341981,12.0289633647895));
#73093=CARTESIAN_POINT('Ctrl Pts',(86.7410003558112,52.3539897096227,12.0650493369797));
#73094=CARTESIAN_POINT('Ctrl Pts',(86.7410003571183,52.3539895440703,12.0650475923927));
#73095=CARTESIAN_POINT('Ctrl Pts',(86.7409228830868,52.3637930183023,12.1683562929114));
#73096=CARTESIAN_POINT('Ctrl Pts',(86.753450462588,52.373289701593,12.2712934287686));
#73097=CARTESIAN_POINT('Ctrl Pts',(86.7836604081648,52.3852655112793,12.3931567335967));
#73098=CARTESIAN_POINT('Ctrl Pts',(86.7895734438675,52.3873983575918,12.4145843449426));
#73099=CARTESIAN_POINT('Ctrl Pts',(86.7997968819516,52.3907937032765,12.4481687713019));
#73100=CARTESIAN_POINT('Ctrl Pts',(86.8037356630307,52.3920449995578,12.4604347292532));
#73101=CARTESIAN_POINT('Ctrl Pts',(86.8116063344157,52.3944439929493,12.4837220629807));
#73102=CARTESIAN_POINT('Ctrl Pts',(86.8155053163813,52.3955905420546,12.4947532228195));
#73103=CARTESIAN_POINT('Ctrl Pts',(86.8226331246346,52.3976169116452,12.5140660134888));
#73104=CARTESIAN_POINT('Ctrl Pts',(86.8257975972196,52.3984945500352,12.5223707234641));
#73105=CARTESIAN_POINT('Ctrl Pts',(86.8326000892366,52.4003369262407,12.5396748536933));
#73106=CARTESIAN_POINT('Ctrl Pts',(86.8362546314832,52.4013021676833,12.5486670927795));
#73107=CARTESIAN_POINT('Ctrl Pts',(86.8461903537524,52.4038640355043,12.5723331414491));
#73108=CARTESIAN_POINT('Ctrl Pts',(86.8526454676223,52.4054664308222,12.586931358009));
#73109=CARTESIAN_POINT('Ctrl Pts',(86.8897303060332,52.4143501938584,12.6666990502503));
#73110=CARTESIAN_POINT('Ctrl Pts',(86.925577989438,52.4218077958084,12.7292794558702));
#73111=CARTESIAN_POINT('Ctrl Pts',(86.9962646864695,52.4348574983519,12.831470748392));
#73112=CARTESIAN_POINT('Ctrl Pts',(87.0286317927001,52.4403866717277,12.8725890138752));
#73113=CARTESIAN_POINT('Ctrl Pts',(87.0829805272465,52.4489575970268,12.9334912719663));
#73114=CARTESIAN_POINT('Ctrl Pts',(87.1032752829178,52.4520235824041,12.9547054532518));
#73115=CARTESIAN_POINT('Ctrl Pts',(87.1334325348802,52.4563751143607,12.9841168135056));
#73116=CARTESIAN_POINT('Ctrl Pts',(87.1427110633365,52.4576878722564,12.992896704501));
#73117=CARTESIAN_POINT('Ctrl Pts',(87.1592318409866,52.4599780164577,13.0080637897263));
#73118=CARTESIAN_POINT('Ctrl Pts',(87.1664172467258,52.460958909738,13.0145110299053));
#73119=CARTESIAN_POINT('Ctrl Pts',(87.1759907852523,52.4622452888258,13.022905998961));
#73120=CARTESIAN_POINT('Ctrl Pts',(87.1783131263503,52.4625557707564,13.0249275523496));
#73121=CARTESIAN_POINT('Ctrl Pts',(87.1806428354249,52.4628656574377,13.0269406741515));
#73122=CARTESIAN_POINT('',(86.7429214405097,52.5228781632973,12.0657516006032));
#73123=CARTESIAN_POINT('Ctrl Pts',(87.1806428293121,52.6319631729084,13.0269406688694));
#73124=CARTESIAN_POINT('Ctrl Pts',(87.1768365540776,52.6314403313266,13.0236516334097));
#73125=CARTESIAN_POINT('Ctrl Pts',(87.1730495891386,52.630916799465,13.0203397830469));
#73126=CARTESIAN_POINT('Ctrl Pts',(87.1308342248737,52.6250431480985,12.9829757150102));
#73127=CARTESIAN_POINT('Ctrl Pts',(87.0944880664598,52.6196322981951,12.9466482670422));
#73128=CARTESIAN_POINT('Ctrl Pts',(87.0209437915815,52.6079403163833,12.8636441858104));
#73129=CARTESIAN_POINT('Ctrl Pts',(86.98462435003,52.6016712815446,12.8163348878005));
#73130=CARTESIAN_POINT('Ctrl Pts',(86.9446491424354,52.594238554194,12.7558998571834));
#73131=CARTESIAN_POINT('Ctrl Pts',(86.9377052946905,52.5929250144058,12.7450467481082));
#73132=CARTESIAN_POINT('Ctrl Pts',(86.927652198721,52.5909911353728,12.7287943141345));
#73133=CARTESIAN_POINT('Ctrl Pts',(86.9244159069601,52.5903633933194,12.723475304578));
#73134=CARTESIAN_POINT('Ctrl Pts',(86.9186716855218,52.5892400262526,12.7138761129677));
#73135=CARTESIAN_POINT('Ctrl Pts',(86.9161495931388,52.5887435426158,12.7096048432044));
#73136=CARTESIAN_POINT('Ctrl Pts',(86.9105220974512,52.5876282991705,12.699945623841));
#73137=CARTESIAN_POINT('Ctrl Pts',(86.9074311557749,52.5870104583669,12.6945495048389));
#73138=CARTESIAN_POINT('Ctrl Pts',(86.8980782401371,52.5851237809178,12.6779396266779));
#73139=CARTESIAN_POINT('Ctrl Pts',(86.8919463018392,52.5838626734678,12.6666528260402));
#73140=CARTESIAN_POINT('Ctrl Pts',(86.8692734898747,52.5790971678405,12.6233669873468));
#73141=CARTESIAN_POINT('Ctrl Pts',(86.853923441756,52.575652527841,12.5907589113411));
#73142=CARTESIAN_POINT('Ctrl Pts',(86.8107868934517,52.5650951835039,12.4879920767538));
#73143=CARTESIAN_POINT('Ctrl Pts',(86.787847405811,52.5581052351373,12.4159820225771));
#73144=CARTESIAN_POINT('Ctrl Pts',(86.7652123732216,52.5482976246684,12.3144562090411));
#73145=CARTESIAN_POINT('Ctrl Pts',(86.759935714398,52.5455886786553,12.2863525667403));
#73146=CARTESIAN_POINT('Ctrl Pts',(86.7511806298997,52.5400552375633,12.2291363832637));
#73147=CARTESIAN_POINT('Ctrl Pts',(86.7477530677977,52.5372312723383,12.2000343623896));
#73148=CARTESIAN_POINT('Ctrl Pts',(86.7443272794877,52.5331868979984,12.1586779702516));
#73149=CARTESIAN_POINT('Ctrl Pts',(86.743495099411,52.5319922188989,12.1465002415837));
#73150=CARTESIAN_POINT('Ctrl Pts',(86.7423624342434,52.5299216426699,12.1254734381258));
#73151=CARTESIAN_POINT('Ctrl Pts',(86.7419787213059,52.5290483877225,12.1166295106733));
#73152=CARTESIAN_POINT('Ctrl Pts',(86.7414406201416,52.5274294647725,12.1002825387802));
#73153=CARTESIAN_POINT('Ctrl Pts',(86.741260223201,52.526684646562,12.0927806738322));
#73154=CARTESIAN_POINT('Ctrl Pts',(86.7410469714205,52.525286242958,12.0787335420508));
#73155=CARTESIAN_POINT('Ctrl Pts',(86.7409982154571,52.5246331820998,12.0721887397098));
#73156=CARTESIAN_POINT('Ctrl Pts',(86.7410000498879,52.5239785351125,12.0656440290264));
#73157=CARTESIAN_POINT('Ctrl Pts',(86.7430172856975,52.522823273187,12.0657569666219));
#73158=CARTESIAN_POINT('Ctrl Pts',(86.7426850306966,52.5032787808449,11.8685299954553));
#73159=CARTESIAN_POINT('Ctrl Pts',(86.8788243097244,52.4417295403419,11.2478608714619));
#73160=CARTESIAN_POINT('Ctrl Pts',(87.847476062713,52.3381755516775,10.5738635505768));
#73161=CARTESIAN_POINT('Ctrl Pts',(89.175880239728,52.2121613071944,11.1192871132785));
#73162=CARTESIAN_POINT('Ctrl Pts',(89.4381831401015,52.086147062711,12.5311446533891));
#73163=CARTESIAN_POINT('Ctrl Pts',(88.4036797289598,51.9612621782764,13.5084625635155));
#73164=CARTESIAN_POINT('Ctrl Pts',(87.489495448972,51.8783820420025,13.2952201808301));
#73165=CARTESIAN_POINT('Ctrl Pts',(87.1792973239246,51.8375066538898,13.0285052387874));
#73166=CARTESIAN_POINT('Origin',(88.011,66.41344859951,12.066));
#73167=CARTESIAN_POINT('',(87.1806428354228,50.8732662532979,13.0269406741497));
#73168=CARTESIAN_POINT('',(87.1806428354228,51.0436650276944,13.0269406741497));
#73169=CARTESIAN_POINT('',(87.1806428354228,66.41344859951,13.0269406741497));
#73170=CARTESIAN_POINT('Ctrl Pts',(87.1806428354228,50.8732662532979,13.0269406741497));
#73171=CARTESIAN_POINT('Ctrl Pts',(87.1806475183611,50.8732668464107,13.0269447207173));
#73172=CARTESIAN_POINT('Ctrl Pts',(87.1806522013294,50.8732674395246,13.026948767251));
#73173=CARTESIAN_POINT('Ctrl Pts',(87.2010075773433,50.8758455061281,13.0445375042818));
#73174=CARTESIAN_POINT('Ctrl Pts',(87.2219099279938,50.8784434310677,13.0614697333693));
#73175=CARTESIAN_POINT('Ctrl Pts',(87.2507103336188,50.8819711428578,13.0833226623144));
#73176=CARTESIAN_POINT('Ctrl Pts',(87.2581491587513,50.8828778254497,13.0888398583794));
#73177=CARTESIAN_POINT('Ctrl Pts',(87.2668241774468,50.8839304024496,13.0951280082915));
#73178=CARTESIAN_POINT('Ctrl Pts',(87.2680023887985,50.8840732588447,13.0959789619348));
#73179=CARTESIAN_POINT('Ctrl Pts',(87.2704084295926,50.8843647843292,13.0977104287168));
#73180=CARTESIAN_POINT('Ctrl Pts',(87.2716363743223,50.8845134593419,13.0985907765699));
#73181=CARTESIAN_POINT('Ctrl Pts',(87.2731954855051,50.884702096019,13.0997043399589));
#73182=CARTESIAN_POINT('Ctrl Pts',(87.2735252026008,50.8847419808244,13.0999395955563));
#73183=CARTESIAN_POINT('Ctrl Pts',(87.2808501879476,50.885627891699,13.1051607406175));
#73184=CARTESIAN_POINT('Ctrl Pts',(87.2878955312112,50.8864765664898,13.1100755293309));
#73185=CARTESIAN_POINT('Ctrl Pts',(87.3029034585386,50.8882776862816,13.1203202035269));
#73186=CARTESIAN_POINT('Ctrl Pts',(87.3108775370951,50.8892307410921,13.1256321661932));
#73187=CARTESIAN_POINT('Ctrl Pts',(87.3320137441215,50.8917473486438,13.1393694052747));
#73188=CARTESIAN_POINT('Ctrl Pts',(87.3452721031549,50.8933163782212,13.1476425135847));
#73189=CARTESIAN_POINT('Ctrl Pts',(87.4189506169962,50.9019883013449,13.1917495479482));
#73190=CARTESIAN_POINT('Ctrl Pts',(87.4820978118385,50.9092586344217,13.2227596055896));
#73191=CARTESIAN_POINT('Ctrl Pts',(87.6020667138533,50.9227845607846,13.2697908767773));
#73192=CARTESIAN_POINT('Ctrl Pts',(87.6580793731078,50.928991823158,13.2873868573782));
#73193=CARTESIAN_POINT('Ctrl Pts',(87.7408897635774,50.9379182683555,13.3072265563895));
#73194=CARTESIAN_POINT('Ctrl Pts',(87.7668618326338,50.9406824759937,13.3125952419291));
#73195=CARTESIAN_POINT('Ctrl Pts',(87.8100368650045,50.9452034581481,13.3201185798864));
#73196=CARTESIAN_POINT('Ctrl Pts',(87.8271491852083,50.9469762946206,13.3227412527986));
#73197=CARTESIAN_POINT('Ctrl Pts',(87.8512374353375,50.9494408784373,13.3259304489418));
#73198=CARTESIAN_POINT('Ctrl Pts',(87.8581713872103,50.9501467390286,13.3267903222324));
#73199=CARTESIAN_POINT('Ctrl Pts',(87.8701048177369,50.951355011114,13.3281702759157));
#73200=CARTESIAN_POINT('Ctrl Pts',(87.8751008088186,50.9518588887623,13.3287179702252));
#73201=CARTESIAN_POINT('Ctrl Pts',(87.8857520150819,50.9529288337518,13.3298216757311));
#73202=CARTESIAN_POINT('Ctrl Pts',(87.8914078800005,50.9534944434384,13.3303694140808));
#73203=CARTESIAN_POINT('Ctrl Pts',(87.9069446667003,50.9550417218643,13.3317688726076));
#73204=CARTESIAN_POINT('Ctrl Pts',(87.9168325429424,50.9560192691645,13.3325428787274));
#73205=CARTESIAN_POINT('Ctrl Pts',(87.9894488021941,50.9631529404859,13.33737198038));
#73206=CARTESIAN_POINT('Ctrl Pts',(88.0524047341841,50.9690911195251,13.3368815752058));
#73207=CARTESIAN_POINT('Ctrl Pts',(88.1652082375716,50.9797181419027,13.327606112865));
#73208=CARTESIAN_POINT('Ctrl Pts',(88.2150498953138,50.9844093451062,13.3205093545668));
#73209=CARTESIAN_POINT('Ctrl Pts',(88.3005304078304,50.9926259398401,13.3031080190138));
#73210=CARTESIAN_POINT('Ctrl Pts',(88.3363801705357,50.9961252892169,13.2941658770595));
#73211=CARTESIAN_POINT('Ctrl Pts',(88.3836293596144,51.0008517473405,13.280166348107));
#73212=CARTESIAN_POINT('Ctrl Pts',(88.3954197416399,51.0020408105421,13.2764850269123));
#73213=CARTESIAN_POINT('Ctrl Pts',(88.4244001382436,51.0049898156787,13.2669703617734));
#73214=CARTESIAN_POINT('Ctrl Pts',(88.4415216933512,51.0067552395283,13.2609395284613));
#73215=CARTESIAN_POINT('Ctrl Pts',(88.4680192946969,51.0095279551601,13.2509627304541));
#73216=CARTESIAN_POINT('Ctrl Pts',(88.4774877682093,51.0105269395311,13.2472673091019));
#73217=CARTESIAN_POINT('Ctrl Pts',(88.4950747915169,51.0123985865962,13.2401589076645));
#73218=CARTESIAN_POINT('Ctrl Pts',(88.5032042416846,51.0132702472347,13.2367743244472));
#73219=CARTESIAN_POINT('Ctrl Pts',(88.5213359187787,51.0152295071382,13.2290032366264));
#73220=CARTESIAN_POINT('Ctrl Pts',(88.531317926608,51.0163185771885,13.2245717563011));
#73221=CARTESIAN_POINT('Ctrl Pts',(88.5568085318832,51.0191275643771,13.2128594303851));
#73222=CARTESIAN_POINT('Ctrl Pts',(88.572228573518,51.020853696034,13.2053927862796));
#73223=CARTESIAN_POINT('Ctrl Pts',(88.6667310003779,51.0316065665054,13.1572493886093));
#73224=CARTESIAN_POINT('Ctrl Pts',(88.7414919890587,51.0409057155117,13.1086803954499));
#73225=CARTESIAN_POINT('Ctrl Pts',(88.8492394954175,51.0555262295804,13.0213711142937));
#73226=CARTESIAN_POINT('Ctrl Pts',(88.8860518416663,51.0607804380291,12.9877723897631));
#73227=CARTESIAN_POINT('Ctrl Pts',(88.9330925070017,51.0677922254182,12.9394734709603));
#73228=CARTESIAN_POINT('Ctrl Pts',(88.9451237139666,51.0696144940624,12.9265948367129));
#73229=CARTESIAN_POINT('Ctrl Pts',(88.9654692388157,51.0727419338406,12.9038866299424));
#73230=CARTESIAN_POINT('Ctrl Pts',(88.9739091574118,51.0740537360569,12.8941736128847));
#73231=CARTESIAN_POINT('Ctrl Pts',(88.9862108198781,51.075985670113,12.8795739613433));
#73232=CARTESIAN_POINT('Ctrl Pts',(88.9901861868078,51.0766131818272,12.8747849846119));
#73233=CARTESIAN_POINT('Ctrl Pts',(88.9972672069768,51.0777364408778,12.8661259983265));
#73234=CARTESIAN_POINT('Ctrl Pts',(89.0003855361722,51.0782330441306,12.8622668401978));
#73235=CARTESIAN_POINT('Ctrl Pts',(89.0073646515024,51.0793489533023,12.8535253762663));
#73236=CARTESIAN_POINT('Ctrl Pts',(89.0112122684,51.0799673365591,12.8486328393164));
#73237=CARTESIAN_POINT('Ctrl Pts',(89.0229039848524,51.0818569883998,12.83353886815));
#73238=CARTESIAN_POINT('Ctrl Pts',(89.0306295454953,51.0831204942264,12.8232458157112));
#73239=CARTESIAN_POINT('Ctrl Pts',(89.0726505548739,51.0900890733903,12.765450170921));
#73240=CARTESIAN_POINT('Ctrl Pts',(89.1037892396832,51.0956206146516,12.7157280493234));
#73241=CARTESIAN_POINT('Ctrl Pts',(89.155273356326,51.105885176255,12.6192736327138));
#73242=CARTESIAN_POINT('Ctrl Pts',(89.1764569382815,51.110616051943,12.5731323794142));
#73243=CARTESIAN_POINT('Ctrl Pts',(89.2080211088673,51.1188293148092,12.4918742429685));
#73244=CARTESIAN_POINT('Ctrl Pts',(89.2197483765835,51.1222837897439,12.4573506732537));
#73245=CARTESIAN_POINT('Ctrl Pts',(89.2334063140848,51.1269530411692,12.4106337177286));
#73246=CARTESIAN_POINT('Ctrl Pts',(89.2366685298787,51.1281307225479,12.3988456536996));
#73247=CARTESIAN_POINT('Ctrl Pts',(89.244314561596,51.1310557365436,12.3695784755436));
#73248=CARTESIAN_POINT('Ctrl Pts',(89.2484974042333,51.1328085065896,12.3520503378366));
#73249=CARTESIAN_POINT('Ctrl Pts',(89.2544482866336,51.1355657781011,12.3245326069871));
#73250=CARTESIAN_POINT('Ctrl Pts',(89.2564720872051,51.1365621252465,12.3146001119612));
#73251=CARTESIAN_POINT('Ctrl Pts',(89.2600318300694,51.1384313750803,12.2959936298492));
#73252=CARTESIAN_POINT('Ctrl Pts',(89.2615968513931,51.1393032976045,12.2873257501095));
#73253=CARTESIAN_POINT('Ctrl Pts',(89.2649062760589,51.1412665006684,12.2678393580063));
#73254=CARTESIAN_POINT('Ctrl Pts',(89.2666010411752,51.1423592796885,12.2570133022467));
#73255=CARTESIAN_POINT('Ctrl Pts',(89.2706037459408,51.1451847713726,12.2290835523616));
#73256=CARTESIAN_POINT('Ctrl Pts',(89.272703408528,51.146923824872,12.2119529915864));
#73257=CARTESIAN_POINT('Ctrl Pts',(89.2831549136372,51.157374972638,12.1094186632909));
#73258=CARTESIAN_POINT('Ctrl Pts',(89.2831802528016,51.1663386329533,12.0234094526222));
#73259=CARTESIAN_POINT('Ctrl Pts',(89.2693112502228,51.1808517088892,11.8864221737266));
#73260=CARTESIAN_POINT('Ctrl Pts',(89.2609190017953,51.18633380876,11.8351352372675));
#73261=CARTESIAN_POINT('Ctrl Pts',(89.2454125038135,51.1936130669747,11.7669163114878));
#73262=CARTESIAN_POINT('Ctrl Pts',(89.2410404169332,51.1954790777445,11.749415176521));
#73263=CARTESIAN_POINT('Ctrl Pts',(89.2328538905988,51.1986732227454,11.7193814029891));
#73264=CARTESIAN_POINT('Ctrl Pts',(89.2292157730967,51.2000083488342,11.7068040085793));
#73265=CARTESIAN_POINT('Ctrl Pts',(89.2235495255271,51.2019676738704,11.6882925572965));
#73266=CARTESIAN_POINT('Ctrl Pts',(89.2216711099963,51.2025995475692,11.6823142774983));
#73267=CARTESIAN_POINT('Ctrl Pts',(89.21822618287,51.2037271941518,11.6716276371158));
#73268=CARTESIAN_POINT('Ctrl Pts',(89.2166762577483,51.2042238579118,11.6669143173981));
#73269=CARTESIAN_POINT('Ctrl Pts',(89.2131331788622,51.2053356875237,11.6563488867037));
#73270=CARTESIAN_POINT('Ctrl Pts',(89.2111248720212,51.2059499648591,11.6505020917065));
#73271=CARTESIAN_POINT('Ctrl Pts',(89.2048776855024,51.2078139831363,11.6327378916362));
#73272=CARTESIAN_POINT('Ctrl Pts',(89.2005031851558,51.2090562621806,11.6208683345868));
#73273=CARTESIAN_POINT('Ctrl Pts',(89.170238728609,51.2172624221028,11.5423846448894));
#73274=CARTESIAN_POINT('Ctrl Pts',(89.138935603695,51.2239623865126,11.4779813141137));
#73275=CARTESIAN_POINT('Ctrl Pts',(89.0561090910428,51.2391383734191,11.3387904389401));
#73276=CARTESIAN_POINT('Ctrl Pts',(89.0016608137928,51.2475847792139,11.2661996161526));
#73277=CARTESIAN_POINT('Ctrl Pts',(88.9289867364727,51.2579154583508,11.1882420656301));
#73278=CARTESIAN_POINT('Ctrl Pts',(88.9177986252339,51.2594827739811,11.1766885601194));
#73279=CARTESIAN_POINT('Ctrl Pts',(88.8994931247381,51.2620137124744,11.1584898468565));
#73280=CARTESIAN_POINT('Ctrl Pts',(88.8925131035788,51.2629712866419,11.1517082818468));
#73281=CARTESIAN_POINT('Ctrl Pts',(88.8790165122139,51.2648093353586,11.1388936491756));
#73282=CARTESIAN_POINT('Ctrl Pts',(88.8725132132093,51.2656891720706,11.1328473734218));
#73283=CARTESIAN_POINT('Ctrl Pts',(88.8574813508069,51.2677101567449,11.1191629535415));
#73284=CARTESIAN_POINT('Ctrl Pts',(88.8489119862787,51.2688531567997,11.1115710864687));
#73285=CARTESIAN_POINT('Ctrl Pts',(88.8215674176925,51.2724732657526,11.0879977762989));
#73286=CARTESIAN_POINT('Ctrl Pts',(88.8024302333195,51.2749674462781,11.0724478584596));
#73287=CARTESIAN_POINT('Ctrl Pts',(88.699655813023,51.2881739062547,10.9937922245773));
#73288=CARTESIAN_POINT('Ctrl Pts',(88.6089125115153,51.2992501117441,10.9406700660958));
#73289=CARTESIAN_POINT('Ctrl Pts',(88.4829718369426,51.3136654021562,10.886512684579));
#73290=CARTESIAN_POINT('Ctrl Pts',(88.4527551870671,51.317053687807,10.8748658944421));
#73291=CARTESIAN_POINT('Ctrl Pts',(88.4033453136906,51.3224553898071,10.8579606479839));
#73292=CARTESIAN_POINT('Ctrl Pts',(88.3844167071596,51.3244927569641,10.8519760975121));
#73293=CARTESIAN_POINT('Ctrl Pts',(88.3582891209898,51.3272551801618,10.844384516329));
#73294=CARTESIAN_POINT('Ctrl Pts',(88.3512064085372,51.3279990629208,10.8423931461976));
#73295=CARTESIAN_POINT('Ctrl Pts',(88.3391987044207,51.329251419441,10.8391293971574));
#73296=CARTESIAN_POINT('Ctrl Pts',(88.3342827609187,51.3297616511068,10.8378248793202));
#73297=CARTESIAN_POINT('Ctrl Pts',(88.3240146246647,51.3308220840184,10.8351660060951));
#73298=CARTESIAN_POINT('Ctrl Pts',(88.3186612444582,51.3313719846676,10.8338169621516));
#73299=CARTESIAN_POINT('Ctrl Pts',(88.3041388757967,51.3328561616506,10.8302578958513));
#73300=CARTESIAN_POINT('Ctrl Pts',(88.2949534791662,51.3337867657434,10.8281149529939));
#73301=CARTESIAN_POINT('Ctrl Pts',(88.2471666561997,51.338590432386,10.8175262773889));
#73302=CARTESIAN_POINT('Ctrl Pts',(88.2082046080001,51.3423797516393,10.8107818300825));
#73303=CARTESIAN_POINT('Ctrl Pts',(88.0808269138722,51.3545554784744,10.7948122457321));
#73304=CARTESIAN_POINT('Ctrl Pts',(87.9917505918072,51.3627570528973,10.7930409782929));
#73305=CARTESIAN_POINT('Ctrl Pts',(87.859973992344,51.3752848362197,10.804265242885));
#73306=CARTESIAN_POINT('Ctrl Pts',(87.8169546560851,51.3794351898445,10.8101620399867));
#73307=CARTESIAN_POINT('Ctrl Pts',(87.7606665597119,51.3850056077569,10.8208387800724));
#73308=CARTESIAN_POINT('Ctrl Pts',(87.7470511953186,51.3863638724029,10.8236537170663));
#73309=CARTESIAN_POINT('Ctrl Pts',(87.7244308013906,51.3886404786809,10.8287190329065));
#73310=CARTESIAN_POINT('Ctrl Pts',(87.7153989849389,51.3895548364401,10.8308457077787));
#73311=CARTESIAN_POINT('Ctrl Pts',(87.6976607825607,51.3913617439212,10.835228122518));
#73312=CARTESIAN_POINT('Ctrl Pts',(87.6889534389196,51.3922540480884,10.8374777651735));
#73313=CARTESIAN_POINT('Ctrl Pts',(87.669782373453,51.3942309325549,10.8426486416162));
#73314=CARTESIAN_POINT('Ctrl Pts',(87.6593309045423,51.3953168147763,10.8456120112212));
#73315=CARTESIAN_POINT('Ctrl Pts',(87.6234042117042,51.3990788443186,10.8562983362493));
#73316=CARTESIAN_POINT('Ctrl Pts',(87.5981367770844,51.4017761319917,10.8646872599623));
#73317=CARTESIAN_POINT('Ctrl Pts',(87.4857161967608,51.4140238234804,10.9059769077466));
#73318=CARTESIAN_POINT('Ctrl Pts',(87.402092817642,51.4238437394858,10.947607468878));
#73319=CARTESIAN_POINT('Ctrl Pts',(87.2808228362238,51.4390337497524,11.0256385787474));
#73320=CARTESIAN_POINT('Ctrl Pts',(87.2395569886027,51.4443923953111,11.0558575977986));
#73321=CARTESIAN_POINT('Ctrl Pts',(87.1905837010173,51.4509155773321,11.0964775279904));
#73322=CARTESIAN_POINT('Ctrl Pts',(87.1810658458023,51.4521914975508,11.1046124248178));
#73323=CARTESIAN_POINT('Ctrl Pts',(87.1670485818414,51.4540811362545,11.1169563176296));
#73324=CARTESIAN_POINT('Ctrl Pts',(87.1624574187888,51.454701792407,11.1210590489672));
#73325=CARTESIAN_POINT('Ctrl Pts',(87.154220216904,51.4558182201388,11.1285283866829));
#73326=CARTESIAN_POINT('Ctrl Pts',(87.1505639191276,51.4563147927477,11.1318831035276));
#73327=CARTESIAN_POINT('Ctrl Pts',(87.1423154210495,51.4574374318566,11.139540772407));
#73328=CARTESIAN_POINT('Ctrl Pts',(87.1377354138947,51.4580625198593,11.143856536677));
#73329=CARTESIAN_POINT('Ctrl Pts',(87.1236246156361,51.4599945921281,11.157352636741));
#73330=CARTESIAN_POINT('Ctrl Pts',(87.1142045750657,51.4612933018189,11.1666485003378));
#73331=CARTESIAN_POINT('Ctrl Pts',(87.0463119314727,51.4707365649291,11.2357739931844));
#73332=CARTESIAN_POINT('Ctrl Pts',(86.993721774966,51.4785204051252,11.3011152185336));
#73333=CARTESIAN_POINT('Ctrl Pts',(86.9194934654134,51.4912329536637,11.4146814228274));
#73334=CARTESIAN_POINT('Ctrl Pts',(86.8937529958692,51.4961117558921,11.4598970818801));
#73335=CARTESIAN_POINT('Ctrl Pts',(86.8564776726467,51.5041836066285,11.5358644190922));
#73336=CARTESIAN_POINT('Ctrl Pts',(86.8432351341186,51.507324868133,11.5657097376064));
#73337=CARTESIAN_POINT('Ctrl Pts',(86.8264795623958,51.5117362128425,11.6077739007571));
#73338=CARTESIAN_POINT('Ctrl Pts',(86.821977084653,51.5129733464209,11.6195872940853));
#73339=CARTESIAN_POINT('Ctrl Pts',(86.8145597080186,51.5151049605263,11.6399573931017));
#73340=CARTESIAN_POINT('Ctrl Pts',(86.8115583567113,51.515996517825,11.6484818460083));
#73341=CARTESIAN_POINT('Ctrl Pts',(86.8059887358412,51.517708698356,11.6648565507218));
#73342=CARTESIAN_POINT('Ctrl Pts',(86.8034055612349,51.5185287806601,11.6727012879839));
#73343=CARTESIAN_POINT('Ctrl Pts',(86.7974945408428,51.5204688244557,11.6912596220072));
#73344=CARTESIAN_POINT('Ctrl Pts',(86.7942318473777,51.5215908472242,11.7019930051687));
#73345=CARTESIAN_POINT('Ctrl Pts',(86.7830220936081,51.5256389372007,11.7407059081105));
#73346=CARTESIAN_POINT('Ctrl Pts',(86.7758953303166,51.5285907381942,11.7689106367472));
#73347=CARTESIAN_POINT('Ctrl Pts',(86.750561903591,51.5408647765453,11.8859521652629));
#73348=CARTESIAN_POINT('Ctrl Pts',(86.7409293229408,51.5504299644905,11.9763568610618));
#73349=CARTESIAN_POINT('Ctrl Pts',(86.7410430757661,51.5657096205168,12.1214365257508));
#73350=CARTESIAN_POINT('Ctrl Pts',(86.7445862925543,51.5714147465689,12.1758269348659));
#73351=CARTESIAN_POINT('Ctrl Pts',(86.7528915680399,51.5779873340751,12.2396711533848));
#73352=CARTESIAN_POINT('Ctrl Pts',(86.7542872187237,51.5789953780693,12.2494979665258));
#73353=CARTESIAN_POINT('Ctrl Pts',(86.7566544540706,51.5805655728232,12.2648690801218));
#73354=CARTESIAN_POINT('Ctrl Pts',(86.7575478766861,51.581131733278,12.2704246528713));
#73355=CARTESIAN_POINT('Ctrl Pts',(86.7593121052029,51.5822014180731,12.2809484866138));
#73356=CARTESIAN_POINT('Ctrl Pts',(86.7601755892262,51.5827052854402,12.2859175600669));
#73357=CARTESIAN_POINT('Ctrl Pts',(86.762326406213,51.5839148162359,12.297872174857));
#73358=CARTESIAN_POINT('Ctrl Pts',(86.7636427848273,51.5846188581633,12.3048523304708));
#73359=CARTESIAN_POINT('Ctrl Pts',(86.7685156466526,51.5871035613752,12.3295511570532));
#73360=CARTESIAN_POINT('Ctrl Pts',(86.7723919341085,51.5888677365882,12.3472059042553));
#73361=CARTESIAN_POINT('Ctrl Pts',(86.7802565610388,51.5921033245222,12.3796979041116));
#73362=CARTESIAN_POINT('Ctrl Pts',(86.784139579768,51.5935785587552,12.394556468848));
#73363=CARTESIAN_POINT('Ctrl Pts',(86.8062828961033,51.6014032959769,12.4734132303857));
#73364=CARTESIAN_POINT('Ctrl Pts',(86.8292843776834,51.6075993535272,12.5359773289825));
#73365=CARTESIAN_POINT('Ctrl Pts',(86.8872910225581,51.6206197714087,12.6621608049326));
#73366=CARTESIAN_POINT('Ctrl Pts',(86.9230474371549,51.6274307846633,12.7251554959279));
#73367=CARTESIAN_POINT('Ctrl Pts',(86.9730248299818,51.6359912189574,12.7979589349563));
#73368=CARTESIAN_POINT('Ctrl Pts',(86.982334295024,51.6375516561407,12.8109853342826));
#73369=CARTESIAN_POINT('Ctrl Pts',(86.9976852581056,51.6400742032395,12.8316289256802));
#73370=CARTESIAN_POINT('Ctrl Pts',(87.0035725913524,51.6410303375728,12.8393591799687));
#73371=CARTESIAN_POINT('Ctrl Pts',(87.0150114201699,51.6428674009647,12.8540264448457));
#73372=CARTESIAN_POINT('Ctrl Pts',(87.0205481762864,51.6437477058152,12.8609742785927));
#73373=CARTESIAN_POINT('Ctrl Pts',(87.0335302257596,51.6457919685805,12.8769187408945));
#73374=CARTESIAN_POINT('Ctrl Pts',(87.0410274803757,51.646957968272,12.885871728769));
#73375=CARTESIAN_POINT('Ctrl Pts',(87.0657872669771,51.650763473949,12.9146241044349));
#73376=CARTESIAN_POINT('Ctrl Pts',(87.0835394131259,51.6534227952322,12.933989965764));
#73377=CARTESIAN_POINT('Ctrl Pts',(87.1270707845374,51.659792555792,12.9786176184718));
#73378=CARTESIAN_POINT('Ctrl Pts',(87.1533498826672,51.6635217203355,13.0033565971518));
#73379=CARTESIAN_POINT('Ctrl Pts',(87.1806428357067,51.6672833294972,13.026940674395));
#73380=CARTESIAN_POINT('',(86.7410004204394,51.72907359951,12.0649665997861));
#73381=CARTESIAN_POINT('Ctrl Pts',(87.1792973239246,51.8375066538898,13.0285052387874));
#73382=CARTESIAN_POINT('Ctrl Pts',(87.1707267540613,51.8363772938414,13.0211360806275));
#73383=CARTESIAN_POINT('Ctrl Pts',(86.8998704527144,51.8002331995894,12.7813463937796));
#73384=CARTESIAN_POINT('Ctrl Pts',(86.7432354015658,51.7640891053375,12.4162822252844));
#73385=CARTESIAN_POINT('Ctrl Pts',(86.7401346566022,51.7290743711339,12.0649736370867));
#73386=CARTESIAN_POINT('Ctrl Pts',(86.7410004204394,51.72907359951,12.0649665997861));
#73387=CARTESIAN_POINT('Ctrl Pts',(86.7410574454711,51.7220838427605,11.9948855554347));
#73388=CARTESIAN_POINT('Ctrl Pts',(86.7469171288941,51.715094086011,11.9250345638552));
#73389=CARTESIAN_POINT('Ctrl Pts',(86.7584556185441,51.7081043292614,11.8561606031191));
#73390=CARTESIAN_POINT('Ctrl Pts',(86.7666237113341,51.7031562829017,11.807404750389));
#73391=CARTESIAN_POINT('Ctrl Pts',(86.7776608791493,51.698208236542,11.759018762359));
#73392=CARTESIAN_POINT('Ctrl Pts',(86.7915187869455,51.6932601901823,11.7113655811865));
#73393=CARTESIAN_POINT('Ctrl Pts',(86.805351196489,51.6883212481217,11.663800080844));
#73394=CARTESIAN_POINT('Ctrl Pts',(86.8219939005199,51.683382306061,11.6169652350239));
#73395=CARTESIAN_POINT('Ctrl Pts',(86.8413475075088,51.6784433640004,11.5712141404515));
#73396=CARTESIAN_POINT('Ctrl Pts',(86.8606814637615,51.6735094367076,11.5255094993744));
#73397=CARTESIAN_POINT('Ctrl Pts',(86.8827206614617,51.6685755094149,11.4808869333989));
#73398=CARTESIAN_POINT('Ctrl Pts',(86.9073164919653,51.6636415821222,11.4376826326671));
#73399=CARTESIAN_POINT('Ctrl Pts',(86.931897815201,51.6587105649896,11.3945038149685));
#73400=CARTESIAN_POINT('Ctrl Pts',(86.9590325132943,51.6537795478569,11.3527420806323));
#73401=CARTESIAN_POINT('Ctrl Pts',(86.9885257684931,51.6488485307243,11.3127095872743));
#73402=CARTESIAN_POINT('Ctrl Pts',(87.0180141771654,51.643918323889,11.2726836723202));
#73403=CARTESIAN_POINT('Ctrl Pts',(87.0498600478677,51.6389881170537,11.234386874561));
#73404=CARTESIAN_POINT('Ctrl Pts',(87.0838264121602,51.6340579102184,11.1981007327965));
#73405=CARTESIAN_POINT('Ctrl Pts',(87.1178259624633,51.6291228864444,11.1617791385394));
#73406=CARTESIAN_POINT('Ctrl Pts',(87.1539497669398,51.6241878626704,11.1274725226636));
#73407=CARTESIAN_POINT('Ctrl Pts',(87.1919231183123,51.6192528388963,11.0954264263413));
#73408=CARTESIAN_POINT('Ctrl Pts',(87.2299169057445,51.6143151592482,11.0633630838208));
#73409=CARTESIAN_POINT('Ctrl Pts',(87.2697617828868,51.6093774796001,11.0335630118872));
#73410=CARTESIAN_POINT('Ctrl Pts',(87.3111518062313,51.6044397999519,11.006229975099));
#73411=CARTESIAN_POINT('Ctrl Pts',(87.3526191203687,51.5994928997925,10.9788458972164));
#73412=CARTESIAN_POINT('Ctrl Pts',(87.3956368650549,51.5945459996332,10.9539383239309));
#73413=CARTESIAN_POINT('Ctrl Pts',(87.4398735480189,51.5895990994738,10.9316655802421));
#73414=CARTESIAN_POINT('Ctrl Pts',(87.462256177663,51.5870960945753,10.9203961418543));
#73415=CARTESIAN_POINT('Ctrl Pts',(87.4849505357424,51.5845930896767,10.9098004835379));
#73416=CARTESIAN_POINT('Ctrl Pts',(87.5079119951131,51.5820900847782,10.8998943189664));
#73417=CARTESIAN_POINT('Ctrl Pts',(87.5533031872588,51.5771420379465,10.8803113903627));
#73418=CARTESIAN_POINT('Ctrl Pts',(87.5999398310792,51.5721939911148,10.8633394471891));
#73419=CARTESIAN_POINT('Ctrl Pts',(87.6474907942364,51.5672459442831,10.8491347415079));
#73420=CARTESIAN_POINT('Ctrl Pts',(87.6949542647047,51.5623070017449,10.8349561721615));
#73421=CARTESIAN_POINT('Ctrl Pts',(87.7433281971118,51.5573680592066,10.8235348974083));
#73422=CARTESIAN_POINT('Ctrl Pts',(87.7922620375085,51.5524291166684,10.814978935523));
#73423=CARTESIAN_POINT('Ctrl Pts',(87.8411461928357,51.547495188895,10.8064316609503));
#73424=CARTESIAN_POINT('Ctrl Pts',(87.890588593523,51.5425612611216,10.8007440337539));
#73425=CARTESIAN_POINT('Ctrl Pts',(87.9402261939047,51.5376273333482,10.7979735537574));
#73426=CARTESIAN_POINT('Ctrl Pts',(87.989834516748,51.5326963157328,10.7952047078614));
#73427=CARTESIAN_POINT('Ctrl Pts',(88.0396372651039,51.5277652981174,10.7953496310471));
#73428=CARTESIAN_POINT('Ctrl Pts',(88.0892665197824,51.522834280502,10.7984139666748));
#73429=CARTESIAN_POINT('Ctrl Pts',(88.1388876190668,51.5179040731827,10.8014777987514));
#73430=CARTESIAN_POINT('Ctrl Pts',(88.1883347346994,51.5129738658635,10.8074600561353));
#73431=CARTESIAN_POINT('Ctrl Pts',(88.2372428085287,51.5080436585442,10.816314362894));
#73432=CARTESIAN_POINT('Ctrl Pts',(88.2861986667775,51.5031086342882,10.8251773205333));
#73433=CARTESIAN_POINT('Ctrl Pts',(88.3346138916304,51.4981736100322,10.8369178313481));
#73434=CARTESIAN_POINT('Ctrl Pts',(88.3821331978085,51.4932385857763,10.8514382891411));
#73435=CARTESIAN_POINT('Ctrl Pts',(88.4296780773711,51.4883009056467,10.8659665613843));
#73436=CARTESIAN_POINT('Ctrl Pts',(88.4763255638781,51.4833632255171,10.8832775689133));
#73437=CARTESIAN_POINT('Ctrl Pts',(88.5217385269754,51.4784255453875,10.903224803729));
#73438=CARTESIAN_POINT('Ctrl Pts',(88.567236293145,51.4734786447531,10.9232092875301));
#73439=CARTESIAN_POINT('Ctrl Pts',(88.6114944466437,51.4685317441187,10.9458395743221));
#73440=CARTESIAN_POINT('Ctrl Pts',(88.6542001742352,51.4635848434842,10.9709230456886));
#73441=CARTESIAN_POINT('Ctrl Pts',(88.6758081444493,51.4610818424212,10.9836146196935));
#73442=CARTESIAN_POINT('Ctrl Pts',(88.6970191400709,51.4585788413581,10.9969335388941));
#73443=CARTESIAN_POINT('Ctrl Pts',(88.7177957541759,51.456075840295,11.0108508342993));
#73444=CARTESIAN_POINT('Ctrl Pts',(88.7588678986207,51.4511277953109,11.0383631692868));
#73445=CARTESIAN_POINT('Ctrl Pts',(88.7984220319169,51.4461797503268,11.0683380283455));
#73446=CARTESIAN_POINT('Ctrl Pts',(88.8361472777453,51.4412317053428,11.1005819713567));
#73447=CARTESIAN_POINT('Ctrl Pts',(88.8738031099641,51.4362927646509,11.132766586233));
#73448=CARTESIAN_POINT('Ctrl Pts',(88.9096363157023,51.4313538239591,11.1672116513664));
#73449=CARTESIAN_POINT('Ctrl Pts',(88.9433660065904,51.4264148832673,11.2036812481718));
#73450=CARTESIAN_POINT('Ctrl Pts',(88.9770614499743,51.421480957338,11.2401138155043));
#73451=CARTESIAN_POINT('Ctrl Pts',(89.008657236395,51.4165470314088,11.2785664447452));
#73452=CARTESIAN_POINT('Ctrl Pts',(89.0379081435998,51.4116131054796,11.3187653215968));
#73453=CARTESIAN_POINT('Ctrl Pts',(89.0671417978915,51.4066820897027,11.3589404881502));
#73454=CARTESIAN_POINT('Ctrl Pts',(89.0940329910739,51.4017510739257,11.4008594196246));
#73455=CARTESIAN_POINT('Ctrl Pts',(89.1183774232072,51.3968200581488,11.4442160804822));
#73456=CARTESIAN_POINT('Ctrl Pts',(89.1427178549522,51.391889852659,11.4875656167752));
#73457=CARTESIAN_POINT('Ctrl Pts',(89.1645120891895,51.3869596471691,11.5323519353977));
#73458=CARTESIAN_POINT('Ctrl Pts',(89.1836010803103,51.3820294416793,11.5782431892274));
#73459=CARTESIAN_POINT('Ctrl Pts',(89.2027087219714,51.3770944192247,11.6241792802448));
#73460=CARTESIAN_POINT('Ctrl Pts',(89.2191056333498,51.3721593967702,11.6712219546057));
#73461=CARTESIAN_POINT('Ctrl Pts',(89.2326811092605,51.3672243743156,11.7190197883509));
#73462=CARTESIAN_POINT('Ctrl Pts',(89.2462638911013,51.3622866959741,11.7668433455137));
#73463=CARTESIAN_POINT('Ctrl Pts',(89.2570220952417,51.3573490176326,11.8154223357806));
#73464=CARTESIAN_POINT('Ctrl Pts',(89.264895947147,51.3524113392911,11.8643940632613));
#73465=CARTESIAN_POINT('Ctrl Pts',(89.272784502565,51.3474644404032,11.91345723981));
#73466=CARTESIAN_POINT('Ctrl Pts',(89.2777779005425,51.3425175415153,11.9629140718333));
#73467=CARTESIAN_POINT('Ctrl Pts',(89.2798682944581,51.3375706426275,12.0123972825424));
#73468=CARTESIAN_POINT('Ctrl Pts',(89.2809259850863,51.3350676270222,12.0374346345097));
#73469=CARTESIAN_POINT('Ctrl Pts',(89.2812413025968,51.332564611417,12.06247875113));
#73470=CARTESIAN_POINT('Ctrl Pts',(89.2808182950789,51.3300615958117,12.087482492471));
#73471=CARTESIAN_POINT('Ctrl Pts',(89.279982079308,51.325113548707,12.136910746011));
#73472=CARTESIAN_POINT('Ctrl Pts',(89.2762536753466,51.3201655016022,12.1863993558836));
#73473=CARTESIAN_POINT('Ctrl Pts',(89.2696269775012,51.3152174544974,12.235582226386));
#73474=CARTESIAN_POINT('Ctrl Pts',(89.2630124726603,51.31027851171,12.2846746012953));
#73475=CARTESIAN_POINT('Ctrl Pts',(89.2535103232701,51.3053395689225,12.3334618139219));
#73476=CARTESIAN_POINT('Ctrl Pts',(89.2411663761222,51.300400626135,12.3815799218239));
#73477=CARTESIAN_POINT('Ctrl Pts',(89.2288349624615,51.2954666981273,12.4296491727693));
#73478=CARTESIAN_POINT('Ctrl Pts',(89.2136675987204,51.2905327701195,12.4770501356944));
#73479=CARTESIAN_POINT('Ctrl Pts',(89.1957613139366,51.2855988421118,12.5234282774371));
#73480=CARTESIAN_POINT('Ctrl Pts',(89.1778655907964,51.2806678242772,12.5697790640134));
#73481=CARTESIAN_POINT('Ctrl Pts',(89.1572343439754,51.2757368064426,12.6151077143118));
#73482=CARTESIAN_POINT('Ctrl Pts',(89.1340138684682,51.270805788608,12.659076598112));
#73483=CARTESIAN_POINT('Ctrl Pts',(89.1107972087694,51.265875581085,12.7030382565289));
#73484=CARTESIAN_POINT('Ctrl Pts',(89.0849924217139,51.2609453735619,12.7456401082241));
#73485=CARTESIAN_POINT('Ctrl Pts',(89.0567920330508,51.2560151660388,12.7865685419219));
#73486=CARTESIAN_POINT('Ctrl Pts',(89.0285640920397,51.2510801416037,12.8275369635243));
#73487=CARTESIAN_POINT('Ctrl Pts',(88.9979361886039,51.2461451171685,12.8668282512264));
#73488=CARTESIAN_POINT('Ctrl Pts',(88.965143515197,51.2412100927333,12.9041587871086));
#73489=CARTESIAN_POINT('Ctrl Pts',(88.9323331939043,51.2362724124382,12.9415094129977));
#73490=CARTESIAN_POINT('Ctrl Pts',(88.897356168362,51.2313347321431,12.9768967956966));
#73491=CARTESIAN_POINT('Ctrl Pts',(88.860484725547,51.226397051848,13.010073991307));
#73492=CARTESIAN_POINT('Ctrl Pts',(88.8235444300621,51.221450151071,13.0433131410564));
#73493=CARTESIAN_POINT('Ctrl Pts',(88.7847030851708,51.216503250294,13.074333524153));
#73494=CARTESIAN_POINT('Ctrl Pts',(88.744264992011,51.211556349517,13.1029293377521));
#73495=CARTESIAN_POINT('Ctrl Pts',(88.7238043991424,51.2090533501208,13.1173980541054));
#73496=CARTESIAN_POINT('Ctrl Pts',(88.7029354661896,51.2065503507247,13.1312467641965));
#73497=CARTESIAN_POINT('Ctrl Pts',(88.6816999912418,51.2040473513286,13.1444533006803));
#73498=CARTESIAN_POINT('Ctrl Pts',(88.6397206804174,51.1990993014309,13.1705606188038));
#73499=CARTESIAN_POINT('Ctrl Pts',(88.5961219425973,51.1941512515332,13.1942708819615));
#73500=CARTESIAN_POINT('Ctrl Pts',(88.5512080313302,51.1892032016355,13.2153803908569));
#73501=CARTESIAN_POINT('Ctrl Pts',(88.5063767603522,51.1842642560055,13.2364510588705));
#73502=CARTESIAN_POINT('Ctrl Pts',(88.4602356072625,51.1793253103755,13.2549302323215));
#73503=CARTESIAN_POINT('Ctrl Pts',(88.4131151955272,51.1743863647455,13.2706590262502));
#73504=CARTESIAN_POINT('Ctrl Pts',(88.3660426274367,51.1694524338672,13.2863718499698));
#73505=CARTESIAN_POINT('Ctrl Pts',(88.3179932863306,51.1645185029888,13.2993396498775));
#73506=CARTESIAN_POINT('Ctrl Pts',(88.2693176518826,51.1595845721104,13.3094516439033));
#73507=CARTESIAN_POINT('Ctrl Pts',(88.2206707274901,51.1546535513827,13.3195576736327));
#73508=CARTESIAN_POINT('Ctrl Pts',(88.1713987770709,51.149722530655,13.3268111231438));
#73509=CARTESIAN_POINT('Ctrl Pts',(88.1218648015373,51.1447915099273,13.331151767884));
#73510=CARTESIAN_POINT('Ctrl Pts',(88.0723389657214,51.1398612994943,13.3354916993437));
#73511=CARTESIAN_POINT('Ctrl Pts',(88.0225517359407,51.1349310890612,13.3369197294466));
#73512=CARTESIAN_POINT('Ctrl Pts',(87.9728710097596,51.1300008786282,13.3354275009244));
#73513=CARTESIAN_POINT('Ctrl Pts',(87.9231417445166,51.1250658512811,13.3339338144652));
#73514=CARTESIAN_POINT('Ctrl Pts',(87.8735197393815,51.120130823934,13.3295141902602));
#73515=CARTESIAN_POINT('Ctrl Pts',(87.8243708362133,51.1151957965869,13.3222123846007));
#73516=CARTESIAN_POINT('Ctrl Pts',(87.7751954827628,51.1102581133745,13.3149066493557));
#73517=CARTESIAN_POINT('Ctrl Pts',(87.7264942751833,51.105320430162,13.3047157563041));
#73518=CARTESIAN_POINT('Ctrl Pts',(87.6786223647281,51.1003827469496,13.2917345175735));
#73519=CARTESIAN_POINT('Ctrl Pts',(87.6306610599554,51.0954358432817,13.2787290381353));
#73520=CARTESIAN_POINT('Ctrl Pts',(87.5835326629146,51.0904889396138,13.2629229877022));
#73521=CARTESIAN_POINT('Ctrl Pts',(87.5375751258267,51.0855420359458,13.2444603890305));
#73522=CARTESIAN_POINT('Ctrl Pts',(87.5143220695857,51.083039059579,13.2351188996368));
#73523=CARTESIAN_POINT('Ctrl Pts',(87.4913684052438,51.0805360832122,13.2250980770676));
#73524=CARTESIAN_POINT('Ctrl Pts',(87.4687554261298,51.0780331068453,13.2144210125683));
#73525=CARTESIAN_POINT('Ctrl Pts',(87.4240553196919,51.0730853593838,13.1933151725478));
#73526=CARTESIAN_POINT('Ctrl Pts',(87.3804905119902,51.0681376119222,13.1695489817321));
#73527=CARTESIAN_POINT('Ctrl Pts',(87.3383971025424,51.0631898644607,13.1432675351702));
#73528=CARTESIAN_POINT('Ctrl Pts',(87.2963761237482,51.0582506306497,13.1170313114205));
#73529=CARTESIAN_POINT('Ctrl Pts',(87.2558219855198,51.0533113968388,13.0882886988727));
#73530=CARTESIAN_POINT('Ctrl Pts',(87.217047557413,51.0483721630279,13.0572313145326));
#73531=CARTESIAN_POINT('Ctrl Pts',(87.204730094991,51.0468031179167,13.047365323383));
#73532=CARTESIAN_POINT('Ctrl Pts',(87.1925920371449,51.0452340728055,13.0372660829162));
#73533=CARTESIAN_POINT('Ctrl Pts',(87.1806428354228,51.0436650276944,13.0269406741497));
#73534=CARTESIAN_POINT('Origin',(88.011,66.41344859951,12.066));
#73535=CARTESIAN_POINT('',(87.1806428554372,50.081424866233,13.0269406914443));
#73536=CARTESIAN_POINT('',(87.1806428354216,50.251127131729,13.0269406741487));
#73537=CARTESIAN_POINT('',(87.1806428354228,66.41344859951,13.0269406741497));
#73538=CARTESIAN_POINT('',(86.7410003813397,50.764592782682,12.066337079236));
#73539=CARTESIAN_POINT('Ctrl Pts',(87.1806428554372,50.081424866233,13.0269406914443));
#73540=CARTESIAN_POINT('Ctrl Pts',(87.2137718936792,50.0856223393657,13.0555677792986));
#73541=CARTESIAN_POINT('Ctrl Pts',(87.2483726174281,50.0897447031932,13.0824741104664));
#73542=CARTESIAN_POINT('Ctrl Pts',(87.3456350912355,50.1008674491368,13.1503343910258));
#73543=CARTESIAN_POINT('Ctrl Pts',(87.4106144382412,50.1078244608523,13.1876182254033));
#73544=CARTESIAN_POINT('Ctrl Pts',(87.4983872052244,50.1170475336888,13.2281567654651));
#73545=CARTESIAN_POINT('Ctrl Pts',(87.5185150137556,50.1191506355758,13.2368281867314));
#73546=CARTESIAN_POINT('Ctrl Pts',(87.5552212134029,50.1229749750837,13.2515279314804));
#73547=CARTESIAN_POINT('Ctrl Pts',(87.5717202782133,50.1246900545637,13.2577399177896));
#73548=CARTESIAN_POINT('Ctrl Pts',(87.5977901198249,50.1273977183724,13.2669404535801));
#73549=CARTESIAN_POINT('Ctrl Pts',(87.6072766813256,50.1283825320622,13.270162715654));
#73550=CARTESIAN_POINT('Ctrl Pts',(87.6251287290019,50.1302355876166,13.275991787139));
#73551=CARTESIAN_POINT('Ctrl Pts',(87.6334850659694,50.1311029029523,13.2786249327349));
#73552=CARTESIAN_POINT('Ctrl Pts',(87.6523647345522,50.1330627636406,13.2843600048799));
#73553=CARTESIAN_POINT('Ctrl Pts',(87.6629021951891,50.1341568571783,13.2874124012293));
#73554=CARTESIAN_POINT('Ctrl Pts',(87.6902678589796,50.1369997060255,13.2949565643126));
#73555=CARTESIAN_POINT('Ctrl Pts',(87.7071505878643,50.1387550291535,13.2992391497411));
#73556=CARTESIAN_POINT('Ctrl Pts',(87.8012166371657,50.1485491745357,13.3210518959149));
#73557=CARTESIAN_POINT('Ctrl Pts',(87.8798028110497,50.1567998306994,13.3316800951234));
#73558=CARTESIAN_POINT('Ctrl Pts',(88.037212816016,50.1734006869207,13.3381494395508));
#73559=CARTESIAN_POINT('Ctrl Pts',(88.1157153056916,50.1817133060103,13.3341044272359));
#73560=CARTESIAN_POINT('Ctrl Pts',(88.2054129762427,50.1910027028717,13.3210904968183));
#73561=CARTESIAN_POINT('Ctrl Pts',(88.2174502242791,50.1922446102772,13.3191667508069));
#73562=CARTESIAN_POINT('Ctrl Pts',(88.2354356132192,50.1940914731074,13.3160261870327));
#73563=CARTESIAN_POINT('Ctrl Pts',(88.2414051997936,50.194703023341,13.3149396551745));
#73564=CARTESIAN_POINT('Ctrl Pts',(88.2517411489544,50.1957591244495,13.3129817636831));
#73565=CARTESIAN_POINT('Ctrl Pts',(88.2561108748048,50.1962047344619,13.3121302022032));
#73566=CARTESIAN_POINT('Ctrl Pts',(88.2664365600203,50.197255703035,13.3100615396305));
#73567=CARTESIAN_POINT('Ctrl Pts',(88.272388399797,50.1978599361106,13.3088246298879));
#73568=CARTESIAN_POINT('Ctrl Pts',(88.2901766777976,50.1996618109895,13.3049944308104));
#73569=CARTESIAN_POINT('Ctrl Pts',(88.3019856901424,50.2008526981427,13.3022743160909));
#73570=CARTESIAN_POINT('Ctrl Pts',(88.3223155981013,50.2028967355451,13.2972840055971));
#73571=CARTESIAN_POINT('Ctrl Pts',(88.3308546986669,50.2037533971276,13.2950934418673));
#73572=CARTESIAN_POINT('Ctrl Pts',(88.3543248069187,50.2061046294642,13.288811402005));
#73573=CARTESIAN_POINT('Ctrl Pts',(88.369205431299,50.2075916242958,13.2845354219099));
#73574=CARTESIAN_POINT('Ctrl Pts',(88.4485676820369,50.2155215360091,13.2601509023413));
#73575=CARTESIAN_POINT('Ctrl Pts',(88.5114509015288,50.2218070896741,13.2351930726608));
#73576=CARTESIAN_POINT('Ctrl Pts',(88.6361172212039,50.2348375539543,13.173803030499));
#73577=CARTESIAN_POINT('Ctrl Pts',(88.697393610511,50.2415669420926,13.1369155606738));
#73578=CARTESIAN_POINT('Ctrl Pts',(88.7681344113431,50.2500313385099,13.0857552260132));
#73579=CARTESIAN_POINT('Ctrl Pts',(88.7808519435079,50.2515825183522,13.0761886797807));
#73580=CARTESIAN_POINT('Ctrl Pts',(88.801032685155,50.254094886571,13.0604056514914));
#73581=CARTESIAN_POINT('Ctrl Pts',(88.8086105592416,50.2550502122455,13.0543378097216));
#73582=CARTESIAN_POINT('Ctrl Pts',(88.8230076339551,50.2568889399281,13.0425362090783));
#73583=CARTESIAN_POINT('Ctrl Pts',(88.829837552629,50.2577717407301,13.036816366452));
#73584=CARTESIAN_POINT('Ctrl Pts',(88.8455418105376,50.259826715194,13.0233809287976));
#73585=CARTESIAN_POINT('Ctrl Pts',(88.8543701089196,50.2610009800321,13.015613138003));
#73586=CARTESIAN_POINT('Ctrl Pts',(88.8828804560114,50.2648575740096,12.9898164663151));
#73587=CARTESIAN_POINT('Ctrl Pts',(88.9021005560537,50.267560399581,12.9712910691408));
#73588=CARTESIAN_POINT('Ctrl Pts',(88.9475185412699,50.2742130459336,12.9246663443893));
#73589=CARTESIAN_POINT('Ctrl Pts',(88.9730511129631,50.2781863677068,12.8959589471802));
#73590=CARTESIAN_POINT('Ctrl Pts',(89.0275875235413,50.2872232905143,12.8287383279579));
#73591=CARTESIAN_POINT('Ctrl Pts',(89.0557794851644,50.2923008789926,12.7896402722075));
#73592=CARTESIAN_POINT('Ctrl Pts',(89.1150213422399,50.3039088817162,12.6967770470786));
#73593=CARTESIAN_POINT('Ctrl Pts',(89.1444953983897,50.3104250348099,12.6421365601638));
#73594=CARTESIAN_POINT('Ctrl Pts',(89.1739587002637,50.3177777033157,12.5764187309047));
#73595=CARTESIAN_POINT('Ctrl Pts',(89.1779462390541,50.3187945622113,12.567235191552));
#73596=CARTESIAN_POINT('Ctrl Pts',(89.1840160766264,50.320376443516,12.5527907890431));
#73597=CARTESIAN_POINT('Ctrl Pts',(89.186172396088,50.3209455401553,12.5475618676405));
#73598=CARTESIAN_POINT('Ctrl Pts',(89.1901873145122,50.3220186595176,12.5376383853029));
#73599=CARTESIAN_POINT('Ctrl Pts',(89.1920528796724,50.3225230402024,12.5329470918492));
#73600=CARTESIAN_POINT('Ctrl Pts',(89.1964714553114,50.3237319166861,12.5216398916832));
#73601=CARTESIAN_POINT('Ctrl Pts',(89.1989971312686,50.3244348074499,12.5150134819995));
#73602=CARTESIAN_POINT('Ctrl Pts',(89.2077239958939,50.3269076760321,12.4915282971825));
#73603=CARTESIAN_POINT('Ctrl Pts',(89.2136233642303,50.3286614086111,12.4745582167289));
#73604=CARTESIAN_POINT('Ctrl Pts',(89.2238518716219,50.3318736059311,12.4429905968366));
#73605=CARTESIAN_POINT('Ctrl Pts',(89.2282822533412,50.3333359160257,12.4284300529639));
#73606=CARTESIAN_POINT('Ctrl Pts',(89.2503729914404,50.3410440870511,12.3508472103654));
#73607=CARTESIAN_POINT('Ctrl Pts',(89.2634051054318,50.3471410737372,12.2866046673119));
#73608=CARTESIAN_POINT('Ctrl Pts',(89.2804878682751,50.3602086205882,12.1482610693548));
#73609=CARTESIAN_POINT('Ctrl Pts',(89.2831223930948,50.3671683498128,12.0742453011175));
#73610=CARTESIAN_POINT('Ctrl Pts',(89.2784875672266,50.3758726795263,11.9845958574865));
#73611=CARTESIAN_POINT('Ctrl Pts',(89.2773726110597,50.3774182246551,11.9687800233279));
#73612=CARTESIAN_POINT('Ctrl Pts',(89.2750999486658,50.3799229114105,11.9433412818497));
#73613=CARTESIAN_POINT('Ctrl Pts',(89.2741276050075,50.3808762400798,11.933703054076));
#73614=CARTESIAN_POINT('Ctrl Pts',(89.2720506654689,50.3827120398874,11.9152339159228));
#73615=CARTESIAN_POINT('Ctrl Pts',(89.2709633065944,50.3835939179016,11.9064016016141));
#73616=CARTESIAN_POINT('Ctrl Pts',(89.2682238289021,50.3856480307401,11.8859263375));
#73617=CARTESIAN_POINT('Ctrl Pts',(89.2665026666512,50.3868223663914,11.8742936881538));
#73618=CARTESIAN_POINT('Ctrl Pts',(89.2603393668592,50.390684237341,11.8362909932978));
#73619=CARTESIAN_POINT('Ctrl Pts',(89.255226247977,50.3933924052873,11.810039356906));
#73620=CARTESIAN_POINT('Ctrl Pts',(89.240741393767,50.4000599490987,11.7464415016833));
#73621=CARTESIAN_POINT('Ctrl Pts',(89.2304931157282,50.4040430247816,11.7093245290532));
#73622=CARTESIAN_POINT('Ctrl Pts',(89.2035935531212,50.4131144433267,11.6267257177769));
#73623=CARTESIAN_POINT('Ctrl Pts',(89.1859939151048,50.4182171604065,11.5816137574962));
#73624=CARTESIAN_POINT('Ctrl Pts',(89.1399589598822,50.4298819883382,11.4809967120988));
#73625=CARTESIAN_POINT('Ctrl Pts',(89.1099196617483,50.4364297026322,11.4263476385792));
#73626=CARTESIAN_POINT('Ctrl Pts',(89.0705327381305,50.4438116426284,11.3657210545662));
#73627=CARTESIAN_POINT('Ctrl Pts',(89.0649793304309,50.444828641422,11.3573902213326));
#73628=CARTESIAN_POINT('Ctrl Pts',(89.0561409434015,50.4464096525536,11.3444653296272));
#73629=CARTESIAN_POINT('Ctrl Pts',(89.0529230629831,50.4469777618668,11.3398263241406));
#73630=CARTESIAN_POINT('Ctrl Pts',(89.0467769061642,50.4480485729273,11.3310907859019));
#73631=CARTESIAN_POINT('Ctrl Pts',(89.0438551719068,50.4485516360892,11.3269901569517));
#73632=CARTESIAN_POINT('Ctrl Pts',(89.0367791852879,50.449755976069,11.3171830134152));
#73633=CARTESIAN_POINT('Ctrl Pts',(89.0326015969653,50.4504556648391,11.3114935374574));
#73634=CARTESIAN_POINT('Ctrl Pts',(89.017727967652,50.4529085512158,11.2915871209789));
#73635=CARTESIAN_POINT('Ctrl Pts',(89.0067800549273,50.4546457966983,11.2775593199254));
#73636=CARTESIAN_POINT('Ctrl Pts',(88.9860543362218,50.4578225300462,11.2521237586053));
#73637=CARTESIAN_POINT('Ctrl Pts',(88.9763624170447,50.4592658959712,11.240651012034));
#73638=CARTESIAN_POINT('Ctrl Pts',(88.9243675354584,50.4668098088022,11.1812718042929));
#73639=CARTESIAN_POINT('Ctrl Pts',(88.8786931270231,50.47276705523,11.1364331914181));
#73640=CARTESIAN_POINT('Ctrl Pts',(88.7765492036836,50.4852895618523,11.0502768623177));
#73641=CARTESIAN_POINT('Ctrl Pts',(88.7196639181814,50.491841812351,11.0098029501408));
#73642=CARTESIAN_POINT('Ctrl Pts',(88.6447652973133,50.5002531834599,10.9652977413729));
#73643=CARTESIAN_POINT('Ctrl Pts',(88.629597446969,50.5019458217325,10.9567024548141));
#73644=CARTESIAN_POINT('Ctrl Pts',(88.6045745914689,50.5047248157208,10.9431953406822));
#73645=CARTESIAN_POINT('Ctrl Pts',(88.5948236951881,50.5058044861767,10.9380944308729));
#73646=CARTESIAN_POINT('Ctrl Pts',(88.5771532202644,50.5077561733276,10.9291411387469));
#73647=CARTESIAN_POINT('Ctrl Pts',(88.5692573981834,50.5086265332205,10.9252431430309));
#73648=CARTESIAN_POINT('Ctrl Pts',(88.5522284441692,50.5105004471694,10.917055449912));
#73649=CARTESIAN_POINT('Ctrl Pts',(88.5430835214305,50.5115048359098,10.9127919012208));
#73650=CARTESIAN_POINT('Ctrl Pts',(88.5176535060523,50.5142932829565,10.9013027759149));
#73651=CARTESIAN_POINT('Ctrl Pts',(88.5012664623239,50.5160850951454,10.8943105735418));
#73652=CARTESIAN_POINT('Ctrl Pts',(88.4641530742585,50.5201346310081,10.8793894650232));
#73653=CARTESIAN_POINT('Ctrl Pts',(88.4433556405824,50.522398066054,10.8716546901673));
#73654=CARTESIAN_POINT('Ctrl Pts',(88.373170963431,50.530020994298,10.8476255774668));
#73655=CARTESIAN_POINT('Ctrl Pts',(88.3229928274774,50.5354484554071,10.8338218043469));
#73656=CARTESIAN_POINT('Ctrl Pts',(88.1902441127786,50.5497156973191,10.8059323301311));
#73657=CARTESIAN_POINT('Ctrl Pts',(88.1068658778822,50.5585974207116,10.7968620043451));
#73658=CARTESIAN_POINT('Ctrl Pts',(88.0112103798305,50.5684156491252,10.7959434690102));
#73659=CARTESIAN_POINT('Ctrl Pts',(87.9992242987896,50.5696389376938,10.7959980292704));
#73660=CARTESIAN_POINT('Ctrl Pts',(87.9811292404922,50.5714735958391,10.7963366223104));
#73661=CARTESIAN_POINT('Ctrl Pts',(87.9750191195292,50.5720910150153,10.7964950820435));
#73662=CARTESIAN_POINT('Ctrl Pts',(87.9638473666615,50.5732158282852,10.7968655354197));
#73663=CARTESIAN_POINT('Ctrl Pts',(87.9587854314221,50.5737239444895,10.7970637117246));
#73664=CARTESIAN_POINT('Ctrl Pts',(87.9481710785332,50.574786056042,10.7975428937645));
#73665=CARTESIAN_POINT('Ctrl Pts',(87.9426191316844,50.5753397099833,10.7978300725215));
#73666=CARTESIAN_POINT('Ctrl Pts',(87.9274763089576,50.5768450851812,10.7987130843112));
#73667=CARTESIAN_POINT('Ctrl Pts',(87.9178896893916,50.5777929552151,10.7993813422276));
#73668=CARTESIAN_POINT('Ctrl Pts',(87.8599047605607,50.583500309318,10.8040852573779));
#73669=CARTESIAN_POINT('Ctrl Pts',(87.8117546841063,50.5881309514798,10.8107862428404));
#73670=CARTESIAN_POINT('Ctrl Pts',(87.656578052346,50.6030622271736,10.8415409595869));
#73671=CARTESIAN_POINT('Ctrl Pts',(87.552277979746,50.6131514530036,10.8766778297455));
#73672=CARTESIAN_POINT('Ctrl Pts',(87.4350904074372,50.6257165006223,10.9338953159463));
#73673=CARTESIAN_POINT('Ctrl Pts',(87.416622740002,50.6277343804381,10.9434812112058));
#73674=CARTESIAN_POINT('Ctrl Pts',(87.3890177082363,50.6308148341375,10.9586821824363));
#73675=CARTESIAN_POINT('Ctrl Pts',(87.3797014794857,50.6318658009791,10.9639669328338));
#73676=CARTESIAN_POINT('Ctrl Pts',(87.3629927282394,50.6337722495248,10.9737265768937));
#73677=CARTESIAN_POINT('Ctrl Pts',(87.355576812171,50.6346262081228,10.9781603562039));
#73678=CARTESIAN_POINT('Ctrl Pts',(87.3398463128581,50.6364548397345,10.987784440479));
#73679=CARTESIAN_POINT('Ctrl Pts',(87.3315454862454,50.6374302453875,10.9929959858024));
#73680=CARTESIAN_POINT('Ctrl Pts',(87.3145643725677,50.6394478998342,11.0039333651496));
#73681=CARTESIAN_POINT('Ctrl Pts',(87.3058924631122,50.6404905207432,11.0096707592265));
#73682=CARTESIAN_POINT('Ctrl Pts',(87.2626117579527,50.6457575760369,11.0390759731378));
#73683=CARTESIAN_POINT('Ctrl Pts',(87.2291246874004,50.6500407490533,11.0643374292269));
#73684=CARTESIAN_POINT('Ctrl Pts',(87.1410672345652,50.661911715154,11.1378738561848));
#73685=CARTESIAN_POINT('Ctrl Pts',(87.0893051868982,50.6695952362075,11.1892575459361));
#73686=CARTESIAN_POINT('Ctrl Pts',(87.0057996198002,50.6831997367175,11.2877665315057));
#73687=CARTESIAN_POINT('Ctrl Pts',(86.9722584683398,50.6891095307555,11.3331336162015));
#73688=CARTESIAN_POINT('Ctrl Pts',(86.9364755486907,50.6958781514125,11.3889505702609));
#73689=CARTESIAN_POINT('Ctrl Pts',(86.9312110986664,50.6968873805576,11.3973785243914));
#73690=CARTESIAN_POINT('Ctrl Pts',(86.9231190805357,50.6984591494907,11.4106780874535));
#73691=CARTESIAN_POINT('Ctrl Pts',(86.9202242573422,50.6990257076263,11.4155078880149));
#73692=CARTESIAN_POINT('Ctrl Pts',(86.9147971950766,50.7000958460839,11.4247006517141));
#73693=CARTESIAN_POINT('Ctrl Pts',(86.9122587913744,50.7005997714842,11.4290594988228));
#73694=CARTESIAN_POINT('Ctrl Pts',(86.9062093966164,50.7018091830133,11.4395910708417));
#73695=CARTESIAN_POINT('Ctrl Pts',(86.9027240679784,50.7025130499213,11.4457783532729));
#73696=CARTESIAN_POINT('Ctrl Pts',(86.8905610885781,50.7049960698484,11.4678004760827));
#73697=CARTESIAN_POINT('Ctrl Pts',(86.8821687623422,50.7067587701328,11.4837919770318));
#73698=CARTESIAN_POINT('Ctrl Pts',(86.871357951743,50.7091064374567,11.5055052232116));
#73699=CARTESIAN_POINT('Ctrl Pts',(86.8686368482392,50.7097043859978,11.5110722331004));
#73700=CARTESIAN_POINT('Ctrl Pts',(86.857612617095,50.7121572463431,11.534051085486));
#73701=CARTESIAN_POINT('Ctrl Pts',(86.8496654974237,50.7139980522281,11.5516320662685));
#73702=CARTESIAN_POINT('Ctrl Pts',(86.8129648770841,50.7229039802973,11.638014589817));
#73703=CARTESIAN_POINT('Ctrl Pts',(86.7899072459362,50.7298164424287,11.7090780399915));
#73704=CARTESIAN_POINT('Ctrl Pts',(86.7665956722931,50.739623894063,11.810592140147));
#73705=CARTESIAN_POINT('Ctrl Pts',(86.7609840665396,50.7424225527554,11.8396479177557));
#73706=CARTESIAN_POINT('Ctrl Pts',(86.7515192764045,50.7482422335109,11.89988575983));
#73707=CARTESIAN_POINT('Ctrl Pts',(86.7477983743734,50.7512643137505,11.931066976616));
#73708=CARTESIAN_POINT('Ctrl Pts',(86.7442145865341,50.7555415829047,11.974832357443));
#73709=CARTESIAN_POINT('Ctrl Pts',(86.7433772602529,50.7567667183457,11.9873273528142));
#73710=CARTESIAN_POINT('Ctrl Pts',(86.7422604385822,50.7588738081213,12.0087340827899));
#73711=CARTESIAN_POINT('Ctrl Pts',(86.7418897624083,50.7597528742209,12.0176403612404));
#73712=CARTESIAN_POINT('Ctrl Pts',(86.7413908361932,50.7613422019641,12.0336941723447));
#73713=CARTESIAN_POINT('Ctrl Pts',(86.7412291216526,50.7620513840103,12.040840379757));
#73714=CARTESIAN_POINT('Ctrl Pts',(86.7410409837832,50.76337102007,12.0541039224022));
#73715=CARTESIAN_POINT('Ctrl Pts',(86.7409984184484,50.7639809463774,12.0602208479458));
#73716=CARTESIAN_POINT('Ctrl Pts',(86.7410000448951,50.7645922586327,12.0663376885773));
#73717=CARTESIAN_POINT('Ctrl Pts',(86.7410000447486,50.7645922035288,12.0663371372026));
#73718=CARTESIAN_POINT('Ctrl Pts',(86.7410023456166,50.7654584163238,12.0750045347553));
#73719=CARTESIAN_POINT('Ctrl Pts',(86.7410933751595,50.7663273812323,12.0836714430582));
#73720=CARTESIAN_POINT('Ctrl Pts',(86.7415718652515,50.7686481774774,12.1067402439223));
#73721=CARTESIAN_POINT('Ctrl Pts',(86.7421156803795,50.7701047204387,12.1211370738178));
#73722=CARTESIAN_POINT('Ctrl Pts',(86.7468349430576,50.7788657526092,12.2072188902602));
#73723=CARTESIAN_POINT('Ctrl Pts',(86.7568383137963,50.7863417879925,12.2784392447491));
#73724=CARTESIAN_POINT('Ctrl Pts',(86.7892680712375,50.8016896527302,12.4206198309249));
#73725=CARTESIAN_POINT('Ctrl Pts',(86.8120207969228,50.8095380783809,12.4912466070921));
#73726=CARTESIAN_POINT('Ctrl Pts',(86.8477272851518,50.8190228295637,12.5759159671575));
#73727=CARTESIAN_POINT('Ctrl Pts',(86.8549989752535,50.8208493164447,12.5921933549002));
#73728=CARTESIAN_POINT('Ctrl Pts',(86.8656287469066,50.8233747536019,12.6147026656477));
#73729=CARTESIAN_POINT('Ctrl Pts',(86.868699284808,50.8240887231853,12.6210666692601));
#73730=CARTESIAN_POINT('Ctrl Pts',(86.8740497445912,50.8253062984407,12.6319235754041));
#73731=CARTESIAN_POINT('Ctrl Pts',(86.876303523269,50.8258114325395,12.6364290376006));
#73732=CARTESIAN_POINT('Ctrl Pts',(86.8811389028331,50.8268788338796,12.6459532297317));
#73733=CARTESIAN_POINT('Ctrl Pts',(86.8837272229446,50.827440679765,12.6509683224287));
#73734=CARTESIAN_POINT('Ctrl Pts',(86.8909961472493,50.8289929786911,12.6648250543686));
#73735=CARTESIAN_POINT('Ctrl Pts',(86.8957480900361,50.829979168734,12.6736292259547));
#73736=CARTESIAN_POINT('Ctrl Pts',(86.9307070500633,50.8370401017552,12.7366074123193));
#73737=CARTESIAN_POINT('Ctrl Pts',(86.964748915361,50.8429027571994,12.788571029944));
#73738=CARTESIAN_POINT('Ctrl Pts',(87.0316113988497,50.8532345390526,12.8759374488599));
#73739=CARTESIAN_POINT('Ctrl Pts',(87.0628969375233,50.8577090726089,12.9123458238389));
#73740=CARTESIAN_POINT('Ctrl Pts',(87.1230896966267,50.8658744272791,12.9748574814305));
#73741=CARTESIAN_POINT('Ctrl Pts',(87.1512780495804,50.8695470862058,13.0015663082118));
#73742=CARTESIAN_POINT('Ctrl Pts',(87.1806428354228,50.8732662532979,13.0269406741497));
#73743=CARTESIAN_POINT('',(86.7410003148723,50.93532359951,12.0668943017129));
#73744=CARTESIAN_POINT('Ctrl Pts',(87.1806428354228,51.0436650276944,13.0269406741497));
#73745=CARTESIAN_POINT('Ctrl Pts',(87.1430769411697,51.0387322644776,12.9944796593588));
#73746=CARTESIAN_POINT('Ctrl Pts',(87.1073801397486,51.0337995012609,12.9597803455295));
#73747=CARTESIAN_POINT('Ctrl Pts',(87.0738248751965,51.0288667380441,12.9230897184365));
#73748=CARTESIAN_POINT('Ctrl Pts',(87.0402848627672,51.0239362169528,12.8864157686058));
#73749=CARTESIAN_POINT('Ctrl Pts',(87.0088848274002,51.0190056958614,12.8477527031886));
#73750=CARTESIAN_POINT('Ctrl Pts',(86.9798597720419,51.01407517477,12.8073837267478));
#73751=CARTESIAN_POINT('Ctrl Pts',(86.9494169468044,51.0089038154027,12.7650428705588));
#73752=CARTESIAN_POINT('Ctrl Pts',(86.9215875510066,51.0037324560354,12.7208256290176));
#73753=CARTESIAN_POINT('Ctrl Pts',(86.8965925656136,50.998561096668,12.6750944673729));
#73754=CARTESIAN_POINT('Ctrl Pts',(86.8727362769691,50.9936253289606,12.6314466806232));
#73755=CARTESIAN_POINT('Ctrl Pts',(86.8514618982502,50.9886895612531,12.5864204923266));
#73756=CARTESIAN_POINT('Ctrl Pts',(86.8329135745309,50.9837537935456,12.5403546923193));
#73757=CARTESIAN_POINT('Ctrl Pts',(86.8143526726114,50.9788146787392,12.4942576536479));
#73758=CARTESIAN_POINT('Ctrl Pts',(86.798521676003,50.9738755639328,12.4471201205344));
#73759=CARTESIAN_POINT('Ctrl Pts',(86.7855151215509,50.9689364491264,12.3992968837125));
#73760=CARTESIAN_POINT('Ctrl Pts',(86.7724856954086,50.9639886490141,12.3513895509634));
#73761=CARTESIAN_POINT('Ctrl Pts',(86.7622907226357,50.9590408489019,12.3027946460171));
#73762=CARTESIAN_POINT('Ctrl Pts',(86.7549735022767,50.9540930487896,12.2538761214657));
#73763=CARTESIAN_POINT('Ctrl Pts',(86.753951008858,50.9534016533138,12.2470403468198));
#73764=CARTESIAN_POINT('Ctrl Pts',(86.7529846253408,50.9527102578379,12.2401982568247));
#73765=CARTESIAN_POINT('Ctrl Pts',(86.752074388931,50.9520188623621,12.2333508464107));
#73766=CARTESIAN_POINT('Ctrl Pts',(86.7447478362555,50.9464537747447,12.1782355900387));
#73767=CARTESIAN_POINT('Ctrl Pts',(86.7410395617865,50.9408886871273,12.1226289244708));
#73768=CARTESIAN_POINT('Ctrl Pts',(86.7410003148723,50.93532359951,12.0668943017129));
#73769=CARTESIAN_POINT('Ctrl Pts',(87.1806428354213,50.2511271317289,13.0269406741484));
#73770=CARTESIAN_POINT('Ctrl Pts',(87.1933607595619,50.2528272069875,13.0379303426189));
#73771=CARTESIAN_POINT('Ctrl Pts',(87.2062963695742,50.2545169653573,13.0486671138574));
#73772=CARTESIAN_POINT('Ctrl Pts',(87.2272751080988,50.2571971502778,13.0653876246349));
#73773=CARTESIAN_POINT('Ctrl Pts',(87.2351819200797,50.2581941239906,13.0715379913703));
#73774=CARTESIAN_POINT('Ctrl Pts',(87.2494778044442,50.2599738176597,13.0823891171531));
#73775=CARTESIAN_POINT('Ctrl Pts',(87.2558395914037,50.2607578654046,13.0871247016414));
#73776=CARTESIAN_POINT('Ctrl Pts',(87.2708688789396,50.2625920355324,13.0980949111228));
#73777=CARTESIAN_POINT('Ctrl Pts',(87.279571595843,50.2636402346878,13.1042805442905));
#73778=CARTESIAN_POINT('Ctrl Pts',(87.3054085375234,50.2667130527024,13.12215857191));
#73779=CARTESIAN_POINT('Ctrl Pts',(87.322753138677,50.2687260882595,13.1335423244838));
#73780=CARTESIAN_POINT('Ctrl Pts',(87.3634020759689,50.2733403115177,13.1588186109842));
#73781=CARTESIAN_POINT('Ctrl Pts',(87.3868884976003,50.2759307516124,13.1723998501801));
#73782=CARTESIAN_POINT('Ctrl Pts',(87.4775169115569,50.2856889010736,13.2210013593576));
#73783=CARTESIAN_POINT('Ctrl Pts',(87.547306137468,50.2927144311646,13.250745019563));
#73784=CARTESIAN_POINT('Ctrl Pts',(87.6721704028295,50.3050655083306,13.291226520702));
#73785=CARTESIAN_POINT('Ctrl Pts',(87.7260675111065,50.3103349249922,13.3048691044664));
#73786=CARTESIAN_POINT('Ctrl Pts',(87.7904358936943,50.316752025255,13.3167397925055));
#73787=CARTESIAN_POINT('Ctrl Pts',(87.8002188967009,50.3177306749078,13.3184255896165));
#73788=CARTESIAN_POINT('Ctrl Pts',(87.8155731595856,50.3192734131746,13.3208864405542));
#73789=CARTESIAN_POINT('Ctrl Pts',(87.8211318773399,50.3198333154589,13.3217395112493));
#73790=CARTESIAN_POINT('Ctrl Pts',(87.8316835314354,50.3208990876806,13.3232871652754));
#73791=CARTESIAN_POINT('Ctrl Pts',(87.8366752082008,50.3214045524627,13.3239889800932));
#73792=CARTESIAN_POINT('Ctrl Pts',(87.8487027672629,50.3226254259054,13.325607062744));
#73793=CARTESIAN_POINT('Ctrl Pts',(87.8557422917161,50.3233423875154,13.3264941013898));
#73794=CARTESIAN_POINT('Ctrl Pts',(87.8806906429315,50.3258910450536,13.3294256529803));
#73795=CARTESIAN_POINT('Ctrl Pts',(87.8986338907768,50.3277381139815,13.3311476790901));
#73796=CARTESIAN_POINT('Ctrl Pts',(87.9318608953387,50.3311779743658,13.3336241578025));
#73797=CARTESIAN_POINT('Ctrl Pts',(87.9471342247533,50.3327667472074,13.3344853623832));
#73798=CARTESIAN_POINT('Ctrl Pts',(88.0284505978251,50.3412555789819,13.3375982472763));
#73799=CARTESIAN_POINT('Ctrl Pts',(88.0945772527446,50.3482573087147,13.3349685354004));
#73800=CARTESIAN_POINT('Ctrl Pts',(88.2328883340389,50.3628884955099,13.3186066593674));
#73801=CARTESIAN_POINT('Ctrl Pts',(88.3047143759776,50.3704751140489,13.303737636321));
#73802=CARTESIAN_POINT('Ctrl Pts',(88.3900694645436,50.3794710610343,13.2782119837858));
#73803=CARTESIAN_POINT('Ctrl Pts',(88.4051793312595,50.3810633500663,13.2733832307786));
#73804=CARTESIAN_POINT('Ctrl Pts',(88.4293645216141,50.3836131183543,13.2651517557138));
#73805=CARTESIAN_POINT('Ctrl Pts',(88.4384976915128,50.384576265869,13.2619262281776));
#73806=CARTESIAN_POINT('Ctrl Pts',(88.4559449078257,50.3864172019866,13.2555390385792));
#73807=CARTESIAN_POINT('Ctrl Pts',(88.4642643365153,50.3872954750221,13.2523939255929));
#73808=CARTESIAN_POINT('Ctrl Pts',(88.4834931184777,50.38932704548,13.2448927943395));
#73809=CARTESIAN_POINT('Ctrl Pts',(88.4943766143245,50.3904781255635,13.2404722384276));
#73810=CARTESIAN_POINT('Ctrl Pts',(88.5297762194812,50.3942281918976,13.2255184943305));
#73811=CARTESIAN_POINT('Ctrl Pts',(88.5540233730338,50.396806280095,13.2143630766783));
#73812=CARTESIAN_POINT('Ctrl Pts',(88.6122499809643,50.4030432885563,13.1853175258539));
#73813=CARTESIAN_POINT('Ctrl Pts',(88.6458049051743,50.4066768378064,13.1666345729477));
#73814=CARTESIAN_POINT('Ctrl Pts',(88.7196479063812,50.4148459089605,13.1210172811799));
#73815=CARTESIAN_POINT('Ctrl Pts',(88.7593428157943,50.419361764589,13.0932421292802));
#73816=CARTESIAN_POINT('Ctrl Pts',(88.8462452540176,50.4297546781969,13.0247187708921));
#73817=CARTESIAN_POINT('Ctrl Pts',(88.8922245497247,50.4356365261322,12.9826332529987));
#73818=CARTESIAN_POINT('Ctrl Pts',(88.9417149479889,50.4427073732877,12.9301571805777));
#73819=CARTESIAN_POINT('Ctrl Pts',(88.9484204601546,50.4436828371823,12.9228785245358));
#73820=CARTESIAN_POINT('Ctrl Pts',(88.9588381586419,50.4452276053274,12.9113017616408));
#73821=CARTESIAN_POINT('Ctrl Pts',(88.9626079806121,50.4457928126501,12.9070555806854));
#73822=CARTESIAN_POINT('Ctrl Pts',(88.9696619846618,50.446862547954,12.8990020891879));
#73823=CARTESIAN_POINT('Ctrl Pts',(88.9729522124265,50.447366622778,12.895200348363));
#73824=CARTESIAN_POINT('Ctrl Pts',(88.9807679078606,50.4485762172832,12.8860604741242));
#73825=CARTESIAN_POINT('Ctrl Pts',(88.985271910514,50.4492832111768,12.8807043711685));
#73826=CARTESIAN_POINT('Ctrl Pts',(89.0008089867568,50.4517562628244,12.8619147941696));
#73827=CARTESIAN_POINT('Ctrl Pts',(89.0116095675138,50.4535365558507,12.8482931531908));
#73828=CARTESIAN_POINT('Ctrl Pts',(89.0382663290889,50.4580815023244,12.8132184416301));
#73829=CARTESIAN_POINT('Ctrl Pts',(89.0537319998744,50.4608624108807,12.7914800106823));
#73830=CARTESIAN_POINT('Ctrl Pts',(89.1247048533258,50.4742988958354,12.6847592195526));
#73831=CARTESIAN_POINT('Ctrl Pts',(89.1705868038097,50.4850736822582,12.5937940156327));
#73832=CARTESIAN_POINT('Ctrl Pts',(89.2145924637585,50.4983692545979,12.4722447051878));
#73833=CARTESIAN_POINT('Ctrl Pts',(89.2231797260878,50.5011973652224,12.4458554832027));
#73834=CARTESIAN_POINT('Ctrl Pts',(89.2352430399156,50.5055758519852,12.4041911337756));
#73835=CARTESIAN_POINT('Ctrl Pts',(89.2393124030434,50.5071445229759,12.3890989946561));
#73836=CARTESIAN_POINT('Ctrl Pts',(89.2454385857783,50.5096657737448,12.3645870303443));
#73837=CARTESIAN_POINT('Ctrl Pts',(89.2476684392079,50.5106237952912,12.3552127613446));
#73838=CARTESIAN_POINT('Ctrl Pts',(89.251753924701,50.5124608699196,12.337125495374));
#73839=CARTESIAN_POINT('Ctrl Pts',(89.2536249877953,50.5133403633046,12.3284166263606));
#73840=CARTESIAN_POINT('Ctrl Pts',(89.2577720109134,50.5153835175523,12.3080744613313));
#73841=CARTESIAN_POINT('Ctrl Pts',(89.2599770783257,50.5165448767635,12.296427370355));
#73842=CARTESIAN_POINT('Ctrl Pts',(89.2667295387395,50.5203696949251,12.2578105425165));
#73843=CARTESIAN_POINT('Ctrl Pts',(89.2705691621717,50.523011032483,12.2307232108686));
#73844=CARTESIAN_POINT('Ctrl Pts',(89.277838373264,50.5294413936635,12.16399184886));
#73845=CARTESIAN_POINT('Ctrl Pts',(89.2802860215701,50.5332027767716,12.1242697655643));
#73846=CARTESIAN_POINT('Ctrl Pts',(89.2813758046904,50.5402405372658,12.0494452071396));
#73847=CARTESIAN_POINT('Ctrl Pts',(89.2804349581069,50.543518450964,12.0143889623366));
#73848=CARTESIAN_POINT('Ctrl Pts',(89.2733458687954,50.5532633789349,11.9106491614456));
#73849=CARTESIAN_POINT('Ctrl Pts',(89.2630569744751,50.5597314506678,11.8423915764317));
#73850=CARTESIAN_POINT('Ctrl Pts',(89.2443826145806,50.5676905537196,11.762968136109));
#73851=CARTESIAN_POINT('Ctrl Pts',(89.2412938357436,50.568936485229,11.7506620586212));
#73852=CARTESIAN_POINT('Ctrl Pts',(89.2364250819374,50.5708048354054,11.7324259174487));
#73853=CARTESIAN_POINT('Ctrl Pts',(89.2347850929626,50.5714197401356,11.7264586323839));
#73854=CARTESIAN_POINT('Ctrl Pts',(89.2317521452105,50.5725320533066,11.7157303801249));
#73855=CARTESIAN_POINT('Ctrl Pts',(89.230374804627,50.5730285670758,11.7109652282235));
#73856=CARTESIAN_POINT('Ctrl Pts',(89.2271971618092,50.5741550208695,11.7002082487243));
#73857=CARTESIAN_POINT('Ctrl Pts',(89.2253804954412,50.5747858442692,11.6942216414149));
#73858=CARTESIAN_POINT('Ctrl Pts',(89.2196398336134,50.5767391296854,11.6757950466257));
#73859=CARTESIAN_POINT('Ctrl Pts',(89.2155685485842,50.5780692034371,11.6634025372838));
#73860=CARTESIAN_POINT('Ctrl Pts',(89.2054431682607,50.581249000772,11.6341114772262));
#73861=CARTESIAN_POINT('Ctrl Pts',(89.1992203433359,50.583105639662,11.617274583164));
#73862=CARTESIAN_POINT('Ctrl Pts',(89.1737815846719,50.590327535794,11.5526892374117));
#73863=CARTESIAN_POINT('Ctrl Pts',(89.1520274808799,50.5957607627426,11.5059959026813));
#73864=CARTESIAN_POINT('Ctrl Pts',(89.0863105150756,50.6102964936842,11.3847672435156));
#73865=CARTESIAN_POINT('Ctrl Pts',(89.0374596709513,50.6193315366198,11.3131665459124));
#73866=CARTESIAN_POINT('Ctrl Pts',(88.9705877513366,50.6298472415509,11.2339012736109));
#73867=CARTESIAN_POINT('Ctrl Pts',(88.9592085198891,50.6315838450733,11.2209570303957));
#73868=CARTESIAN_POINT('Ctrl Pts',(88.9401741325998,50.6344060316017,11.2001736327621));
#73869=CARTESIAN_POINT('Ctrl Pts',(88.9326752626552,50.6354979334889,11.1921953328077));
#73870=CARTESIAN_POINT('Ctrl Pts',(88.9189614076943,50.6374599564657,11.1779777022235));
#73871=CARTESIAN_POINT('Ctrl Pts',(88.9127830440334,50.6383315712694,11.1717042599807));
#73872=CARTESIAN_POINT('Ctrl Pts',(88.8993522803582,50.640200580341,11.1583475461461));
#73873=CARTESIAN_POINT('Ctrl Pts',(88.8920792528265,50.641196991888,11.1512857735986));
#73874=CARTESIAN_POINT('Ctrl Pts',(88.8716371367725,50.6439555543264,11.1319074999547));
#73875=CARTESIAN_POINT('Ctrl Pts',(88.8582886754994,50.6457095340881,11.1197827639675));
#73876=CARTESIAN_POINT('Ctrl Pts',(88.827685685288,50.6496321805462,11.0931524624263));
#73877=CARTESIAN_POINT('Ctrl Pts',(88.8102938984672,50.6517942513949,11.0788134761274));
#73878=CARTESIAN_POINT('Ctrl Pts',(88.7504328539674,50.6590354612147,11.0320797101052));
#73879=CARTESIAN_POINT('Ctrl Pts',(88.7063036785166,50.6640443439526,11.0019014526015));
#73880=CARTESIAN_POINT('Ctrl Pts',(88.5883545841602,50.6769025714163,10.9317203834137));
#73881=CARTESIAN_POINT('Ctrl Pts',(88.512254065804,50.6847074000522,10.8960995081019));
#73882=CARTESIAN_POINT('Ctrl Pts',(88.4222478726026,50.6940316630985,10.8643717289543));
#73883=CARTESIAN_POINT('Ctrl Pts',(88.4112251605279,50.6951752405397,10.8606556092584));
#73884=CARTESIAN_POINT('Ctrl Pts',(88.39439041845,50.6969267161178,10.8552364210392));
#73885=CARTESIAN_POINT('Ctrl Pts',(88.3886141778352,50.6975285445198,10.8534225038224));
#73886=CARTESIAN_POINT('Ctrl Pts',(88.3785533584201,50.6985786807131,10.8503419517906));
#73887=CARTESIAN_POINT('Ctrl Pts',(88.3742746963736,50.6990258940004,10.8490565115931));
#73888=CARTESIAN_POINT('Ctrl Pts',(88.3641013667044,50.7000907055486,10.8460585654577));
#73889=CARTESIAN_POINT('Ctrl Pts',(88.3582011108808,50.7007094072312,10.8443662325694));
#73890=CARTESIAN_POINT('Ctrl Pts',(88.3403197923637,50.7025874454875,10.8393774465212));
#73891=CARTESIAN_POINT('Ctrl Pts',(88.3283029698728,50.7038536018419,10.8362141658418));
#73892=CARTESIAN_POINT('Ctrl Pts',(88.2674624978797,50.7102785868745,10.8211496635686));
#73893=CARTESIAN_POINT('Ctrl Pts',(88.2180150528518,50.7155454192613,10.8119789597148));
#73894=CARTESIAN_POINT('Ctrl Pts',(88.0782726214735,50.7303768945394,10.7945519608485));
#73895=CARTESIAN_POINT('Ctrl Pts',(87.9874236354046,50.7399365560761,10.7929894504075));
#73896=CARTESIAN_POINT('Ctrl Pts',(87.8681451949257,50.7522120735621,10.8037235797317));
#73897=CARTESIAN_POINT('Ctrl Pts',(87.8392161648363,50.7551702834468,10.8073340702816));
#73898=CARTESIAN_POINT('Ctrl Pts',(87.7993527411348,50.7592251288385,10.8137095501827));
#73899=CARTESIAN_POINT('Ctrl Pts',(87.7882951149303,50.7603476224732,10.8156286600132));
#73900=CARTESIAN_POINT('Ctrl Pts',(87.7691461853345,50.762288154719,10.8192141562275));
#73901=CARTESIAN_POINT('Ctrl Pts',(87.7610432345023,50.7631082581969,10.8208133346681));
#73902=CARTESIAN_POINT('Ctrl Pts',(87.7441107979463,50.7648201708318,10.824327030018));
#73903=CARTESIAN_POINT('Ctrl Pts',(87.7352849389046,50.7657114411779,10.8262569515287));
#73904=CARTESIAN_POINT('Ctrl Pts',(87.7141703174142,50.7678417775888,10.8311106614747));
#73905=CARTESIAN_POINT('Ctrl Pts',(87.7019028786637,50.769077928063,10.8341239768997));
#73906=CARTESIAN_POINT('Ctrl Pts',(87.6581701957626,50.7734820319056,10.8455607238672));
#73907=CARTESIAN_POINT('Ctrl Pts',(87.6269844028073,50.7766171820344,10.8550114260545));
#73908=CARTESIAN_POINT('Ctrl Pts',(87.5472197120588,50.7846678443899,10.8825758630856));
#73909=CARTESIAN_POINT('Ctrl Pts',(87.4993246728235,50.7895319408776,10.902482063593));
#73910=CARTESIAN_POINT('Ctrl Pts',(87.3783376234381,50.8021533318055,10.9616873993773));
#73911=CARTESIAN_POINT('Ctrl Pts',(87.307657228934,50.8098615479298,11.0053059913324));
#73912=CARTESIAN_POINT('Ctrl Pts',(87.2317311902766,50.8191515321603,11.0631049954354));
#73913=CARTESIAN_POINT('Ctrl Pts',(87.2218356063798,50.8203841734155,11.0708729803637));
#73914=CARTESIAN_POINT('Ctrl Pts',(87.2071927750937,50.8222442295094,11.0827232770878));
#73915=CARTESIAN_POINT('Ctrl Pts',(87.2023571983565,50.8228645204907,11.0866961748154));
#73916=CARTESIAN_POINT('Ctrl Pts',(87.1936715635788,50.823990096353,11.0939404589562));
#73917=CARTESIAN_POINT('Ctrl Pts',(87.1898112996983,50.8244944943799,11.0971993802937));
#73918=CARTESIAN_POINT('Ctrl Pts',(87.1818559772851,50.8255428392805,11.1039971514426));
#73919=CARTESIAN_POINT('Ctrl Pts',(87.1777640663151,50.8260869821424,11.1075391683529));
#73920=CARTESIAN_POINT('Ctrl Pts',(87.1675202616545,50.8274613913342,11.1165215246915));
#73921=CARTESIAN_POINT('Ctrl Pts',(87.16139841877,50.8282939675565,11.1219954532139));
#73922=CARTESIAN_POINT('Ctrl Pts',(87.1475748063007,50.8301989646515,11.1345993949217));
#73923=CARTESIAN_POINT('Ctrl Pts',(87.1399075858775,50.8312736297951,11.1417661902698));
#73924=CARTESIAN_POINT('Ctrl Pts',(87.1166108724021,50.8345930437667,11.1640897565982));
#73925=CARTESIAN_POINT('Ctrl Pts',(87.1012824287929,50.8368536336616,11.1795532795196));
#73926=CARTESIAN_POINT('Ctrl Pts',(87.0346016725022,50.8470131674831,11.250373181455));
#73927=CARTESIAN_POINT('Ctrl Pts',(86.9878484774379,50.855025435301,11.309850435194));
#73928=CARTESIAN_POINT('Ctrl Pts',(86.9128489266427,50.8694115247047,11.4250602058156));
#73929=CARTESIAN_POINT('Ctrl Pts',(86.8828829344972,50.875805445719,11.4794043279298));
#73930=CARTESIAN_POINT('Ctrl Pts',(86.8504864413318,50.8836373421491,11.5499072950956));
#73931=CARTESIAN_POINT('Ctrl Pts',(86.8442337816867,50.8852031886813,11.5642031810678));
#73932=CARTESIAN_POINT('Ctrl Pts',(86.8345504019281,50.887721023568,11.5875033294502));
#73933=CARTESIAN_POINT('Ctrl Pts',(86.8309561373216,50.8886784270204,11.596437207851));
#73934=CARTESIAN_POINT('Ctrl Pts',(86.8242327904738,50.8905150375786,11.6137136350366));
#73935=CARTESIAN_POINT('Ctrl Pts',(86.8210892210585,50.8913946796686,11.6220498745539));
#73936=CARTESIAN_POINT('Ctrl Pts',(86.8139637432605,50.8934392516797,11.6415650776602));
#73937=CARTESIAN_POINT('Ctrl Pts',(86.810050207516,50.8946018695847,11.6527683187081));
#73938=CARTESIAN_POINT('Ctrl Pts',(86.8021406192779,50.8970399120771,11.6764731092283));
#73939=CARTESIAN_POINT('Ctrl Pts',(86.7981801392068,50.8983141025145,11.6889851253288));
#73940=CARTESIAN_POINT('Ctrl Pts',(86.7878534175345,50.9017929641555,11.7234578347432));
#73941=CARTESIAN_POINT('Ctrl Pts',(86.7818848923609,50.9039857019889,11.7455333348979));
#73942=CARTESIAN_POINT('Ctrl Pts',(86.7528442359326,50.9157727302543,11.865739128937));
#73943=CARTESIAN_POINT('Ctrl Pts',(86.7409239715871,50.9250457026798,11.9661780945622));
#73944=CARTESIAN_POINT('Ctrl Pts',(86.7410003648342,50.9346029221184,12.0669626415845));
#73945=CARTESIAN_POINT('Origin',(88.011,65.0896,12.066));
#73946=CARTESIAN_POINT('',(86.3066601088578,64.6798399153869,12.0666091481311));
#73947=CARTESIAN_POINT('',(88.8060699928714,64.9396,13.5735272939604));
#73948=CARTESIAN_POINT('Ctrl Pts',(86.306660108858,64.6798399154298,12.0666091487058));
#73949=CARTESIAN_POINT('Ctrl Pts',(86.3066704464735,64.6819963896155,12.095532809473));
#73950=CARTESIAN_POINT('Ctrl Pts',(86.3074170166427,64.6841528638012,12.1244434963871));
#73951=CARTESIAN_POINT('Ctrl Pts',(86.3088981128696,64.6863093379869,12.1533155279848));
#73952=CARTESIAN_POINT('Ctrl Pts',(86.3120611916116,64.6909147765331,12.214975606324));
#73953=CARTESIAN_POINT('Ctrl Pts',(86.3185854995964,64.6955202150793,12.2765881435167));
#73954=CARTESIAN_POINT('Ctrl Pts',(86.3284654841818,64.7001256536254,12.3377580517307));
#73955=CARTESIAN_POINT('Ctrl Pts',(86.3384945128726,64.7048005673273,12.399850736105));
#73956=CARTESIAN_POINT('Ctrl Pts',(86.3519813709746,64.7094754810292,12.461486795159));
#73957=CARTESIAN_POINT('Ctrl Pts',(86.3688652169034,64.714150394731,12.5222545229849));
#73958=CARTESIAN_POINT('Ctrl Pts',(86.3854521571814,64.7187430991839,12.5819536387276));
#73959=CARTESIAN_POINT('Ctrl Pts',(86.4053174346001,64.7233358036367,12.6408142071515));
#73960=CARTESIAN_POINT('Ctrl Pts',(86.4283517349835,64.7279285080896,12.6984549824615));
#73961=CARTESIAN_POINT('Ctrl Pts',(86.4513717033921,64.7325183549551,12.7560598935981));
#73962=CARTESIAN_POINT('Ctrl Pts',(86.4775565967264,64.7371082018206,12.8124460468413));
#73963=CARTESIAN_POINT('Ctrl Pts',(86.506747924809,64.7416980486861,12.8672493556213));
#73964=CARTESIAN_POINT('Ctrl Pts',(86.5359317104231,64.7462867096249,12.9220385042976));
#73965=CARTESIAN_POINT('Ctrl Pts',(86.5681201503177,64.7508753705637,12.975245173118));
#73966=CARTESIAN_POINT('Ctrl Pts',(86.6031083773965,64.7554640315025,13.0265290285061));
#73967=CARTESIAN_POINT('Ctrl Pts',(86.6392375609678,64.7602023274165,13.0794852363583));
#73968=CARTESIAN_POINT('Ctrl Pts',(86.6783520305866,64.7649406233304,13.1303905425967));
#73969=CARTESIAN_POINT('Ctrl Pts',(86.720178601905,64.7696789192444,13.1789038385324));
#73970=CARTESIAN_POINT('Ctrl Pts',(86.760733202724,64.774273120808,13.2259418167618));
#73971=CARTESIAN_POINT('Ctrl Pts',(86.8038368845309,64.7788673223717,13.2707308699209));
#73972=CARTESIAN_POINT('Ctrl Pts',(86.8492022623125,64.7834615239353,13.3129967330768));
#73973=CARTESIAN_POINT('Ctrl Pts',(86.8967019265033,64.7882718670245,13.3572510610425));
#73974=CARTESIAN_POINT('Ctrl Pts',(86.946680901022,64.7930822101136,13.398738486692));
#73975=CARTESIAN_POINT('Ctrl Pts',(86.9987718552393,64.7978925532027,13.43719255342));
#73976=CARTESIAN_POINT('Ctrl Pts',(87.0508628094566,64.8027028962919,13.475646620148));
#73977=CARTESIAN_POINT('Ctrl Pts',(87.1050651763733,64.807513239381,13.5110670434374));
#73978=CARTESIAN_POINT('Ctrl Pts',(87.1609813508699,64.8123235824701,13.543241730974));
#73979=CARTESIAN_POINT('Ctrl Pts',(87.2144523232767,64.8169235703073,13.5740094264566));
#73980=CARTESIAN_POINT('Ctrl Pts',(87.2697035984548,64.8215235581445,13.6019321206037));
#73981=CARTESIAN_POINT('Ctrl Pts',(87.3264006550764,64.8261235459817,13.6268006190831));
#73982=CARTESIAN_POINT('Ctrl Pts',(87.3840296067459,64.8307991410222,13.6520778659519));
#73983=CARTESIAN_POINT('Ctrl Pts',(87.4431518843408,64.8354747360627,13.6741992645683));
#73984=CARTESIAN_POINT('Ctrl Pts',(87.5033875661512,64.8401503311031,13.6929924562216));
#73985=CARTESIAN_POINT('Ctrl Pts',(87.5624893325295,64.8447379097186,13.7114318726807));
#73986=CARTESIAN_POINT('Ctrl Pts',(87.6226624393423,64.8493254883341,13.726667145479));
#73987=CARTESIAN_POINT('Ctrl Pts',(87.6835277454027,64.8539130669496,13.7385838568123));
#73988=CARTESIAN_POINT('Ctrl Pts',(87.7443569176477,64.8584979220641,13.7504934935693));
#73989=CARTESIAN_POINT('Ctrl Pts',(87.8058769765099,64.8630827771787,13.7590883781332));
#73990=CARTESIAN_POINT('Ctrl Pts',(87.8676965928791,64.8676676322932,13.7643047338766));
#73991=CARTESIAN_POINT('Ctrl Pts',(87.9295021218816,64.8722514426175,13.7695199009242));
#73992=CARTESIAN_POINT('Ctrl Pts',(87.9916065666705,64.8768352529417,13.7713580249794));
#73993=CARTESIAN_POINT('Ctrl Pts',(88.0536134849601,64.881419063266,13.769807185834));
#73994=CARTESIAN_POINT('Ctrl Pts',(88.1177769370419,64.8861622935732,13.7682024101745));
#73995=CARTESIAN_POINT('Ctrl Pts',(88.1818353744046,64.8909055238805,13.7629685434884));
#73996=CARTESIAN_POINT('Ctrl Pts',(88.2453521333063,64.8956487541878,13.7541510338873));
#73997=CARTESIAN_POINT('Ctrl Pts',(88.3068136763909,64.9002385074897,13.7456188330066));
#73998=CARTESIAN_POINT('Ctrl Pts',(88.3677675604565,64.9048282607915,13.7337315525005));
#73999=CARTESIAN_POINT('Ctrl Pts',(88.4278283183883,64.9094180140933,13.7185825209621));
#74000=CARTESIAN_POINT('Ctrl Pts',(88.4909016386516,64.9142379829033,13.7026736355134));
#74001=CARTESIAN_POINT('Ctrl Pts',(88.5529892627615,64.9190579517134,13.6831673404478));
#74002=CARTESIAN_POINT('Ctrl Pts',(88.6136655192791,64.9238779205234,13.6602299418441));
#74003=CARTESIAN_POINT('Ctrl Pts',(88.6743417757967,64.9286978893333,13.6372925432403));
#74004=CARTESIAN_POINT('Ctrl Pts',(88.7336061107467,64.9335178581434,13.6109243717016));
#74005=CARTESIAN_POINT('Ctrl Pts',(88.7910626927788,64.9383378269534,13.5813471651522));
#74006=CARTESIAN_POINT('Ctrl Pts',(88.7960779499343,64.9387585513022,13.5787654366271));
#74007=CARTESIAN_POINT('Ctrl Pts',(88.8010804362425,64.9391792756511,13.5761587864509));
#74008=CARTESIAN_POINT('Ctrl Pts',(88.8060699928714,64.9396,13.5735272939604));
#74009=CARTESIAN_POINT('',(87.2157910724421,64.9396,13.5734540116143));
#74010=CARTESIAN_POINT('Origin',(88.011,64.9396,12.066));
#74011=CARTESIAN_POINT('',(86.306311228203,64.8024850845702,12.0672964986124));
#74012=CARTESIAN_POINT('Ctrl Pts',(87.2157910724421,64.9396,13.5734540116144));
#74013=CARTESIAN_POINT('Ctrl Pts',(86.7145593062453,64.8975952518389,13.309045298523));
#74014=CARTESIAN_POINT('Ctrl Pts',(86.3287535439272,64.851890280029,12.7301966984418));
#74015=CARTESIAN_POINT('Ctrl Pts',(86.3044108940433,64.8061853082191,12.1169819374226));
#74016=CARTESIAN_POINT('Ctrl Pts',(86.3047298421322,64.8024850845702,12.0672977013333));
#74017=CARTESIAN_POINT('',(86.3066602867323,64.0087350846259,12.0669886246394));
#74018=CARTESIAN_POINT('Ctrl Pts',(86.306660492924,64.8024850845702,12.0672962329796));
#74019=CARTESIAN_POINT('Ctrl Pts',(86.3066145342196,64.7979795717007,12.0068678711104));
#74020=CARTESIAN_POINT('Ctrl Pts',(86.309786550778,64.7934740588313,11.9462894264899));
#74021=CARTESIAN_POINT('Ctrl Pts',(86.3161980195603,64.7889685459618,11.8859414464744));
#74022=CARTESIAN_POINT('Ctrl Pts',(86.3225985529314,64.7844707177022,11.8256963960686));
#74023=CARTESIAN_POINT('Ctrl Pts',(86.3322275268003,64.7799728894426,11.7656815533077));
#74024=CARTESIAN_POINT('Ctrl Pts',(86.3450544185545,64.7754750611829,11.7062776692192));
#74025=CARTESIAN_POINT('Ctrl Pts',(86.3578692724028,64.7709814540889,11.6469295350653));
#74026=CARTESIAN_POINT('Ctrl Pts',(86.3738759928126,64.7664878469948,11.5881917405843));
#74027=CARTESIAN_POINT('Ctrl Pts',(86.3929924649126,64.7619942399008,11.5304381903082));
#74028=CARTESIAN_POINT('Ctrl Pts',(86.4120986283622,64.7575030560062,11.4727157839144));
#74029=CARTESIAN_POINT('Ctrl Pts',(86.4343110558028,64.7530118721116,11.4159770732769));
#74030=CARTESIAN_POINT('Ctrl Pts',(86.45949751305,64.748520688217,11.3605817775334));
#74031=CARTESIAN_POINT('Ctrl Pts',(86.4846804398158,64.7440301338687,11.3051942467589));
#74032=CARTESIAN_POINT('Ctrl Pts',(86.5128363483428,64.7395395795204,11.2511502394488));
#74033=CARTESIAN_POINT('Ctrl Pts',(86.5437854254147,64.7350490251721,11.1987882451646));
#74034=CARTESIAN_POINT('Ctrl Pts',(86.5747636162918,64.7305542465581,11.1463769939383));
#74035=CARTESIAN_POINT('Ctrl Pts',(86.6085399490278,64.7260594679441,11.0956513711113));
#74036=CARTESIAN_POINT('Ctrl Pts',(86.6448901103306,64.7215646893301,11.0469226697902));
#74037=CARTESIAN_POINT('Ctrl Pts',(86.6812590641617,64.717067586978,10.9981687764078));
#74038=CARTESIAN_POINT('Ctrl Pts',(86.7202041512511,64.7125704846259,10.9514142637556));
#74039=CARTESIAN_POINT('Ctrl Pts',(86.7614615221642,64.7080733822739,10.9069364003612));
#74040=CARTESIAN_POINT('Ctrl Pts',(86.8027923199855,64.7035682763017,10.8623793784571));
#74041=CARTESIAN_POINT('Ctrl Pts',(86.8464432283836,64.6990631703296,10.8201074552435));
#74042=CARTESIAN_POINT('Ctrl Pts',(86.8921154391265,64.6945580643574,10.7803592356187));
#74043=CARTESIAN_POINT('Ctrl Pts',(86.9157250454818,64.6922292132495,10.7598119530721));
#74044=CARTESIAN_POINT('Ctrl Pts',(86.9398742803986,64.6899003621415,10.7399383743142));
#74045=CARTESIAN_POINT('Ctrl Pts',(86.964518941691,64.6875715110336,10.7207668491297));
#74046=CARTESIAN_POINT('Ctrl Pts',(87.0132040064965,64.6829709094766,10.6828938617531));
#74047=CARTESIAN_POINT('Ctrl Pts',(87.0640472917073,64.6783703079196,10.6475897303211));
#74048=CARTESIAN_POINT('Ctrl Pts',(87.1167469574559,64.6737697063626,10.6151084356505));
#74049=CARTESIAN_POINT('Ctrl Pts',(87.1703047911227,64.6690941880371,10.5820982115335));
#74050=CARTESIAN_POINT('Ctrl Pts',(87.2257796473751,64.6644186697116,10.5520039826383));
#74051=CARTESIAN_POINT('Ctrl Pts',(87.2828196869196,64.6597431513861,10.5250495571751));
#74052=CARTESIAN_POINT('Ctrl Pts',(87.3387900792101,64.6551553110387,10.4986005964243));
#74053=CARTESIAN_POINT('Ctrl Pts',(87.3962669781763,64.6505674706913,10.4751749229019));
#74054=CARTESIAN_POINT('Ctrl Pts',(87.454891069006,64.6459796303438,10.4549389544562));
#74055=CARTESIAN_POINT('Ctrl Pts',(87.5134786793428,64.6413946449094,10.4347155784122));
#74056=CARTESIAN_POINT('Ctrl Pts',(87.5732115866053,64.6368096594749,10.4176781369421));
#74057=CARTESIAN_POINT('Ctrl Pts',(87.6337112909016,64.6322246740405,10.4039446261972));
#74058=CARTESIAN_POINT('Ctrl Pts',(87.6941954774681,64.6276408646211,10.3902146379969));
#74059=CARTESIAN_POINT('Ctrl Pts',(87.7554455752919,64.6230570552018,10.3797870106611));
#74060=CARTESIAN_POINT('Ctrl Pts',(87.8170707322931,64.6184732457824,10.3727291195067));
#74061=CARTESIAN_POINT('Ctrl Pts',(87.8808360388893,64.613730247513,10.3654261183414));
#74062=CARTESIAN_POINT('Ctrl Pts',(87.9450023692494,64.6089872492437,10.3617313487824));
#74063=CARTESIAN_POINT('Ctrl Pts',(88.0091310074875,64.6042442509744,10.3616610247762));
#74064=CARTESIAN_POINT('Ctrl Pts',(88.0711832546621,64.5996548240187,10.3615929777579));
#74065=CARTESIAN_POINT('Ctrl Pts',(88.1331996911742,64.5950653970631,10.3649181350441));
#74066=CARTESIAN_POINT('Ctrl Pts',(88.1947855492387,64.5904759701075,10.3715981269218));
#74067=CARTESIAN_POINT('Ctrl Pts',(88.259462584444,64.5856561861813,10.378613407433));
#74068=CARTESIAN_POINT('Ctrl Pts',(88.3236640465969,64.5808364022551,10.3893290966777));
#74069=CARTESIAN_POINT('Ctrl Pts',(88.3869450187697,64.5760166183289,10.4036401778008));
#74070=CARTESIAN_POINT('Ctrl Pts',(88.4502259909424,64.5711968344027,10.4179512589238));
#74071=CARTESIAN_POINT('Ctrl Pts',(88.5125858776316,64.5663770504765,10.435857483342));
#74072=CARTESIAN_POINT('Ctrl Pts',(88.5736014800555,64.5615572665503,10.4571947258169));
#74073=CARTESIAN_POINT('Ctrl Pts',(88.6318937333619,64.5569526071788,10.4775796092532));
#74074=CARTESIAN_POINT('Ctrl Pts',(88.6891919339384,64.5523479478074,10.5011770587036));
#74075=CARTESIAN_POINT('Ctrl Pts',(88.7451186757438,64.5477432884359,10.5278697696475));
#74076=CARTESIAN_POINT('Ctrl Pts',(88.8018998874603,64.5430682773372,10.5549703019236));
#74077=CARTESIAN_POINT('Ctrl Pts',(88.8572668522401,64.5383932662385,10.5852613856813));
#74078=CARTESIAN_POINT('Ctrl Pts',(88.9108417461413,64.5337182551398,10.6185679057374));
#74079=CARTESIAN_POINT('Ctrl Pts',(88.9634697272463,64.5291258728157,10.6512857476321));
#74080=CARTESIAN_POINT('Ctrl Pts',(89.014368024192,64.5245334904916,10.6869130163857));
#74081=CARTESIAN_POINT('Ctrl Pts',(89.0632019382488,64.5199411081675,10.7252368155616));
#74082=CARTESIAN_POINT('Ctrl Pts',(89.1120072809413,64.5153514127185,10.7635381925489));
#74083=CARTESIAN_POINT('Ctrl Pts',(89.1587502378458,64.5107617172695,10.8045326587561));
#74084=CARTESIAN_POINT('Ctrl Pts',(89.203126525106,64.5061720218205,10.8479650318079));
#74085=CARTESIAN_POINT('Ctrl Pts',(89.2474929939635,64.501583341857,10.8913877953012));
#74086=CARTESIAN_POINT('Ctrl Pts',(89.2894934706362,64.4969946618936,10.9372470400611));
#74087=CARTESIAN_POINT('Ctrl Pts',(89.328859613144,64.4924059819301,10.9852498551265));
#74088=CARTESIAN_POINT('Ctrl Pts',(89.3695117432992,64.4876674019416,11.0348207950649));
#74089=CARTESIAN_POINT('Ctrl Pts',(89.4073540249063,64.482928821953,11.0866773847202));
#74090=CARTESIAN_POINT('Ctrl Pts',(89.4421367360521,64.4781902419644,11.1404609795789));
#74091=CARTESIAN_POINT('Ctrl Pts',(89.4758628999393,64.4735955993956,11.1926108630955));
#74092=CARTESIAN_POINT('Ctrl Pts',(89.5067125275981,64.4690009568268,11.2465718563188));
#74093=CARTESIAN_POINT('Ctrl Pts',(89.5345040421865,64.4644063142581,11.3019906616792));
#74094=CARTESIAN_POINT('Ctrl Pts',(89.5636015034866,64.4595957655596,11.3600136434472));
#74095=CARTESIAN_POINT('Ctrl Pts',(89.5893460680003,64.4547852168611,11.4196342673676));
#74096=CARTESIAN_POINT('Ctrl Pts',(89.6115863532925,64.4499746681626,11.4804249311541));
#74097=CARTESIAN_POINT('Ctrl Pts',(89.6338266385846,64.4451641194641,11.5412155949405));
#74098=CARTESIAN_POINT('Ctrl Pts',(89.6525625340892,64.4403535707656,11.6031756741928));
#74099=CARTESIAN_POINT('Ctrl Pts',(89.6677033646476,64.4355430220671,11.6658640266545));
#74100=CARTESIAN_POINT('Ctrl Pts',(89.6821577798346,64.4309505614424,11.7257103785685));
#74101=CARTESIAN_POINT('Ctrl Pts',(89.6933954589065,64.4263581008177,11.7864662781755));
#74102=CARTESIAN_POINT('Ctrl Pts',(89.7013086450358,64.4217656401929,11.8477535335518));
#74103=CARTESIAN_POINT('Ctrl Pts',(89.7093666998291,64.4170891042509,11.9101627899345));
#74104=CARTESIAN_POINT('Ctrl Pts',(89.7139770955883,64.4124125683089,11.9731225581595));
#74105=CARTESIAN_POINT('Ctrl Pts',(89.7150797883853,64.4077360323668,12.036218958769));
#74106=CARTESIAN_POINT('Ctrl Pts',(89.7161596377748,64.4031563756426,12.0980082530039));
#74107=CARTESIAN_POINT('Ctrl Pts',(89.7138757163543,64.3985767189185,12.1599280362992));
#74108=CARTESIAN_POINT('Ctrl Pts',(89.7082237910141,64.3939970621943,12.2215835428821));
#74109=CARTESIAN_POINT('Ctrl Pts',(89.7025753799761,64.389420253048,12.2832007127805));
#74110=CARTESIAN_POINT('Ctrl Pts',(89.6935631635928,64.3848434439016,12.3445534247203));
#74111=CARTESIAN_POINT('Ctrl Pts',(89.681234938173,64.3802666347553,12.4052492990506));
#74112=CARTESIAN_POINT('Ctrl Pts',(89.6689098239339,64.3756909806236,12.4659298560236));
#74113=CARTESIAN_POINT('Ctrl Pts',(89.653270463239,64.3711153264919,12.5259534045835));
#74114=CARTESIAN_POINT('Ctrl Pts',(89.6344158767858,64.3665396723601,12.5849371123748));
#74115=CARTESIAN_POINT('Ctrl Pts',(89.6148391340697,64.3617887644621,12.6461799762655));
#74116=CARTESIAN_POINT('Ctrl Pts',(89.5917959979519,64.3570378565641,12.7063011518721));
#74117=CARTESIAN_POINT('Ctrl Pts',(89.5654535786364,64.3522869486661,12.7648911985886));
#74118=CARTESIAN_POINT('Ctrl Pts',(89.5400509202948,64.3477055285353,12.8213910561425));
#74119=CARTESIAN_POINT('Ctrl Pts',(89.5115807307275,64.3431241084046,12.876466755529));
#74120=CARTESIAN_POINT('Ctrl Pts',(89.480240170224,64.3385426882738,12.9297755251222));
#74121=CARTESIAN_POINT('Ctrl Pts',(89.4488774219902,64.3339580247002,12.983122034966));
#74122=CARTESIAN_POINT('Ctrl Pts',(89.4146405440095,64.3293733611267,13.0346987031291));
#74123=CARTESIAN_POINT('Ctrl Pts',(89.3777694578984,64.3247886975532,13.0841925577003));
#74124=CARTESIAN_POINT('Ctrl Pts',(89.3408368947595,64.320196389738,13.1337689358798));
#74125=CARTESIAN_POINT('Ctrl Pts',(89.3012616941458,64.3156040819229,13.1812551876722));
#74126=CARTESIAN_POINT('Ctrl Pts',(89.259322423621,64.3110117741078,13.226373199572));
#74127=CARTESIAN_POINT('Ctrl Pts',(89.2548079329476,64.3105174419332,13.2312298611538));
#74128=CARTESIAN_POINT('Ctrl Pts',(89.2502660819866,64.3100231097585,13.2360591193132));
#74129=CARTESIAN_POINT('Ctrl Pts',(89.2456972411236,64.3095287775839,13.2408606548701));
#74130=CARTESIAN_POINT('Ctrl Pts',(89.203200857864,64.3049308215201,13.2855214126807));
#74131=CARTESIAN_POINT('Ctrl Pts',(89.1581911054405,64.3003328654562,13.3279649817505));
#74132=CARTESIAN_POINT('Ctrl Pts',(89.1109284721037,64.2957349093924,13.3678956148077));
#74133=CARTESIAN_POINT('Ctrl Pts',(89.0628651730352,64.2910590603802,13.408502703815));
#74134=CARTESIAN_POINT('Ctrl Pts',(89.0124722475177,64.2863832113681,13.4465104722219));
#74135=CARTESIAN_POINT('Ctrl Pts',(88.9600647117717,64.2817073623559,13.4816450856305));
#74136=CARTESIAN_POINT('Ctrl Pts',(88.9086719748842,64.2771220546404,13.5160993662382));
#74137=CARTESIAN_POINT('Ctrl Pts',(88.8553423955163,64.2725367469249,13.5477904729261));
#74138=CARTESIAN_POINT('Ctrl Pts',(88.8004063281201,64.2679514392094,13.5765007397297));
#74139=CARTESIAN_POINT('Ctrl Pts',(88.7455038702107,64.2633689367518,13.6051934418006));
#74140=CARTESIAN_POINT('Ctrl Pts',(88.6889973231742,64.2587864342942,13.6309086848791));
#74141=CARTESIAN_POINT('Ctrl Pts',(88.6312431891249,64.2542039318366,13.6534738492158));
#74142=CARTESIAN_POINT('Ctrl Pts',(88.5735031945594,64.2496225512765,13.6760334891035));
#74143=CARTESIAN_POINT('Ctrl Pts',(88.5145166930798,64.2450411707164,13.6954443961278));
#74144=CARTESIAN_POINT('Ctrl Pts',(88.4546598940543,64.2404597901563,13.7115821869502));
#74145=CARTESIAN_POINT('Ctrl Pts',(88.3926596453967,64.2357143520684,13.7282978660386));
#74146=CARTESIAN_POINT('Ctrl Pts',(88.3297261296616,64.2309689139804,13.7415013476342));
#74147=CARTESIAN_POINT('Ctrl Pts',(88.2662917545099,64.2262234758924,13.751111555856));
#74148=CARTESIAN_POINT('Ctrl Pts',(88.2049731094462,64.2216363126534,13.7604012342918));
#74149=CARTESIAN_POINT('Ctrl Pts',(88.1431870238345,64.2170491494143,13.7663335972473));
#74150=CARTESIAN_POINT('Ctrl Pts',(88.081329211241,64.2124619861752,13.7688883221299));
#74151=CARTESIAN_POINT('Ctrl Pts',(88.0162698984721,64.2076374106628,13.7715752688259));
#74152=CARTESIAN_POINT('Ctrl Pts',(87.9511318747261,64.2028128351504,13.7705254476601));
#74153=CARTESIAN_POINT('Ctrl Pts',(87.8863722166979,64.1979882596379,13.7657772651819));
#74154=CARTESIAN_POINT('Ctrl Pts',(87.8216125586697,64.1931636841255,13.7610290827036));
#74155=CARTESIAN_POINT('Ctrl Pts',(87.7572318972208,64.188339108613,13.7525826992389));
#74156=CARTESIAN_POINT('Ctrl Pts',(87.6936744123666,64.1835145331006,13.7405385355474));
#74157=CARTESIAN_POINT('Ctrl Pts',(87.6331015097317,64.1789165137888,13.7290599511402));
#74158=CARTESIAN_POINT('Ctrl Pts',(87.5730283945625,64.174318494477,13.7142670174428));
#74159=CARTESIAN_POINT('Ctrl Pts',(87.5138448271403,64.1697204751652,13.6962182583013));
#74160=CARTESIAN_POINT('Ctrl Pts',(87.4536595737528,64.165044634059,13.677864022665));
#74161=CARTESIAN_POINT('Ctrl Pts',(87.3943947979762,64.1603687929529,13.6561427314989));
#74162=CARTESIAN_POINT('Ctrl Pts',(87.3364513882402,64.1556929518467,13.6311705996385));
#74163=CARTESIAN_POINT('Ctrl Pts',(87.2796285339039,64.1511075358471,13.6066813985779));
#74164=CARTESIAN_POINT('Ctrl Pts',(87.2240768824105,64.1465221198475,13.5790661837745));
#74165=CARTESIAN_POINT('Ctrl Pts',(87.1701584656107,64.1419367038479,13.5484845191927));
#74166=CARTESIAN_POINT('Ctrl Pts',(87.1162728404869,64.1373540765703,13.5179214535255));
#74167=CARTESIAN_POINT('Ctrl Pts',(87.0640189221741,64.1327714492927,13.4843957659505));
#74168=CARTESIAN_POINT('Ctrl Pts',(87.0137350678613,64.1281888220151,13.4481134145672));
#74169=CARTESIAN_POINT('Ctrl Pts',(86.9634633440896,64.1236073002564,13.4118398159845));
#74170=CARTESIAN_POINT('Ctrl Pts',(86.9151611532857,64.1190257784977,13.3728111714002));
#74171=CARTESIAN_POINT('Ctrl Pts',(86.8691370058838,64.1144442567389,13.3312761509915));
#74172=CARTESIAN_POINT('Ctrl Pts',(86.8214672991706,64.1096989260621,13.2882560766833));
#74173=CARTESIAN_POINT('Ctrl Pts',(86.7762420968786,64.1049535953853,13.2425473434725));
#74174=CARTESIAN_POINT('Ctrl Pts',(86.7337639413596,64.1002082647085,13.1944692667985));
#74175=CARTESIAN_POINT('Ctrl Pts',(86.6927000151676,64.0956209207835,13.1479918581664));
#74176=CARTESIAN_POINT('Ctrl Pts',(86.6542033522433,64.0910335768584,13.0993008622936));
#74177=CARTESIAN_POINT('Ctrl Pts',(86.618505603288,64.0864462329333,13.0487177574084));
#74178=CARTESIAN_POINT('Ctrl Pts',(86.5809637246491,64.0816219088806,12.9955215520355));
#74179=CARTESIAN_POINT('Ctrl Pts',(86.5465181371553,64.076797584828,12.9402329811251));
#74180=CARTESIAN_POINT('Ctrl Pts',(86.5153843596422,64.0719732607754,12.8832568090369));
#74181=CARTESIAN_POINT('Ctrl Pts',(86.4842505821292,64.0671489367227,12.8262806369487));
#74182=CARTESIAN_POINT('Ctrl Pts',(86.456428821725,64.0623246126701,12.7676174804095));
#74183=CARTESIAN_POINT('Ctrl Pts',(86.4320755186073,64.0575002886174,12.7076948789408));
#74184=CARTESIAN_POINT('Ctrl Pts',(86.4060606507051,64.0523468130358,12.6436839086822));
#74185=CARTESIAN_POINT('Ctrl Pts',(86.3839120926027,64.0471933374543,12.5780148787507));
#74186=CARTESIAN_POINT('Ctrl Pts',(86.3658179547188,64.0420398618727,12.5111414084137));
#74187=CARTESIAN_POINT('Ctrl Pts',(86.34779236838,64.0369059107756,12.4445212952546));
#74188=CARTESIAN_POINT('Ctrl Pts',(86.3337906946726,64.0317719596785,12.3767061001825));
#74189=CARTESIAN_POINT('Ctrl Pts',(86.3239521898502,64.0266380085813,12.3081663103502));
#74190=CARTESIAN_POINT('Ctrl Pts',(86.3141736527811,64.0215353499945,12.2400442849331));
#74191=CARTESIAN_POINT('Ctrl Pts',(86.3085078171002,64.0164326914076,12.1712067393078));
#74192=CARTESIAN_POINT('Ctrl Pts',(86.30704307437,64.0113300328208,12.1021335190311));
#74193=CARTESIAN_POINT('Ctrl Pts',(86.3067947769097,64.0104650500891,12.0904244968143));
#74194=CARTESIAN_POINT('Ctrl Pts',(86.3066670851384,64.0096000673575,12.0787087386656));
#74195=CARTESIAN_POINT('Ctrl Pts',(86.3066602867323,64.0087350846259,12.0669886246394));
#74196=CARTESIAN_POINT('',(86.306660578502,63.2149850845225,12.064595746523));
#74197=CARTESIAN_POINT('Ctrl Pts',(86.3066602867319,64.0087350845702,12.0669886238853));
#74198=CARTESIAN_POINT('Ctrl Pts',(86.3066239196403,64.0041079808479,12.0042935188232));
#74199=CARTESIAN_POINT('Ctrl Pts',(86.3100513046104,63.9994808771256,11.9415921390125));
#74200=CARTESIAN_POINT('Ctrl Pts',(86.3169180933848,63.9948537734033,11.8792881115757));
#74201=CARTESIAN_POINT('Ctrl Pts',(86.3237866480857,63.9902254797324,11.8169680614621));
#74202=CARTESIAN_POINT('Ctrl Pts',(86.3340963066402,63.9855971860615,11.7550460578555));
#74203=CARTESIAN_POINT('Ctrl Pts',(86.347771042048,63.9809688923906,11.6939190020573));
#74204=CARTESIAN_POINT('Ctrl Pts',(86.3614647011323,63.9763341938915,11.6327073560576));
#74205=CARTESIAN_POINT('Ctrl Pts',(86.3785326224402,63.9716994953924,11.5722933369329));
#74206=CARTESIAN_POINT('Ctrl Pts',(86.3988481836135,63.9670647968932,11.513061163851));
#74207=CARTESIAN_POINT('Ctrl Pts',(86.4191791147488,63.9624265919618,11.453784178015));
#74208=CARTESIAN_POINT('Ctrl Pts',(86.4427623903478,63.9577883870304,11.3956912762091));
#74209=CARTESIAN_POINT('Ctrl Pts',(86.4694233889334,63.9531501820989,11.3391462404222));
#74210=CARTESIAN_POINT('Ctrl Pts',(86.4961384510343,63.948502571756,11.2824865418854));
#74211=CARTESIAN_POINT('Ctrl Pts',(86.5259434617493,63.943854961413,11.2273814113902));
#74212=CARTESIAN_POINT('Ctrl Pts',(86.5586184485326,63.93920735107,11.174168925997));
#74213=CARTESIAN_POINT('Ctrl Pts',(86.576713310441,63.9366335820914,11.1447007403976));
#74214=CARTESIAN_POINT('Ctrl Pts',(86.5956875624115,63.9340598131128,11.1158124513202));
#74215=CARTESIAN_POINT('Ctrl Pts',(86.615498525731,63.9314860441341,11.0875571192384));
#74216=CARTESIAN_POINT('Ctrl Pts',(86.6508855750261,63.9268886861838,11.0370864372678));
#74217=CARTESIAN_POINT('Ctrl Pts',(86.6890868020166,63.9222913282335,10.9884344196781));
#74218=CARTESIAN_POINT('Ctrl Pts',(86.7298886226617,63.9176939702831,10.9419321753318));
#74219=CARTESIAN_POINT('Ctrl Pts',(86.7713877196069,63.9130180465068,10.8946352381906));
#74220=CARTESIAN_POINT('Ctrl Pts',(86.8155769034407,63.9083421227304,10.8495627296339));
#74221=CARTESIAN_POINT('Ctrl Pts',(86.8621852912376,63.9036661989541,10.807032327448));
#74222=CARTESIAN_POINT('Ctrl Pts',(86.907884525315,63.899081484801,10.7653315328748));
#74223=CARTESIAN_POINT('Ctrl Pts',(86.9559090376499,63.894496770648,10.7260749207465));
#74224=CARTESIAN_POINT('Ctrl Pts',(87.0059645427723,63.8899120564949,10.6895267654926));
#74225=CARTESIAN_POINT('Ctrl Pts',(87.05598945735,63.8853301442096,10.6530009460034));
#74226=CARTESIAN_POINT('Ctrl Pts',(87.1080424933373,63.8807482319242,10.6191806008449));
#74227=CARTESIAN_POINT('Ctrl Pts',(87.1617968156538,63.8761663196389,10.5882893424975));
#74228=CARTESIAN_POINT('Ctrl Pts',(87.2155380274884,63.8715855248651,10.5574056184147));
#74229=CARTESIAN_POINT('Ctrl Pts',(87.270979260806,63.8670047300914,10.5294498164671));
#74230=CARTESIAN_POINT('Ctrl Pts',(87.3277670277041,63.8624239353176,10.5046007745718));
#74231=CARTESIAN_POINT('Ctrl Pts',(87.3866029714709,63.8576779240121,10.4788554968216));
#74232=CARTESIAN_POINT('Ctrl Pts',(87.4468839301898,63.8529319127065,10.4564456591323));
#74233=CARTESIAN_POINT('Ctrl Pts',(87.5081941086608,63.848185901401,10.4375157135439));
#74234=CARTESIAN_POINT('Ctrl Pts',(87.5674449113936,63.8435993060485,10.4192216145904));
#74235=CARTESIAN_POINT('Ctrl Pts',(87.6276563540583,63.839012710696,10.4041773813569));
#74236=CARTESIAN_POINT('Ctrl Pts',(87.6884402080479,63.8344261153436,10.3924618270814));
#74237=CARTESIAN_POINT('Ctrl Pts',(87.7523930518672,63.8296003960615,10.3801354778347));
#74238=CARTESIAN_POINT('Ctrl Pts',(87.8169789902477,63.8247746767794,10.371494489716));
#74239=CARTESIAN_POINT('Ctrl Pts',(87.8817399184812,63.8199489574973,10.3665687225057));
#74240=CARTESIAN_POINT('Ctrl Pts',(87.9465008467147,63.8151232382152,10.3616429552955));
#74241=CARTESIAN_POINT('Ctrl Pts',(88.0114361157952,63.8102975189331,10.3604323437773));
#74242=CARTESIAN_POINT('Ctrl Pts',(88.0760911879079,63.8054717996509,10.3629034164626));
#74243=CARTESIAN_POINT('Ctrl Pts',(88.1376859515102,63.8008744953919,10.3652575262474));
#74244=CARTESIAN_POINT('Ctrl Pts',(88.1992792246782,63.7962771911329,10.3709622604175));
#74245=CARTESIAN_POINT('Ctrl Pts',(88.2604769952076,63.7916798868738,10.3800177745711));
#74246=CARTESIAN_POINT('Ctrl Pts',(88.3227214116909,63.7870039563861,10.3892281622955));
#74247=CARTESIAN_POINT('Ctrl Pts',(88.3845561365458,63.7823280258983,10.4019050968116));
#74248=CARTESIAN_POINT('Ctrl Pts',(88.445567347191,63.7776520954106,10.4179933081582));
#74249=CARTESIAN_POINT('Ctrl Pts',(88.5053877157701,63.7730674316698,10.4337675031357));
#74250=CARTESIAN_POINT('Ctrl Pts',(88.5644159129872,63.768482767929,10.4528208698359));
#74251=CARTESIAN_POINT('Ctrl Pts',(88.6222703039524,63.7638981041882,10.4750495133079));
#74252=CARTESIAN_POINT('Ctrl Pts',(88.6800893551115,63.7593162409457,10.4972645786238));
#74253=CARTESIAN_POINT('Ctrl Pts',(88.7367355475692,63.7547343777033,10.5226508925969));
#74254=CARTESIAN_POINT('Ctrl Pts',(88.7918437532103,63.7501525144609,10.5510551598581));
#74255=CARTESIAN_POINT('Ctrl Pts',(88.8469385355215,63.7455717672748,10.5794525083703));
#74256=CARTESIAN_POINT('Ctrl Pts',(88.900495622447,63.7409910200887,10.6108661177419));
#74257=CARTESIAN_POINT('Ctrl Pts',(88.952173046271,63.7364102729026,10.6450960157094));
#74258=CARTESIAN_POINT('Ctrl Pts',(89.0057154345313,63.7316642130914,10.6805612218181));
#74259=CARTESIAN_POINT('Ctrl Pts',(89.0572393760856,63.7269181532801,10.719049608478));
#74260=CARTESIAN_POINT('Ctrl Pts',(89.1063979774428,63.7221720934689,10.7602901905039));
#74261=CARTESIAN_POINT('Ctrl Pts',(89.1539044331854,63.7175855414892,10.8001447394684));
#74262=CARTESIAN_POINT('Ctrl Pts',(89.1992016919601,63.7129989895095,10.8425689986601));
#74263=CARTESIAN_POINT('Ctrl Pts',(89.2420129780526,63.7084124375298,10.8872795566946));
#74264=CARTESIAN_POINT('Ctrl Pts',(89.2870575546779,63.7035866238028,10.9343224825483));
#74265=CARTESIAN_POINT('Ctrl Pts',(89.329349261722,63.6987608100758,10.983896292323));
#74266=CARTESIAN_POINT('Ctrl Pts',(89.3686145299541,63.6939349963488,11.0356322871627));
#74267=CARTESIAN_POINT('Ctrl Pts',(89.4078797981862,63.6891091826218,11.0873682820025));
#74268=CARTESIAN_POINT('Ctrl Pts',(89.4441183303605,63.6842833688948,11.1412658811746));
#74269=CARTESIAN_POINT('Ctrl Pts',(89.4771117056078,63.6794575551678,11.1969250306909));
#74270=CARTESIAN_POINT('Ctrl Pts',(89.5085417152874,63.6748604088917,11.2499468144563));
#74271=CARTESIAN_POINT('Ctrl Pts',(89.5371562642813,63.6702632626157,11.3047846688));
#74272=CARTESIAN_POINT('Ctrl Pts',(89.5627414986066,63.6656661163397,11.3611076982246));
#74273=CARTESIAN_POINT('Ctrl Pts',(89.5887653132273,63.660990166104,11.4183962130762));
#74274=CARTESIAN_POINT('Ctrl Pts',(89.6116546258482,63.6563142158684,11.4772208925681));
#74275=CARTESIAN_POINT('Ctrl Pts',(89.6312313783171,63.6516382656328,11.5372040882185));
#74276=CARTESIAN_POINT('Ctrl Pts',(89.6504252492963,63.6470537674801,11.5960141344746));
#74277=CARTESIAN_POINT('Ctrl Pts',(89.6664348019616,63.6424692693275,11.6559372812805));
#74278=CARTESIAN_POINT('Ctrl Pts',(89.6791403089382,63.6378847711749,11.7165965866001));
#74279=CARTESIAN_POINT('Ctrl Pts',(89.6918380480151,63.6333030758952,11.777218806001));
#74280=CARTESIAN_POINT('Ctrl Pts',(89.7012356426772,63.6287213806155,11.8385757942671));
#74281=CARTESIAN_POINT('Ctrl Pts',(89.7072638202796,63.6241396853358,11.9002776792029));
#74282=CARTESIAN_POINT('Ctrl Pts',(89.7132905267104,63.6195591082149,11.9619645058468));
#74283=CARTESIAN_POINT('Ctrl Pts',(89.7159493989979,63.614978531094,12.0239955556393));
#74284=CARTESIAN_POINT('Ctrl Pts',(89.7152229405887,63.6103979539731,12.085975093775));
#74285=CARTESIAN_POINT('Ctrl Pts',(89.7144702119392,63.6056517336991,12.1501959403432));
#74286=CARTESIAN_POINT('Ctrl Pts',(89.7100825619892,63.600905513425,12.2143608961065));
#74287=CARTESIAN_POINT('Ctrl Pts',(89.7020994909172,63.596159293151,12.2780314774261));
#74288=CARTESIAN_POINT('Ctrl Pts',(89.6943852710916,63.5915729145249,12.339557781814));
#74289=CARTESIAN_POINT('Ctrl Pts',(89.6833141320636,63.5869865358989,12.4006219767003));
#74290=CARTESIAN_POINT('Ctrl Pts',(89.6689740403695,63.5824001572728,12.4608378364098));
#74291=CARTESIAN_POINT('Ctrl Pts',(89.6538842905872,63.5775740161748,12.5242016052985));
#74292=CARTESIAN_POINT('Ctrl Pts',(89.6351745986117,63.5727478750768,12.5866252872646));
#74293=CARTESIAN_POINT('Ctrl Pts',(89.6130063747922,63.5679217339787,12.6476789584687));
#74294=CARTESIAN_POINT('Ctrl Pts',(89.5908381509727,63.5630955928807,12.7087326296728));
#74295=CARTESIAN_POINT('Ctrl Pts',(89.5652117221723,63.5582694517826,12.7684157250627));
#74296=CARTESIAN_POINT('Ctrl Pts',(89.5363447766494,63.5534433106846,12.8263276582818));
#74297=CARTESIAN_POINT('Ctrl Pts',(89.5088469416784,63.5488460653212,12.8814929261572));
#74298=CARTESIAN_POINT('Ctrl Pts',(89.4782961644025,63.5442488199578,12.9352777815762));
#74299=CARTESIAN_POINT('Ctrl Pts',(89.4448544642557,63.5396515745944,12.9873230763061));
#74300=CARTESIAN_POINT('Ctrl Pts',(89.4108403320712,63.5349756367447,13.0402592466189));
#74301=CARTESIAN_POINT('Ctrl Pts',(89.3738355276833,63.530299698895,13.0913952257273));
#74302=CARTESIAN_POINT('Ctrl Pts',(89.3340607475308,63.5256237610453,13.1403766071277));
#74303=CARTESIAN_POINT('Ctrl Pts',(89.2950629069714,63.5210391605012,13.1884012120384));
#74304=CARTESIAN_POINT('Ctrl Pts',(89.2534026684274,63.5164545599571,13.2343542219115));
#74305=CARTESIAN_POINT('Ctrl Pts',(89.2093317869495,63.511869959413,13.2779305937166));
#74306=CARTESIAN_POINT('Ctrl Pts',(89.1652878398618,63.5072881607965,13.3214803333565));
#74307=CARTESIAN_POINT('Ctrl Pts',(89.1188365323839,63.50270636218,13.3626559578748));
#74308=CARTESIAN_POINT('Ctrl Pts',(89.0702678479934,63.4981245635635,13.4011878002017));
#74309=CARTESIAN_POINT('Ctrl Pts',(89.0217110082514,63.4935438823294,13.4397102456068));
#74310=CARTESIAN_POINT('Ctrl Pts',(88.971038215284,63.4889632010953,13.4755898725143));
#74311=CARTESIAN_POINT('Ctrl Pts',(88.9185724602104,63.4843825198612,13.5085973329615));
#74312=CARTESIAN_POINT('Ctrl Pts',(88.8642118058735,63.4796363987229,13.5427969198233));
#74313=CARTESIAN_POINT('Ctrl Pts',(88.8079266560086,63.4748902775846,13.5739125378752));
#74314=CARTESIAN_POINT('Ctrl Pts',(88.7501067800997,63.4701441564462,13.6017395622991));
#74315=CARTESIAN_POINT('Ctrl Pts',(88.6942316986764,63.465557672977,13.6286306137068));
#74316=CARTESIAN_POINT('Ctrl Pts',(88.6369240162277,63.4609711895078,13.6524506638998));
#74317=CARTESIAN_POINT('Ctrl Pts',(88.5785559360207,63.4563847060386,13.6730641228923));
#74318=CARTESIAN_POINT('Ctrl Pts',(88.5171405066834,63.4515587660657,13.6947537935079));
#74319=CARTESIAN_POINT('Ctrl Pts',(88.4545515346259,63.4467328260928,13.7128926772634));
#74320=CARTESIAN_POINT('Ctrl Pts',(88.3912376859154,63.4419068861199,13.7273832001708));
#74321=CARTESIAN_POINT('Ctrl Pts',(88.3279238372049,63.4370809461471,13.7418737230782));
#74322=CARTESIAN_POINT('Ctrl Pts',(88.2638857636009,63.4322550061742,13.7527158532581));
#74323=CARTESIAN_POINT('Ctrl Pts',(88.1995780088928,63.4274290662013,13.759875193207));
#74324=CARTESIAN_POINT('Ctrl Pts',(88.1383178995474,63.4228318350933,13.7666952408063));
#74325=CARTESIAN_POINT('Ctrl Pts',(88.0765615899772,63.4182346039852,13.7702017341098));
#74326=CARTESIAN_POINT('Ctrl Pts',(88.0146986851029,63.4136373728772,13.7703359866319));
#74327=CARTESIAN_POINT('Ctrl Pts',(87.9517766344529,63.4089614332456,13.7704725376718));
#74328=CARTESIAN_POINT('Ctrl Pts',(87.88874482066,63.4042854936139,13.7671201368571));
#74329=CARTESIAN_POINT('Ctrl Pts',(87.8260206957689,63.3996095539823,13.7602719653604));
#74330=CARTESIAN_POINT('Ctrl Pts',(87.7645220040835,63.3950249675852,13.7535575857144));
#74331=CARTESIAN_POINT('Ctrl Pts',(87.7033196171185,63.3904403811881,13.7434828577989));
#74332=CARTESIAN_POINT('Ctrl Pts',(87.6428063576431,63.385855794791,13.7300938306862));
#74333=CARTESIAN_POINT('Ctrl Pts',(87.5823300805425,63.3812740102409,13.7167129862103));
#74334=CARTESIAN_POINT('Ctrl Pts',(87.522542591832,63.3766922256908,13.7000219685882));
#74335=CARTESIAN_POINT('Ctrl Pts',(87.463827729285,63.3721104411407,13.6801181312905));
#74336=CARTESIAN_POINT('Ctrl Pts',(87.4051271844849,63.3675297738687,13.6602191475867));
#74337=CARTESIAN_POINT('Ctrl Pts',(87.3474992284899,63.3629491065967,13.6371090628348));
#74338=CARTESIAN_POINT('Ctrl Pts',(87.2913117294407,63.3583684393247,13.6109348299587));
#74339=CARTESIAN_POINT('Ctrl Pts',(87.2330945683247,63.3536223045241,13.5838151047845));
#74340=CARTESIAN_POINT('Ctrl Pts',(87.1764244778286,63.3488761697236,13.55340580834));
#74341=CARTESIAN_POINT('Ctrl Pts',(87.1216847825832,63.344130034923,13.5199234091488));
#74342=CARTESIAN_POINT('Ctrl Pts',(87.0687865871181,63.3395435649901,13.4875673923841));
#74343=CARTESIAN_POINT('Ctrl Pts',(87.0176913535797,63.3349570950571,13.4523421268085));
#74344=CARTESIAN_POINT('Ctrl Pts',(86.9687148743522,63.3303706251242,13.4144867639148));
#74345=CARTESIAN_POINT('Ctrl Pts',(86.9171809305,63.3255446578898,13.3746546613088));
#74346=CARTESIAN_POINT('Ctrl Pts',(86.8679935764349,63.3207186906555,13.3319106662234));
#74347=CARTESIAN_POINT('Ctrl Pts',(86.8214781474381,63.3158927234211,13.2865787962592));
#74348=CARTESIAN_POINT('Ctrl Pts',(86.7749627184413,63.3110667561868,13.2412469262951));
#74349=CARTESIAN_POINT('Ctrl Pts',(86.7311195948234,63.3062407889525,13.1933277117473));
#74350=CARTESIAN_POINT('Ctrl Pts',(86.6902242220587,63.3014148217181,13.1431843760488));
#74351=CARTESIAN_POINT('Ctrl Pts',(86.6514214335936,63.2968357954598,13.0956068356938));
#74352=CARTESIAN_POINT('Ctrl Pts',(86.6151082745464,63.2922567692015,13.0458263197573));
#74353=CARTESIAN_POINT('Ctrl Pts',(86.5815453095547,63.2876777429431,12.9941347550674));
#74354=CARTESIAN_POINT('Ctrl Pts',(86.5480322635142,63.2831055271733,12.9425200724017));
#74355=CARTESIAN_POINT('Ctrl Pts',(86.5172615811686,63.2785333114035,12.8890004005237));
#74356=CARTESIAN_POINT('Ctrl Pts',(86.4894535277513,63.2739610956337,12.8339004938059));
#74357=CARTESIAN_POINT('Ctrl Pts',(86.4616764260128,63.2693939689563,12.7788619158907));
#74358=CARTESIAN_POINT('Ctrl Pts',(86.4368556441183,63.2648268422789,12.7222470465303));
#74359=CARTESIAN_POINT('Ctrl Pts',(86.4151669271033,63.2602597156015,12.6644075860558));
#74360=CARTESIAN_POINT('Ctrl Pts',(86.3934918302003,63.255695456995,12.6066044476898));
#74361=CARTESIAN_POINT('Ctrl Pts',(86.3749450801124,63.2511311983884,12.5475787214813));
#74362=CARTESIAN_POINT('Ctrl Pts',(86.3596546020395,63.2465669397819,12.4877027534112));
#74363=CARTESIAN_POINT('Ctrl Pts',(86.3443695284116,63.2420042944202,12.4278479486022));
#74364=CARTESIAN_POINT('Ctrl Pts',(86.3323385650718,63.2374416490585,12.3671439962651));
#74365=CARTESIAN_POINT('Ctrl Pts',(86.3236393684921,63.2328790036969,12.3059769464703));
#74366=CARTESIAN_POINT('Ctrl Pts',(86.3149375352517,63.2283149754319,12.2447913574053));
#74367=CARTESIAN_POINT('Ctrl Pts',(86.3095695536903,63.2237509471669,12.1831428992014));
#74368=CARTESIAN_POINT('Ctrl Pts',(86.3075614321109,63.2191869189019,12.1214245525729));
#74369=CARTESIAN_POINT('Ctrl Pts',(86.3069451786826,63.217786307458,12.1024843932294));
#74370=CARTESIAN_POINT('Ctrl Pts',(86.3066449717231,63.2163856960141,12.0835376691406));
#74371=CARTESIAN_POINT('Ctrl Pts',(86.3066605785015,63.2149850845702,12.0645957471688));
#74372=CARTESIAN_POINT('',(86.306660007507,62.4212350846317,12.0658400339999));
#74373=CARTESIAN_POINT('Ctrl Pts',(86.306660578502,63.2149850845225,12.064595746523));
#74374=CARTESIAN_POINT('Ctrl Pts',(86.306721132394,63.2095507512284,11.9911016181765));
#74375=CARTESIAN_POINT('Ctrl Pts',(86.3115393780642,63.2041164179344,11.9178111520133));
#74376=CARTESIAN_POINT('Ctrl Pts',(86.3210134498976,63.1986820846404,11.8452732547402));
#74377=CARTESIAN_POINT('Ctrl Pts',(86.3306070180728,63.1931792081729,11.7718204379349));
#74378=CARTESIAN_POINT('Ctrl Pts',(86.3449745067232,63.1876763317055,11.6991393584463));
#74379=CARTESIAN_POINT('Ctrl Pts',(86.36396116775,63.182173455238,11.6277786852962));
#74380=CARTESIAN_POINT('Ctrl Pts',(86.3717506901681,63.179915829237,11.5985020493209));
#74381=CARTESIAN_POINT('Ctrl Pts',(86.380317132937,63.1776582032359,11.5694474071227));
#74382=CARTESIAN_POINT('Ctrl Pts',(86.389647512673,63.1754005772349,11.5406515942363));
#74383=CARTESIAN_POINT('Ctrl Pts',(86.4086470601855,63.1708033503603,11.4820143864718));
#74384=CARTESIAN_POINT('Ctrl Pts',(86.4308706862237,63.1662061234857,11.424288837461));
#74385=CARTESIAN_POINT('Ctrl Pts',(86.4562115126177,63.1616088966111,11.3678541734685));
#74386=CARTESIAN_POINT('Ctrl Pts',(86.481986222258,63.1569329564503,11.3104532404665));
#74387=CARTESIAN_POINT('Ctrl Pts',(86.5109858086307,63.1522570162895,11.2543883470906));
#74388=CARTESIAN_POINT('Ctrl Pts',(86.5430446607671,63.1475810761287,11.2000427506986));
#74389=CARTESIAN_POINT('Ctrl Pts',(86.5744771476656,63.142996494397,11.1467589575261));
#74390=CARTESIAN_POINT('Ctrl Pts',(86.6088501606325,63.1384119126653,11.0951283417784));
#74391=CARTESIAN_POINT('Ctrl Pts',(86.6459600448921,63.1338273309337,11.0454899527397));
#74392=CARTESIAN_POINT('Ctrl Pts',(86.6830472484086,63.1292455511973,10.9958819015901));
#74393=CARTESIAN_POINT('Ctrl Pts',(86.7228677022946,63.1246637714609,10.9482640696739));
#74394=CARTESIAN_POINT('Ctrl Pts',(86.765174693131,63.1200819917245,10.9029462005716));
#74395=CARTESIAN_POINT('Ctrl Pts',(86.807471366005,63.115501329407,10.8576393837342));
#74396=CARTESIAN_POINT('Ctrl Pts',(86.8522530247635,63.1109206670895,10.8146317881271));
#74397=CARTESIAN_POINT('Ctrl Pts',(86.899234326083,63.106340004772,10.77419818784));
#74398=CARTESIAN_POINT('Ctrl Pts',(86.9479128329776,63.101593865437,10.7323039185229));
#74399=CARTESIAN_POINT('Ctrl Pts',(86.9989525509673,63.096847726102,10.6931736046698));
#74400=CARTESIAN_POINT('Ctrl Pts',(87.0519984186674,63.0921015867669,10.6570674953705));
#74401=CARTESIAN_POINT('Ctrl Pts',(87.1032596610378,63.0875151220841,10.6221761060862));
#74402=CARTESIAN_POINT('Ctrl Pts',(87.1563937126347,63.0829286574012,10.5901088635486));
#74403=CARTESIAN_POINT('Ctrl Pts',(87.2110526384385,63.0783421927184,10.5610551324614));
#74404=CARTESIAN_POINT('Ctrl Pts',(87.2685659342977,63.0735162160573,10.5304841725082));
#74405=CARTESIAN_POINT('Ctrl Pts',(87.3277671532957,63.0686902393961,10.5032503734019));
#74406=CARTESIAN_POINT('Ctrl Pts',(87.3882270847903,63.063864262735,10.4795168668778));
#74407=CARTESIAN_POINT('Ctrl Pts',(87.4486870162849,63.0590382860739,10.4557833603537));
#74408=CARTESIAN_POINT('Ctrl Pts',(87.5104050204361,63.0542123094127,10.4355502747426));
#74409=CARTESIAN_POINT('Ctrl Pts',(87.5729366906525,63.0493863327516,10.4189191359853));
#74410=CARTESIAN_POINT('Ctrl Pts',(87.6325043444477,63.0447891085614,10.4030763172617));
#74411=CARTESIAN_POINT('Ctrl Pts',(87.6930548305815,63.0401918843712,10.3904365935124));
#74412=CARTESIAN_POINT('Ctrl Pts',(87.7542115829353,63.0355946601809,10.3811158661613));
#74413=CARTESIAN_POINT('Ctrl Pts',(87.816415496237,63.0309187196846,10.371635543977));
#74414=CARTESIAN_POINT('Ctrl Pts',(87.879246144788,63.0262427791882,10.3655891755679));
#74415=CARTESIAN_POINT('Ctrl Pts',(87.9422917184275,63.0215668386919,10.3630455062911));
#74416=CARTESIAN_POINT('Ctrl Pts',(88.0041054679006,63.016982259669,10.3605515368283));
#74417=CARTESIAN_POINT('Ctrl Pts',(88.0661252863284,63.0123976806461,10.3614246431067));
#74418=CARTESIAN_POINT('Ctrl Pts',(88.1279558695297,63.0078131016232,10.3656776305116));
#74419=CARTESIAN_POINT('Ctrl Pts',(88.1897486631999,63.0032313245971,10.3699280185816));
#74420=CARTESIAN_POINT('Ctrl Pts',(88.2513519441803,62.9986495475709,10.3775541569119));
#74421=CARTESIAN_POINT('Ctrl Pts',(88.3123716736544,62.9940677705448,10.3885167810321));
#74422=CARTESIAN_POINT('Ctrl Pts',(88.3733765214763,62.9894871109344,10.3994767315588));
#74423=CARTESIAN_POINT('Ctrl Pts',(88.4337975995137,62.9849064513241,10.4137714625632));
#74424=CARTESIAN_POINT('Ctrl Pts',(88.4932492947337,62.9803257917138,10.4313102883639));
#74425=CARTESIAN_POINT('Ctrl Pts',(88.5548487605118,62.97557964976,10.4494827272776));
#74426=CARTESIAN_POINT('Ctrl Pts',(88.6154068862498,62.9708335078062,10.4711380400035));
#74427=CARTESIAN_POINT('Ctrl Pts',(88.6745124453264,62.9660873658525,10.4961190903457));
#74428=CARTESIAN_POINT('Ctrl Pts',(88.7316294477733,62.9615009038373,10.5202596743417));
#74429=CARTESIAN_POINT('Ctrl Pts',(88.7873896358226,62.9569144418222,10.5475054553707));
#74430=CARTESIAN_POINT('Ctrl Pts',(88.8414452010442,62.9523279798071,10.5776668371421));
#74431=CARTESIAN_POINT('Ctrl Pts',(88.8983237230385,62.947501997884,10.6094033440018));
#74432=CARTESIAN_POINT('Ctrl Pts',(88.9533141489289,62.9426760159609,10.6443679899557));
#74433=CARTESIAN_POINT('Ctrl Pts',(89.0060466236306,62.9378500340378,10.6822886672426));
#74434=CARTESIAN_POINT('Ctrl Pts',(89.0587790983324,62.9330240521147,10.7202093445295));
#74435=CARTESIAN_POINT('Ctrl Pts',(89.10925316698,62.9281980701916,10.7610855852075));
#74436=CARTESIAN_POINT('Ctrl Pts',(89.1571424888919,62.9233720882684,10.8045990999065));
#74437=CARTESIAN_POINT('Ctrl Pts',(89.2027617782286,62.9187748658211,10.8460500024847));
#74438=CARTESIAN_POINT('Ctrl Pts',(89.2462231695869,62.9141776433737,10.8900639566383));
#74439=CARTESIAN_POINT('Ctrl Pts',(89.2872250427154,62.9095804209263,10.9363874664532));
#74440=CARTESIAN_POINT('Ctrl Pts',(89.328928991157,62.9049044802121,10.9835041739972));
#74441=CARTESIAN_POINT('Ctrl Pts',(89.3680879435471,62.9002285394979,11.0330099884105));
#74442=CARTESIAN_POINT('Ctrl Pts',(89.4044207797161,62.8955525987837,11.0845962266961));
#74443=CARTESIAN_POINT('Ctrl Pts',(89.4400437060474,62.8909680216035,11.1351745178484));
#74444=CARTESIAN_POINT('Ctrl Pts',(89.472949655108,62.8863834444233,11.1877522288493));
#74445=CARTESIAN_POINT('Ctrl Pts',(89.5029134562567,62.8817988672431,11.2420042022922));
#74446=CARTESIAN_POINT('Ctrl Pts',(89.5328589439531,62.8772170920918,11.2962230176948));
#74447=CARTESIAN_POINT('Ctrl Pts',(89.5598656037087,62.8726353169405,11.3521136218362));
#74448=CARTESIAN_POINT('Ctrl Pts',(89.5837526961807,62.8680535417892,11.4093236777099));
#74449=CARTESIAN_POINT('Ctrl Pts',(89.6076339628515,62.8634728840828,11.4665197806754));
#74450=CARTESIAN_POINT('Ctrl Pts',(89.6283969765519,62.8588922263765,11.5250342270168));
#74451=CARTESIAN_POINT('Ctrl Pts',(89.6459087681079,62.8543115686701,11.584493867574));
#74452=CARTESIAN_POINT('Ctrl Pts',(89.6640532105012,62.8495654249297,11.6461016145237));
#74453=CARTESIAN_POINT('Ctrl Pts',(89.6787067925887,62.8448192811893,11.7087236179717));
#74454=CARTESIAN_POINT('Ctrl Pts',(89.6897784786873,62.8400731374489,11.7719291665323));
#74455=CARTESIAN_POINT('Ctrl Pts',(89.7004776586677,62.8354866773885,11.8330081687542));
#74456=CARTESIAN_POINT('Ctrl Pts',(89.7078321649599,62.8309002173282,11.8946315377005));
#74457=CARTESIAN_POINT('Ctrl Pts',(89.7118126304884,62.8263137572678,11.9564042356148));
#74458=CARTESIAN_POINT('Ctrl Pts',(89.7160009737839,62.8214877716874,12.0214029809383));
#74459=CARTESIAN_POINT('Ctrl Pts',(89.716453181955,62.816661786107,12.0865664362988));
#74460=CARTESIAN_POINT('Ctrl Pts',(89.7131972496079,62.8118358005265,12.1514362863616));
#74461=CARTESIAN_POINT('Ctrl Pts',(89.7099413172608,62.8070098149461,12.2163061364244));
#74462=CARTESIAN_POINT('Ctrl Pts',(89.7029773908056,62.8021838293657,12.2808817452318));
#74463=CARTESIAN_POINT('Ctrl Pts',(89.6923958654503,62.7973578437852,12.3447163060295));
#74464=CARTESIAN_POINT('Ctrl Pts',(89.6823159258857,62.7927606197219,12.4055249790108));
#74465=CARTESIAN_POINT('Ctrl Pts',(89.6689122687689,62.7881633956585,12.4659109509055));
#74466=CARTESIAN_POINT('Ctrl Pts',(89.6522342632398,62.7835661715951,12.5254833280629));
#74467=CARTESIAN_POINT('Ctrl Pts',(89.6352706868203,62.7788902310829,12.5860757394659));
#74468=CARTESIAN_POINT('Ctrl Pts',(89.6149195688735,62.7742142905707,12.6458258934939));
#74469=CARTESIAN_POINT('Ctrl Pts',(89.5912877614663,62.7695383500585,12.7043301861575));
#74470=CARTESIAN_POINT('Ctrl Pts',(89.5681176881313,62.7649537712021,12.7616913827882));
#74471=CARTESIAN_POINT('Ctrl Pts',(89.541794172757,62.7603691923457,12.8178544705603));
#74472=CARTESIAN_POINT('Ctrl Pts',(89.5124682549575,62.7557846134893,12.8724539137204));
#74473=CARTESIAN_POINT('Ctrl Pts',(89.4831602606247,62.751202836644,12.9270199866956));
#74474=CARTESIAN_POINT('Ctrl Pts',(89.4508537428031,62.7466210597986,12.9800238624931));
#74475=CARTESIAN_POINT('Ctrl Pts',(89.4157466747345,62.7420392829533,13.0311225908777));
#74476=CARTESIAN_POINT('Ctrl Pts',(89.3806481687782,62.7374586235379,13.0822088570124));
#74477=CARTESIAN_POINT('Ctrl Pts',(89.3427507565923,62.7328779641225,13.1313904787341));
#74478=CARTESIAN_POINT('Ctrl Pts',(89.3022958066175,62.7282973047071,13.17835335007));
#74479=CARTESIAN_POINT('Ctrl Pts',(89.260379365226,62.72355116259,13.2270128205465));
#74480=CARTESIAN_POINT('Ctrl Pts',(89.2157173897576,62.7188050204729,13.2732896781071));
#74481=CARTESIAN_POINT('Ctrl Pts',(89.1686223518987,62.7140588783558,13.3168738249657));
#74482=CARTESIAN_POINT('Ctrl Pts',(89.1231117906529,62.7094724165687,13.3589916164601));
#74483=CARTESIAN_POINT('Ctrl Pts',(89.0753297472791,62.7048859547816,13.398594738683));
#74484=CARTESIAN_POINT('Ctrl Pts',(89.0255921728988,62.7002994929946,13.4354442516191));
#74485=CARTESIAN_POINT('Ctrl Pts',(88.9732571347242,62.6954735107125,13.4742181703365));
#74486=CARTESIAN_POINT('Ctrl Pts',(88.9187572485301,62.6906475284304,13.509942625556));
#74487=CARTESIAN_POINT('Ctrl Pts',(88.8624927379216,62.6858215461483,13.54239254701));
#74488=CARTESIAN_POINT('Ctrl Pts',(88.8062282273131,62.6809955638662,13.5748424684641));
#74489=CARTESIAN_POINT('Ctrl Pts',(88.7481997059805,62.6761695815841,13.6040176342137));
#74490=CARTESIAN_POINT('Ctrl Pts',(88.6888315748493,62.671343599302,13.6297516400431));
#74491=CARTESIAN_POINT('Ctrl Pts',(88.6322775804682,62.6667463756794,13.6542658161396));
#74492=CARTESIAN_POINT('Ctrl Pts',(88.5742759260267,62.6621491520569,13.6757583949161));
#74493=CARTESIAN_POINT('Ctrl Pts',(88.5151817872298,62.6575519284343,13.6940588321758));
#74494=CARTESIAN_POINT('Ctrl Pts',(88.4550757964022,62.652875987867,13.7126726225867));
#74495=CARTESIAN_POINT('Ctrl Pts',(88.3938400052592,62.6482000472997,13.7279836282808));
#74496=CARTESIAN_POINT('Ctrl Pts',(88.331871446533,62.6435241067324,13.7398627035691));
#74497=CARTESIAN_POINT('Ctrl Pts',(88.271113677649,62.6389395283245,13.751509676256));
#74498=CARTESIAN_POINT('Ctrl Pts',(88.2096520422967,62.6343549499166,13.7598575234163));
#74499=CARTESIAN_POINT('Ctrl Pts',(88.1478755584302,62.6297703715087,13.764834870464));
#74500=CARTESIAN_POINT('Ctrl Pts',(88.0861368312507,62.6251885951134,13.7698091754458));
#74501=CARTESIAN_POINT('Ctrl Pts',(88.0240841434678,62.6206068187182,13.7714170241801));
#74502=CARTESIAN_POINT('Ctrl Pts',(87.9621129952099,62.616025042323,13.7696387223712));
#74503=CARTESIAN_POINT('Ctrl Pts',(87.9001569608432,62.6114443833586,13.7678608542651));
#74504=CARTESIAN_POINT('Ctrl Pts',(87.8382829351339,62.6068637243942,13.7626984896173));
#74505=CARTESIAN_POINT('Ctrl Pts',(87.7768857230408,62.6022830654298,13.7541840364498));
#74506=CARTESIAN_POINT('Ctrl Pts',(87.7132704390637,62.5975369228789,13.745361985127));
#74507=CARTESIAN_POINT('Ctrl Pts',(87.6501676643083,62.592790780328,13.732941025464));
#74508=CARTESIAN_POINT('Ctrl Pts',(87.5880074029217,62.588044637777,13.7170154749175));
#74509=CARTESIAN_POINT('Ctrl Pts',(87.5279384874551,62.5834581764378,13.7016257302767));
#74510=CARTESIAN_POINT('Ctrl Pts',(87.468750149575,62.5788717150986,13.6829637124893));
#74511=CARTESIAN_POINT('Ctrl Pts',(87.4108144992807,62.5742852537594,13.6611652579988));
#74512=CARTESIAN_POINT('Ctrl Pts',(87.3498532370308,62.5694592706027,13.6382284083373));
#74513=CARTESIAN_POINT('Ctrl Pts',(87.2902796832104,62.5646332874459,13.6118187974817));
#74514=CARTESIAN_POINT('Ctrl Pts',(87.232500005162,62.5598073042891,13.5821505840903));
#74515=CARTESIAN_POINT('Ctrl Pts',(87.1747203271136,62.5549813211323,13.5524823706988));
#74516=CARTESIAN_POINT('Ctrl Pts',(87.1187350441588,62.5501553379755,13.5195559499669));
#74517=CARTESIAN_POINT('Ctrl Pts',(87.0649141507492,62.5453293548187,13.4836376128783));
#74518=CARTESIAN_POINT('Ctrl Pts',(87.0137790463661,62.5407441995595,13.449511685196));
#74519=CARTESIAN_POINT('Ctrl Pts',(86.9643850283897,62.5361590443002,13.4125435669695));
#74520=CARTESIAN_POINT('Ctrl Pts',(86.9170670094507,62.531573889041,13.3729374307089));
#74521=CARTESIAN_POINT('Ctrl Pts',(86.8696221089916,62.5269764388573,13.3332250920566));
#74522=CARTESIAN_POINT('Ctrl Pts',(86.8242648202487,62.5223789886736,13.290860805712));
#74523=CARTESIAN_POINT('Ctrl Pts',(86.7813047057607,62.5177815384898,13.2460950465644));
#74524=CARTESIAN_POINT('Ctrl Pts',(86.7385766298091,62.5132089203072,13.2015710787005));
#74525=CARTESIAN_POINT('Ctrl Pts',(86.6982202733338,62.5086363021247,13.1546718683068));
#74526=CARTESIAN_POINT('Ctrl Pts',(86.6605063021084,62.5040636839421,13.1056834169858));
#74527=CARTESIAN_POINT('Ctrl Pts',(86.6228152326411,62.4994938424757,13.0567247138355));
#74528=CARTESIAN_POINT('Ctrl Pts',(86.5877636789865,62.4949240010093,13.0056796899132));
#74529=CARTESIAN_POINT('Ctrl Pts',(86.5555825005124,62.4903541595429,12.9528679370601));
#74530=CARTESIAN_POINT('Ctrl Pts',(86.5234088769549,62.4857853909015,12.9000685823978));
#74531=CARTESIAN_POINT('Ctrl Pts',(86.4941045572299,62.48121662226,12.8455037592586));
#74532=CARTESIAN_POINT('Ctrl Pts',(86.4678563091501,62.4766478536186,12.78952082554));
#74533=CARTESIAN_POINT('Ctrl Pts',(86.4413267665586,62.4720301228697,12.7329379397046));
#74534=CARTESIAN_POINT('Ctrl Pts',(86.4179194492552,62.4674123921208,12.674906833083));
#74535=CARTESIAN_POINT('Ctrl Pts',(86.3977778179899,62.4627946613718,12.6158081729755));
#74536=CARTESIAN_POINT('Ctrl Pts',(86.3778244481651,62.458220092005,12.5572619010403));
#74537=CARTESIAN_POINT('Ctrl Pts',(86.3610760526445,62.4536455226381,12.4976684658435));
#74538=CARTESIAN_POINT('Ctrl Pts',(86.347621530971,62.4490709532713,12.4374120412304));
#74539=CARTESIAN_POINT('Ctrl Pts',(86.3339765927674,62.4444316418314,12.3763028312437));
#74540=CARTESIAN_POINT('Ctrl Pts',(86.3237195974269,62.4397923303914,12.3145122529744));
#74541=CARTESIAN_POINT('Ctrl Pts',(86.3168890009944,62.4351530189515,12.2524477370426));
#74542=CARTESIAN_POINT('Ctrl Pts',(86.3100584045619,62.4305137075115,12.1903832211108));
#74543=CARTESIAN_POINT('Ctrl Pts',(86.306654169042,62.4258743960716,12.1280453121899));
#74544=CARTESIAN_POINT('Ctrl Pts',(86.306660007507,62.4212350846317,12.0658400339999));
#74545=CARTESIAN_POINT('',(86.3066606648187,61.6274850846366,12.0675053748877));
#74546=CARTESIAN_POINT('Ctrl Pts',(86.3066600075071,62.4212350845702,12.0658400331759));
#74547=CARTESIAN_POINT('Ctrl Pts',(86.3066608129255,62.4205950931586,12.0572588365243));
#74548=CARTESIAN_POINT('Ctrl Pts',(86.3067264261332,62.4199551017471,12.0486779912057));
#74549=CARTESIAN_POINT('Ctrl Pts',(86.3068568343893,62.4193151103355,12.0400981332293));
#74550=CARTESIAN_POINT('Ctrl Pts',(86.3077935905844,62.4147178866782,11.9784667966938));
#74551=CARTESIAN_POINT('Ctrl Pts',(86.3120799811377,62.4101206630209,11.9167598298027));
#74552=CARTESIAN_POINT('Ctrl Pts',(86.3197252405793,62.4055234393636,11.8553711231895));
#74553=CARTESIAN_POINT('Ctrl Pts',(86.3275014075449,62.4008474988007,11.792931275847));
#74554=CARTESIAN_POINT('Ctrl Pts',(86.3387526387959,62.3961715582377,11.7308212219863));
#74555=CARTESIAN_POINT('Ctrl Pts',(86.3534332112112,62.3914956176747,11.6694559591868));
#74556=CARTESIAN_POINT('Ctrl Pts',(86.3678269433106,62.3869110392351,11.6092896980933));
#74557=CARTESIAN_POINT('Ctrl Pts',(86.3855170874842,62.3823264607956,11.5498399039925));
#74558=CARTESIAN_POINT('Ctrl Pts',(86.4064085691986,62.377741882356,11.4914904911155));
#74559=CARTESIAN_POINT('Ctrl Pts',(86.4272872824058,62.3731601059303,11.4331767403761));
#74560=CARTESIAN_POINT('Ctrl Pts',(86.4513632822594,62.3685783295047,11.3759625155834));
#74561=CARTESIAN_POINT('Ctrl Pts',(86.4784917266961,62.363996553079,11.3202163665947));
#74562=CARTESIAN_POINT('Ctrl Pts',(86.5056135548793,62.3594158940855,11.264483813323));
#74563=CARTESIAN_POINT('Ctrl Pts',(86.5357861271527,62.3548352350919,11.2102190826047));
#74564=CARTESIAN_POINT('Ctrl Pts',(86.56881740355,62.3502545760984,11.1577686450597));
#74565=CARTESIAN_POINT('Ctrl Pts',(86.6030419868765,62.3455084335778,11.1034233527774));
#74566=CARTESIAN_POINT('Ctrl Pts',(86.6403355237341,62.3407622910574,11.0510264780217));
#74567=CARTESIAN_POINT('Ctrl Pts',(86.6804350640614,62.3360161485369,11.0009310882151));
#74568=CARTESIAN_POINT('Ctrl Pts',(86.7191854790905,62.3314296871721,10.9525211281456));
#74569=CARTESIAN_POINT('Ctrl Pts',(86.7605556654545,62.3268432258073,10.9062605835551));
#74570=CARTESIAN_POINT('Ctrl Pts',(86.8042686639268,62.3222567644425,10.8624326698771));
#74571=CARTESIAN_POINT('Ctrl Pts',(86.8502645145462,62.3174307813442,10.8163159027611));
#74572=CARTESIAN_POINT('Ctrl Pts',(86.8988541147888,62.3126047982458,10.7728932528154));
#74573=CARTESIAN_POINT('Ctrl Pts',(86.9496751073592,62.3077788151474,10.732446736024));
#74574=CARTESIAN_POINT('Ctrl Pts',(87.0004960999296,62.3029528320491,10.6920002192326));
#74575=CARTESIAN_POINT('Ctrl Pts',(87.0535479109055,62.2981268489507,10.6545301462196));
#74576=CARTESIAN_POINT('Ctrl Pts',(87.1084355606251,62.2933008658524,10.6202641083601));
#74577=CARTESIAN_POINT('Ctrl Pts',(87.1607214457935,62.2887036422621,10.5876223368532));
#74578=CARTESIAN_POINT('Ctrl Pts',(87.2148877071279,62.2841064186718,10.5577536421674));
#74579=CARTESIAN_POINT('Ctrl Pts',(87.2706084375798,62.2795091950815,10.5308794282217));
#74580=CARTESIAN_POINT('Ctrl Pts',(87.3272832586035,62.2748332545102,10.5035450545842));
#74581=CARTESIAN_POINT('Ctrl Pts',(87.3855658837477,62.2701573139388,10.4793090355932));
#74582=CARTESIAN_POINT('Ctrl Pts',(87.4450828645907,62.2654813733675,10.4583580524724));
#74583=CARTESIAN_POINT('Ctrl Pts',(87.5034369559052,62.2608967949965,10.4378164261191));
#74584=CARTESIAN_POINT('Ctrl Pts',(87.562977097953,62.2563122166254,10.4204327960473));
#74585=CARTESIAN_POINT('Ctrl Pts',(87.6233291879626,62.2517276382544,10.4063355227353));
#74586=CARTESIAN_POINT('Ctrl Pts',(87.6836443918281,62.2471458618977,10.3922468654307));
#74587=CARTESIAN_POINT('Ctrl Pts',(87.7447700649916,62.2425640855409,10.3814406977421));
#74588=CARTESIAN_POINT('Ctrl Pts',(87.8063180187702,62.2379823091842,10.3739952357751));
#74589=CARTESIAN_POINT('Ctrl Pts',(87.8678509618479,62.2334016502598,10.366551589654));
#74590=CARTESIAN_POINT('Ctrl Pts',(87.9298054759566,62.2288209913354,10.3624670832712));
#74591=CARTESIAN_POINT('Ctrl Pts',(87.9917863215632,62.224240332411,10.361768305024));
#74592=CARTESIAN_POINT('Ctrl Pts',(88.0560063247892,62.2194941898242,10.3610442822899));
#74593=CARTESIAN_POINT('Ctrl Pts',(88.1202540178258,62.2147480472374,10.3639553717578));
#74594=CARTESIAN_POINT('Ctrl Pts',(88.1840901574413,62.2100019046506,10.3704721668469));
#74595=CARTESIAN_POINT('Ctrl Pts',(88.2457785661354,62.2054154433548,10.3767697080399));
#74596=CARTESIAN_POINT('Ctrl Pts',(88.3070821661325,62.2008289820591,10.3864340147995));
#74597=CARTESIAN_POINT('Ctrl Pts',(88.3676127998188,62.1962425207633,10.3993860235179));
#74598=CARTESIAN_POINT('Ctrl Pts',(88.4313045666032,62.1914165375309,10.413014433935));
#74599=CARTESIAN_POINT('Ctrl Pts',(88.494139795063,62.1865905542986,10.4302831943551));
#74600=CARTESIAN_POINT('Ctrl Pts',(88.5556850154075,62.1817645710662,10.4510408458446));
#74601=CARTESIAN_POINT('Ctrl Pts',(88.6172302357521,62.1769385878338,10.471798497334));
#74602=CARTESIAN_POINT('Ctrl Pts',(88.6774848757244,62.1721126046015,10.4960447262106));
#74603=CARTESIAN_POINT('Ctrl Pts',(88.7360434944745,62.1672866213691,10.5235711469503));
#74604=CARTESIAN_POINT('Ctrl Pts',(88.7918263370121,62.1626893977923,10.5497927694292));
#74605=CARTESIAN_POINT('Ctrl Pts',(88.8462993727308,62.1580921742156,10.5790982491545));
#74606=CARTESIAN_POINT('Ctrl Pts',(88.8990998239316,62.1534949506388,10.611333873931));
#74607=CARTESIAN_POINT('Ctrl Pts',(88.9528043627521,62.1488190100658,10.6441214604542));
#74608=CARTESIAN_POINT('Ctrl Pts',(89.0047779792158,62.1441430694927,10.6799403409917));
#74609=CARTESIAN_POINT('Ctrl Pts',(89.0546612805093,62.1394671289197,10.7185780292849));
#74610=CARTESIAN_POINT('Ctrl Pts',(89.1035699224995,62.1348825505633,10.7564607839356));
#74611=CARTESIAN_POINT('Ctrl Pts',(89.1504687774279,62.1302979722069,10.7970528581824));
#74612=CARTESIAN_POINT('Ctrl Pts',(89.1950470940587,62.1257133938505,10.8401095829352));
#74613=CARTESIAN_POINT('Ctrl Pts',(89.2395981651965,62.1211316175088,10.8831399921656));
#74614=CARTESIAN_POINT('Ctrl Pts',(89.281831144881,62.1165498411671,10.9286317121107));
#74615=CARTESIAN_POINT('Ctrl Pts',(89.3214697690442,62.1119680648254,10.9763010415619));
#74616=CARTESIAN_POINT('Ctrl Pts',(89.3610987258882,62.1073874059164,11.0239587451144));
#74617=CARTESIAN_POINT('Ctrl Pts',(89.3981342579493,62.1028067470074,11.0737926126485));
#74618=CARTESIAN_POINT('Ctrl Pts',(89.4323396503179,62.0982260880984,11.1254850165818));
#74619=CARTESIAN_POINT('Ctrl Pts',(89.4677807676618,62.0934799454973,11.179044891991));
#74620=CARTESIAN_POINT('Ctrl Pts',(89.5001829691893,62.0887338028963,11.234599710581));
#74621=CARTESIAN_POINT('Ctrl Pts',(89.529332715001,62.0839876602952,11.291764504716));
#74622=CARTESIAN_POINT('Ctrl Pts',(89.5575017338686,62.0794011990156,11.3470060212271));
#74623=CARTESIAN_POINT('Ctrl Pts',(89.5826335419652,62.0748147377359,11.4037503812814));
#74624=CARTESIAN_POINT('Ctrl Pts',(89.6045840260914,62.0702282764563,11.4616286014491));
#74625=CARTESIAN_POINT('Ctrl Pts',(89.6276808457352,62.0654022931945,11.5225294364757));
#74626=CARTESIAN_POINT('Ctrl Pts',(89.6472547448984,62.0605763099328,11.5846851968848));
#74627=CARTESIAN_POINT('Ctrl Pts',(89.6631978539558,62.0557503266711,11.6476495643794));
#74628=CARTESIAN_POINT('Ctrl Pts',(89.6791409630131,62.0509243434093,11.710613931874));
#74629=CARTESIAN_POINT('Ctrl Pts',(89.6914532351042,62.0460983601476,11.7743862555481));
#74630=CARTESIAN_POINT('Ctrl Pts',(89.700089828703,62.0412723768858,11.8385128878986));
#74631=CARTESIAN_POINT('Ctrl Pts',(89.7083170333511,62.036675153285,11.8995998108521));
#74632=CARTESIAN_POINT('Ctrl Pts',(89.7132429865986,62.0320779296842,11.9612590177146));
#74633=CARTESIAN_POINT('Ctrl Pts',(89.7148000551434,62.0274807060833,12.0231023579518));
#74634=CARTESIAN_POINT('Ctrl Pts',(89.7163837849359,62.0228047655133,12.0860046243433));
#74635=CARTESIAN_POINT('Ctrl Pts',(89.7144820103083,62.0181288249433,12.1490968763259));
#74636=CARTESIAN_POINT('Ctrl Pts',(89.7090783112516,62.0134528843732,12.2119619281077));
#74637=CARTESIAN_POINT('Ctrl Pts',(89.7037801938987,62.0088683059918,12.2735986732782));
#74638=CARTESIAN_POINT('Ctrl Pts',(89.6951158137425,62.0042837276103,12.3350164853722));
#74639=CARTESIAN_POINT('Ctrl Pts',(89.683122171383,61.9996991492289,12.3958215874824));
#74640=CARTESIAN_POINT('Ctrl Pts',(89.6711358593285,61.9951173728618,12.4565895265744));
#74641=CARTESIAN_POINT('Ctrl Pts',(89.6558244180651,61.9905355964947,12.5167449998295));
#74642=CARTESIAN_POINT('Ctrl Pts',(89.6372763456987,61.9859538201276,12.575902032768));
#74643=CARTESIAN_POINT('Ctrl Pts',(89.6187327969528,61.981373161193,12.6350446381171));
#74644=CARTESIAN_POINT('Ctrl Pts',(89.5969543363508,61.9767925022584,12.693188801032));
#74645=CARTESIAN_POINT('Ctrl Pts',(89.572079415678,61.9722118433237,12.7499633714948));
#74646=CARTESIAN_POINT('Ctrl Pts',(89.5463058486468,61.967465700747,12.8087890142671));
#74647=CARTESIAN_POINT('Ctrl Pts',(89.5172079834779,61.9627195581702,12.8661436542454));
#74648=CARTESIAN_POINT('Ctrl Pts',(89.4849934158513,61.9579734155935,12.9216390860795));
#74649=CARTESIAN_POINT('Ctrl Pts',(89.4538626890542,61.9533869542878,12.9752674056317));
#74650=CARTESIAN_POINT('Ctrl Pts',(89.4198220121885,61.9488004929822,13.0271592405708));
#74651=CARTESIAN_POINT('Ctrl Pts',(89.3831032092268,61.9442140316766,13.0769933821888));
#74652=CARTESIAN_POINT('Ctrl Pts',(89.3444668150961,61.9393880484642,13.1294300462794));
#74653=CARTESIAN_POINT('Ctrl Pts',(89.302865303941,61.9345620652519,13.1795877003108));
#74654=CARTESIAN_POINT('Ctrl Pts',(89.258615128848,61.9297360820396,13.2271336382474));
#74655=CARTESIAN_POINT('Ctrl Pts',(89.214364953755,61.9249100988273,13.274679576184));
#74656=CARTESIAN_POINT('Ctrl Pts',(89.1674666361469,61.920084115615,13.3196134056069));
#74657=CARTESIAN_POINT('Ctrl Pts',(89.1182769728918,61.9152581324026,13.3616513963654));
#74658=CARTESIAN_POINT('Ctrl Pts',(89.0714189813886,61.9106609088115,13.4016967165287));
#74659=CARTESIAN_POINT('Ctrl Pts',(89.0222896073878,61.9060636852203,13.4392789915989));
#74660=CARTESIAN_POINT('Ctrl Pts',(88.9711782601494,61.9014664616292,13.4741308690376));
#74661=CARTESIAN_POINT('Ctrl Pts',(88.9191917475371,61.8967905210579,13.5095795054739));
#74662=CARTESIAN_POINT('Ctrl Pts',(88.8651550907164,61.8921145804867,13.5422029438071));
#74663=CARTESIAN_POINT('Ctrl Pts',(88.8094098701109,61.8874386399155,13.5717611081807));
#74664=CARTESIAN_POINT('Ctrl Pts',(88.7547538434122,61.882854061544,13.6007417419214));
#74665=CARTESIAN_POINT('Ctrl Pts',(88.6984558902489,61.8782694831724,13.6267755579987));
#74666=CARTESIAN_POINT('Ctrl Pts',(88.6408669000153,61.8736849048009,13.6496800572922));
#74667=CARTESIAN_POINT('Ctrl Pts',(88.5833131071693,61.8691031284439,13.6725705577548));
#74668=CARTESIAN_POINT('Ctrl Pts',(88.524470313871,61.8645213520868,13.6923353460748));
#74669=CARTESIAN_POINT('Ctrl Pts',(88.4647107867141,61.8599395757297,13.7088394193041));
#74670=CARTESIAN_POINT('Ctrl Pts',(88.4049658340872,61.8553589168051,13.7253394674159));
#74671=CARTESIAN_POINT('Ctrl Pts',(88.3443050818981,61.8507782578806,13.7385802436641));
#74672=CARTESIAN_POINT('Ctrl Pts',(88.2831154372097,61.846197598956,13.7484767530139));
#74673=CARTESIAN_POINT('Ctrl Pts',(88.2197152183149,61.8414514563696,13.7587307896613));
#74674=CARTESIAN_POINT('Ctrl Pts',(88.1557477248056,61.8367053137832,13.7653941429532));
#74675=CARTESIAN_POINT('Ctrl Pts',(88.0916516958592,61.8319591711968,13.7684306563132));
#74676=CARTESIAN_POINT('Ctrl Pts',(88.0297121416607,61.8273727099013,13.7713650078936));
#74677=CARTESIAN_POINT('Ctrl Pts',(87.9676530916298,61.8227862486057,13.7709127817225));
#74678=CARTESIAN_POINT('Ctrl Pts',(87.9058701410369,61.8181997873101,13.7670945148211));
#74679=CARTESIAN_POINT('Ctrl Pts',(87.8408606567402,61.8133738040784,13.7630768439299));
#74680=CARTESIAN_POINT('Ctrl Pts',(87.7761575412377,61.8085478208466,13.7553319831836));
#74681=CARTESIAN_POINT('Ctrl Pts',(87.7122119516828,61.8037218376148,13.7439453321795));
#74682=CARTESIAN_POINT('Ctrl Pts',(87.648266362128,61.798895854383,13.7325586811753));
#74683=CARTESIAN_POINT('Ctrl Pts',(87.5850789110193,61.7940698711512,13.717530465124));
#74684=CARTESIAN_POINT('Ctrl Pts',(87.5230814922492,61.7892438879194,13.6990065417488));
#74685=CARTESIAN_POINT('Ctrl Pts',(87.4640228543667,61.7846466643291,13.6813606831874));
#74686=CARTESIAN_POINT('Ctrl Pts',(87.4058014777533,61.7800494407387,13.660470635492));
#74687=CARTESIAN_POINT('Ctrl Pts',(87.3487989461613,61.7754522171483,13.6364345258224));
#74688=CARTESIAN_POINT('Ctrl Pts',(87.2908203760746,61.7707762765769,13.6119868525318));
#74689=CARTESIAN_POINT('Ctrl Pts',(87.2341033190426,61.7661003360056,13.5842844257315));
#74690=CARTESIAN_POINT('Ctrl Pts',(87.1790347406746,61.7614243954343,13.5534839975192));
#74691=CARTESIAN_POINT('Ctrl Pts',(87.1250421354572,61.7568398170636,13.5232853722726));
#74692=CARTESIAN_POINT('Ctrl Pts',(87.072634635261,61.752255238693,13.4901089795872));
#74693=CARTESIAN_POINT('Ctrl Pts',(87.0221558834339,61.7476706603223,13.4541506217744));
#74694=CARTESIAN_POINT('Ctrl Pts',(86.971707983341,61.7430888839662,13.4182142410838));
#74695=CARTESIAN_POINT('Ctrl Pts',(86.9231869079409,61.73850710761,13.3794995614247));
#74696=CARTESIAN_POINT('Ctrl Pts',(86.8769079930086,61.7339253312539,13.3382461064111));
#74697=CARTESIAN_POINT('Ctrl Pts',(86.8306403648701,61.7293446723302,13.2970027125505));
#74698=CARTESIAN_POINT('Ctrl Pts',(86.7866141914748,61.7247640134066,13.2532221110623));
#74699=CARTESIAN_POINT('Ctrl Pts',(86.7451107368634,61.720183354483,13.2071832495596));
#74700=CARTESIAN_POINT('Ctrl Pts',(86.7021079032683,61.7154372118957,13.159481160212));
#74701=CARTESIAN_POINT('Ctrl Pts',(86.6618139897296,61.7106910693085,13.1093549092388));
#74702=CARTESIAN_POINT('Ctrl Pts',(86.6244973437402,61.7059449267213,13.0571534794292));
#74703=CARTESIAN_POINT('Ctrl Pts',(86.5884361952756,61.7013584654267,13.0067083373078));
#74704=CARTESIAN_POINT('Ctrl Pts',(86.555155368084,61.6967720041322,12.9543259286243));
#74705=CARTESIAN_POINT('Ctrl Pts',(86.5248521789646,61.6921855428377,12.9003497405954));
#74706=CARTESIAN_POINT('Ctrl Pts',(86.4929664454496,61.6873595596041,12.8435547167826));
#74707=CARTESIAN_POINT('Ctrl Pts',(86.4643781770976,61.6825335763705,12.7849954567107));
#74708=CARTESIAN_POINT('Ctrl Pts',(86.4392603349813,61.677707593137,12.7250973076921));
#74709=CARTESIAN_POINT('Ctrl Pts',(86.414142492865,61.6728816099034,12.6651991586735));
#74710=CARTESIAN_POINT('Ctrl Pts',(86.3924952199985,61.6680556266698,12.6039627574354));
#74711=CARTESIAN_POINT('Ctrl Pts',(86.3744302369339,61.6632296434362,12.5418300602294));
#74712=CARTESIAN_POINT('Ctrl Pts',(86.3521299505428,61.6572722169696,12.4651304620624));
#74713=CARTESIAN_POINT('Ctrl Pts',(86.335208780096,61.651314790503,12.3868010792025));
#74714=CARTESIAN_POINT('Ctrl Pts',(86.3238591749853,61.6453573640364,12.3075174365728));
#74715=CARTESIAN_POINT('Ctrl Pts',(86.313151704821,61.6397369952637,12.2327194828383));
#74716=CARTESIAN_POINT('Ctrl Pts',(86.3074028970101,61.6341166264909,12.1570722506466));
#74717=CARTESIAN_POINT('Ctrl Pts',(86.3067274670126,61.6284962577181,12.0811647256718));
#74718=CARTESIAN_POINT('Ctrl Pts',(86.3066869609735,61.6281592000243,12.0766124949644));
#74719=CARTESIAN_POINT('Ctrl Pts',(86.3066646871496,61.6278221423304,12.072059334826));
#74720=CARTESIAN_POINT('Ctrl Pts',(86.3066606648186,61.6274850846366,12.0675053748877));
#74721=CARTESIAN_POINT('',(86.3066601613137,60.8337350845235,12.065258469835));
#74722=CARTESIAN_POINT('Ctrl Pts',(86.3066606648178,61.6274850845702,12.0675053739911));
#74723=CARTESIAN_POINT('Ctrl Pts',(86.306606406938,61.6229384555704,12.0060762278913));
#74724=CARTESIAN_POINT('Ctrl Pts',(86.3098775506704,61.6183918265706,11.9445793182848));
#74725=CARTESIAN_POINT('Ctrl Pts',(86.3164694016912,61.6138451975707,11.8834051287813));
#74726=CARTESIAN_POINT('Ctrl Pts',(86.3230581031606,61.6093007409262,11.8222601679815));
#74727=CARTESIAN_POINT('Ctrl Pts',(86.3329643112659,61.6047562842816,11.7614381359344));
#74728=CARTESIAN_POINT('Ctrl Pts',(86.3461313706499,61.600211827637,11.7013257856581));
#74729=CARTESIAN_POINT('Ctrl Pts',(86.3592971677434,61.5956678066573,11.6412191981911));
#74730=CARTESIAN_POINT('Ctrl Pts',(86.3757230830511,61.5911237856775,11.5818226629785));
#74731=CARTESIAN_POINT('Ctrl Pts',(86.3953015242927,61.5865797646978,11.5235119621622));
#74732=CARTESIAN_POINT('Ctrl Pts',(86.414899289768,61.5820312586969,11.4651437077544));
#74733=CARTESIAN_POINT('Ctrl Pts',(86.4376556276918,61.577482752696,11.407863919384));
#74734=CARTESIAN_POINT('Ctrl Pts',(86.4634137187882,61.572934246695,11.3520311366698));
#74735=CARTESIAN_POINT('Ctrl Pts',(86.4891853727869,61.5683833456819,11.2961689552485));
#74736=CARTESIAN_POINT('Ctrl Pts',(86.5179616824663,61.5638324446688,11.2417557537004));
#74737=CARTESIAN_POINT('Ctrl Pts',(86.5495399535247,61.5592815436557,11.1891252266392));
#74738=CARTESIAN_POINT('Ctrl Pts',(86.581175969965,61.5547223206696,11.1363984571373));
#74739=CARTESIAN_POINT('Ctrl Pts',(86.6156238843628,61.5501630976836,11.0854612979128));
#74740=CARTESIAN_POINT('Ctrl Pts',(86.6526384547238,61.5456038746976,11.0366172976415));
#74741=CARTESIAN_POINT('Ctrl Pts',(86.6753393861925,61.542807716116,11.0066614102165));
#74742=CARTESIAN_POINT('Ctrl Pts',(86.6990049287886,61.5400115575345,10.9774921751297));
#74743=CARTESIAN_POINT('Ctrl Pts',(86.7235716774766,61.5372153989529,10.9491727304706));
#74744=CARTESIAN_POINT('Ctrl Pts',(86.7639623897164,61.5326181753611,10.9026121312417));
#74745=CARTESIAN_POINT('Ctrl Pts',(86.8069651078682,61.5280209517692,10.8581499110785));
#74746=CARTESIAN_POINT('Ctrl Pts',(86.8523333400228,61.5234237281773,10.8160934408296));
#74747=CARTESIAN_POINT('Ctrl Pts',(86.8984783997819,61.5187477876061,10.773316849353));
#74748=CARTESIAN_POINT('Ctrl Pts',(86.9470704683404,61.514071847035,10.7330296320008));
#74749=CARTESIAN_POINT('Ctrl Pts',(86.9978074100754,61.5093959064639,10.6955199339933));
#74750=CARTESIAN_POINT('Ctrl Pts',(87.0475530135985,61.5048113280916,10.6587431299221));
#74751=CARTESIAN_POINT('Ctrl Pts',(87.0993599987467,61.5002267497194,10.6246365997431));
#74752=CARTESIAN_POINT('Ctrl Pts',(87.1529084727936,61.4956421713472,10.5934329330939));
#74753=CARTESIAN_POINT('Ctrl Pts',(87.2064242189458,61.4910603949895,10.5622483375822));
#74754=CARTESIAN_POINT('Ctrl Pts',(87.2616789045999,61.4864786186317,10.5339633434187));
#74755=CARTESIAN_POINT('Ctrl Pts',(87.3183244427234,61.4818968422739,10.5087667458112));
#74756=CARTESIAN_POINT('Ctrl Pts',(87.3749561657757,61.4773161833487,10.4835762933088));
#74757=CARTESIAN_POINT('Ctrl Pts',(87.4329776030128,61.4727355244234,10.4614729489047));
#74758=CARTESIAN_POINT('Ctrl Pts',(87.4920187620624,61.4681548654982,10.4425982289437));
#74759=CARTESIAN_POINT('Ctrl Pts',(87.5531928778059,61.4634087229125,10.4230416294103));
#74760=CARTESIAN_POINT('Ctrl Pts',(87.6154612699018,61.4586625803268,10.4069516372537));
#74761=CARTESIAN_POINT('Ctrl Pts',(87.6783954351681,61.4539164377411,10.3944291701956));
#74762=CARTESIAN_POINT('Ctrl Pts',(87.7392122159518,61.4493299764449,10.3823280144765));
#74763=CARTESIAN_POINT('Ctrl Pts',(87.800650146486,61.4447435151487,10.3735581289527));
#74764=CARTESIAN_POINT('Ctrl Pts',(87.8623149687829,61.4401570538525,10.3681579587335));
#74765=CARTESIAN_POINT('Ctrl Pts',(87.9272001556612,61.435331070622,10.3624757716972));
#74766=CARTESIAN_POINT('Ctrl Pts',(87.9923359390259,61.4305050873916,10.3605249392997));
#74767=CARTESIAN_POINT('Ctrl Pts',(88.0572634817533,61.4256791041611,10.3622880155801));
#74768=CARTESIAN_POINT('Ctrl Pts',(88.1221910244806,61.4208531209306,10.3640510918604));
#74769=CARTESIAN_POINT('Ctrl Pts',(88.1869096874165,61.4160271377002,10.3695279450747));
#74770=CARTESIAN_POINT('Ctrl Pts',(88.250970703728,61.4112011544697,10.3786384806591));
#74771=CARTESIAN_POINT('Ctrl Pts',(88.311995121229,61.4066039308778,10.3873171616913));
#74772=CARTESIAN_POINT('Ctrl Pts',(88.372673394828,61.4020067072859,10.3993284023983));
#74773=CARTESIAN_POINT('Ctrl Pts',(88.4326135988613,61.397409483694,10.414631837277));
#74774=CARTESIAN_POINT('Ctrl Pts',(88.4935801423151,61.3927335431229,10.4301973086091));
#74775=CARTESIAN_POINT('Ctrl Pts',(88.5537825644107,61.3880576025517,10.449168797285));
#74776=CARTESIAN_POINT('Ctrl Pts',(88.61281491026,61.3833816619806,10.4714487623821));
#74777=CARTESIAN_POINT('Ctrl Pts',(88.6706938357778,61.3787970836084,10.4932934040246));
#74778=CARTESIAN_POINT('Ctrl Pts',(88.7274474985102,61.3742125052362,10.5183182092679));
#74779=CARTESIAN_POINT('Ctrl Pts',(88.7827069855596,61.3696279268639,10.5463805857918));
#74780=CARTESIAN_POINT('Ctrl Pts',(88.8379326989729,61.3650461505062,10.5744258110798));
#74781=CARTESIAN_POINT('Ctrl Pts',(88.8916655945412,61.3604643741484,10.6055046964431));
#74782=CARTESIAN_POINT('Ctrl Pts',(88.9435582594377,61.3558825977906,10.6394272088833));
#74783=CARTESIAN_POINT('Ctrl Pts',(88.9954382684238,61.3513019388654,10.6733414480872));
#74784=CARTESIAN_POINT('Ctrl Pts',(89.0454785117945,61.3467212799401,10.7100976592132));
#74785=CARTESIAN_POINT('Ctrl Pts',(89.0933594152672,61.3421406210148,10.7494617621268));
#74786=CARTESIAN_POINT('Ctrl Pts',(89.142970093277,61.3373944784292,10.7902479564787));
#74787=CARTESIAN_POINT('Ctrl Pts',(89.1902619351784,61.3326483358435,10.8338337591143));
#74788=CARTESIAN_POINT('Ctrl Pts',(89.2349177382608,61.3279021932578,10.8799139130862));
#74789=CARTESIAN_POINT('Ctrl Pts',(89.2780711220437,61.3233157319616,10.9244437262764));
#74790=CARTESIAN_POINT('Ctrl Pts',(89.3187627460656,61.3187292706654,10.9713022573559));
#74791=CARTESIAN_POINT('Ctrl Pts',(89.3567464667318,61.3141428093692,11.0201791344217));
#74792=CARTESIAN_POINT('Ctrl Pts',(89.3967138374619,61.3093168261387,11.0716085423776));
#74793=CARTESIAN_POINT('Ctrl Pts',(89.433682341388,61.3044908429083,11.1252723638878));
#74794=CARTESIAN_POINT('Ctrl Pts',(89.4674177625429,61.2996648596779,11.1807756575028));
#74795=CARTESIAN_POINT('Ctrl Pts',(89.5011531836978,61.2948388764474,11.2362789511179));
#74796=CARTESIAN_POINT('Ctrl Pts',(89.5316552860858,61.290012893217,11.2936211084133));
#74797=CARTESIAN_POINT('Ctrl Pts',(89.5587479482707,61.2851869099865,11.3523816676796));
#74798=CARTESIAN_POINT('Ctrl Pts',(89.5845563731709,61.2805896863943,11.4083568786268));
#74799=CARTESIAN_POINT('Ctrl Pts',(89.6073772961101,61.2759924628021,11.4658488629993));
#74800=CARTESIAN_POINT('Ctrl Pts',(89.6270320490069,61.2713952392099,11.5245064615504));
#74801=CARTESIAN_POINT('Ctrl Pts',(89.647023344762,61.2667192986387,11.5841684378208));
#74802=CARTESIAN_POINT('Ctrl Pts',(89.6637387147587,61.2620433580676,11.645035879155));
#74803=CARTESIAN_POINT('Ctrl Pts',(89.6770399157617,61.2573674174965,11.7067148281815));
#74804=CARTESIAN_POINT('Ctrl Pts',(89.6900812274551,61.252782839124,11.7671886454702));
#74805=CARTESIAN_POINT('Ctrl Pts',(89.6998404752371,61.2481982607514,11.8284420224734));
#74806=CARTESIAN_POINT('Ctrl Pts',(89.7062373560354,61.2436136823788,11.8900876857573));
#74807=CARTESIAN_POINT('Ctrl Pts',(89.7126303271715,61.2390319060207,11.9516956722856));
#74808=CARTESIAN_POINT('Ctrl Pts',(89.7156649536999,61.2344501296626,12.0136949644102));
#74809=CARTESIAN_POINT('Ctrl Pts',(89.7153124500783,61.2298683533045,12.0756906195969));
#74810=CARTESIAN_POINT('Ctrl Pts',(89.7149600324274,61.2252876943789,12.1376711548923));
#74811=CARTESIAN_POINT('Ctrl Pts',(89.711222127403,61.2207070354533,12.1996475461998));
#74812=CARTESIAN_POINT('Ctrl Pts',(89.7041220539864,61.2161263765277,12.2612243476233));
#74813=CARTESIAN_POINT('Ctrl Pts',(89.6967654790156,61.2113802339423,12.3250257098842));
#74814=CARTESIAN_POINT('Ctrl Pts',(89.685799160019,61.206634091357,12.3883974729087));
#74815=CARTESIAN_POINT('Ctrl Pts',(89.671307499463,61.2018879487716,12.4509075769934));
#74816=CARTESIAN_POINT('Ctrl Pts',(89.657303402648,61.197301487475,12.5113145639037));
#74817=CARTESIAN_POINT('Ctrl Pts',(89.6400076451835,61.1927150261785,12.5709164680236));
#74818=CARTESIAN_POINT('Ctrl Pts',(89.6195474690945,61.1881285648819,12.6293381535717));
#74819=CARTESIAN_POINT('Ctrl Pts',(89.5980187871109,61.1833025816521,12.6908108351185));
#74820=CARTESIAN_POINT('Ctrl Pts',(89.5729863453518,61.1784765984224,12.7509760483229));
#74821=CARTESIAN_POINT('Ctrl Pts',(89.5446549040389,61.1736506151926,12.8094228076386));
#74822=CARTESIAN_POINT('Ctrl Pts',(89.5163234627261,61.1688246319628,12.8678695669544));
#74823=CARTESIAN_POINT('Ctrl Pts',(89.4846934050063,61.1639986487331,12.9245973441079));
#74824=CARTESIAN_POINT('Ctrl Pts',(89.4500224416137,61.1591726655033,12.9792301178411));
#74825=CARTESIAN_POINT('Ctrl Pts',(89.4169949395942,61.1545754419113,13.0312732071655));
#74826=CARTESIAN_POINT('Ctrl Pts',(89.3810727467405,61.1499782183192,13.0816291288742));
#74827=CARTESIAN_POINT('Ctrl Pts',(89.3424539700237,61.1453809947272,13.1299573117885));
#74828=CARTESIAN_POINT('Ctrl Pts',(89.3031739347497,61.1407050541561,13.1791130047178));
#74829=CARTESIAN_POINT('Ctrl Pts',(89.2611043046755,61.1360291135849,13.2261703658227));
#74830=CARTESIAN_POINT('Ctrl Pts',(89.2165010687694,61.1313531730138,13.2707995720434));
#74831=CARTESIAN_POINT('Ctrl Pts',(89.1727693259121,61.1267685946414,13.3145567777869));
#74832=CARTESIAN_POINT('Ctrl Pts',(89.1266024710288,61.122184016269,13.3559794843794));
#74833=CARTESIAN_POINT('Ctrl Pts',(89.0782823044433,61.1175994378967,13.3947901708781));
#74834=CARTESIAN_POINT('Ctrl Pts',(89.0299916703019,61.1130176615387,13.4335771369612));
#74835=CARTESIAN_POINT('Ctrl Pts',(88.9795507300838,61.1084358851808,13.4697549303118));
#74836=CARTESIAN_POINT('Ctrl Pts',(88.9272756701305,61.1038541088229,13.5030851512443));
#74837=CARTESIAN_POINT('Ctrl Pts',(88.8750133593484,61.0992734498975,13.5364072433924));
#74838=CARTESIAN_POINT('Ctrl Pts',(88.8209182458546,61.0946927909721,13.5668828682304));
#74839=CARTESIAN_POINT('Ctrl Pts',(88.7653352003049,61.0901121320467,13.5943171271634));
#74840=CARTESIAN_POINT('Ctrl Pts',(88.7077441279694,61.0853659894611,13.6227424927592));
#74841=CARTESIAN_POINT('Ctrl Pts',(88.6485560503527,61.0806198468755,13.6479022218827));
#74842=CARTESIAN_POINT('Ctrl Pts',(88.588179729752,61.07587370429,13.6696328741839));
#74843=CARTESIAN_POINT('Ctrl Pts',(88.5298347363895,61.0712872429936,13.6906324109504));
#74844=CARTESIAN_POINT('Ctrl Pts',(88.4703807174589,61.0667007816973,13.7084298780083));
#74845=CARTESIAN_POINT('Ctrl Pts',(88.4102018483891,61.0621143204009,13.7229287008929));
#74846=CARTESIAN_POINT('Ctrl Pts',(88.3468802167051,61.0572883371708,13.7381847058119));
#74847=CARTESIAN_POINT('Ctrl Pts',(88.2827565818875,61.0524623539406,13.7497879587534));
#74848=CARTESIAN_POINT('Ctrl Pts',(88.2182872832856,61.0476363707105,13.7576875650628));
#74849=CARTESIAN_POINT('Ctrl Pts',(88.1538179846837,61.0428103874803,13.7655871713722));
#74850=CARTESIAN_POINT('Ctrl Pts',(88.0890036739298,61.0379844042502,13.7697831664042));
#74851=CARTESIAN_POINT('Ctrl Pts',(88.024300036427,61.03315842102,13.7702881049374));
#74852=CARTESIAN_POINT('Ctrl Pts',(87.9626634590428,61.028561197428,13.7707691085436));
#74853=CARTESIAN_POINT('Ctrl Pts',(87.9008742301636,61.0239639738359,13.7679031034688));
#74854=CARTESIAN_POINT('Ctrl Pts',(87.8393259238227,61.0193667502438,13.7616717981876));
#74855=CARTESIAN_POINT('Ctrl Pts',(87.776723742976,61.0146908096727,13.7553337960016));
#74856=CARTESIAN_POINT('Ctrl Pts',(87.7143713423495,61.0100148691016,13.7455140635796));
#74857=CARTESIAN_POINT('Ctrl Pts',(87.6526846613781,61.0053389285305,13.7322487670538));
#74858=CARTESIAN_POINT('Ctrl Pts',(87.59220326322,61.0007543501581,13.7192426583083));
#74859=CARTESIAN_POINT('Ctrl Pts',(87.5323623254715,60.9961697717857,13.7029245309443));
#74860=CARTESIAN_POINT('Ctrl Pts',(87.4735478474987,60.9915851934133,13.6833806043637));
#74861=CARTESIAN_POINT('Ctrl Pts',(87.4147693159106,60.9870034170553,13.6638486226905));
#74862=CARTESIAN_POINT('Ctrl Pts',(87.3570164822173,60.9824216406974,13.6410949112955));
#74863=CARTESIAN_POINT('Ctrl Pts',(87.3006611301225,60.9778398643395,13.6152557973237));
#74864=CARTESIAN_POINT('Ctrl Pts',(87.2443195223264,60.973259205414,13.589422985158));
#74865=CARTESIAN_POINT('Ctrl Pts',(87.1893751820561,60.9686785464886,13.5605064762839));
#74866=CARTESIAN_POINT('Ctrl Pts',(87.1361789051645,60.9640978875632,13.5286902910838));
#74867=CARTESIAN_POINT('Ctrl Pts',(87.0810608273384,60.9593517449776,13.4957246950974));
#74868=CARTESIAN_POINT('Ctrl Pts',(87.0278200661602,60.9546056023921,13.4596461439811));
#74869=CARTESIAN_POINT('Ctrl Pts',(86.9768156434923,60.9498594598066,13.420709397751));
#74870=CARTESIAN_POINT('Ctrl Pts',(86.9275272358445,60.9452729985102,13.3830826563766));
#74871=CARTESIAN_POINT('Ctrl Pts',(86.8803274206532,60.9406865372138,13.3427874004942));
#74872=CARTESIAN_POINT('Ctrl Pts',(86.8355057084484,60.9361000759175,13.3000940021447));
#74873=CARTESIAN_POINT('Ctrl Pts',(86.7883432410324,60.9312740926873,13.2551709969874));
#74874=CARTESIAN_POINT('Ctrl Pts',(86.7438145223771,60.9264481094572,13.2075929638639));
#74875=CARTESIAN_POINT('Ctrl Pts',(86.702209828058,60.9216221262271,13.1577156779253));
#74876=CARTESIAN_POINT('Ctrl Pts',(86.6606051337388,60.916796142997,13.1078383919867));
#74877=CARTESIAN_POINT('Ctrl Pts',(86.6219247874981,60.9119701597669,13.0556624198593));
#74878=CARTESIAN_POINT('Ctrl Pts',(86.5864054049996,60.9071441765368,13.0015774021938));
#74879=CARTESIAN_POINT('Ctrl Pts',(86.5519012991686,60.9024561379394,12.949038336418));
#74880=CARTESIAN_POINT('Ctrl Pts',(86.5202420108511,60.8977680993419,12.8944887870569));
#74881=CARTESIAN_POINT('Ctrl Pts',(86.4916626353851,60.8930800607445,12.8382621368972));
#74882=CARTESIAN_POINT('Ctrl Pts',(86.4631330034052,60.8884001818559,12.7821333513531));
#74883=CARTESIAN_POINT('Ctrl Pts',(86.4376728583687,60.8837203029673,12.7243336868688));
#74884=CARTESIAN_POINT('Ctrl Pts',(86.4154735085036,60.8790404240787,12.6652245409971));
#74885=CARTESIAN_POINT('Ctrl Pts',(86.3933119945547,60.8743685214374,12.6062161390075));
#74886=CARTESIAN_POINT('Ctrl Pts',(86.374400394826,60.8696966187961,12.5459031421756));
#74887=CARTESIAN_POINT('Ctrl Pts',(86.3588827577064,60.8650247161548,12.4846686677029));
#74888=CARTESIAN_POINT('Ctrl Pts',(86.3433806101681,60.8603574769695,12.4234953169933));
#74889=CARTESIAN_POINT('Ctrl Pts',(86.3312658171752,60.8556902377841,12.3614027807631));
#74890=CARTESIAN_POINT('Ctrl Pts',(86.3226328405803,60.8510229985987,12.298789970989));
#74891=CARTESIAN_POINT('Ctrl Pts',(86.3140063629978,60.8463592729692,12.2362242969188));
#74892=CARTESIAN_POINT('Ctrl Pts',(86.3088565581616,60.8416955473396,12.1731396048206));
#74893=CARTESIAN_POINT('Ctrl Pts',(86.3072266081747,60.8370318217101,12.1099438836244));
#74894=CARTESIAN_POINT('Ctrl Pts',(86.3068425435101,60.8359329093301,12.0950530933207));
#74895=CARTESIAN_POINT('Ctrl Pts',(86.306653679578,60.8348339969502,12.0801561643758));
#74896=CARTESIAN_POINT('Ctrl Pts',(86.3066601613135,60.8337350845702,12.0652584704679));
#74897=CARTESIAN_POINT('',(86.3066603586072,60.0399850846269,12.0648943883226));
#74898=CARTESIAN_POINT('Ctrl Pts',(86.3066601613138,60.8337350845235,12.065258469835));
#74899=CARTESIAN_POINT('Ctrl Pts',(86.3066897126874,60.8287249537047,11.9973373173053));
#74900=CARTESIAN_POINT('Ctrl Pts',(86.3107836349031,60.8237148228858,11.9295475736294));
#74901=CARTESIAN_POINT('Ctrl Pts',(86.3188700121392,60.818704692067,11.8623558501151));
#74902=CARTESIAN_POINT('Ctrl Pts',(86.3269823930434,60.8136784499816,11.7949480556427));
#74903=CARTESIAN_POINT('Ctrl Pts',(86.3391128067182,60.8086522078963,11.7281424584012));
#74904=CARTESIAN_POINT('Ctrl Pts',(86.3551385560175,60.8036259658109,11.6623941106326));
#74905=CARTESIAN_POINT('Ctrl Pts',(86.3712365037121,60.7985770797539,11.5963495567324));
#74906=CARTESIAN_POINT('Ctrl Pts',(86.3912648081972,60.7935281936968,11.5313721138635));
#74907=CARTESIAN_POINT('Ctrl Pts',(86.4150508733927,60.7884793076398,11.4679019972601));
#74908=CARTESIAN_POINT('Ctrl Pts',(86.426592213064,60.7860295157778,11.4371053871997));
#74909=CARTESIAN_POINT('Ctrl Pts',(86.4390175462652,60.7835797239157,11.4066633072305));
#74910=CARTESIAN_POINT('Ctrl Pts',(86.4523032711897,60.7811299320537,11.3766239464587));
#74911=CARTESIAN_POINT('Ctrl Pts',(86.4772349598801,60.7765327084616,11.3202527664535));
#74912=CARTESIAN_POINT('Ctrl Pts',(86.5052798154291,60.7719354848695,11.2651201185229));
#74913=CARTESIAN_POINT('Ctrl Pts',(86.5362925101349,60.7673382612775,11.2115922197594));
#74914=CARTESIAN_POINT('Ctrl Pts',(86.5678362265738,60.7626623207063,11.157147777695));
#74915=CARTESIAN_POINT('Ctrl Pts',(86.6024502461152,60.7579863801352,11.1043640807809));
#74916=CARTESIAN_POINT('Ctrl Pts',(86.6399304046922,60.7533104395641,11.0536053139104));
#74917=CARTESIAN_POINT('Ctrl Pts',(86.6766782464991,60.7487258611917,11.0038383116859));
#74918=CARTESIAN_POINT('Ctrl Pts',(86.7161809160319,60.7441412828193,10.956018250926));
#74919=CARTESIAN_POINT('Ctrl Pts',(86.7582009561544,60.7395567044469,10.9104614280174));
#74920=CARTESIAN_POINT('Ctrl Pts',(86.8001953143602,60.7349749280889,10.8649324486456));
#74921=CARTESIAN_POINT('Ctrl Pts',(86.8447036479709,60.730393151731,10.8216643377432));
#74922=CARTESIAN_POINT('Ctrl Pts',(86.8914486848574,60.725811375373,10.7809398113853));
#74923=CARTESIAN_POINT('Ctrl Pts',(86.9381823212695,60.7212307164476,10.7402252171818));
#74924=CARTESIAN_POINT('Ctrl Pts',(86.9871511944086,60.7166500575221,10.7020533102775));
#74925=CARTESIAN_POINT('Ctrl Pts',(87.0380432051213,60.7120693985967,10.6666680483533));
#74926=CARTESIAN_POINT('Ctrl Pts',(87.0907737714519,60.7073232560111,10.6300044370145));
#74927=CARTESIAN_POINT('Ctrl Pts',(87.1455686478471,60.7025771134256,10.5963330541753));
#74928=CARTESIAN_POINT('Ctrl Pts',(87.2020478798997,60.6978309708401,10.565876237444));
#74929=CARTESIAN_POINT('Ctrl Pts',(87.2566269000601,60.6932445095437,10.5364441231253));
#74930=CARTESIAN_POINT('Ctrl Pts',(87.3127782216355,60.6886580482473,10.5100138509726));
#74931=CARTESIAN_POINT('Ctrl Pts',(87.370136273385,60.6840715869509,10.4867379826295));
#74932=CARTESIAN_POINT('Ctrl Pts',(87.4304897742575,60.6792456037208,10.4622465625498));
#74933=CARTESIAN_POINT('Ctrl Pts',(87.4921788951917,60.6744196204907,10.4412482678737));
#74934=CARTESIAN_POINT('Ctrl Pts',(87.554759916953,60.6695936372607,10.423861204946));
#74935=CARTESIAN_POINT('Ctrl Pts',(87.6173409387144,60.6647676540306,10.4064741420184));
#74936=CARTESIAN_POINT('Ctrl Pts',(87.680813211647,60.6599416708005,10.3926983726578));
#74937=CARTESIAN_POINT('Ctrl Pts',(87.744724239612,60.6551156875704,10.3825891603563));
#74938=CARTESIAN_POINT('Ctrl Pts',(87.805605778471,60.6505184639783,10.3729591415448));
#74939=CARTESIAN_POINT('Ctrl Pts',(87.8671353781665,60.6459212403862,10.3666163383851));
#74940=CARTESIAN_POINT('Ctrl Pts',(87.9289265464004,60.6413240167941,10.3636372936961));
#74941=CARTESIAN_POINT('Ctrl Pts',(87.9917757475964,60.636648076223,10.3606072396547));
#74942=CARTESIAN_POINT('Ctrl Pts',(88.0548950502372,60.6319721356519,10.3610573983662));
#74943=CARTESIAN_POINT('Ctrl Pts',(88.1178677565465,60.6272961950808,10.3650137807111));
#74944=CARTESIAN_POINT('Ctrl Pts',(88.1796100526699,60.6227116167083,10.368892860151));
#74945=CARTESIAN_POINT('Ctrl Pts',(88.2412108972013,60.6181270383359,10.3761423473277));
#74946=CARTESIAN_POINT('Ctrl Pts',(88.302275766393,60.6135424599635,10.386734308243));
#74947=CARTESIAN_POINT('Ctrl Pts',(88.3633033138001,60.6089606836056,10.3973197955362));
#74948=CARTESIAN_POINT('Ctrl Pts',(88.4237950348914,60.6043789072476,10.4112436190516));
#74949=CARTESIAN_POINT('Ctrl Pts',(88.4833630218469,60.5997971308896,10.4284261814527));
#74950=CARTESIAN_POINT('Ctrl Pts',(88.5429164809861,60.5952164719642,10.4456045532621));
#74951=CARTESIAN_POINT('Ctrl Pts',(88.60154616433,60.5906358130387,10.466039945214));
#74952=CARTESIAN_POINT('Ctrl Pts',(88.6588778356715,60.5860551541133,10.4896024785462));
#74953=CARTESIAN_POINT('Ctrl Pts',(88.7182807057128,60.5813090115278,10.5140162462357));
#74954=CARTESIAN_POINT('Ctrl Pts',(88.7762894204689,60.5765628689422,10.5417872655508));
#74955=CARTESIAN_POINT('Ctrl Pts',(88.8325111026076,60.5718167263567,10.5727169243936));
#74956=CARTESIAN_POINT('Ctrl Pts',(88.8868412379758,60.5672302650603,10.6026059723178));
#74957=CARTESIAN_POINT('Ctrl Pts',(88.9395022765314,60.5626438037639,10.6354441394256));
#74958=CARTESIAN_POINT('Ctrl Pts',(88.9901677626185,60.5580573424675,10.6710070508248));
#74959=CARTESIAN_POINT('Ctrl Pts',(89.0434791873529,60.5532313592375,10.70842718869));
#74960=CARTESIAN_POINT('Ctrl Pts',(89.0945804021524,60.5484053760074,10.7488640761435));
#74961=CARTESIAN_POINT('Ctrl Pts',(89.1431315106124,60.5435793927773,10.7920089959978));
#74962=CARTESIAN_POINT('Ctrl Pts',(89.1916826190724,60.5387534095473,10.835153915852));
#74963=CARTESIAN_POINT('Ctrl Pts',(89.2376832168851,60.5339274263172,10.8810063558477));
#74964=CARTESIAN_POINT('Ctrl Pts',(89.280841442675,60.5291014430871,10.9292161392485));
#74965=CARTESIAN_POINT('Ctrl Pts',(89.3219538967252,60.5245042194951,10.9751406986705));
#74966=CARTESIAN_POINT('Ctrl Pts',(89.3606561987092,60.519906995903,11.0233926894249));
#74967=CARTESIAN_POINT('Ctrl Pts',(89.3966744104397,60.5153097723109,11.0736889278797));
#74968=CARTESIAN_POINT('Ctrl Pts',(89.433309351977,60.5106338317398,11.1248463748159));
#74969=CARTESIAN_POINT('Ctrl Pts',(89.4671669957909,60.5059578911687,11.1781184027865));
#74970=CARTESIAN_POINT('Ctrl Pts',(89.4979994732315,60.5012819505975,11.2331690434372));
#74971=CARTESIAN_POINT('Ctrl Pts',(89.5282295215163,60.4966973722251,11.2871440614417));
#74972=CARTESIAN_POINT('Ctrl Pts',(89.5555512957382,60.4921127938527,11.3428283479567));
#74973=CARTESIAN_POINT('Ctrl Pts',(89.5797742746477,60.4875282154803,11.399875303863));
#74974=CARTESIAN_POINT('Ctrl Pts',(89.6039824488944,60.4829464391223,11.4568873936634));
#74975=CARTESIAN_POINT('Ctrl Pts',(89.6250953846744,60.4783646627644,11.5152600338695));
#74976=CARTESIAN_POINT('Ctrl Pts',(89.6429695526732,60.4737828864064,11.5746241614126));
#74977=CARTESIAN_POINT('Ctrl Pts',(89.6608393614073,60.469202227481,11.6339738108579));
#74978=CARTESIAN_POINT('Ctrl Pts',(89.6754718237169,60.4646215685555,11.6943139803969));
#74979=CARTESIAN_POINT('Ctrl Pts',(89.6867730682438,60.4600409096301,11.7552598201892));
#74980=CARTESIAN_POINT('Ctrl Pts',(89.6984825883786,60.4552947670445,11.8184074263208));
#74981=CARTESIAN_POINT('Ctrl Pts',(89.7066154222443,60.450548624459,11.8822047422107));
#74982=CARTESIAN_POINT('Ctrl Pts',(89.7111253318904,60.4458024818735,11.9462139763385));
#74983=CARTESIAN_POINT('Ctrl Pts',(89.7154835081713,60.4412160205771,12.0080696559035));
#74984=CARTESIAN_POINT('Ctrl Pts',(89.7164587509438,60.4366295592807,12.0701226904972));
#74985=CARTESIAN_POINT('Ctrl Pts',(89.7140624931613,60.4320430979843,12.1319771171478));
#74986=CARTESIAN_POINT('Ctrl Pts',(89.7115410939549,60.4272171147543,12.1970618102108));
#74987=CARTESIAN_POINT('Ctrl Pts',(89.7052864444172,60.4223911315242,12.2619259403604));
#74988=CARTESIAN_POINT('Ctrl Pts',(89.6953735450039,60.4175651482941,12.3261165056106));
#74989=CARTESIAN_POINT('Ctrl Pts',(89.6854606455906,60.4127391650641,12.3903070708608));
#74990=CARTESIAN_POINT('Ctrl Pts',(89.6718897073655,60.407913181834,12.4538234536952));
#74991=CARTESIAN_POINT('Ctrl Pts',(89.6547966159694,60.4030871986039,12.5162305197647));
#74992=CARTESIAN_POINT('Ctrl Pts',(89.638513765557,60.3984899750119,12.5756793870255));
#74993=CARTESIAN_POINT('Ctrl Pts',(89.6189683273089,60.3938927514198,12.634365830386));
#74994=CARTESIAN_POINT('Ctrl Pts',(89.5962496260556,60.3892955278277,12.6919061101239));
#74995=CARTESIAN_POINT('Ctrl Pts',(89.5731419188089,60.3846195872566,12.7504316360445));
#74996=CARTESIAN_POINT('Ctrl Pts',(89.5467513044177,60.3799436466855,12.8077708414871));
#74997=CARTESIAN_POINT('Ctrl Pts',(89.5172255933602,60.3752677061143,12.8635332579315));
#74998=CARTESIAN_POINT('Ctrl Pts',(89.4882767788307,60.3706831277419,12.9182061444953));
#74999=CARTESIAN_POINT('Ctrl Pts',(89.4563145273844,60.3660985493695,12.9713628335739));
#75000=CARTESIAN_POINT('Ctrl Pts',(89.4215266857891,60.3615139709971,13.0226552692985));
#75001=CARTESIAN_POINT('Ctrl Pts',(89.3867601059168,60.3569321946391,13.0739163559798));
#75002=CARTESIAN_POINT('Ctrl Pts',(89.3491716453288,60.3523504182812,13.1233150281532));
#75003=CARTESIAN_POINT('Ctrl Pts',(89.3089935115999,60.3477686419232,13.1705305244512));
#75004=CARTESIAN_POINT('Ctrl Pts',(89.2688251767677,60.3431879829978,13.2177345055362));
#75005=CARTESIAN_POINT('Ctrl Pts',(89.2260687523383,60.3386073240723,13.262755980226));
#75006=CARTESIAN_POINT('Ctrl Pts',(89.1809966431017,60.3340266651469,13.3053073431279));
#75007=CARTESIAN_POINT('Ctrl Pts',(89.1342962315347,60.3292805225614,13.3493959423505));
#75008=CARTESIAN_POINT('Ctrl Pts',(89.0851099948366,60.3245343799758,13.3908320934861));
#75009=CARTESIAN_POINT('Ctrl Pts',(89.0337806515249,60.3197882373903,13.4293394934741));
#75010=CARTESIAN_POINT('Ctrl Pts',(88.9841782550046,60.3152017760939,13.4665513337187));
#75011=CARTESIAN_POINT('Ctrl Pts',(88.9325751573961,60.3106153147975,13.5010281450264));
#75012=CARTESIAN_POINT('Ctrl Pts',(88.8793102167946,60.3060288535011,13.5325647626375));
#75013=CARTESIAN_POINT('Ctrl Pts',(88.8232635844387,60.3012028702711,13.5657483387955));
#75014=CARTESIAN_POINT('Ctrl Pts',(88.765377341294,60.296376887041,13.5956758992624));
#75015=CARTESIAN_POINT('Ctrl Pts',(88.7060727440737,60.2915509038109,13.622164745792));
#75016=CARTESIAN_POINT('Ctrl Pts',(88.6467681468534,60.2867249205809,13.6486535923216));
#75017=CARTESIAN_POINT('Ctrl Pts',(88.586045828827,60.2818989373508,13.671703567293));
#75018=CARTESIAN_POINT('Ctrl Pts',(88.5243450597767,60.2770729541207,13.691192814777));
#75019=CARTESIAN_POINT('Ctrl Pts',(88.4655690098809,60.2724757305286,13.7097582394902));
#75020=CARTESIAN_POINT('Ctrl Pts',(88.4056638648384,60.2678785069365,13.7251691573103));
#75021=CARTESIAN_POINT('Ctrl Pts',(88.3450004621917,60.2632812833445,13.7372924719677));
#75022=CARTESIAN_POINT('Ctrl Pts',(88.2832983369987,60.2586053427733,13.749623370765));
#75023=CARTESIAN_POINT('Ctrl Pts',(88.2208122199804,60.2539294022022,13.7585527710084));
#75024=CARTESIAN_POINT('Ctrl Pts',(88.1579503242277,60.2492534616311,13.7639930617672));
#75025=CARTESIAN_POINT('Ctrl Pts',(88.0963166735571,60.2446688832587,13.7693270558531));
#75026=CARTESIAN_POINT('Ctrl Pts',(88.034322328037,60.2400843048863,13.7713070141474));
#75027=CARTESIAN_POINT('Ctrl Pts',(87.9723615846257,60.2354997265138,13.769901965624));
#75028=CARTESIAN_POINT('Ctrl Pts',(87.9104387105417,60.2309179501559,13.7684977758418));
#75029=CARTESIAN_POINT('Ctrl Pts',(87.8485499057051,60.2263361737979,13.7637126930032));
#75030=CARTESIAN_POINT('Ctrl Pts',(87.787090597633,60.2217543974399,13.7555678190388));
#75031=CARTESIAN_POINT('Ctrl Pts',(87.7256462786444,60.2171737385145,13.7474249314977));
#75032=CARTESIAN_POINT('Ctrl Pts',(87.664631752888,60.212593079589,13.7359239463246));
#75033=CARTESIAN_POINT('Ctrl Pts',(87.6044363957642,60.2080124206636,13.7211377197414));
#75034=CARTESIAN_POINT('Ctrl Pts',(87.5420663846926,60.2032662780781,13.7058173169767));
#75035=CARTESIAN_POINT('Ctrl Pts',(87.4805764429374,60.1985201354926,13.6869698353306));
#75036=CARTESIAN_POINT('Ctrl Pts',(87.4203845886494,60.193773992907,13.6647333334472));
#75037=CARTESIAN_POINT('Ctrl Pts',(87.3622178553335,60.1891875316106,13.6432449661219));
#75038=CARTESIAN_POINT('Ctrl Pts',(87.305263699935,60.1846010703142,13.6185922911435));
#75039=CARTESIAN_POINT('Ctrl Pts',(87.2498782819239,60.1800146090178,13.5909487092597));
#75040=CARTESIAN_POINT('Ctrl Pts',(87.1916004330032,60.1751886257878,13.5618614775207));
#75041=CARTESIAN_POINT('Ctrl Pts',(87.135060229181,60.1703626425577,13.5294626909284));
#75042=CARTESIAN_POINT('Ctrl Pts',(87.0806396482421,60.1655366593276,13.4940071608633));
#75043=CARTESIAN_POINT('Ctrl Pts',(87.0262190673033,60.1607106760976,13.4585516307983));
#75044=CARTESIAN_POINT('Ctrl Pts',(86.9739185851529,60.1558846928675,13.42003980379));
#75045=CARTESIAN_POINT('Ctrl Pts',(86.9240788349235,60.1510587096374,13.3787746251771));
#75046=CARTESIAN_POINT('Ctrl Pts',(86.8762830329794,60.1464306419287,13.3392017482045));
#75047=CARTESIAN_POINT('Ctrl Pts',(86.8305379272261,60.1418025742199,13.2969210980014));
#75048=CARTESIAN_POINT('Ctrl Pts',(86.787171265087,60.1371745065111,13.2521779222365));
#75049=CARTESIAN_POINT('Ctrl Pts',(86.7447554783474,60.1326479157322,13.2084158038791));
#75050=CARTESIAN_POINT('Ctrl Pts',(86.7046152985981,60.1281213249533,13.162298431376));
#75051=CARTESIAN_POINT('Ctrl Pts',(86.6670253249706,60.1235947341743,13.1140968030099));
#75052=CARTESIAN_POINT('Ctrl Pts',(86.6294715645995,60.1190725042017,13.0659416109076));
#75053=CARTESIAN_POINT('Ctrl Pts',(86.5944634655044,60.114550274229,13.015706550762));
#75054=CARTESIAN_POINT('Ctrl Pts',(86.5622372035043,60.1100280442564,12.9636977192184));
#75055=CARTESIAN_POINT('Ctrl Pts',(86.5300293850305,60.1055084024172,12.9117186530337));
#75056=CARTESIAN_POINT('Ctrl Pts',(86.5006005239128,60.100988760578,12.8579682721358));
#75057=CARTESIAN_POINT('Ctrl Pts',(86.4741437523452,60.0964691187388,12.80278199601));
#75058=CARTESIAN_POINT('Ctrl Pts',(86.4465902196966,60.0917621158962,12.7453079819525));
#75059=CARTESIAN_POINT('Ctrl Pts',(86.4222609259181,60.0870551130535,12.6862769207695));
#75060=CARTESIAN_POINT('Ctrl Pts',(86.40132014105,60.0823481102108,12.6260942664325));
#75061=CARTESIAN_POINT('Ctrl Pts',(86.3812012386156,60.0778258474807,12.5682736566287));
#75062=CARTESIAN_POINT('Ctrl Pts',(86.3642098974303,60.0733035847505,12.5093907181173));
#75063=CARTESIAN_POINT('Ctrl Pts',(86.3504409737101,60.0687813220203,12.4498209944845));
#75064=CARTESIAN_POINT('Ctrl Pts',(86.3366653153358,60.0642568473616,12.3902221341168));
#75065=CARTESIAN_POINT('Ctrl Pts',(86.3261152994707,60.059732372703,12.3299363366975));
#75066=CARTESIAN_POINT('Ctrl Pts',(86.318834348335,60.0552078980443,12.2693475913923));
#75067=CARTESIAN_POINT('Ctrl Pts',(86.3115430861579,60.0506770159747,12.2086730423168));
#75068=CARTESIAN_POINT('Ctrl Pts',(86.3075301486019,60.0461461339052,12.1476952119335));
#75069=CARTESIAN_POINT('Ctrl Pts',(86.3067869250066,60.0416152518357,12.086799774553));
#75070=CARTESIAN_POINT('Ctrl Pts',(86.306697790138,60.0410718627661,12.0794965796007));
#75071=CARTESIAN_POINT('Ctrl Pts',(86.306655622955,60.0405284736965,12.0721945642732));
#75072=CARTESIAN_POINT('Ctrl Pts',(86.3066603586072,60.0399850846269,12.0648943883225));
#75073=CARTESIAN_POINT('',(86.3066606119916,59.2462350845034,12.0674443279418));
#75074=CARTESIAN_POINT('Ctrl Pts',(86.3066603586077,60.0399850845702,12.0648943875605));
#75075=CARTESIAN_POINT('Ctrl Pts',(86.3067037612879,60.0350048780982,11.9979876616978));
#75076=CARTESIAN_POINT('Ctrl Pts',(86.3106868359654,60.0300246716262,11.9312088054057));
#75077=CARTESIAN_POINT('Ctrl Pts',(86.3185655492583,60.0250444651542,11.8649018509712));
#75078=CARTESIAN_POINT('Ctrl Pts',(86.3258383815855,60.0204472415621,11.8036939679327));
#75079=CARTESIAN_POINT('Ctrl Pts',(86.3364508532806,60.01585001797,11.7427554888319));
#75080=CARTESIAN_POINT('Ctrl Pts',(86.3503716237528,60.011252794378,11.6824791640566));
#75081=CARTESIAN_POINT('Ctrl Pts',(86.3645307557003,60.0065768538068,11.6211707445617));
#75082=CARTESIAN_POINT('Ctrl Pts',(86.3821125786744,60.0019009132357,11.5605479063764));
#75083=CARTESIAN_POINT('Ctrl Pts',(86.40302891446,59.9972249726646,11.5010187404283));
#75084=CARTESIAN_POINT('Ctrl Pts',(86.4235365704521,59.9926403942921,11.4426527020705));
#75085=CARTESIAN_POINT('Ctrl Pts',(86.4472494296751,59.9880558159197,11.3853384855202));
#75086=CARTESIAN_POINT('Ctrl Pts',(86.4740334224729,59.9834712375473,11.3294481856891));
#75087=CARTESIAN_POINT('Ctrl Pts',(86.5008010453608,59.9788894611894,11.2735920450358));
#75088=CARTESIAN_POINT('Ctrl Pts',(86.5306358604229,59.9743076848315,11.21915855358));
#75089=CARTESIAN_POINT('Ctrl Pts',(86.563355875376,59.9697259084735,11.1664994029787));
#75090=CARTESIAN_POINT('Ctrl Pts',(86.5960679103656,59.9651452495481,11.1138530952231));
#75091=CARTESIAN_POINT('Ctrl Pts',(86.6316634798331,59.9605645906227,11.062980701457));
#75092=CARTESIAN_POINT('Ctrl Pts',(86.6699159157286,59.9559839316972,11.0142070952351));
#75093=CARTESIAN_POINT('Ctrl Pts',(86.709550282303,59.9512377891117,10.9636714641595));
#75094=CARTESIAN_POINT('Ctrl Pts',(86.7520368494761,59.9464916465262,10.9153896651943));
#75095=CARTESIAN_POINT('Ctrl Pts',(86.7970777366679,59.9417455039407,10.8696858380063));
#75096=CARTESIAN_POINT('Ctrl Pts',(86.8406032486259,59.9371590426443,10.8255196902942));
#75097=CARTESIAN_POINT('Ctrl Pts',(86.8865134825776,59.9325725813479,10.7837610909495));
#75098=CARTESIAN_POINT('Ctrl Pts',(86.9345038099913,59.9279861200516,10.7446632569641));
#75099=CARTESIAN_POINT('Ctrl Pts',(86.9850003693947,59.9231601368215,10.7035235898105));
#75100=CARTESIAN_POINT('Ctrl Pts',(87.0377997247886,59.9183341535914,10.6653306049712));
#75101=CARTESIAN_POINT('Ctrl Pts',(87.092512426132,59.9135081703613,10.630327540053));
#75102=CARTESIAN_POINT('Ctrl Pts',(87.1472251274755,59.9086821871312,10.5953244751349));
#75103=CARTESIAN_POINT('Ctrl Pts',(87.2038505719327,59.9038562039012,10.5635115800648));
#75104=CARTESIAN_POINT('Ctrl Pts',(87.2619724597879,59.8990302206711,10.5350746002487));
#75105=CARTESIAN_POINT('Ctrl Pts',(87.3173392734142,59.894432997079,10.5079855806095));
#75106=CARTESIAN_POINT('Ctrl Pts',(87.374291171351,59.8898357734869,10.4838483870692));
#75107=CARTESIAN_POINT('Ctrl Pts',(87.4324811965851,59.8852385498949,10.4628497170585));
#75108=CARTESIAN_POINT('Ctrl Pts',(87.4916675934129,59.8805626093237,10.4414914926702));
#75109=CARTESIAN_POINT('Ctrl Pts',(87.5521344822472,59.8758866687526,10.4233806019292));
#75110=CARTESIAN_POINT('Ctrl Pts',(87.6134911895053,59.8712107281815,10.4086643124644));
#75111=CARTESIAN_POINT('Ctrl Pts',(87.673649061236,59.8666261498091,10.3942355614193));
#75112=CARTESIAN_POINT('Ctrl Pts',(87.7346617734659,59.8620415714367,10.3830700763129));
#75113=CARTESIAN_POINT('Ctrl Pts',(87.7961440021667,59.8574569930643,10.3752570462087));
#75114=CARTESIAN_POINT('Ctrl Pts',(87.8575886540001,59.8528752167063,10.3674487912923));
#75115=CARTESIAN_POINT('Ctrl Pts',(87.9195017493652,59.8482934403483,10.3629889926218));
#75116=CARTESIAN_POINT('Ctrl Pts',(87.9814891122661,59.8437116639904,10.3619155117468));
#75117=CARTESIAN_POINT('Ctrl Pts',(88.0434613572981,59.8391310050649,10.3608422926791));
#75118=CARTESIAN_POINT('Ctrl Pts',(88.1055073251662,59.8345503461395,10.3631537607271));
#75119=CARTESIAN_POINT('Ctrl Pts',(88.1672311382493,59.829969687214,10.3688356982775));
#75120=CARTESIAN_POINT('Ctrl Pts',(88.2311848232063,59.8252235446285,10.3747229049468));
#75121=CARTESIAN_POINT('Ctrl Pts',(88.2947920461684,59.820477402043,10.3842287814717));
#75122=CARTESIAN_POINT('Ctrl Pts',(88.3576189204811,59.8157312594575,10.3972788850247));
#75123=CARTESIAN_POINT('Ctrl Pts',(88.4183320200597,59.8111447981611,10.4098899252076));
#75124=CARTESIAN_POINT('Ctrl Pts',(88.4783159575446,59.8065583368647,10.4258102720808));
#75125=CARTESIAN_POINT('Ctrl Pts',(88.537192769841,59.8019718755683,10.4449213453484));
#75126=CARTESIAN_POINT('Ctrl Pts',(88.5991443465405,59.7971458923382,10.465030469385));
#75127=CARTESIAN_POINT('Ctrl Pts',(88.6598693867404,59.7923199091081,10.4886724979279));
#75128=CARTESIAN_POINT('Ctrl Pts',(88.7189523041574,59.787493925878,10.5156521775298));
#75129=CARTESIAN_POINT('Ctrl Pts',(88.7780352215745,59.782667942648,10.5426318571317));
#75130=CARTESIAN_POINT('Ctrl Pts',(88.8354754792623,59.7778419594179,10.5729488168974));
#75131=CARTESIAN_POINT('Ctrl Pts',(88.8908912281221,59.7730159761878,10.6063540627009));
#75132=CARTESIAN_POINT('Ctrl Pts',(88.943680178246,59.7684187525957,10.63817584425));
#75133=CARTESIAN_POINT('Ctrl Pts',(88.9948489845408,59.7638215290036,10.6729303555109));
#75134=CARTESIAN_POINT('Ctrl Pts',(89.0440526094874,59.7592243054116,10.7104273750067));
#75135=CARTESIAN_POINT('Ctrl Pts',(89.0940987343988,59.7545483648404,10.7485664455229));
#75136=CARTESIAN_POINT('Ctrl Pts',(89.1421112428444,59.7498724242693,10.7895426342364));
#75137=CARTESIAN_POINT('Ctrl Pts',(89.1877545113035,59.7451964836982,10.8331076057794));
#75138=CARTESIAN_POINT('Ctrl Pts',(89.2325059657415,59.7406119053258,10.8758213706986));
#75139=CARTESIAN_POINT('Ctrl Pts',(89.2749795458075,59.7360273269534,10.9210232966276));
#75140=CARTESIAN_POINT('Ctrl Pts',(89.3148913226047,59.731442748581,10.9684380407302));
#75141=CARTESIAN_POINT('Ctrl Pts',(89.354778706019,59.726860972223,11.0158238057671));
#75142=CARTESIAN_POINT('Ctrl Pts',(89.3921070636436,59.722279195865,11.0654193186582));
#75143=CARTESIAN_POINT('Ctrl Pts',(89.4266307866161,59.7176974195071,11.1169139598621));
#75144=CARTESIAN_POINT('Ctrl Pts',(89.4611460897254,59.7131167605816,11.1683960422282));
#75145=CARTESIAN_POINT('Ctrl Pts',(89.4928578327069,59.7085361016562,11.2217759108146));
#75146=CARTESIAN_POINT('Ctrl Pts',(89.5215632365467,59.7039554427307,11.2767132688348));
#75147=CARTESIAN_POINT('Ctrl Pts',(89.5513056692001,59.6992093001452,11.3336353271409));
#75148=CARTESIAN_POINT('Ctrl Pts',(89.5778200601397,59.6944631575597,11.3922290774437));
#75149=CARTESIAN_POINT('Ctrl Pts',(89.6009336107763,59.6897170149742,11.4520896246815));
#75150=CARTESIAN_POINT('Ctrl Pts',(89.6232695190444,59.6851305536778,11.5099361975859));
#75151=CARTESIAN_POINT('Ctrl Pts',(89.6424297120832,59.6805440923814,11.5689651498336));
#75152=CARTESIAN_POINT('Ctrl Pts',(89.6583088049945,59.675957631085,11.6287946288214));
#75153=CARTESIAN_POINT('Ctrl Pts',(89.6750171627342,59.671131647855,11.6917486239822));
#75154=CARTESIAN_POINT('Ctrl Pts',(89.688092180723,59.6663056646249,11.7555884228971));
#75155=CARTESIAN_POINT('Ctrl Pts',(89.6974724820299,59.6614796813948,11.8198589775027));
#75156=CARTESIAN_POINT('Ctrl Pts',(89.7068527833367,59.6566536981648,11.8841295321083));
#75157=CARTESIAN_POINT('Ctrl Pts',(89.7125383883193,59.6518277149347,11.9488301901317));
#75158=CARTESIAN_POINT('Ctrl Pts',(89.7145313677356,59.6470017317046,12.0135050979548));
#75159=CARTESIAN_POINT('Ctrl Pts',(89.7164298766103,59.6424045081125,12.0751143074951));
#75160=CARTESIAN_POINT('Ctrl Pts',(89.7149857731566,59.6378072845205,12.1369531088728));
#75161=CARTESIAN_POINT('Ctrl Pts',(89.7101717185409,59.6332100609284,12.1986284528696));
#75162=CARTESIAN_POINT('Ctrl Pts',(89.705275234209,59.6285341203573,12.2613598466025));
#75163=CARTESIAN_POINT('Ctrl Pts',(89.6968921957595,59.6238581797861,12.3239216054898));
#75164=CARTESIAN_POINT('Ctrl Pts',(89.6850491932099,59.619182239215,12.38589706831));
#75165=CARTESIAN_POINT('Ctrl Pts',(89.6734375885439,59.6145976608426,12.4466616058708));
#75166=CARTESIAN_POINT('Ctrl Pts',(89.6585001108952,59.6100130824702,12.5068620284009));
#75167=CARTESIAN_POINT('Ctrl Pts',(89.6403140789271,59.6054285040978,12.5661104556095));
#75168=CARTESIAN_POINT('Ctrl Pts',(89.622139161945,59.6008467277398,12.6253226712111));
#75169=CARTESIAN_POINT('Ctrl Pts',(89.6007197765852,59.5962649513818,12.6835835595728));
#75170=CARTESIAN_POINT('Ctrl Pts',(89.5761836629574,59.5916831750239,12.7405182998342));
#75171=CARTESIAN_POINT('Ctrl Pts',(89.5516535333517,59.5871025160984,12.7974391544923));
#75172=CARTESIAN_POINT('Ctrl Pts',(89.524008385819,59.582521857173,12.8530340358315));
#75173=CARTESIAN_POINT('Ctrl Pts',(89.4934241238076,59.5779411982475,12.9069480083532));
#75174=CARTESIAN_POINT('Ctrl Pts',(89.4617349562139,59.573195055662,12.9628097097161));
#75175=CARTESIAN_POINT('Ctrl Pts',(89.4268904789498,59.5684489130765,13.0168661885659));
#75176=CARTESIAN_POINT('Ctrl Pts',(89.3891371271877,59.563702770491,13.0687526585689));
#75177=CARTESIAN_POINT('Ctrl Pts',(89.3526539656419,59.5591163091946,13.1188934375673));
#75178=CARTESIAN_POINT('Ctrl Pts',(89.3134549581655,59.5545298478982,13.167007552062));
#75179=CARTESIAN_POINT('Ctrl Pts',(89.2718037465764,59.5499433866018,13.2127993495895));
#75180=CARTESIAN_POINT('Ctrl Pts',(89.2279773550185,59.5451174033717,13.2609825637628));
#75181=CARTESIAN_POINT('Ctrl Pts',(89.181436061987,59.5402914201416,13.306593791151));
#75182=CARTESIAN_POINT('Ctrl Pts',(89.1325288722219,59.5354654369115,13.3493346501878));
#75183=CARTESIAN_POINT('Ctrl Pts',(89.0836216824568,59.5306394536815,13.3920755092247));
#75184=CARTESIAN_POINT('Ctrl Pts',(89.0323491549886,59.5258134704514,13.4319456632212));
#75185=CARTESIAN_POINT('Ctrl Pts',(88.9790953852693,59.5209874872213,13.4686995974264));
#75186=CARTESIAN_POINT('Ctrl Pts',(88.928365932876,59.5163902636292,13.5037113339731));
#75187=CARTESIAN_POINT('Ctrl Pts',(88.8756305667272,59.5117930400372,13.5360394014651));
#75188=CARTESIAN_POINT('Ctrl Pts',(88.8212046672429,59.5071958164451,13.5654476425597));
#75189=CARTESIAN_POINT('Ctrl Pts',(88.7658468482415,59.502519875874,13.5953594327751));
#75190=CARTESIAN_POINT('Ctrl Pts',(88.7087404404245,59.4978439353028,13.6222500853325));
#75191=CARTESIAN_POINT('Ctrl Pts',(88.6502499120977,59.4931679947317,13.6459159425371));
#75192=CARTESIAN_POINT('Ctrl Pts',(88.5929022176438,59.4885834163593,13.6691193976398));
#75193=CARTESIAN_POINT('Ctrl Pts',(88.5342244987779,59.4839988379869,13.6892227411431));
#75194=CARTESIAN_POINT('Ctrl Pts',(88.4745845594918,59.4794142596145,13.7060805443029));
#75195=CARTESIAN_POINT('Ctrl Pts',(88.4149810710979,59.4748324832565,13.722928044267));
#75196=CARTESIAN_POINT('Ctrl Pts',(88.3544170172239,59.4702507068986,13.7365337989402));
#75197=CARTESIAN_POINT('Ctrl Pts',(88.2932765788874,59.4656689305406,13.7468018231224));
#75198=CARTESIAN_POINT('Ctrl Pts',(88.2321510518664,59.4610882716152,13.7570673430741));
#75199=CARTESIAN_POINT('Ctrl Pts',(88.1704499212321,59.4565076126897,13.7639966642296));
#75200=CARTESIAN_POINT('Ctrl Pts',(88.1085667856242,59.4519269537643,13.7675450502243));
#75201=CARTESIAN_POINT('Ctrl Pts',(88.0444480223602,59.4471808111788,13.7712216273617));
#75202=CARTESIAN_POINT('Ctrl Pts',(87.9801344286854,59.4424346685933,13.7712682115861));
#75203=CARTESIAN_POINT('Ctrl Pts',(87.9160661354544,59.4376885260077,13.7676939786467));
#75204=CARTESIAN_POINT('Ctrl Pts',(87.8541533837963,59.4331020647113,13.7642399987577));
#75205=CARTESIAN_POINT('Ctrl Pts',(87.7924702044208,59.428515603415,13.7574051188854));
#75206=CARTESIAN_POINT('Ctrl Pts',(87.7314079802175,59.4239291421186,13.7472504685721));
#75207=CARTESIAN_POINT('Ctrl Pts',(87.667156861337,59.4191031588885,13.7365655049472));
#75208=CARTESIAN_POINT('Ctrl Pts',(87.6035939638048,59.4142771756584,13.7222046526664));
#75209=CARTESIAN_POINT('Ctrl Pts',(87.5411592640312,59.4094511924283,13.7042992762082));
#75210=CARTESIAN_POINT('Ctrl Pts',(87.4787245642576,59.4046252091983,13.6863938997501));
#75211=CARTESIAN_POINT('Ctrl Pts',(87.4174186483194,59.3997992259682,13.6649442861482));
#75212=CARTESIAN_POINT('Ctrl Pts',(87.3576561112549,59.3949732427381,13.6401399552262));
#75213=CARTESIAN_POINT('Ctrl Pts',(87.3007264179224,59.390376019146,13.6165113908768));
#75214=CARTESIAN_POINT('Ctrl Pts',(87.2449633266387,59.385778795554,13.5897419971388));
#75215=CARTESIAN_POINT('Ctrl Pts',(87.1907363001367,59.3811815719619,13.559968640329));
#75216=CARTESIAN_POINT('Ctrl Pts',(87.1355807593645,59.3765056313907,13.5296854826238));
#75217=CARTESIAN_POINT('Ctrl Pts',(87.0820149078883,59.3718296908196,13.4962946371064));
#75218=CARTESIAN_POINT('Ctrl Pts',(87.0304075300075,59.3671537502485,13.4599918376354));
#75219=CARTESIAN_POINT('Ctrl Pts',(86.9798084976009,59.3625691718761,13.4243983507675));
#75220=CARTESIAN_POINT('Ctrl Pts',(86.9310925309854,59.3579845935037,13.3860059855364));
#75221=CARTESIAN_POINT('Ctrl Pts',(86.8845813043578,59.3534000151312,13.3450448614915));
#75222=CARTESIAN_POINT('Ctrl Pts',(86.8380985045819,59.3488182387733,13.3041087721722));
#75223=CARTESIAN_POINT('Ctrl Pts',(86.7938181541273,59.3442364624153,13.2606073728211));
#75224=CARTESIAN_POINT('Ctrl Pts',(86.7520292715015,59.3396546860573,13.2148113597906));
#75225=CARTESIAN_POINT('Ctrl Pts',(86.7102505806119,59.3350740271319,13.1690265157805));
#75226=CARTESIAN_POINT('Ctrl Pts',(86.6709624942735,59.3304933682064,13.1209485448884));
#75227=CARTESIAN_POINT('Ctrl Pts',(86.6344160838686,59.325912709281,13.0708838527156));
#75228=CARTESIAN_POINT('Ctrl Pts',(86.5965493756957,59.3211665666955,13.0190104931359));
#75229=CARTESIAN_POINT('Ctrl Pts',(86.5616266256454,59.3164204241099,12.9650045487374));
#75230=CARTESIAN_POINT('Ctrl Pts',(86.5298788514076,59.3116742815244,12.909240759684));
#75231=CARTESIAN_POINT('Ctrl Pts',(86.4991992131193,59.307087820228,12.8553531118466));
#75232=CARTESIAN_POINT('Ctrl Pts',(86.4714844602057,59.3025013589316,12.799824536575));
#75233=CARTESIAN_POINT('Ctrl Pts',(86.4468955220396,59.2979148976352,12.743016999509));
#75234=CARTESIAN_POINT('Ctrl Pts',(86.4210224587854,59.2930889144052,12.6832427632287));
#75235=CARTESIAN_POINT('Ctrl Pts',(86.398610877821,59.2882629311751,12.6220529188133));
#75236=CARTESIAN_POINT('Ctrl Pts',(86.3797890597276,59.283436947945,12.5598883516905));
#75237=CARTESIAN_POINT('Ctrl Pts',(86.3609672416341,59.2786109647149,12.4977237845676));
#75238=CARTESIAN_POINT('Ctrl Pts',(86.3457352631559,59.2737849814849,12.4345851427995));
#75239=CARTESIAN_POINT('Ctrl Pts',(86.3341587805129,59.2689589982548,12.370923531773));
#75240=CARTESIAN_POINT('Ctrl Pts',(86.317476416287,59.2620044843083,12.2791835607388));
#75241=CARTESIAN_POINT('Ctrl Pts',(86.3083194512944,59.2550499703619,12.1860357551626));
#75242=CARTESIAN_POINT('Ctrl Pts',(86.3068657192959,59.2480954564154,12.092479972224));
#75243=CARTESIAN_POINT('Ctrl Pts',(86.3067360921165,59.247475332467,12.0841377383939));
#75244=CARTESIAN_POINT('Ctrl Pts',(86.3066676863994,59.2468552085185,12.0757922827587));
#75245=CARTESIAN_POINT('Ctrl Pts',(86.3066606119924,59.2462350845701,12.0674443288396));
#75246=CARTESIAN_POINT('',(86.3066600110215,58.4524850846251,12.0661938267317));
#75247=CARTESIAN_POINT('Ctrl Pts',(86.3066606119916,59.2462350845034,12.0674443279418));
#75248=CARTESIAN_POINT('Ctrl Pts',(86.3066090340479,59.2417138945661,12.0065811967051));
#75249=CARTESIAN_POINT('Ctrl Pts',(86.3098218829355,59.2371927046287,11.9456054229486));
#75250=CARTESIAN_POINT('Ctrl Pts',(86.316308791185,59.2326715146914,11.8849018432859));
#75251=CARTESIAN_POINT('Ctrl Pts',(86.3227894495779,59.2281546807257,11.8242567489068));
#75252=CARTESIAN_POINT('Ctrl Pts',(86.3325378663834,59.2236378467601,11.7638838491837));
#75253=CARTESIAN_POINT('Ctrl Pts',(86.3455116517119,59.2191210127945,11.7041666166359));
#75254=CARTESIAN_POINT('Ctrl Pts',(86.3584780340612,59.2146067561822,11.6444834593736));
#75255=CARTESIAN_POINT('Ctrl Pts',(86.3746660274517,59.2100924995698,11.5854557406869));
#75256=CARTESIAN_POINT('Ctrl Pts',(86.3939818959597,59.2055782429575,11.5274581847191));
#75257=CARTESIAN_POINT('Ctrl Pts',(86.4132943289906,59.2010647892408,11.469470944067));
#75258=CARTESIAN_POINT('Ctrl Pts',(86.4357333662765,59.1965513355241,11.4125140007435));
#75259=CARTESIAN_POINT('Ctrl Pts',(86.4611556745391,59.1920378818073,11.3569461216265));
#75260=CARTESIAN_POINT('Ctrl Pts',(86.4866007770444,59.1875203812213,11.3013284190351));
#75261=CARTESIAN_POINT('Ctrl Pts',(86.5150342723639,59.1830028806352,11.2471027464347));
#75262=CARTESIAN_POINT('Ctrl Pts',(86.5462656085468,59.1784853800492,11.1946057160537));
#75263=CARTESIAN_POINT('Ctrl Pts',(86.5775117273783,59.1739657412061,11.1420838373874));
#75264=CARTESIAN_POINT('Ctrl Pts',(86.6115580285535,59.169446102363,11.091292665473));
#75265=CARTESIAN_POINT('Ctrl Pts',(86.6481708840654,59.1649264635199,11.0425393821154));
#75266=CARTESIAN_POINT('Ctrl Pts',(86.6848489330696,59.1603987769287,10.9936992878067));
#75267=CARTESIAN_POINT('Ctrl Pts',(86.7241023185719,59.1558710903375,10.9469047261865));
#75268=CARTESIAN_POINT('Ctrl Pts',(86.7656582713082,59.1513434037462,10.902428423182));
#75269=CARTESIAN_POINT('Ctrl Pts',(86.7913530637336,59.1485438537547,10.8749279257008));
#75270=CARTESIAN_POINT('Ctrl Pts',(86.8179274394261,59.1457443037632,10.8483130006402));
#75271=CARTESIAN_POINT('Ctrl Pts',(86.8453106821457,59.1429447537717,10.8226403376978));
#75272=CARTESIAN_POINT('Ctrl Pts',(86.8902775124721,59.1383475301797,10.7804825008638));
#75273=CARTESIAN_POINT('Ctrl Pts',(86.9376265916061,59.1337503065876,10.7406806479449));
#75274=CARTESIAN_POINT('Ctrl Pts',(86.9870811113661,59.1291530829955,10.7035151578463));
#75275=CARTESIAN_POINT('Ctrl Pts',(87.0373824270928,59.1244771424244,10.6657132934129));
#75276=CARTESIAN_POINT('Ctrl Pts',(87.0898616419325,59.1198012018533,10.6306393569566));
#75277=CARTESIAN_POINT('Ctrl Pts',(87.1441885773489,59.1151252612821,10.5985488787828));
#75278=CARTESIAN_POINT('Ctrl Pts',(87.1974540304404,59.1105406829097,10.5670854095709));
#75279=CARTESIAN_POINT('Ctrl Pts',(87.2524951897762,59.1059561045373,10.5384901321586));
#75280=CARTESIAN_POINT('Ctrl Pts',(87.3089699298852,59.1013715261649,10.512961489127));
#75281=CARTESIAN_POINT('Ctrl Pts',(87.3654101536167,59.0967897498069,10.4874484487574));
#75282=CARTESIAN_POINT('Ctrl Pts',(87.4232817578894,59.092207973449,10.4649985356));
#75283=CARTESIAN_POINT('Ctrl Pts',(87.4822190784173,59.087626197091,10.4457637293993));
#75284=CARTESIAN_POINT('Ctrl Pts',(87.5411420249399,59.0830455381655,10.4265336143044));
#75285=CARTESIAN_POINT('Ctrl Pts',(87.6011296880393,59.0784648792401,10.4105172074319));
#75286=CARTESIAN_POINT('Ctrl Pts',(87.661799478708,59.0738842203146,10.3978172067998));
#75287=CARTESIAN_POINT('Ctrl Pts',(87.7246610629982,59.0691380777291,10.384658398249));
#75288=CARTESIAN_POINT('Ctrl Pts',(87.7882544484531,59.0643919351436,10.3750603865884));
#75289=CARTESIAN_POINT('Ctrl Pts',(87.8521430228283,59.0596457925581,10.3690794666798));
#75290=CARTESIAN_POINT('Ctrl Pts',(87.9138821021699,59.0550593312617,10.3632997714465));
#75291=CARTESIAN_POINT('Ctrl Pts',(87.9758962913229,59.0504728699653,10.3608975756909));
#75292=CARTESIAN_POINT('Ctrl Pts',(88.0377894691039,59.0458864086689,10.3618705565758));
#75293=CARTESIAN_POINT('Ctrl Pts',(88.1029149370244,59.0410604254388,10.362894350113));
#75294=CARTESIAN_POINT('Ctrl Pts',(88.1679057646038,59.0362344422087,10.3676554793341));
#75295=CARTESIAN_POINT('Ctrl Pts',(88.2323073446897,59.0314084589786,10.3760893826044));
#75296=CARTESIAN_POINT('Ctrl Pts',(88.2967089247756,59.0265824757486,10.3845232858747));
#75297=CARTESIAN_POINT('Ctrl Pts',(88.3605206351605,59.0217564925185,10.3966297663892));
#75298=CARTESIAN_POINT('Ctrl Pts',(88.4233043312516,59.0169305092884,10.4122829824812));
#75299=CARTESIAN_POINT('Ctrl Pts',(88.483111975644,59.0123332856963,10.4271942100756));
#75300=CARTESIAN_POINT('Ctrl Pts',(88.5422324368774,59.0077360621043,10.4453846980889));
#75301=CARTESIAN_POINT('Ctrl Pts',(88.6002800222825,59.0031388385122,10.466773971279));
#75302=CARTESIAN_POINT('Ctrl Pts',(88.6593215403238,58.998462897941,10.4885294870361));
#75303=CARTESIAN_POINT('Ctrl Pts',(88.7172525581037,58.9937869573699,10.5135943267067));
#75304=CARTESIAN_POINT('Ctrl Pts',(88.7736793107733,58.9891110167988,10.5418296996338));
#75305=CARTESIAN_POINT('Ctrl Pts',(88.8290035532396,58.9845264384264,10.5695133876725));
#75306=CARTESIAN_POINT('Ctrl Pts',(88.8828813079232,58.979941860054,10.6002445878048));
#75307=CARTESIAN_POINT('Ctrl Pts',(88.9349602905783,58.9753572816816,10.6338435081897));
#75308=CARTESIAN_POINT('Ctrl Pts',(88.9870074434662,58.9707755053236,10.6674218934996));
#75309=CARTESIAN_POINT('Ctrl Pts',(89.037257577369,58.9661937289657,10.7038642483169));
#75310=CARTESIAN_POINT('Ctrl Pts',(89.0853846750293,58.9616119526077,10.7429458039588));
#75311=CARTESIAN_POINT('Ctrl Pts',(89.1335000351496,58.9570312936823,10.7820178281445));
#75312=CARTESIAN_POINT('Ctrl Pts',(89.1794929919092,58.9524506347568,10.8237274546321));
#75313=CARTESIAN_POINT('Ctrl Pts',(89.2230697507249,58.9478699758314,10.8678089655744));
#75314=CARTESIAN_POINT('Ctrl Pts',(89.2682207899355,58.9431238332458,10.913482991893));
#75315=CARTESIAN_POINT('Ctrl Pts',(89.3107772563399,58.9383776906603,10.9617031916916));
#75316=CARTESIAN_POINT('Ctrl Pts',(89.3504550374916,58.9336315480748,11.0121332920438));
#75317=CARTESIAN_POINT('Ctrl Pts',(89.3887978820859,58.9290450867784,11.0608667001265));
#75318=CARTESIAN_POINT('Ctrl Pts',(89.4244524370856,58.9244586254821,11.1116631853249));
#75319=CARTESIAN_POINT('Ctrl Pts',(89.4572057983156,58.9198721641857,11.1641886979427));
#75320=CARTESIAN_POINT('Ctrl Pts',(89.4916696609342,58.9150461809556,11.2194572866571));
#75321=CARTESIAN_POINT('Ctrl Pts',(89.5229206799675,58.9102201977255,11.2766398874224));
#75322=CARTESIAN_POINT('Ctrl Pts',(89.5507665166544,58.9053942144955,11.3353195569949));
#75323=CARTESIAN_POINT('Ctrl Pts',(89.5786123533412,58.9005682312654,11.3939992265674));
#75324=CARTESIAN_POINT('Ctrl Pts',(89.6030528355372,58.8957422480353,11.4541753354705));
#75325=CARTESIAN_POINT('Ctrl Pts',(89.6239560364055,58.8909162648052,11.5154115327915));
#75326=CARTESIAN_POINT('Ctrl Pts',(89.6438683907591,58.8863190412132,11.5737450324314));
#75327=CARTESIAN_POINT('Ctrl Pts',(89.6606530417143,58.8817218176211,11.6332798817462));
#75328=CARTESIAN_POINT('Ctrl Pts',(89.6741683989992,58.877124594029,11.693648402487));
#75329=CARTESIAN_POINT('Ctrl Pts',(89.6879151759822,58.8724486534579,11.7550505965932));
#75330=CARTESIAN_POINT('Ctrl Pts',(89.6982793859158,58.8677727128868,11.8173148091167));
#75331=CARTESIAN_POINT('Ctrl Pts',(89.7051640522025,58.8630967723156,11.880034949991));
#75332=CARTESIAN_POINT('Ctrl Pts',(89.711914200473,58.8585121939432,11.9415296155013));
#75333=CARTESIAN_POINT('Ctrl Pts',(89.715319496131,58.8539276155708,12.0034620227918));
#75334=CARTESIAN_POINT('Ctrl Pts',(89.7153399075691,58.8493430371984,12.0654386915373));
#75335=CARTESIAN_POINT('Ctrl Pts',(89.7153603065322,58.8447612608404,12.1273774812223));
#75336=CARTESIAN_POINT('Ctrl Pts',(89.7119999232045,58.8401794844825,12.1893599707316));
#75337=CARTESIAN_POINT('Ctrl Pts',(89.7052707591578,58.8355977081245,12.2509903518097));
#75338=CARTESIAN_POINT('Ctrl Pts',(89.6985432362622,58.8310170491991,12.3126057020819));
#75339=CARTESIAN_POINT('Ctrl Pts',(89.6884486188747,58.8264363902736,12.3738686085835));
#75340=CARTESIAN_POINT('Ctrl Pts',(89.6750507883657,58.8218557313482,12.4343881232336));
#75341=CARTESIAN_POINT('Ctrl Pts',(89.661168939713,58.8171095887627,12.4970940025428));
#75342=CARTESIAN_POINT('Ctrl Pts',(89.6437407037342,58.8123634461771,12.5590011676541));
#75343=CARTESIAN_POINT('Ctrl Pts',(89.6228944881943,58.8076173035916,12.6196885356668));
#75344=CARTESIAN_POINT('Ctrl Pts',(89.6027496318131,58.8030308422952,12.6783341114277));
#75345=CARTESIAN_POINT('Ctrl Pts',(89.5794134157189,58.7984443809988,12.7358402086623));
#75346=CARTESIAN_POINT('Ctrl Pts',(89.5530510031723,58.7938579197024,12.7918467739235));
#75347=CARTESIAN_POINT('Ctrl Pts',(89.5253118481611,58.7890319364724,12.8507782086959));
#75348=CARTESIAN_POINT('Ctrl Pts',(89.4942220487179,58.7842059532423,12.9080486233223));
#75349=CARTESIAN_POINT('Ctrl Pts',(89.4600275633828,58.7793799700122,12.9632702804379));
#75350=CARTESIAN_POINT('Ctrl Pts',(89.4258330780476,58.7745539867822,13.0184919375534));
#75351=CARTESIAN_POINT('Ctrl Pts',(89.3885343422863,58.7697280035521,13.0716643511086));
#75352=CARTESIAN_POINT('Ctrl Pts',(89.3484263867851,58.764902020322,13.1224400103796));
#75353=CARTESIAN_POINT('Ctrl Pts',(89.3102196151348,58.76030479673,13.1708088188845));
#75354=CARTESIAN_POINT('Ctrl Pts',(89.2693071017345,58.7557075731379,13.2172015881259));
#75355=CARTESIAN_POINT('Ctrl Pts',(89.2259209424767,58.7511103495458,13.261299936891));
#75356=CARTESIAN_POINT('Ctrl Pts',(89.1817918940987,58.7464344089747,13.3061533693988));
#75357=CARTESIAN_POINT('Ctrl Pts',(89.1351039456151,58.7417584684036,13.3486325934397));
#75358=CARTESIAN_POINT('Ctrl Pts',(89.0861456619014,58.7370825278324,13.3884358741711));
#75359=CARTESIAN_POINT('Ctrl Pts',(89.0381439635799,58.73249794946,13.4274614471476));
#75360=CARTESIAN_POINT('Ctrl Pts',(88.9879602652018,58.7279133710876,13.4639143692309));
#75361=CARTESIAN_POINT('Ctrl Pts',(88.9359034248243,58.7233287927152,13.4975475857785));
#75362=CARTESIAN_POINT('Ctrl Pts',(88.883878400681,58.7187470163572,13.5311602462899));
#75363=CARTESIAN_POINT('Ctrl Pts',(88.8299829312574,58.7141652399993,13.5619563427552));
#75364=CARTESIAN_POINT('Ctrl Pts',(88.7745560530864,58.7095834636413,13.5897312720408));
#75365=CARTESIAN_POINT('Ctrl Pts',(88.719142692772,58.7050028047159,13.6174994274015));
#75366=CARTESIAN_POINT('Ctrl Pts',(88.6621991200432,58.7004221457904,13.64224765033));
#75367=CARTESIAN_POINT('Ctrl Pts',(88.6040884278359,58.695841486865,13.6638175591622));
#75368=CARTESIAN_POINT('Ctrl Pts',(88.5438783935489,58.6910953442794,13.6861667155915));
#75369=CARTESIAN_POINT('Ctrl Pts',(88.48241581987,58.6863492016939,13.7051032553549));
#75370=CARTESIAN_POINT('Ctrl Pts',(88.4201241156717,58.6816030591084,13.7205066616898));
#75371=CARTESIAN_POINT('Ctrl Pts',(88.3599281807109,58.677016597812,13.7353918291104));
#75372=CARTESIAN_POINT('Ctrl Pts',(88.298958556223,58.6724301365156,13.746977815929));
#75373=CARTESIAN_POINT('Ctrl Pts',(88.23760731508,58.6678436752192,13.7552080867532));
#75374=CARTESIAN_POINT('Ctrl Pts',(88.1730520857285,58.6630176919892,13.7638681726907));
#75375=CARTESIAN_POINT('Ctrl Pts',(88.1080749291716,58.6581917087591,13.7688123760322));
#75376=CARTESIAN_POINT('Ctrl Pts',(88.0431349993862,58.653365725529,13.770037023487));
#75377=CARTESIAN_POINT('Ctrl Pts',(87.9781950696008,58.648539742299,13.7712616709419));
#75378=CARTESIAN_POINT('Ctrl Pts',(87.9132930111233,58.6437137590689,13.7687668647215));
#75379=CARTESIAN_POINT('Ctrl Pts',(87.8488807993496,58.6388877758388,13.7626119769648));
#75380=CARTESIAN_POINT('Ctrl Pts',(87.7875218336287,58.6342905522468,13.7567488411327));
#75381=CARTESIAN_POINT('Ctrl Pts',(87.7263553893494,58.6296933286547,13.7475407531209));
#75382=CARTESIAN_POINT('Ctrl Pts',(87.6657748338337,58.6250961050626,13.7350100120267));
#75383=CARTESIAN_POINT('Ctrl Pts',(87.6041569743401,58.6204201644915,13.7222647105431));
#75384=CARTESIAN_POINT('Ctrl Pts',(87.5431457933917,58.6157442239204,13.7060818551707));
#75385=CARTESIAN_POINT('Ctrl Pts',(87.4831513020492,58.6110682833492,13.6865402147653));
#75386=CARTESIAN_POINT('Ctrl Pts',(87.42432903019,58.6064837049768,13.6673803942755));
#75387=CARTESIAN_POINT('Ctrl Pts',(87.3664845826797,58.6018991266044,13.6449920266809));
#75388=CARTESIAN_POINT('Ctrl Pts',(87.3099930395823,58.597314548232,13.6195005880417));
#75389=CARTESIAN_POINT('Ctrl Pts',(87.2535360231321,58.592732771874,13.5940247293258));
#75390=CARTESIAN_POINT('Ctrl Pts',(87.1984307345598,58.5881509955161,13.5654497690762));
#75391=CARTESIAN_POINT('Ctrl Pts',(87.1450329582858,58.5835692191581,13.5339495625752));
#75392=CARTESIAN_POINT('Ctrl Pts',(87.0916482049982,58.5789885602326,13.5024570385433));
#75393=CARTESIAN_POINT('Ctrl Pts',(87.0399705755609,58.5744079013072,13.4680409430503));
#75394=CARTESIAN_POINT('Ctrl Pts',(86.9903300709222,58.5698272423817,13.43092041214));
#75395=CARTESIAN_POINT('Ctrl Pts',(86.9388962233326,58.5650810997962,13.3924588424363));
#75396=CARTESIAN_POINT('Ctrl Pts',(86.8896500114354,58.5603349572107,13.3510939888136));
#75397=CARTESIAN_POINT('Ctrl Pts',(86.8429223403631,58.5555888146252,13.3071161978869));
#75398=CARTESIAN_POINT('Ctrl Pts',(86.7977667954163,58.5510023533288,13.2646180149199));
#75399=CARTESIAN_POINT('Ctrl Pts',(86.7549633136975,58.5464158920324,13.2196803675238));
#75400=CARTESIAN_POINT('Ctrl Pts',(86.7147720516274,58.541829430736,13.1726019796918));
#75401=CARTESIAN_POINT('Ctrl Pts',(86.67248185354,58.5370034475059,13.1230649847206));
#75402=CARTESIAN_POINT('Ctrl Pts',(86.6330845942958,58.5321774642759,13.0711580296476));
#75403=CARTESIAN_POINT('Ctrl Pts',(86.5968324044532,58.5273514810458,13.0172648670615));
#75404=CARTESIAN_POINT('Ctrl Pts',(86.5605802146106,58.5225254978157,12.9633717044754));
#75405=CARTESIAN_POINT('Ctrl Pts',(86.5274733578954,58.5176995145857,12.9074929313042));
#75406=CARTESIAN_POINT('Ctrl Pts',(86.4977071054124,58.5128735313556,12.8500404650213));
#75407=CARTESIAN_POINT('Ctrl Pts',(86.4666678734959,58.5078411607947,12.7901309945178));
#75408=CARTESIAN_POINT('Ctrl Pts',(86.4391419040733,58.5028087902338,12.7282820959685));
#75409=CARTESIAN_POINT('Ctrl Pts',(86.4153585462241,58.497776419673,12.6649183471827));
#75410=CARTESIAN_POINT('Ctrl Pts',(86.3923709072428,58.492912416936,12.6036745568471));
#75411=CARTESIAN_POINT('Ctrl Pts',(86.3728796178103,58.4880484141989,12.5410160954335));
#75412=CARTESIAN_POINT('Ctrl Pts',(86.3570458087894,58.4831844114619,12.4773518797536));
#75413=CARTESIAN_POINT('Ctrl Pts',(86.3412447005935,58.4783304541222,12.4138191468002));
#75414=CARTESIAN_POINT('Ctrl Pts',(86.3290861550402,58.4734764967825,12.3492851894886));
#75415=CARTESIAN_POINT('Ctrl Pts',(86.3206822455971,58.4686225394428,12.2841759032306));
#75416=CARTESIAN_POINT('Ctrl Pts',(86.3122999148258,58.4637810455825,12.2192337977265));
#75417=CARTESIAN_POINT('Ctrl Pts',(86.3076530849219,58.4589395517222,12.153719713652));
#75418=CARTESIAN_POINT('Ctrl Pts',(86.3068028996812,58.4540980578619,12.0880698632754));
#75419=CARTESIAN_POINT('Ctrl Pts',(86.3067084848801,58.4535604001163,12.0807793137938));
#75420=CARTESIAN_POINT('Ctrl Pts',(86.3066608404519,58.4530227423707,12.0734871001454));
#75421=CARTESIAN_POINT('Ctrl Pts',(86.3066600110215,58.4524850846251,12.0661938267317));
#75422=CARTESIAN_POINT('',(86.3066607017018,57.6587350846356,12.0644534307351));
#75423=CARTESIAN_POINT('Ctrl Pts',(86.3066600110214,58.4524850845702,12.0661938259872));
#75424=CARTESIAN_POINT('Ctrl Pts',(86.3066526701297,58.4477265146277,12.0016443018099));
#75425=CARTESIAN_POINT('Ctrl Pts',(86.3103167313048,58.4429679446852,11.9371518094558));
#75426=CARTESIAN_POINT('Ctrl Pts',(86.3176069473779,58.4382093747427,11.8731404528388));
#75427=CARTESIAN_POINT('Ctrl Pts',(86.3249149448926,58.4334391982535,11.8089729672149));
#75428=CARTESIAN_POINT('Ctrl Pts',(86.335866710533,58.4286690217644,11.7452894092002));
#75429=CARTESIAN_POINT('Ctrl Pts',(86.3503654536597,58.4238988452752,11.6825058812692));
#75430=CARTESIAN_POINT('Ctrl Pts',(86.3648829022572,58.41912251457,11.6196413535275));
#75431=CARTESIAN_POINT('Ctrl Pts',(86.3829563199365,58.4143461838648,11.5576796008999));
#75432=CARTESIAN_POINT('Ctrl Pts',(86.4044392596024,58.4095698531597,11.4970207182917));
#75433=CARTESIAN_POINT('Ctrl Pts',(86.4259782863255,58.4047810525441,11.4362034691719));
#75434=CARTESIAN_POINT('Ctrl Pts',(86.4509444481393,58.3999922519284,11.3766963024248));
#75435=CARTESIAN_POINT('Ctrl Pts',(86.4791434823621,58.3952034513128,11.3188785607612));
#75436=CARTESIAN_POINT('Ctrl Pts',(86.4955217920549,58.392422063166,11.2852973795325));
#75437=CARTESIAN_POINT('Ctrl Pts',(86.5129898292057,58.3896406750192,11.2522856335913));
#75438=CARTESIAN_POINT('Ctrl Pts',(86.5315028123033,58.3868592868723,11.21991317987));
#75439=CARTESIAN_POINT('Ctrl Pts',(86.5621020376408,58.3822620632802,11.1664062976502));
#75440=CARTESIAN_POINT('Ctrl Pts',(86.5956704799675,58.3776648396882,11.114451678314));
#75441=CARTESIAN_POINT('Ctrl Pts',(86.6320259039401,58.3730676160961,11.0643986431739));
#75442=CARTESIAN_POINT('Ctrl Pts',(86.6690038317109,58.368391675525,11.0134885638551));
#75443=CARTESIAN_POINT('Ctrl Pts',(86.7088649000607,58.3637157349538,10.964546309731));
#75444=CARTESIAN_POINT('Ctrl Pts',(86.7513685586074,58.3590397943827,10.9179131272177));
#75445=CARTESIAN_POINT('Ctrl Pts',(86.7930417472969,58.3544552160103,10.8721911004435));
#75446=CARTESIAN_POINT('Ctrl Pts',(86.8372548295851,58.3498706376379,10.8286891181222));
#75447=CARTESIAN_POINT('Ctrl Pts',(86.8837390657971,58.3452860592655,10.7876973668884));
#75448=CARTESIAN_POINT('Ctrl Pts',(86.9301948916535,58.3407042829075,10.746730669099));
#75449=CARTESIAN_POINT('Ctrl Pts',(86.9789187380448,58.3361225065496,10.7082714962698));
#75450=CARTESIAN_POINT('Ctrl Pts',(87.0296057165671,58.3315407301916,10.6725725364967));
#75451=CARTESIAN_POINT('Ctrl Pts',(87.0802803332294,58.3269600712662,10.6368822832111));
#75452=CARTESIAN_POINT('Ctrl Pts',(87.1329167155715,58.3223794123407,10.6039511996096));
#75453=CARTESIAN_POINT('Ctrl Pts',(87.1871793207144,58.3177987534153,10.5739898378424));
#75454=CARTESIAN_POINT('Ctrl Pts',(87.243402249612,58.3130526108298,10.5429460737646));
#75455=CARTESIAN_POINT('Ctrl Pts',(87.3013706727908,58.3083064682442,10.5150910488029));
#75456=CARTESIAN_POINT('Ctrl Pts',(87.3606837766397,58.3035603256587,10.4906068283649));
#75457=CARTESIAN_POINT('Ctrl Pts',(87.4180013245791,58.2989738643623,10.4669463657075));
#75458=CARTESIAN_POINT('Ctrl Pts',(87.4765739800833,58.2943874030659,10.4464335836454));
#75459=CARTESIAN_POINT('Ctrl Pts',(87.5360224153988,58.2898009417696,10.4291826217545));
#75460=CARTESIAN_POINT('Ctrl Pts',(87.5985754673809,58.2849749585395,10.4110307509748));
#75461=CARTESIAN_POINT('Ctrl Pts',(87.6620976550911,58.2801489753094,10.396490885452));
#75462=CARTESIAN_POINT('Ctrl Pts',(87.7261354625014,58.2753229920793,10.3856348519218));
#75463=CARTESIAN_POINT('Ctrl Pts',(87.7901732699117,58.2704970088493,10.3747788183917));
#75464=CARTESIAN_POINT('Ctrl Pts',(87.8547260444536,58.2656710256192,10.367606611504));
#75465=CARTESIAN_POINT('Ctrl Pts',(87.9193380054694,58.2608450423891,10.3641266456171));
#75466=CARTESIAN_POINT('Ctrl Pts',(87.980887251986,58.2562478187971,10.3608116359055));
#75467=CARTESIAN_POINT('Ctrl Pts',(88.0427429092134,58.251650595205,10.3608330737158));
#75468=CARTESIAN_POINT('Ctrl Pts',(88.1045126606968,58.2470533716129,10.3642273307256));
#75469=CARTESIAN_POINT('Ctrl Pts',(88.1673400784293,58.2423774310418,10.3676797066527));
#75470=CARTESIAN_POINT('Ctrl Pts',(88.2300780964387,58.2377014904707,10.3746216159706));
#75471=CARTESIAN_POINT('Ctrl Pts',(88.2923095521568,58.2330255498995,10.3850360588444));
#75472=CARTESIAN_POINT('Ctrl Pts',(88.3533250808252,58.2284409715271,10.3952470161553));
#75473=CARTESIAN_POINT('Ctrl Pts',(88.4138531382947,58.2238563931547,10.4087959412156));
#75474=CARTESIAN_POINT('Ctrl Pts',(88.4735041685626,58.2192718147823,10.4256144570064));
#75475=CARTESIAN_POINT('Ctrl Pts',(88.5331187411596,58.2146900384243,10.4424226936134));
#75476=CARTESIAN_POINT('Ctrl Pts',(88.5918568604838,58.2101082620664,10.4624964207244));
#75477=CARTESIAN_POINT('Ctrl Pts',(88.6493408668227,58.2055264857084,10.4857165528476));
#75478=CARTESIAN_POINT('Ctrl Pts',(88.7068108535999,58.200945826783,10.5089310218985));
#75479=CARTESIAN_POINT('Ctrl Pts',(88.7630268627893,58.1963651678575,10.5352901820531));
#75480=CARTESIAN_POINT('Ctrl Pts',(88.8176300070296,58.1917845089321,10.5646263398609));
#75481=CARTESIAN_POINT('Ctrl Pts',(88.8742057775462,58.1870383663465,10.5950223134824));
#75482=CARTESIAN_POINT('Ctrl Pts',(88.9290493747618,58.182292223761,10.6286142819556));
#75483=CARTESIAN_POINT('Ctrl Pts',(88.9817904408662,58.1775460811755,10.665164265332));
#75484=CARTESIAN_POINT('Ctrl Pts',(89.0327570635624,58.1729596198791,10.7004845451423));
#75485=CARTESIAN_POINT('Ctrl Pts',(89.081760021942,58.1683731585827,10.738566565451));
#75486=CARTESIAN_POINT('Ctrl Pts',(89.1284976780263,58.1637866972863,10.7791535541465));
#75487=CARTESIAN_POINT('Ctrl Pts',(89.1776761469809,58.1589607140563,10.8218601451642));
#75488=CARTESIAN_POINT('Ctrl Pts',(89.2243457518699,58.1541347308262,10.867340074808));
#75489=CARTESIAN_POINT('Ctrl Pts',(89.2682001629992,58.1493087475961,10.9152512933943));
#75490=CARTESIAN_POINT('Ctrl Pts',(89.3120545741286,58.1444827643661,10.9631625119805));
#75491=CARTESIAN_POINT('Ctrl Pts',(89.3530934420407,58.139656781136,11.0135044683705));
#75492=CARTESIAN_POINT('Ctrl Pts',(89.3910624827904,58.1348307979059,11.0658988155219));
#75493=CARTESIAN_POINT('Ctrl Pts',(89.4272317278088,58.1302335743138,11.1158095834077));
#75494=CARTESIAN_POINT('Ctrl Pts',(89.4607641494191,58.1256363507218,11.1677874584275));
#75495=CARTESIAN_POINT('Ctrl Pts',(89.4914163990448,58.1210391271297,11.2215225751749));
#75496=CARTESIAN_POINT('Ctrl Pts',(89.5225934986028,58.1163631865586,11.2761777833587));
#75497=CARTESIAN_POINT('Ctrl Pts',(89.5507904769835,58.1116872459874,11.3326506035374));
#75498=CARTESIAN_POINT('Ctrl Pts',(89.5757953476468,58.1070113054163,11.3905813479162));
#75499=CARTESIAN_POINT('Ctrl Pts',(89.6003116535118,58.1024267270439,11.4473801959205));
#75500=CARTESIAN_POINT('Ctrl Pts',(89.6217592582274,58.0978421486715,11.5055800186288));
#75501=CARTESIAN_POINT('Ctrl Pts',(89.6399843120806,58.0932575702991,11.5648164541856));
#75502=CARTESIAN_POINT('Ctrl Pts',(89.6581982270984,58.0886757939411,11.6240166854645));
#75503=CARTESIAN_POINT('Ctrl Pts',(89.673193347239,58.0840940175832,11.6842517878039));
#75504=CARTESIAN_POINT('Ctrl Pts',(89.6848648765849,58.0795122412252,11.7451398894603));
#75505=CARTESIAN_POINT('Ctrl Pts',(89.6965335594045,58.0749315822998,11.8060131413426));
#75506=CARTESIAN_POINT('Ctrl Pts',(89.7048801647596,58.0703509233743,11.8675385766705));
#75507=CARTESIAN_POINT('Ctrl Pts',(89.7098509154069,58.0657702644489,11.9293237298535));
#75508=CARTESIAN_POINT('Ctrl Pts',(89.7150012424042,58.0610241218634,11.9933409709199));
#75509=CARTESIAN_POINT('Ctrl Pts',(89.7165270178085,58.0562779792778,12.0576364801789));
#75510=CARTESIAN_POINT('Ctrl Pts',(89.7144272919947,58.0515318366923,12.1217700321634));
#75511=CARTESIAN_POINT('Ctrl Pts',(89.7123982102711,58.0469453753959,12.1837458469809));
#75512=CARTESIAN_POINT('Ctrl Pts',(89.7069838427897,58.0423589140995,12.2455699104637));
#75513=CARTESIAN_POINT('Ctrl Pts',(89.6982363011712,58.0377724528032,12.3068495372842));
#75514=CARTESIAN_POINT('Ctrl Pts',(89.6890319306496,58.0329464695731,12.371329412349));
#75515=CARTESIAN_POINT('Ctrl Pts',(89.6761368148682,58.028120486343,12.4352057930377));
#75516=CARTESIAN_POINT('Ctrl Pts',(89.6596721641605,58.0232945031129,12.4980357979638));
#75517=CARTESIAN_POINT('Ctrl Pts',(89.6432075134529,58.0184685198829,12.5608658028898));
#75518=CARTESIAN_POINT('Ctrl Pts',(89.6231736012971,58.0136425366528,12.6226488395295));
#75519=CARTESIAN_POINT('Ctrl Pts',(89.5997503617558,58.0088165534227,12.6829660635892));
#75520=CARTESIAN_POINT('Ctrl Pts',(89.5774374227569,58.0042193298306,12.7404241508301));
#75521=CARTESIAN_POINT('Ctrl Pts',(89.5519576535371,57.9996221062385,12.7967881832545));
#75522=CARTESIAN_POINT('Ctrl Pts',(89.5234393866178,57.9950248826465,12.8516856479581));
#75523=CARTESIAN_POINT('Ctrl Pts',(89.4944328093575,57.9903489420753,12.9075231066585));
#75524=CARTESIAN_POINT('Ctrl Pts',(89.4622828037395,57.9856730015042,12.9618427729636));
#75525=CARTESIAN_POINT('Ctrl Pts',(89.427176569858,57.9809970609331,13.0142714582782));
#75526=CARTESIAN_POINT('Ctrl Pts',(89.3927562691416,57.9764124825607,13.0656757507691));
#75527=CARTESIAN_POINT('Ctrl Pts',(89.3554945202088,57.9718279041882,13.1152618494036));
#75528=CARTESIAN_POINT('Ctrl Pts',(89.3156139832743,57.9672433258158,13.1627028723611));
#75529=CARTESIAN_POINT('Ctrl Pts',(89.2757578206295,57.9626615494579,13.2101149001916));
#75530=CARTESIAN_POINT('Ctrl Pts',(89.2332863705377,57.9580797730999,13.2553840630841));
#75531=CARTESIAN_POINT('Ctrl Pts',(89.1884636103591,57.9534979967419,13.2982151930081));
#75532=CARTESIAN_POINT('Ctrl Pts',(89.1436517818379,57.9489173378165,13.3410358770061));
#75533=CARTESIAN_POINT('Ctrl Pts',(89.0964901494892,57.944336678891,13.3814193568888));
#75534=CARTESIAN_POINT('Ctrl Pts',(89.0472792632542,57.9397560199656,13.4191075804049));
#75535=CARTESIAN_POINT('Ctrl Pts',(88.996290554723,57.9350098773801,13.4581573515216));
#75536=CARTESIAN_POINT('Ctrl Pts',(88.9431021148915,57.9302637347945,13.4943129924332));
#75537=CARTESIAN_POINT('Ctrl Pts',(88.8880832714187,57.925517592209,13.527334927591));
#75538=CARTESIAN_POINT('Ctrl Pts',(88.8349155058883,57.9209311309126,13.5592458583742));
#75539=CARTESIAN_POINT('Ctrl Pts',(88.7800390550594,57.9163446696162,13.5882304291864));
#75540=CARTESIAN_POINT('Ctrl Pts',(88.7238120874676,57.9117582083198,13.6141194280675));
#75541=CARTESIAN_POINT('Ctrl Pts',(88.6646487401417,57.9069322250898,13.6413604460047));
#75542=CARTESIAN_POINT('Ctrl Pts',(88.603990545554,57.9021062418597,13.6651734561096));
#75543=CARTESIAN_POINT('Ctrl Pts',(88.5422753220686,57.8972802586296,13.6854200714333));
#75544=CARTESIAN_POINT('Ctrl Pts',(88.4805600985832,57.8924542753996,13.7056666867569));
#75545=CARTESIAN_POINT('Ctrl Pts',(88.4177884923259,57.8876282921695,13.72234681567));
#75546=CARTESIAN_POINT('Ctrl Pts',(88.3544099792681,57.8828023089394,13.735384443961));
#75547=CARTESIAN_POINT('Ctrl Pts',(88.2940357132232,57.8782050853474,13.7478040669699));
#75548=CARTESIAN_POINT('Ctrl Pts',(88.2328629009972,57.8736078617553,13.7569697548862));
#75549=CARTESIAN_POINT('Ctrl Pts',(88.1712741059682,57.8690106381632,13.7627872720398));
#75550=CARTESIAN_POINT('Ctrl Pts',(88.1086307431569,57.8643346975921,13.7687044009191));
#75551=CARTESIAN_POINT('Ctrl Pts',(88.0455575182171,57.8596587570209,13.7711574203679));
#75552=CARTESIAN_POINT('Ctrl Pts',(87.9824694918876,57.8549828164498,13.7701011841164));
#75553=CARTESIAN_POINT('Ctrl Pts',(87.920614128957,57.8503982380774,13.7690655854381));
#75554=CARTESIAN_POINT('Ctrl Pts',(87.8587450711802,57.845813659705,13.7646566398585));
#75555=CARTESIAN_POINT('Ctrl Pts',(87.7972577095201,57.8412290813326,13.7568841086427));
#75556=CARTESIAN_POINT('Ctrl Pts',(87.7358079278645,57.8366473049746,13.7491163278626));
#75557=CARTESIAN_POINT('Ctrl Pts',(87.6747398837335,57.8320655286167,13.7379891014385));
#75558=CARTESIAN_POINT('Ctrl Pts',(87.614444735032,57.8274837522587,13.7235641035647));
#75559=CARTESIAN_POINT('Ctrl Pts',(87.5541642914916,57.8229030933333,13.7091426237503));
#75560=CARTESIAN_POINT('Ctrl Pts',(87.4946568640368,57.8183224344078,13.6914250874954));
#75561=CARTESIAN_POINT('Ctrl Pts',(87.4363022657435,57.8137417754824,13.6705240259468));
#75562=CARTESIAN_POINT('Ctrl Pts',(87.3758395138713,57.8089956328969,13.6488678799833));
#75563=CARTESIAN_POINT('Ctrl Pts',(87.3166150505194,57.8042494903113,13.6237939205407));
#75564=CARTESIAN_POINT('Ctrl Pts',(87.2590304710439,57.7995033477258,13.5954824821231));
#75565=CARTESIAN_POINT('Ctrl Pts',(87.2033832922507,57.7949168864294,13.5681235660754));
#75566=CARTESIAN_POINT('Ctrl Pts',(87.1492678216305,57.790330425133,13.5377418933054));
#75567=CARTESIAN_POINT('Ctrl Pts',(87.097020487904,57.7857439638366,13.5045465884249));
#75568=CARTESIAN_POINT('Ctrl Pts',(87.0420446056094,57.7809179806066,13.4696177022275));
#75569=CARTESIAN_POINT('Ctrl Pts',(86.989137861963,57.7760919973765,13.4315736159901));
#75570=CARTESIAN_POINT('Ctrl Pts',(86.9386539909095,57.7712660141464,13.3907070892796));
#75571=CARTESIAN_POINT('Ctrl Pts',(86.888170119856,57.7664400309164,13.3498405625691));
#75572=CARTESIAN_POINT('Ctrl Pts',(86.8401095488331,57.7616140476863,13.3061520885097));
#75573=CARTESIAN_POINT('Ctrl Pts',(86.7947799342,57.7567880644562,13.2599780513667));
#75574=CARTESIAN_POINT('Ctrl Pts',(86.7521948455824,57.7522542751182,13.216599666629));
#75575=CARTESIAN_POINT('Ctrl Pts',(86.7118345839947,57.7477204857802,13.1708391521557));
#75576=CARTESIAN_POINT('Ctrl Pts',(86.6739822128349,57.7431866964423,13.1229570816283));
#75577=CARTESIAN_POINT('Ctrl Pts',(86.6361827559377,57.7386592449402,13.0751419459949));
#75578=CARTESIAN_POINT('Ctrl Pts',(86.6008845694283,57.7341317934382,13.0252115336295));
#75579=CARTESIAN_POINT('Ctrl Pts',(86.5683338286842,57.7296043419362,12.9734630316111));
#75580=CARTESIAN_POINT('Ctrl Pts',(86.5358158593164,57.7250814485736,12.921766628857));
#75581=CARTESIAN_POINT('Ctrl Pts',(86.5060401334303,57.7205585552111,12.8682562039503));
#75582=CARTESIAN_POINT('Ctrl Pts',(86.4792110692454,57.7160356618486,12.8132599997442));
#75583=CARTESIAN_POINT('Ctrl Pts',(86.4523985287984,57.7115155540884,12.7582976671208));
#75584=CARTESIAN_POINT('Ctrl Pts',(86.4285292807412,57.7069954463283,12.7018518396974));
#75585=CARTESIAN_POINT('Ctrl Pts',(86.4077619763422,57.7024753385681,12.6442756047923));
#75586=CARTESIAN_POINT('Ctrl Pts',(86.3869919659206,57.6979546418286,12.5866918675851));
#75587=CARTESIAN_POINT('Ctrl Pts',(86.3693248955293,57.6934339450891,12.5279779177786));
#75588=CARTESIAN_POINT('Ctrl Pts',(86.3548706951831,57.6889132483495,12.4685053556498));
#75589=CARTESIAN_POINT('Ctrl Pts',(86.3404150396387,57.6843920964821,12.4090268060319));
#75590=CARTESIAN_POINT('Ctrl Pts',(86.3291730065193,57.6798709446147,12.3487900050384));
#75591=CARTESIAN_POINT('Ctrl Pts',(86.3212035647576,57.6753497927472,12.2881775034565));
#75592=CARTESIAN_POINT('Ctrl Pts',(86.3132266214071,57.670824385146,12.2275079476818));
#75593=CARTESIAN_POINT('Ctrl Pts',(86.3085284608619,57.6662989775448,12.1664625077594));
#75594=CARTESIAN_POINT('Ctrl Pts',(86.307116119423,57.6617735699435,12.1054278722451));
#75595=CARTESIAN_POINT('Ctrl Pts',(86.3068000242341,57.6607607415076,12.0917677514613));
#75596=CARTESIAN_POINT('Ctrl Pts',(86.3066483109801,57.6597479130716,12.0781081660735));
#75597=CARTESIAN_POINT('Ctrl Pts',(86.3066607017018,57.6587350846356,12.0644534307351));
#75598=CARTESIAN_POINT('',(86.3066601734134,56.8649850845176,12.0667688372946));
#75599=CARTESIAN_POINT('Ctrl Pts',(86.3066607017026,57.6587350845702,12.0644534298534));
#75600=CARTESIAN_POINT('Ctrl Pts',(86.3067373367494,57.6524708723721,11.980000667048));
#75601=CARTESIAN_POINT('Ctrl Pts',(86.3130947576162,57.6462066601741,11.8958234833704));
#75602=CARTESIAN_POINT('Ctrl Pts',(86.3255895191783,57.639942447976,11.8126892289375));
#75603=CARTESIAN_POINT('Ctrl Pts',(86.3316855142865,57.6368862386417,11.772129350637));
#75604=CARTESIAN_POINT('Ctrl Pts',(86.3392416907942,57.6338300293073,11.7318172679732));
#75605=CARTESIAN_POINT('Ctrl Pts',(86.3482375021317,57.630773819973,11.6918399924058));
#75606=CARTESIAN_POINT('Ctrl Pts',(86.3617692179229,57.6261765963809,11.6317052129194));
#75607=CARTESIAN_POINT('Ctrl Pts',(86.3785951317794,57.6215793727888,11.5721820122873));
#75608=CARTESIAN_POINT('Ctrl Pts',(86.3986436606239,57.6169821491968,11.5136578320698));
#75609=CARTESIAN_POINT('Ctrl Pts',(86.4190354748435,57.6123062086256,11.4541315586159));
#75610=CARTESIAN_POINT('Ctrl Pts',(86.4427612789035,57.6076302680545,11.3956393776817));
#75611=CARTESIAN_POINT('Ctrl Pts',(86.4696913753969,57.6029543274834,11.3385781421183));
#75612=CARTESIAN_POINT('Ctrl Pts',(86.4960952905178,57.598369749111,11.2826318137832));
#75613=CARTESIAN_POINT('Ctrl Pts',(86.5255791805818,57.5937851707386,11.2280614982444));
#75614=CARTESIAN_POINT('Ctrl Pts',(86.5579714037962,57.5892005923661,11.1752235217441));
#75615=CARTESIAN_POINT('Ctrl Pts',(86.5903438294479,57.5846188160082,11.1224178388948));
#75616=CARTESIAN_POINT('Ctrl Pts',(86.6256207981772,57.5800370396502,11.0713428287709));
#75617=CARTESIAN_POINT('Ctrl Pts',(86.6635850991102,57.5754552632923,11.0223295920358));
#75618=CARTESIAN_POINT('Ctrl Pts',(86.7015401410702,57.5708746043668,10.9733283089578));
#75619=CARTESIAN_POINT('Ctrl Pts',(86.7421809025778,57.5662939454414,10.9263882033198));
#75620=CARTESIAN_POINT('Ctrl Pts',(86.7852484933105,57.5617132865159,10.8818091034599));
#75621=CARTESIAN_POINT('Ctrl Pts',(86.8298719699235,57.5569671439304,10.835619512025));
#75622=CARTESIAN_POINT('Ctrl Pts',(86.8771006212783,57.5522210013449,10.7919652454218));
#75623=CARTESIAN_POINT('Ctrl Pts',(86.926604797949,57.5474748587594,10.7511380751696));
#75624=CARTESIAN_POINT('Ctrl Pts',(86.97444343453,57.542888397463,10.7116845120224));
#75625=CARTESIAN_POINT('Ctrl Pts',(87.0244064327555,57.5383019361666,10.6748710768518));
#75626=CARTESIAN_POINT('Ctrl Pts',(87.0761647280618,57.5337154748702,10.6409183006086));
#75627=CARTESIAN_POINT('Ctrl Pts',(87.1306260325454,57.5288894916401,10.6051923850988));
#75628=CARTESIAN_POINT('Ctrl Pts',(87.1870747377085,57.52406350841,10.5726344412704));
#75629=CARTESIAN_POINT('Ctrl Pts',(87.2450984343659,57.51923752518,10.5434463466402));
#75630=CARTESIAN_POINT('Ctrl Pts',(87.3031221310233,57.5144115419499,10.51425825201));
#75631=CARTESIAN_POINT('Ctrl Pts',(87.3627201938244,57.5095855587198,10.4884401931547));
#75632=CARTESIAN_POINT('Ctrl Pts',(87.4234594215836,57.5047595754897,10.4661340980213));
#75633=CARTESIAN_POINT('Ctrl Pts',(87.481319508846,57.5001623518977,10.4448853489259));
#75634=CARTESIAN_POINT('Ctrl Pts',(87.5404525647213,57.4955651283056,10.4267358449806));
#75635=CARTESIAN_POINT('Ctrl Pts',(87.6004942647793,57.4909679047135,10.4118355955496));
#75636=CARTESIAN_POINT('Ctrl Pts',(87.6615640421432,57.4862919641424,10.3966802132979));
#75637=CARTESIAN_POINT('Ctrl Pts',(87.7235734084541,57.4816160235713,10.3848866769984));
#75638=CARTESIAN_POINT('Ctrl Pts',(87.786118611517,57.4769400830001,10.376561277609));
#75639=CARTESIAN_POINT('Ctrl Pts',(87.8474417572882,57.4723555046277,10.3683985464106));
#75640=CARTESIAN_POINT('Ctrl Pts',(87.9092794601771,57.4677709262553,10.3635697150064));
#75641=CARTESIAN_POINT('Ctrl Pts',(87.9712392646679,57.4631863478829,10.3621238544055));
#75642=CARTESIAN_POINT('Ctrl Pts',(88.0331612004054,57.458604571525,10.3606788774895));
#75643=CARTESIAN_POINT('Ctrl Pts',(88.0952045819187,57.454022795167,10.3626127834504));
#75644=CARTESIAN_POINT('Ctrl Pts',(88.1569734296218,57.449441018809,10.3679226774247));
#75645=CARTESIAN_POINT('Ctrl Pts',(88.2187272127489,57.4448603598836,10.3732312763886));
#75646=CARTESIAN_POINT('Ctrl Pts',(88.2802060880323,57.4402797009581,10.3819141852975));
#75647=CARTESIAN_POINT('Ctrl Pts',(88.3410177415467,57.4356990420327,10.3939165314302));
#75648=CARTESIAN_POINT('Ctrl Pts',(88.4040263137057,57.4309528994472,10.4063524815923));
#75649=CARTESIAN_POINT('Ctrl Pts',(88.4663179493559,57.4262067568617,10.4223522512616));
#75650=CARTESIAN_POINT('Ctrl Pts',(88.5274687236262,57.4214606142762,10.4417971514876));
#75651=CARTESIAN_POINT('Ctrl Pts',(88.5865621146025,57.4168741529798,10.4605878390179));
#75652=CARTESIAN_POINT('Ctrl Pts',(88.6445897293,57.4122876916834,10.4825952498893));
#75653=CARTESIAN_POINT('Ctrl Pts',(88.7011878107857,57.407701230387,10.50766254571));
#75654=CARTESIAN_POINT('Ctrl Pts',(88.7607416529426,57.4028752471569,10.534038948221));
#75655=CARTESIAN_POINT('Ctrl Pts',(88.8187119786913,57.3980492639268,10.5638033120392));
#75656=CARTESIAN_POINT('Ctrl Pts',(88.8747054962242,57.3932232806968,10.5967186615927));
#75657=CARTESIAN_POINT('Ctrl Pts',(88.9306990137571,57.3883972974667,10.6296340111461));
#75658=CARTESIAN_POINT('Ctrl Pts',(88.9847152271377,57.3835713142366,10.6656999222634));
#75659=CARTESIAN_POINT('Ctrl Pts',(89.0363999319057,57.3787453310065,10.7046294350003));
#75660=CARTESIAN_POINT('Ctrl Pts',(89.0856346956381,57.3741481074145,10.7417136240349));
#75661=CARTESIAN_POINT('Ctrl Pts',(89.1329561745072,57.3695508838224,10.7815482876868));
#75662=CARTESIAN_POINT('Ctrl Pts',(89.1780407333497,57.3649536602303,10.823908714183));
#75663=CARTESIAN_POINT('Ctrl Pts',(89.2238972625354,57.3602777196592,10.8669944664629));
#75664=CARTESIAN_POINT('Ctrl Pts',(89.2674390656458,57.3556017790881,10.9126930483951));
#75665=CARTESIAN_POINT('Ctrl Pts',(89.3083578507059,57.3509258385169,10.9607229112971));
#75666=CARTESIAN_POINT('Ctrl Pts',(89.3484771324116,57.3463412601445,11.0078143290216));
#75667=CARTESIAN_POINT('Ctrl Pts',(89.3860746294626,57.3417566817721,11.0571463401991));
#75668=CARTESIAN_POINT('Ctrl Pts',(89.4208962488789,57.3371721033997,11.1084158506966));
#75669=CARTESIAN_POINT('Ctrl Pts',(89.4556965859279,57.3325903270417,11.1596540261622));
#75670=CARTESIAN_POINT('Ctrl Pts',(89.4877241239766,57.3280085506838,11.2128269326882));
#75671=CARTESIAN_POINT('Ctrl Pts',(89.5167665162233,57.3234267743258,11.2676003292707));
#75672=CARTESIAN_POINT('Ctrl Pts',(89.5458018254284,57.3188461154004,11.3223603673719));
#75673=CARTESIAN_POINT('Ctrl Pts',(89.5718531957369,57.3142654564749,11.3787196711139));
#75674=CARTESIAN_POINT('Ctrl Pts',(89.594753936296,57.3096847975495,11.4363188863663));
#75675=CARTESIAN_POINT('Ctrl Pts',(89.6184820028855,57.3049386549639,11.4959989657719));
#75676=CARTESIAN_POINT('Ctrl Pts',(89.6388271637822,57.3001925123784,11.5570097429308));
#75677=CARTESIAN_POINT('Ctrl Pts',(89.6556591957603,57.2954463697929,11.6189306928439));
#75678=CARTESIAN_POINT('Ctrl Pts',(89.6719249235205,57.2908599084965,11.6787683473381));
#75679=CARTESIAN_POINT('Ctrl Pts',(89.6849101381656,57.2862734472001,11.7394553673784));
#75680=CARTESIAN_POINT('Ctrl Pts',(89.6945493016383,57.2816869859037,11.8006010841146));
#75681=CARTESIAN_POINT('Ctrl Pts',(89.7046918577976,57.2768610026737,11.8649400558162));
#75682=CARTESIAN_POINT('Ctrl Pts',(89.7111292185952,57.2720350194436,11.9297863078811));
#75683=CARTESIAN_POINT('Ctrl Pts',(89.7138471512364,57.2672090362135,11.9946808922782));
#75684=CARTESIAN_POINT('Ctrl Pts',(89.7165650838775,57.2623830529835,12.0595754766754));
#75685=CARTESIAN_POINT('Ctrl Pts',(89.7155636757222,57.2575570697534,12.124517746688));
#75686=CARTESIAN_POINT('Ctrl Pts',(89.7108918878337,57.2527310865233,12.1890544809313));
#75687=CARTESIAN_POINT('Ctrl Pts',(89.7064415504673,57.2481338629312,12.2505320665497));
#75688=CARTESIAN_POINT('Ctrl Pts',(89.6986427178016,57.2435366393392,12.3118941150787));
#75689=CARTESIAN_POINT('Ctrl Pts',(89.6875086356423,57.2389394157471,12.3727468503782));
#75690=CARTESIAN_POINT('Ctrl Pts',(89.6761839076955,57.234263475176,12.4346415501142));
#75691=CARTESIAN_POINT('Ctrl Pts',(89.6614085816817,57.2295875346049,12.496008795041));
#75692=CARTESIAN_POINT('Ctrl Pts',(89.6432519754239,57.2249115940337,12.5564368708864));
#75693=CARTESIAN_POINT('Ctrl Pts',(89.6254501271968,57.2203270156613,12.6156842555341));
#75694=CARTESIAN_POINT('Ctrl Pts',(89.6043980960972,57.2157424372889,12.6740283306222));
#75695=CARTESIAN_POINT('Ctrl Pts',(89.5802126982047,57.2111578589165,12.7310912293762));
#75696=CARTESIAN_POINT('Ctrl Pts',(89.5560420820062,57.2065760825585,12.7881192522803));
#75697=CARTESIAN_POINT('Ctrl Pts',(89.5287420945357,57.2019943062006,12.8438671837755));
#75698=CARTESIAN_POINT('Ctrl Pts',(89.4984783620945,57.1974125298426,12.8979753349112));
#75699=CARTESIAN_POINT('Ctrl Pts',(89.4682220105632,57.1928318709172,12.9520702898098));
#75700=CARTESIAN_POINT('Ctrl Pts',(89.4350035973426,57.1882512119917,13.0045258141742));
#75701=CARTESIAN_POINT('Ctrl Pts',(89.3990346105331,57.1836705530663,13.0550069542538));
#75702=CARTESIAN_POINT('Ctrl Pts',(89.3617661863101,57.1789244104807,13.1073118065897));
#75703=CARTESIAN_POINT('Ctrl Pts',(89.3215449308692,57.1741782678952,13.1574963770492));
#75704=CARTESIAN_POINT('Ctrl Pts',(89.2786535032484,57.1694321253097,13.2052231701041));
#75705=CARTESIAN_POINT('Ctrl Pts',(89.237205133507,57.1648456640133,13.251344222138));
#75706=CARTESIAN_POINT('Ctrl Pts',(89.1932638475326,57.1602592027169,13.295169940474));
#75707=CARTESIAN_POINT('Ctrl Pts',(89.147122306736,57.1556727414205,13.3364333669016));
#75708=CARTESIAN_POINT('Ctrl Pts',(89.0985710844093,57.1508467581905,13.3798517217258));
#75709=CARTESIAN_POINT('Ctrl Pts',(89.0475839917287,57.1460207749604,13.420432411726));
#75710=CARTESIAN_POINT('Ctrl Pts',(88.9945388808011,57.1411947917303,13.4579145467853));
#75711=CARTESIAN_POINT('Ctrl Pts',(88.9414937698736,57.1363688085003,13.4953966818446));
#75712=CARTESIAN_POINT('Ctrl Pts',(88.8863912314035,57.1315428252702,13.5297799845778));
#75713=CARTESIAN_POINT('Ctrl Pts',(88.8296385826915,57.1267168420401,13.5608597614923));
#75714=CARTESIAN_POINT('Ctrl Pts',(88.7755761039937,57.1221196184481,13.5904663052485));
#75715=CARTESIAN_POINT('Ctrl Pts',(88.7197944707422,57.117522394856,13.6171970400385));
#75716=CARTESIAN_POINT('Ctrl Pts',(88.6626316871176,57.1129251712639,13.640849510253));
#75717=CARTESIAN_POINT('Ctrl Pts',(88.6044901210713,57.1082492306928,13.6649069751268));
#75718=CARTESIAN_POINT('Ctrl Pts',(88.5449200808534,57.1035732901217,13.6857794286762));
#75719=CARTESIAN_POINT('Ctrl Pts',(88.4843050542421,57.0988973495505,13.7033017929596));
#75720=CARTESIAN_POINT('Ctrl Pts',(88.4248743716193,57.0943127711781,13.7204817915301));
#75721=CARTESIAN_POINT('Ctrl Pts',(88.3644396833116,57.0897281928057,13.7344412886722));
#75722=CARTESIAN_POINT('Ctrl Pts',(88.3033818040932,57.0851436144333,13.7450734695764));
#75723=CARTESIAN_POINT('Ctrl Pts',(88.2423612423872,57.0805618380753,13.7556991522768));
#75724=CARTESIAN_POINT('Ctrl Pts',(88.1807187454674,57.0759800617174,13.7630014639232));
#75725=CARTESIAN_POINT('Ctrl Pts',(88.1188463311372,57.0713982853594,13.7669244558358));
#75726=CARTESIAN_POINT('Ctrl Pts',(88.0569890066415,57.066817626434,13.7708464909843));
#75727=CARTESIAN_POINT('Ctrl Pts',(87.9949023838495,57.0622369675085,13.7713908103042));
#75728=CARTESIAN_POINT('Ctrl Pts',(87.9329825753824,57.057656308583,13.7685534109261));
#75729=CARTESIAN_POINT('Ctrl Pts',(87.8688258143933,57.0529101659975,13.7656135059386));
#75730=CARTESIAN_POINT('Ctrl Pts',(87.8048487350968,57.048164023412,13.7590428266637));
#75731=CARTESIAN_POINT('Ctrl Pts',(87.7414881885438,57.0434178808265,13.7488957837863));
#75732=CARTESIAN_POINT('Ctrl Pts',(87.6802593718263,57.0388314195301,13.7390901324406));
#75733=CARTESIAN_POINT('Ctrl Pts',(87.6196067588616,57.0342449582337,13.7259451432318));
#75734=CARTESIAN_POINT('Ctrl Pts',(87.5599133660812,57.0296584969373,13.7095618894036));
#75735=CARTESIAN_POINT('Ctrl Pts',(87.4971025640516,57.0248325137073,13.6923230416036));
#75736=CARTESIAN_POINT('Ctrl Pts',(87.4353545312499,57.0200065304772,13.6714986216592));
#75737=CARTESIAN_POINT('Ctrl Pts',(87.3750933935017,57.0151805472471,13.6472645646481));
#75738=CARTESIAN_POINT('Ctrl Pts',(87.3148322557535,57.010354564017,13.6230305076371));
#75739=CARTESIAN_POINT('Ctrl Pts',(87.2560585664935,57.005528580787,13.5953871593694));
#75740=CARTESIAN_POINT('Ctrl Pts',(87.1991652214584,57.0007025975569,13.5645656902353));
#75741=CARTESIAN_POINT('Ctrl Pts',(87.1449687156773,56.9961053739648,13.5352052100406));
#75742=CARTESIAN_POINT('Ctrl Pts',(87.0922557705887,56.9915081503727,13.5028405964833));
#75743=CARTESIAN_POINT('Ctrl Pts',(87.0413798064858,56.9869109267807,13.4676460023592));
#75744=CARTESIAN_POINT('Ctrl Pts',(86.9896327074207,56.9822349862095,13.4318487810031));
#75745=CARTESIAN_POINT('Ctrl Pts',(86.9397866011751,56.9775590456384,13.3931239220507));
#75746=CARTESIAN_POINT('Ctrl Pts',(86.8921881765191,56.9728831050673,13.3517040636318));
#75747=CARTESIAN_POINT('Ctrl Pts',(86.8455197672612,56.9682985266949,13.3110934989321));
#75748=CARTESIAN_POINT('Ctrl Pts',(86.8010123979926,56.9637139483225,13.2678926518096));
#75749=CARTESIAN_POINT('Ctrl Pts',(86.7589623595588,56.95912936995,13.2223635165978));
#75750=CARTESIAN_POINT('Ctrl Pts',(86.716938021376,56.9545475935921,13.1768622080004));
#75751=CARTESIAN_POINT('Ctrl Pts',(86.6773683806839,56.9499658172341,13.1290358061143));
#75752=CARTESIAN_POINT('Ctrl Pts',(86.6405130711245,56.9453840408761,13.0791833069003));
#75753=CARTESIAN_POINT('Ctrl Pts',(86.6036667500704,56.9408033819507,13.0293429660282));
#75754=CARTESIAN_POINT('Ctrl Pts',(86.569533748481,56.9362227230252,12.9774779179155));
#75755=CARTESIAN_POINT('Ctrl Pts',(86.5383322802473,56.9316420640998,12.9239187740098));
#75756=CARTESIAN_POINT('Ctrl Pts',(86.5060036088653,56.9268959215143,12.8684247200164));
#75757=CARTESIAN_POINT('Ctrl Pts',(86.4768226869568,56.9221497789288,12.8111122929345));
#75758=CARTESIAN_POINT('Ctrl Pts',(86.4509807504232,56.9174036363432,12.7523780128688));
#75759=CARTESIAN_POINT('Ctrl Pts',(86.426008251262,56.9128171750468,12.6956198145131));
#75760=CARTESIAN_POINT('Ctrl Pts',(86.4041537327394,56.9082307137504,12.6375344444024));
#75761=CARTESIAN_POINT('Ctrl Pts',(86.3855400287221,56.9036442524541,12.5784985047522));
#75762=CARTESIAN_POINT('Ctrl Pts',(86.3659542483934,56.898818269224,12.5163794904813));
#75763=CARTESIAN_POINT('Ctrl Pts',(86.3499572278478,56.8939922859939,12.4532085212426));
#75764=CARTESIAN_POINT('Ctrl Pts',(86.3376312056248,56.8891663027639,12.3894373410898));
#75765=CARTESIAN_POINT('Ctrl Pts',(86.3253051834018,56.8843403195338,12.325666160937));
#75766=CARTESIAN_POINT('Ctrl Pts',(86.3166501691614,56.8795143363037,12.2612954223893));
#75767=CARTESIAN_POINT('Ctrl Pts',(86.3116850579265,56.8746883530737,12.1967805920066));
#75768=CARTESIAN_POINT('Ctrl Pts',(86.3083573900941,56.8714539302392,12.1535420993296));
#75769=CARTESIAN_POINT('Ctrl Pts',(86.3066797541958,56.8682195074047,12.1101749998648));
#75770=CARTESIAN_POINT('Ctrl Pts',(86.3066601734137,56.8649850845702,12.0667688380001));
#75771=CARTESIAN_POINT('',(86.3066603287391,56.0712350846273,12.0670585679921));
#75772=CARTESIAN_POINT('Ctrl Pts',(86.3066601734134,56.8649850845176,12.0667688372946));
#75773=CARTESIAN_POINT('Ctrl Pts',(86.3066326469133,56.8604381556952,12.0057487608988));
#75774=CARTESIAN_POINT('Ctrl Pts',(86.3098864040988,56.8558912268728,11.9445956778901));
#75775=CARTESIAN_POINT('Ctrl Pts',(86.3164380357149,56.8513442980503,11.88369644875));
#75776=CARTESIAN_POINT('Ctrl Pts',(86.3229791074586,56.8468046979349,11.8228953765471));
#75777=CARTESIAN_POINT('Ctrl Pts',(86.3328074517629,56.8422650978195,11.7623478602083));
#75778=CARTESIAN_POINT('Ctrl Pts',(86.3458876518779,56.8377254977041,11.7024402336185));
#75779=CARTESIAN_POINT('Ctrl Pts',(86.3589562899846,56.8331899102868,11.6425855613012));
#75780=CARTESIAN_POINT('Ctrl Pts',(86.375270979909,56.8286543228695,11.5833701651223));
#75781=CARTESIAN_POINT('Ctrl Pts',(86.3947447908381,56.8241187354522,11.5251729163059));
#75782=CARTESIAN_POINT('Ctrl Pts',(86.4142089121486,56.8195854048152,11.4670046247979));
#75783=CARTESIAN_POINT('Ctrl Pts',(86.4368288739004,56.8150520741782,11.4098539698692));
#75784=CARTESIAN_POINT('Ctrl Pts',(86.4624677567148,56.8105187435412,11.354085168643));
#75785=CARTESIAN_POINT('Ctrl Pts',(86.4881037872398,56.8059859172308,11.2983225716169));
#75786=CARTESIAN_POINT('Ctrl Pts',(86.516757853045,56.8014530909204,11.2439419956563));
#75787=CARTESIAN_POINT('Ctrl Pts',(86.5482455976834,56.79692026461,11.1912861072879));
#75788=CARTESIAN_POINT('Ctrl Pts',(86.57976336295,56.7923831166724,11.1385800164404));
#75789=CARTESIAN_POINT('Ctrl Pts',(86.6141199317628,56.7878459687348,11.0876023433603));
#75790=CARTESIAN_POINT('Ctrl Pts',(86.6510865547072,56.7833088207972,11.0386683802627));
#75791=CARTESIAN_POINT('Ctrl Pts',(86.6880724563637,56.7787693066611,10.9897088972851));
#75792=CARTESIAN_POINT('Ctrl Pts',(86.7276707835967,56.774229792525,10.9427956426883));
#75793=CARTESIAN_POINT('Ctrl Pts',(86.7696133021856,56.7696902783889,10.898209821034));
#75794=CARTESIAN_POINT('Ctrl Pts',(86.8116301298614,56.7651427216468,10.8535450071825));
#75795=CARTESIAN_POINT('Ctrl Pts',(86.8559990591959,56.7605951649048,10.8112162136019));
#75796=CARTESIAN_POINT('Ctrl Pts',(86.9024168423656,56.7560476081627,10.7714660227675));
#75797=CARTESIAN_POINT('Ctrl Pts',(86.927504416768,56.7535897749719,10.7499821042783));
#75798=CARTESIAN_POINT('Ctrl Pts',(86.953189941594,56.7511319417812,10.7292507026567));
#75799=CARTESIAN_POINT('Ctrl Pts',(86.9794221332777,56.7486741085904,10.7093047724383));
#75800=CARTESIAN_POINT('Ctrl Pts',(87.0284878106936,56.7440768849983,10.6719971547732));
#75801=CARTESIAN_POINT('Ctrl Pts',(87.0796806949913,56.7394796614063,10.6372781198228));
#75802=CARTESIAN_POINT('Ctrl Pts',(87.1326965997162,56.7348824378142,10.6053980786505));
#75803=CARTESIAN_POINT('Ctrl Pts',(87.1866202810107,56.7302064972431,10.572972164413));
#75804=CARTESIAN_POINT('Ctrl Pts',(87.2424296358469,56.7255305566719,10.5434837781992));
#75805=CARTESIAN_POINT('Ctrl Pts',(87.2997699472393,56.7208546161008,10.5171531232397));
#75806=CARTESIAN_POINT('Ctrl Pts',(87.3559898986006,56.7162700377284,10.4913369372933));
#75807=CARTESIAN_POINT('Ctrl Pts',(87.4136810337534,56.711685459356,10.4685564185088));
#75808=CARTESIAN_POINT('Ctrl Pts',(87.472482625749,56.7071008809836,10.4489737561716));
#75809=CARTESIAN_POINT('Ctrl Pts',(87.5312482792357,56.7025191046256,10.4294030624166));
#75810=CARTESIAN_POINT('Ctrl Pts',(87.5911225618507,56.6979373282677,10.4130265101782));
#75811=CARTESIAN_POINT('Ctrl Pts',(87.651726113159,56.6933555519097,10.399957650648));
#75812=CARTESIAN_POINT('Ctrl Pts',(87.7123148840911,56.6887748929843,10.3868919784338));
#75813=CARTESIAN_POINT('Ctrl Pts',(87.7736320732545,56.6841942340588,10.3771325047629));
#75814=CARTESIAN_POINT('Ctrl Pts',(87.8352865557474,56.6796135751334,10.3707420193054));
#75815=CARTESIAN_POINT('Ctrl Pts',(87.8991684054352,56.6748674325478,10.3641206672978));
#75816=CARTESIAN_POINT('Ctrl Pts',(87.9634118138756,56.6701212899623,10.3611165079455));
#75817=CARTESIAN_POINT('Ctrl Pts',(88.0275766938965,56.6653751473768,10.3617406157455));
#75818=CARTESIAN_POINT('Ctrl Pts',(88.0895827827364,56.6607886860804,10.3623437257908));
#75819=CARTESIAN_POINT('Ctrl Pts',(88.1515150214752,56.656202224784,10.3663347163375));
#75820=CARTESIAN_POINT('Ctrl Pts',(88.2129796301034,56.6516157634876,10.3736705212568));
#75821=CARTESIAN_POINT('Ctrl Pts',(88.2776541474084,56.6467897802576,10.3813894289792));
#75822=CARTESIAN_POINT('Ctrl Pts',(88.3418102165966,56.6419637970275,10.3928119859271));
#75823=CARTESIAN_POINT('Ctrl Pts',(88.405002285617,56.6371378137974,10.4078272000396));
#75824=CARTESIAN_POINT('Ctrl Pts',(88.4681943546375,56.6323118305674,10.4228424141521));
#75825=CARTESIAN_POINT('Ctrl Pts',(88.5304218248333,56.6274858473373,10.4414500256515));
#75826=CARTESIAN_POINT('Ctrl Pts',(88.5912618242507,56.6226598641072,10.4634797814326));
#75827=CARTESIAN_POINT('Ctrl Pts',(88.6492179064269,56.6180626405152,10.484465290121));
#75828=CARTESIAN_POINT('Ctrl Pts',(88.7061530598434,56.6134654169231,10.5086419544082));
#75829=CARTESIAN_POINT('Ctrl Pts',(88.7616919185075,56.608868193331,10.535890043465));
#75830=CARTESIAN_POINT('Ctrl Pts',(88.8181817535786,56.6041922527599,10.5636046939609));
#75831=CARTESIAN_POINT('Ctrl Pts',(88.8732264961636,56.5995163121888,10.5944968502872));
#75832=CARTESIAN_POINT('Ctrl Pts',(88.926448750812,56.5948403716176,10.6283879451546));
#75833=CARTESIAN_POINT('Ctrl Pts',(88.9786311072557,56.5902557932452,10.6616168491971));
#75834=CARTESIAN_POINT('Ctrl Pts',(89.0290611037177,56.5856712148728,10.6977282680028));
#75835=CARTESIAN_POINT('Ctrl Pts',(89.0774068236945,56.5810866365004,10.736507118493));
#75836=CARTESIAN_POINT('Ctrl Pts',(89.1257229956094,56.5765048601425,10.7752622680252));
#75837=CARTESIAN_POINT('Ctrl Pts',(89.1719570206811,56.5719230837845,10.8166812987665));
#75838=CARTESIAN_POINT('Ctrl Pts',(89.215807737519,56.5673413074265,10.8605070920099));
#75839=CARTESIAN_POINT('Ctrl Pts',(89.2596477597674,56.5627606485011,10.9043221967425));
#75840=CARTESIAN_POINT('Ctrl Pts',(89.301105267772,56.5581799895756,10.9505425390528));
#75841=CARTESIAN_POINT('Ctrl Pts',(89.3399153649386,56.5535993306502,10.9988735836697));
#75842=CARTESIAN_POINT('Ctrl Pts',(89.3801275391931,56.5488531880647,11.0489506648913));
#75843=CARTESIAN_POINT('Ctrl Pts',(89.4174969423386,56.5441070454791,11.1012934600975));
#75844=CARTESIAN_POINT('Ctrl Pts',(89.4517755677182,56.5393609028936,11.1555382495314));
#75845=CARTESIAN_POINT('Ctrl Pts',(89.4849009080898,56.5347744415972,11.2079580036344));
#75846=CARTESIAN_POINT('Ctrl Pts',(89.5151399621241,56.5301879803008,11.2621532968973));
#75847=CARTESIAN_POINT('Ctrl Pts',(89.5423153247976,56.5256015190044,11.3177699473826));
#75848=CARTESIAN_POINT('Ctrl Pts',(89.5709098851914,56.5207755357744,11.3762911045904));
#75849=CARTESIAN_POINT('Ctrl Pts',(89.596111725844,56.5159495525443,11.436385557318));
#75850=CARTESIAN_POINT('Ctrl Pts',(89.6177724266541,56.5111235693142,11.4976187858981));
#75851=CARTESIAN_POINT('Ctrl Pts',(89.6394331274642,56.5062975860842,11.5588520144781));
#75852=CARTESIAN_POINT('Ctrl Pts',(89.6575525819659,56.5014716028541,11.6212233750633));
#75853=CARTESIAN_POINT('Ctrl Pts',(89.6720444581726,56.496645619624,11.6842852588988));
#75854=CARTESIAN_POINT('Ctrl Pts',(89.6858493953253,56.492048396032,11.7443579044736));
#75855=CARTESIAN_POINT('Ctrl Pts',(89.6964196246031,56.4874511724399,11.8053037250327));
#75856=CARTESIAN_POINT('Ctrl Pts',(89.7036521363606,56.4828539488478,11.8667424258054));
#75857=CARTESIAN_POINT('Ctrl Pts',(89.7110084884024,56.4781780082767,11.9292331243382));
#75858=CARTESIAN_POINT('Ctrl Pts',(89.7149115341484,56.4735020677056,11.9922332453114));
#75859=CARTESIAN_POINT('Ctrl Pts',(89.7153065929332,56.4688261271344,12.0553288761405));
#75860=CARTESIAN_POINT('Ctrl Pts',(89.7156939327493,56.464241548762,12.117191694988));
#75861=CARTESIAN_POINT('Ctrl Pts',(89.7127091330007,56.4596569703896,12.1791457915578));
#75862=CARTESIAN_POINT('Ctrl Pts',(89.7063528584347,56.4550723920172,12.2407956549726));
#75863=CARTESIAN_POINT('Ctrl Pts',(89.7000004687129,56.4504906156592,12.3024078390647));
#75864=CARTESIAN_POINT('Ctrl Pts',(89.6902807421184,56.4459088393013,12.3637156533857));
#75865=CARTESIAN_POINT('Ctrl Pts',(89.6772463399544,56.4413270629433,12.4243266250066));
#75866=CARTESIAN_POINT('Ctrl Pts',(89.6642151167026,56.4367464040179,12.4849228144415));
#75867=CARTESIAN_POINT('Ctrl Pts',(89.6478709296617,56.4321657450924,12.5448220011071));
#75868=CARTESIAN_POINT('Ctrl Pts',(89.6283175445639,56.427585086167,12.6036418841998));
#75869=CARTESIAN_POINT('Ctrl Pts',(89.6080577620272,56.4228389435814,12.6645867300321));
#75870=CARTESIAN_POINT('Ctrl Pts',(89.5843525896718,56.4180928009959,12.7243722241343));
#75871=CARTESIAN_POINT('Ctrl Pts',(89.5573730776615,56.4133466584104,12.7825927297172));
#75872=CARTESIAN_POINT('Ctrl Pts',(89.5313012761087,56.408760197114,12.8388544392428));
#75873=CARTESIAN_POINT('Ctrl Pts',(89.5021722883785,56.4041737358176,12.8936543687552));
#75874=CARTESIAN_POINT('Ctrl Pts',(89.4701874459501,56.3995872745212,12.9466513686935));
#75875=CARTESIAN_POINT('Ctrl Pts',(89.4365322370208,56.3947612912912,13.0024160675359));
#75876=CARTESIAN_POINT('Ctrl Pts',(89.3997150622263,56.3899353080611,13.0561838242406));
#75877=CARTESIAN_POINT('Ctrl Pts',(89.3600204678588,56.385109324831,13.1075942650083));
#75878=CARTESIAN_POINT('Ctrl Pts',(89.3203258734913,56.380283341601,13.1590047057759));
#75879=CARTESIAN_POINT('Ctrl Pts',(89.2777543427136,56.3754573583709,13.2080573919401));
#75880=CARTESIAN_POINT('Ctrl Pts',(89.2326350947542,56.3706313751408,13.2544370117364));
#75881=CARTESIAN_POINT('Ctrl Pts',(89.1896545742493,56.3660341515487,13.2986181603551));
#75882=CARTESIAN_POINT('Ctrl Pts',(89.1441859794039,56.3614369279567,13.3405553714379));
#75883=CARTESIAN_POINT('Ctrl Pts',(89.096492931602,56.3568397043646,13.3799558329876));
#75884=CARTESIAN_POINT('Ctrl Pts',(89.0479832490271,56.3521637637934,13.4200309376656));
#75885=CARTESIAN_POINT('Ctrl Pts',(88.9971725208118,56.3474878232223,13.4574811567165));
#75886=CARTESIAN_POINT('Ctrl Pts',(88.9443788249558,56.3428118826512,13.4920360460816));
#75887=CARTESIAN_POINT('Ctrl Pts',(88.8926166537863,56.3382273042788,13.5259157748838));
#75888=CARTESIAN_POINT('Ctrl Pts',(88.8389487539412,56.3336427259064,13.5570120067701));
#75889=CARTESIAN_POINT('Ctrl Pts',(88.7837077630397,56.3290581475339,13.5851107755981));
#75890=CARTESIAN_POINT('Ctrl Pts',(88.7285005344698,56.324476371176,13.6131923709479));
#75891=CARTESIAN_POINT('Ctrl Pts',(88.6717225740338,56.319894594818,13.6382799055139));
#75892=CARTESIAN_POINT('Ctrl Pts',(88.6137321699741,56.3153128184601,13.6602047443407));
#75893=CARTESIAN_POINT('Ctrl Pts',(88.5557559089797,56.3107321595346,13.6821242359996));
#75894=CARTESIAN_POINT('Ctrl Pts',(88.4965682673067,56.3061515006092,13.7008823832009));
#75895=CARTESIAN_POINT('Ctrl Pts',(88.4365467063585,56.3015708416837,13.7163590022499));
#75896=CARTESIAN_POINT('Ctrl Pts',(88.3743567701286,56.2968246990982,13.732394739017));
#75897=CARTESIAN_POINT('Ctrl Pts',(88.3112720546555,56.2920785565127,13.744907099911));
#75898=CARTESIAN_POINT('Ctrl Pts',(88.2477261213912,56.2873324139272,13.753819770903));
#75899=CARTESIAN_POINT('Ctrl Pts',(88.1863181551937,56.2827459526308,13.7624325801087));
#75900=CARTESIAN_POINT('Ctrl Pts',(88.1244800473313,56.2781594913344,13.7676841148125));
#75901=CARTESIAN_POINT('Ctrl Pts',(88.0626076067181,56.273573030038,13.7695584787523));
#75902=CARTESIAN_POINT('Ctrl Pts',(87.9975039589366,56.2687470468079,13.7715307288937));
#75903=CARTESIAN_POINT('Ctrl Pts',(87.932362938148,56.2639210635778,13.7697634056245));
#75904=CARTESIAN_POINT('Ctrl Pts',(87.8676416395676,56.2590950803478,13.764300096006));
#75905=CARTESIAN_POINT('Ctrl Pts',(87.8029203409871,56.2542690971177,13.7588367863876));
#75906=CARTESIAN_POINT('Ctrl Pts',(87.7386193952144,56.2494431138876,13.749677658403));
#75907=CARTESIAN_POINT('Ctrl Pts',(87.6751822704408,56.2446171306575,13.736928271385));
#75908=CARTESIAN_POINT('Ctrl Pts',(87.614752170973,56.2400199070655,13.7247832265331));
#75909=CARTESIAN_POINT('Ctrl Pts',(87.5548577224907,56.2354226834734,13.709330788809));
#75910=CARTESIAN_POINT('Ctrl Pts',(87.4958879104644,56.2308254598813,13.6906336112534));
#75911=CARTESIAN_POINT('Ctrl Pts',(87.4359083747724,56.2261495193102,13.6716162871345));
#75912=CARTESIAN_POINT('Ctrl Pts',(87.3768859767579,56.2214735787391,13.6492420711404));
#75913=CARTESIAN_POINT('Ctrl Pts',(87.3192204473137,56.2167976381679,13.62363149881));
#75914=CARTESIAN_POINT('Ctrl Pts',(87.2626816322662,56.2122130597955,13.5985213259528));
#75915=CARTESIAN_POINT('Ctrl Pts',(87.2074476270305,56.2076284814231,13.570300344805));
#75916=CARTESIAN_POINT('Ctrl Pts',(87.153878611326,56.2030439030507,13.5391319563018));
#75917=CARTESIAN_POINT('Ctrl Pts',(87.1003423360712,56.1984621266927,13.5079826173749));
#75918=CARTESIAN_POINT('Ctrl Pts',(87.0484694716465,56.1938803503348,13.4738896984878));
#75919=CARTESIAN_POINT('Ctrl Pts',(86.9985960269477,56.1892985739768,13.437062737787));
#75920=CARTESIAN_POINT('Ctrl Pts',(86.948734745699,56.1847179150514,13.4002447586775));
#75921=CARTESIAN_POINT('Ctrl Pts',(86.9008723254761,56.1801372561259,13.3606943636905));
#75922=CARTESIAN_POINT('Ctrl Pts',(86.8553144697435,56.1755565972005,13.3186634786549));
#75923=CARTESIAN_POINT('Ctrl Pts',(86.8081107633081,56.170810454615,13.2751141603971));
#75924=CARTESIAN_POINT('Ctrl Pts',(86.7633817923823,56.1660643120295,13.2289020444386));
#75925=CARTESIAN_POINT('Ctrl Pts',(86.7214268331923,56.161318169444,13.1803499822989));
#75926=CARTESIAN_POINT('Ctrl Pts',(86.6808834249297,56.1567317081476,13.1334314268927));
#75927=CARTESIAN_POINT('Ctrl Pts',(86.6429305862306,56.1521452468512,13.0843283492353));
#75928=CARTESIAN_POINT('Ctrl Pts',(86.6077963581465,56.1475587855548,13.0333646546619));
#75929=CARTESIAN_POINT('Ctrl Pts',(86.5708272910209,56.1427328023247,12.9797394478937));
#75930=CARTESIAN_POINT('Ctrl Pts',(86.536979647615,56.1379068190946,12.9240545032787));
#75931=CARTESIAN_POINT('Ctrl Pts',(86.506464737395,56.1330808358645,12.8667174777524));
#75932=CARTESIAN_POINT('Ctrl Pts',(86.4759498271751,56.1282548526345,12.8093804522262));
#75933=CARTESIAN_POINT('Ctrl Pts',(86.4487678510513,56.1234288694044,12.7503919666829));
#75934=CARTESIAN_POINT('Ctrl Pts',(86.425070662992,56.1186028861743,12.6901818433898));
#75935=CARTESIAN_POINT('Ctrl Pts',(86.3995423106974,56.1134039824159,12.625319074217));
#75936=CARTESIAN_POINT('Ctrl Pts',(86.3779687741055,56.1082050786575,12.5588164507142));
#75937=CARTESIAN_POINT('Ctrl Pts',(86.360535813958,56.1030061748991,12.4911385729297));
#75938=CARTESIAN_POINT('Ctrl Pts',(86.3427800146496,56.0977109931871,12.4222073756234));
#75939=CARTESIAN_POINT('Ctrl Pts',(86.3293199176743,56.0924158114752,12.3520571510168));
#75940=CARTESIAN_POINT('Ctrl Pts',(86.320301082368,56.0871206297632,12.2812022432926));
#75941=CARTESIAN_POINT('Ctrl Pts',(86.3112822470618,56.0818254480512,12.2103473355684));
#75942=CARTESIAN_POINT('Ctrl Pts',(86.3067048800023,56.0765302663393,12.13878800421));
#75943=CARTESIAN_POINT('Ctrl Pts',(86.3066603287391,56.0712350846273,12.0670585679921));
#75944=CARTESIAN_POINT('',(86.3066605389047,55.2774850845187,12.0646446574837));
#75945=CARTESIAN_POINT('Ctrl Pts',(86.3066603287386,56.0712350845702,12.0670585672184));
#75946=CARTESIAN_POINT('Ctrl Pts',(86.3066214924812,56.0666191618022,12.0045304887141));
#75947=CARTESIAN_POINT('Ctrl Pts',(86.310027997416,56.0620032390342,11.9419890370945));
#75948=CARTESIAN_POINT('Ctrl Pts',(86.3168577898452,56.0573873162662,11.8798360739244));
#75949=CARTESIAN_POINT('Ctrl Pts',(86.3236886814535,56.0527706506168,11.8176731079272));
#75950=CARTESIAN_POINT('Ctrl Pts',(86.3339438978837,56.0481539849675,11.7558992492126));
#75951=CARTESIAN_POINT('Ctrl Pts',(86.3475496637027,56.0435373193181,11.694909964736));
#75952=CARTESIAN_POINT('Ctrl Pts',(86.3611730542256,56.0389146733097,11.6338416756595));
#75953=CARTESIAN_POINT('Ctrl Pts',(86.3781555491344,56.0342920273012,11.573560476663));
#75954=CARTESIAN_POINT('Ctrl Pts',(86.3983727018363,56.0296693812928,11.5144494285949));
#75955=CARTESIAN_POINT('Ctrl Pts',(86.4186037073804,56.025043567836,11.4552978774931));
#75956=CARTESIAN_POINT('Ctrl Pts',(86.4420735959647,56.0204177543793,11.3973185353219));
#75957=CARTESIAN_POINT('Ctrl Pts',(86.4686098104151,56.0157919409226,11.3408742600954));
#75958=CARTESIAN_POINT('Ctrl Pts',(86.4951999452586,56.0111567280212,11.2843152926427));
#75959=CARTESIAN_POINT('Ctrl Pts',(86.524868612324,56.0065215151197,11.2292980601706));
#75960=CARTESIAN_POINT('Ctrl Pts',(86.557397738338,56.0018863022183,11.1761599579187));
#75961=CARTESIAN_POINT('Ctrl Pts',(86.5791475318828,55.9987870820426,11.1406304834152));
#75962=CARTESIAN_POINT('Ctrl Pts',(86.6021752031633,55.9956878618668,11.1059405079902));
#75963=CARTESIAN_POINT('Ctrl Pts',(86.6264055081682,55.9925886416911,11.0721826481747));
#75964=CARTESIAN_POINT('Ctrl Pts',(86.6623474946987,55.987991418099,11.0221079775279));
#75965=CARTESIAN_POINT('Ctrl Pts',(86.7010832335385,55.9833941945069,10.9738828250952));
#75966=CARTESIAN_POINT('Ctrl Pts',(86.7423955159203,55.9787969709148,10.9278359087667));
#75967=CARTESIAN_POINT('Ctrl Pts',(86.7844151770062,55.9741210303437,10.8810005439159));
#75968=CARTESIAN_POINT('Ctrl Pts',(86.8291002149384,55.9694450897726,10.8364191981116));
#75969=CARTESIAN_POINT('Ctrl Pts',(86.8761762461845,55.9647691492015,10.7944065573556));
#75970=CARTESIAN_POINT('Ctrl Pts',(86.9223324689652,55.9601845708291,10.7532147925657));
#75971=CARTESIAN_POINT('Ctrl Pts',(86.9707866931789,55.9555999924566,10.7144926120077));
#75972=CARTESIAN_POINT('Ctrl Pts',(87.0212417489732,55.9510154140842,10.6785010125682));
#75973=CARTESIAN_POINT('Ctrl Pts',(87.0716659675162,55.9464336377263,10.6425314105673));
#75974=CARTESIAN_POINT('Ctrl Pts',(87.1240881793043,55.9418518613683,10.6092893755345));
#75975=CARTESIAN_POINT('Ctrl Pts',(87.1781791156971,55.9372700850103,10.5789948855942));
#75976=CARTESIAN_POINT('Ctrl Pts',(87.2322568600514,55.9326894260849,10.5487077840652));
#75977=CARTESIAN_POINT('Ctrl Pts',(87.28800207716,55.9281087671594,10.521367049204));
#75978=CARTESIAN_POINT('Ctrl Pts',(87.3450593418189,55.923528108234,10.4971475928624));
#75979=CARTESIAN_POINT('Ctrl Pts',(87.4041778917956,55.9187819656485,10.472053169765));
#75980=CARTESIAN_POINT('Ctrl Pts',(87.4647045938634,55.9140358230629,10.4503101516155));
#75981=CARTESIAN_POINT('Ctrl Pts',(87.526222029381,55.9092896804774,10.4320583992068));
#75982=CARTESIAN_POINT('Ctrl Pts',(87.5856697454938,55.904703219181,10.4144207167088));
#75983=CARTESIAN_POINT('Ctrl Pts',(87.6460420538035,55.9001167578846,10.4000431442394));
#75984=CARTESIAN_POINT('Ctrl Pts',(87.70694989617,55.8955302965882,10.3890001878471));
#75985=CARTESIAN_POINT('Ctrl Pts',(87.7710385708246,55.8907043133582,10.3773805275216));
#75986=CARTESIAN_POINT('Ctrl Pts',(87.8357196106168,55.8858783301281,10.3694534150399));
#75987=CARTESIAN_POINT('Ctrl Pts',(87.9005345162743,55.881052346898,10.3652436351713));
#75988=CARTESIAN_POINT('Ctrl Pts',(87.9653494219317,55.876226363668,10.3610338553027));
#75989=CARTESIAN_POINT('Ctrl Pts',(88.0302975448992,55.8714003804379,10.3605413355845));
#75990=CARTESIAN_POINT('Ctrl Pts',(88.0949246575862,55.8665743972078,10.3637275519327));
#75991=CARTESIAN_POINT('Ctrl Pts',(88.1564883375595,55.8619771736158,10.3667627363225));
#75992=CARTESIAN_POINT('Ctrl Pts',(88.2180135259219,55.8573799500237,10.373148187565));
#75993=CARTESIAN_POINT('Ctrl Pts',(88.2791062460481,55.8527827264316,10.3828797201537));
#75994=CARTESIAN_POINT('Ctrl Pts',(88.3412450398043,55.8481067858605,10.3927778830642));
#75995=CARTESIAN_POINT('Ctrl Pts',(88.4029358815445,55.8434308452894,10.4061378626346));
#75996=CARTESIAN_POINT('Ctrl Pts',(88.4637655716076,55.8387549047182,10.4228998287485));
#75997=CARTESIAN_POINT('Ctrl Pts',(88.523406723419,55.8341703263458,10.4393342864058));
#75998=CARTESIAN_POINT('Ctrl Pts',(88.5822195583685,55.8295857479734,10.4590388431506));
#75999=CARTESIAN_POINT('Ctrl Pts',(88.639823622886,55.825001169601,10.4819054046868));
#76000=CARTESIAN_POINT('Ctrl Pts',(88.6973924808026,55.8204193932431,10.5047579905788));
#76001=CARTESIAN_POINT('Ctrl Pts',(88.753753561029,55.8158376168851,10.530768561845));
#76002=CARTESIAN_POINT('Ctrl Pts',(88.8085434603824,55.8112558405271,10.5597798087924));
#76003=CARTESIAN_POINT('Ctrl Pts',(88.8633199972296,55.8066751816017,10.588783980294));
#76004=CARTESIAN_POINT('Ctrl Pts',(88.9165256642212,55.8020945226762,10.6207871365946));
#76005=CARTESIAN_POINT('Ctrl Pts',(88.9678207320166,55.7975138637508,10.6555855494277));
#76006=CARTESIAN_POINT('Ctrl Pts',(89.0209689165142,55.7927677211653,10.6916411108095));
#76007=CARTESIAN_POINT('Ctrl Pts',(89.0720652947151,55.7880215785798,10.7306974884732));
#76008=CARTESIAN_POINT('Ctrl Pts',(89.1207659592515,55.7832754359943,10.7724798605021));
#76009=CARTESIAN_POINT('Ctrl Pts',(89.1678281174105,55.7786889746979,10.8128564882012));
#76010=CARTESIAN_POINT('Ctrl Pts',(89.2126528857788,55.7741025134015,10.8557781650263));
#76011=CARTESIAN_POINT('Ctrl Pts',(89.2549666455938,55.7695160521051,10.9009584469857));
#76012=CARTESIAN_POINT('Ctrl Pts',(89.2994901860911,55.764690068875,10.9484982099916));
#76013=CARTESIAN_POINT('Ctrl Pts',(89.3412328370882,55.7598640856449,10.9985384648737));
#76014=CARTESIAN_POINT('Ctrl Pts',(89.3799250869373,55.7550381024149,11.0507074599143));
#76015=CARTESIAN_POINT('Ctrl Pts',(89.4186173367865,55.7502121191848,11.102876454955));
#76016=CARTESIAN_POINT('Ctrl Pts',(89.4542588945896,55.7453861359547,11.1571736059858));
#76017=CARTESIAN_POINT('Ctrl Pts',(89.4866357527621,55.7405601527246,11.2131964113759));
#76018=CARTESIAN_POINT('Ctrl Pts',(89.5174778939656,55.7359629291326,11.2665636425399));
#76019=CARTESIAN_POINT('Ctrl Pts',(89.5454845272557,55.7313657055405,11.3217157166837));
#76020=CARTESIAN_POINT('Ctrl Pts',(89.570445476531,55.7267684819484,11.3783193754897));
#76021=CARTESIAN_POINT('Ctrl Pts',(89.5958338251882,55.7220925413773,11.435892242979));
#76022=CARTESIAN_POINT('Ctrl Pts',(89.61807085976,55.7174166008062,11.4949664615704));
#76023=CARTESIAN_POINT('Ctrl Pts',(89.6369827258091,55.712740660235,11.5551624416996));
#76024=CARTESIAN_POINT('Ctrl Pts',(89.6555250769686,55.7081560818626,11.6141822654994));
#76025=CARTESIAN_POINT('Ctrl Pts',(89.6708708706124,55.7035715034902,11.6742799004675));
#76026=CARTESIAN_POINT('Ctrl Pts',(89.6829045615013,55.6989869251178,11.7350770892925));
#76027=CARTESIAN_POINT('Ctrl Pts',(89.6949308976079,55.6944051487598,11.7958371199345));
#76028=CARTESIAN_POINT('Ctrl Pts',(89.703649046219,55.6898233724019,11.8572953583299));
#76029=CARTESIAN_POINT('Ctrl Pts',(89.7089940571011,55.6852415960439,11.9190611771885));
#76030=CARTESIAN_POINT('Ctrl Pts',(89.7143377644083,55.6806609371185,11.9808119322097));
#76031=CARTESIAN_POINT('Ctrl Pts',(89.716309923228,55.676080278193,12.0428696118538));
#76032=CARTESIAN_POINT('Ctrl Pts',(89.7148974212158,55.6714996192676,12.1048383003497));
#76033=CARTESIAN_POINT('Ctrl Pts',(89.7134338903,55.6667534766821,12.1690457072371));
#76034=CARTESIAN_POINT('Ctrl Pts',(89.7083364128982,55.6620073340966,12.2331569872555));
#76035=CARTESIAN_POINT('Ctrl Pts',(89.6996493377902,55.657261191511,12.2967341534767));
#76036=CARTESIAN_POINT('Ctrl Pts',(89.6912545344222,55.6526747302146,12.3581723018159));
#76037=CARTESIAN_POINT('Ctrl Pts',(89.6795080239475,55.6480882689183,12.4191112031222));
#76038=CARTESIAN_POINT('Ctrl Pts',(89.6645020435493,55.6435018076219,12.4791656176138));
#76039=CARTESIAN_POINT('Ctrl Pts',(89.6487123954803,55.6386758243918,12.5423562952405));
#76040=CARTESIAN_POINT('Ctrl Pts',(89.6293136802233,55.6338498411617,12.6045669524247));
#76041=CARTESIAN_POINT('Ctrl Pts',(89.6064720314822,55.6290238579316,12.6653695290536));
#76042=CARTESIAN_POINT('Ctrl Pts',(89.5836303827412,55.6241978747016,12.7261721056825));
#76043=CARTESIAN_POINT('Ctrl Pts',(89.5573461335055,55.6193718914715,12.7855660405143));
#76044=CARTESIAN_POINT('Ctrl Pts',(89.5278413564675,55.6145459082414,12.8431532248596));
#76045=CARTESIAN_POINT('Ctrl Pts',(89.4997351549721,55.6099486846493,12.8980106808127));
#76046=CARTESIAN_POINT('Ctrl Pts',(89.4685914931177,55.6053514610573,12.9514540631619));
#76047=CARTESIAN_POINT('Ctrl Pts',(89.4345763490148,55.6007542374652,13.0031260396156));
#76048=CARTESIAN_POINT('Ctrl Pts',(89.3999787730742,55.5960782968941,13.0556827809292));
#76049=CARTESIAN_POINT('Ctrl Pts',(89.3624106114259,55.5914023563229,13.1064063675443));
#76050=CARTESIAN_POINT('Ctrl Pts',(89.3220964668672,55.5867264157518,13.1549448517571));
#76051=CARTESIAN_POINT('Ctrl Pts',(89.2825700117221,55.5821418373794,13.20253495295));
#76052=CARTESIAN_POINT('Ctrl Pts',(89.2404042557537,55.577557259007,13.2480241619443));
#76053=CARTESIAN_POINT('Ctrl Pts',(89.1958543093425,55.5729726806346,13.2911102404407));
#76054=CARTESIAN_POINT('Ctrl Pts',(89.1513315910827,55.5683909042766,13.3341699854762));
#76055=CARTESIAN_POINT('Ctrl Pts',(89.104427936902,55.5638091279187,13.3748291591812));
#76056=CARTESIAN_POINT('Ctrl Pts',(89.0554362921307,55.5592273515607,13.4128213197304));
#76057=CARTESIAN_POINT('Ctrl Pts',(89.0064565957507,55.5546466926353,13.4508042145119));
#76058=CARTESIAN_POINT('Ctrl Pts',(88.9553903217678,55.5500660337098,13.4861210755661));
#76059=CARTESIAN_POINT('Ctrl Pts',(88.902562975284,55.5454853747844,13.5185461427103));
#76060=CARTESIAN_POINT('Ctrl Pts',(88.8478271560696,55.5407392321988,13.5521426174787));
#76061=CARTESIAN_POINT('Ctrl Pts',(88.7912010469939,55.5359930896133,13.5826339977754));
#76062=CARTESIAN_POINT('Ctrl Pts',(88.7330766648711,55.5312469470278,13.6098199783811));
#76063=CARTESIAN_POINT('Ctrl Pts',(88.6769078447862,55.5266604857314,13.6360913020099));
#76064=CARTESIAN_POINT('Ctrl Pts',(88.6193404909143,55.522074024435,13.6592759945665));
#76065=CARTESIAN_POINT('Ctrl Pts',(88.5607482806862,55.5174875631386,13.6792425928801));
#76066=CARTESIAN_POINT('Ctrl Pts',(88.4990961690254,55.5126615799086,13.7002519206376));
#76067=CARTESIAN_POINT('Ctrl Pts',(88.4363098397077,55.5078355966785,13.7176976327675));
#76068=CARTESIAN_POINT('Ctrl Pts',(88.3728390258118,55.5030096134484,13.7314871224358));
#76069=CARTESIAN_POINT('Ctrl Pts',(88.3093682119159,55.4981836302183,13.7452766121042));
#76070=CARTESIAN_POINT('Ctrl Pts',(88.245213565566,55.4933576469883,13.7554098546456));
#76071=CARTESIAN_POINT('Ctrl Pts',(88.180829998254,55.4885316637582,13.7618574843698));
#76072=CARTESIAN_POINT('Ctrl Pts',(88.1194983191995,55.4839344401661,13.7679994857129));
#76073=CARTESIAN_POINT('Ctrl Pts',(88.0577071185754,55.479337216574,13.770822660529));
#76074=CARTESIAN_POINT('Ctrl Pts',(87.9958466251266,55.474739992982,13.7702726339497));
#76075=CARTESIAN_POINT('Ctrl Pts',(87.9329269116793,55.4700640524108,13.7697131894185));
#76076=CARTESIAN_POINT('Ctrl Pts',(87.8699360282904,55.4653881118397,13.7656637921032));
#76077=CARTESIAN_POINT('Ctrl Pts',(87.8072914779564,55.4607121712686,13.7581222395698));
#76078=CARTESIAN_POINT('Ctrl Pts',(87.745870926039,55.4561275928962,13.7507280398119));
#76079=CARTESIAN_POINT('Ctrl Pts',(87.6847838246336,55.4515430145238,13.7399769862261));
#76080=CARTESIAN_POINT('Ctrl Pts',(87.6244224620891,55.4469584361513,13.7259194687643));
#76081=CARTESIAN_POINT('Ctrl Pts',(87.564097991358,55.4423766597934,13.7118705430123));
#76082=CARTESIAN_POINT('Ctrl Pts',(87.5044988747256,55.4377948834354,13.6945192756662));
#76083=CARTESIAN_POINT('Ctrl Pts',(87.4460078487948,55.4332131070774,13.6739672585835));
#76084=CARTESIAN_POINT('Ctrl Pts',(87.3875310880244,55.428632448152,13.6534202538564));
#76085=CARTESIAN_POINT('Ctrl Pts',(87.3301623615197,55.4240517892265,13.6296742177143));
#76086=CARTESIAN_POINT('Ctrl Pts',(87.2742678887547,55.4194711303011,13.6028801618409));
#76087=CARTESIAN_POINT('Ctrl Pts',(87.2163541383964,55.4147249877156,13.5751181276687));
#76088=CARTESIAN_POINT('Ctrl Pts',(87.1600237527588,55.4099788451301,13.5440838215642));
#76089=CARTESIAN_POINT('Ctrl Pts',(87.1056576419326,55.4052327025445,13.5099979398493));
#76090=CARTESIAN_POINT('Ctrl Pts',(87.0531206482273,55.4006462412482,13.4770588583906));
#76091=CARTESIAN_POINT('Ctrl Pts',(87.0024182356365,55.3960597799518,13.4412706542136));
#76092=CARTESIAN_POINT('Ctrl Pts',(86.9538635313293,55.3914733186554,13.4028759561778));
#76093=CARTESIAN_POINT('Ctrl Pts',(86.9027731211883,55.3866473354253,13.362476145328));
#76094=CARTESIAN_POINT('Ctrl Pts',(86.8540613817271,55.3818213521952,13.3191905535037));
#76095=CARTESIAN_POINT('Ctrl Pts',(86.8080500485729,55.3769953689651,13.2733467811534));
#76096=CARTESIAN_POINT('Ctrl Pts',(86.7620387154187,55.3721693857351,13.2275030088032));
#76097=CARTESIAN_POINT('Ctrl Pts',(86.7187281630047,55.367343402505,13.1791015904119));
#76098=CARTESIAN_POINT('Ctrl Pts',(86.6783898054996,55.3625174192749,13.1285087788407));
#76099=CARTESIAN_POINT('Ctrl Pts',(86.6400443941757,55.357929867291,13.0804155422857));
#76100=CARTESIAN_POINT('Ctrl Pts',(86.6042233165221,55.3533423153071,13.0301403208289));
#76101=CARTESIAN_POINT('Ctrl Pts',(86.5711844148976,55.3487547633232,12.9779791206471));
#76102=CARTESIAN_POINT('Ctrl Pts',(86.5381952169409,55.3441741128448,12.9258963916868));
#76103=CARTESIAN_POINT('Ctrl Pts',(86.5079801689771,55.3395934623664,12.87193373564));
#76104=CARTESIAN_POINT('Ctrl Pts',(86.4807564203913,55.3350128118879,12.816419497792));
#76105=CARTESIAN_POINT('Ctrl Pts',(86.4522648267378,55.3302188346114,12.7583198903199));
#76106=CARTESIAN_POINT('Ctrl Pts',(86.4270503576331,55.325424857335,12.6985210776844));
#76107=CARTESIAN_POINT('Ctrl Pts',(86.4053099444063,55.3206308800585,12.6374317815517));
#76108=CARTESIAN_POINT('Ctrl Pts',(86.3845752197675,55.316058667115,12.5791684118324));
#76109=CARTESIAN_POINT('Ctrl Pts',(86.3670004043682,55.3114864541715,12.5197318589521));
#76110=CARTESIAN_POINT('Ctrl Pts',(86.3527074033412,55.3069142412281,12.4594977756818));
#76111=CARTESIAN_POINT('Ctrl Pts',(86.3384195452644,55.3023436734719,12.3992853660188));
#76112=CARTESIAN_POINT('Ctrl Pts',(86.3274112711726,55.2977731057157,12.3382764932761));
#76113=CARTESIAN_POINT('Ctrl Pts',(86.3197539981865,55.2932025379595,12.2768596617421));
#76114=CARTESIAN_POINT('Ctrl Pts',(86.3120950388772,55.2886309636499,12.2154293046841));
#76115=CARTESIAN_POINT('Ctrl Pts',(86.3077886127174,55.2840593893402,12.1535913168771));
#76116=CARTESIAN_POINT('Ctrl Pts',(86.3068543848883,55.2794878150306,12.0917402038738));
#76117=CARTESIAN_POINT('Ctrl Pts',(86.306717961678,55.2788202382105,12.0827082235222));
#76118=CARTESIAN_POINT('Ctrl Pts',(86.3066533569379,55.2781526613903,12.0736759654379));
#76119=CARTESIAN_POINT('Ctrl Pts',(86.3066605389041,55.2774850845702,12.0646446581799));
#76120=CARTESIAN_POINT('',(86.3066600222213,54.4837350846202,12.065724781343));
#76121=CARTESIAN_POINT('Ctrl Pts',(86.3066605389047,55.2774850845187,12.0646446574837));
#76122=CARTESIAN_POINT('Ctrl Pts',(86.3067183698751,55.272109593413,11.9919223723883));
#76123=CARTESIAN_POINT('Ctrl Pts',(86.3114346070278,55.2667341023073,11.9193961867115));
#76124=CARTESIAN_POINT('Ctrl Pts',(86.3207108495257,55.2613586112016,11.8476026021471));
#76125=CARTESIAN_POINT('Ctrl Pts',(86.3300933787503,55.2559215279853,11.7749864102502));
#76126=CARTESIAN_POINT('Ctrl Pts',(86.344140905695,55.2504844447691,11.7031198126283));
#76127=CARTESIAN_POINT('Ctrl Pts',(86.362702441516,55.2450473615528,11.6325372054077));
#76128=CARTESIAN_POINT('Ctrl Pts',(86.3724253770384,55.2421992992991,11.5955645030609));
#76129=CARTESIAN_POINT('Ctrl Pts',(86.3833861065539,55.2393512370455,11.5589437609058));
#76130=CARTESIAN_POINT('Ctrl Pts',(86.3955577594668,55.2365031747918,11.5227494103998));
#76131=CARTESIAN_POINT('Ctrl Pts',(86.4152047351794,55.2319059511997,11.4643259957317));
#76132=CARTESIAN_POINT('Ctrl Pts',(86.4380655035453,55.2273087276076,11.4068498436307));
#76133=CARTESIAN_POINT('Ctrl Pts',(86.464028998772,55.2227115040156,11.3506989745851));
#76134=CARTESIAN_POINT('Ctrl Pts',(86.4904370596955,55.2180355634444,11.2935866498493));
#76135=CARTESIAN_POINT('Ctrl Pts',(86.5200550228199,55.2133596228733,11.2378459531449));
#76136=CARTESIAN_POINT('Ctrl Pts',(86.5527130481342,55.2086836823022,11.1838582871114));
#76137=CARTESIAN_POINT('Ctrl Pts',(86.5847329753049,55.2040991039298,11.1309254744913));
#76138=CARTESIAN_POINT('Ctrl Pts',(86.6196749587524,55.1995145255574,11.0796782608688));
#76139=CARTESIAN_POINT('Ctrl Pts',(86.6573316063267,55.194929947185,11.0304534218251));
#76140=CARTESIAN_POINT('Ctrl Pts',(86.6949652388138,55.190348170827,10.9812586681456));
#76141=CARTESIAN_POINT('Ctrl Pts',(86.73530993691,55.185766394469,10.9340842416265));
#76142=CARTESIAN_POINT('Ctrl Pts',(86.7781155765936,55.1811846181111,10.8892371376858));
#76143=CARTESIAN_POINT('Ctrl Pts',(86.8209107765679,55.1766039591856,10.8444009713395));
#76144=CARTESIAN_POINT('Ctrl Pts',(86.8661653753469,55.1720233002602,10.8018913688645));
#76145=CARTESIAN_POINT('Ctrl Pts',(86.9135910081573,55.1674426413347,10.7619799310506));
#76146=CARTESIAN_POINT('Ctrl Pts',(86.9627299681169,55.1626964987492,10.7206266284493));
#76147=CARTESIAN_POINT('Ctrl Pts',(87.0141994260388,55.1579503561637,10.6820632338545));
#76148=CARTESIAN_POINT('Ctrl Pts',(87.0676414624996,55.1532042135781,10.6465460538203));
#76149=CARTESIAN_POINT('Ctrl Pts',(87.1192854718,55.1486177522818,10.6122238292667));
#76150=CARTESIAN_POINT('Ctrl Pts',(87.1727709347492,55.1440312909854,10.5807462903879));
#76151=CARTESIAN_POINT('Ctrl Pts',(87.2277478433918,55.139444829689,10.5522989414126));
#76152=CARTESIAN_POINT('Ctrl Pts',(87.2855958490775,55.1346188464589,10.5223659668984));
#76153=CARTESIAN_POINT('Ctrl Pts',(87.3450947661675,55.1297928632288,10.4957886290704));
#76154=CARTESIAN_POINT('Ctrl Pts',(87.4058136035802,55.1249668799987,10.4727253026586));
#76155=CARTESIAN_POINT('Ctrl Pts',(87.4665324409929,55.1201408967687,10.4496619762467));
#76156=CARTESIAN_POINT('Ctrl Pts',(87.5284705574999,55.1153149135386,10.4301127824971));
#76157=CARTESIAN_POINT('Ctrl Pts',(87.5911824483766,55.1104889303085,10.4141743254965));
#76158=CARTESIAN_POINT('Ctrl Pts',(87.6509216912412,55.1058917067164,10.3989913778875));
#76159=CARTESIAN_POINT('Ctrl Pts',(87.7116082759286,55.1012944831244,10.3870221995701));
#76160=CARTESIAN_POINT('Ctrl Pts',(87.7728643774751,55.0966972595323,10.378378519666));
#76161=CARTESIAN_POINT('Ctrl Pts',(87.835169350186,55.0920213189612,10.3695868364386));
#76162=CARTESIAN_POINT('Ctrl Pts',(87.8980630361323,55.08734537839,10.3642358293543));
#76163=CARTESIAN_POINT('Ctrl Pts',(87.9611328898701,55.0826694378189,10.3623896845442));
#76164=CARTESIAN_POINT('Ctrl Pts',(88.0229704352794,55.0780848594465,10.3605796111612));
#76165=CARTESIAN_POINT('Ctrl Pts',(88.0849767929952,55.0735002810741,10.3621386859302));
#76166=CARTESIAN_POINT('Ctrl Pts',(88.1467565414764,55.0689157027017,10.3670753409741));
#76167=CARTESIAN_POINT('Ctrl Pts',(88.2084985312513,55.0643339263437,10.3720089788203));
#76168=CARTESIAN_POINT('Ctrl Pts',(88.2700136800395,55.0597521499858,10.3803160632334));
#76169=CARTESIAN_POINT('Ctrl Pts',(88.3309084075311,55.0551703736278,10.3919529736621));
#76170=CARTESIAN_POINT('Ctrl Pts',(88.3917882836326,55.0505897147024,10.4035870460076));
#76171=CARTESIAN_POINT('Ctrl Pts',(88.4520475390398,55.0460090557769,10.4185492367228));
#76172=CARTESIAN_POINT('Ctrl Pts',(88.5113015874829,55.0414283968515,10.4367446003889));
#76173=CARTESIAN_POINT('Ctrl Pts',(88.572696283586,55.0366822542659,10.4555973007885));
#76174=CARTESIAN_POINT('Ctrl Pts',(88.6330111781199,55.0319361116804,10.4779211445169));
#76175=CARTESIAN_POINT('Ctrl Pts',(88.6918368074698,55.0271899690949,10.5035544562468));
#76176=CARTESIAN_POINT('Ctrl Pts',(88.7486832817145,55.0226035077985,10.5283253496679));
#76177=CARTESIAN_POINT('Ctrl Pts',(88.8041386774804,55.0180170465021,10.556186241276));
#76178=CARTESIAN_POINT('Ctrl Pts',(88.8578573048559,55.0134305852057,10.5869436992419));
#76179=CARTESIAN_POINT('Ctrl Pts',(88.9143813171833,55.0086046019757,10.6193074251627));
#76180=CARTESIAN_POINT('Ctrl Pts',(88.9689816403924,55.0037786187456,10.6548782098936));
#76181=CARTESIAN_POINT('Ctrl Pts',(89.02129145149,54.9989526355155,10.6933798709598));
#76182=CARTESIAN_POINT('Ctrl Pts',(89.0736012625875,54.9941266522855,10.731881532026));
#76183=CARTESIAN_POINT('Ctrl Pts',(89.1236201119107,54.9893006690554,10.7733135964818));
#76184=CARTESIAN_POINT('Ctrl Pts',(89.1710251991094,54.9844746858253,10.8173541843136));
#76185=CARTESIAN_POINT('Ctrl Pts',(89.2161832062687,54.9798774622332,10.8593071749762));
#76186=CARTESIAN_POINT('Ctrl Pts',(89.2591550948405,54.9752802386412,10.9037991920487));
#76187=CARTESIAN_POINT('Ctrl Pts',(89.2996420670314,54.9706830150491,10.9505734185178));
#76188=CARTESIAN_POINT('Ctrl Pts',(89.3408222863697,54.966007074478,10.9981485470381));
#76189=CARTESIAN_POINT('Ctrl Pts',(89.3794312381686,54.9613311339068,11.0480844844952));
#76190=CARTESIAN_POINT('Ctrl Pts',(89.415191234162,54.9566551933357,11.1000694572058));
#76191=CARTESIAN_POINT('Ctrl Pts',(89.4502525232727,54.9520706149633,11.1510387066979));
#76192=CARTESIAN_POINT('Ctrl Pts',(89.4825748832792,54.9474860365909,11.2039772007729));
#76193=CARTESIAN_POINT('Ctrl Pts',(89.5119367540217,54.9429014582185,11.2585573109956));
#76194=CARTESIAN_POINT('Ctrl Pts',(89.5412806793003,54.9383196818605,11.3131040628055));
#76195=CARTESIAN_POINT('Ctrl Pts',(89.5676674624285,54.9337379055025,11.3692899939451));
#76196=CARTESIAN_POINT('Ctrl Pts',(89.5909202724816,54.9291561291446,11.4267607895306));
#76197=CARTESIAN_POINT('Ctrl Pts',(89.6141674114928,54.9245754702191,11.4842175687761));
#76198=CARTESIAN_POINT('Ctrl Pts',(89.6342819039056,54.9199948112937,11.5429581187242));
#76199=CARTESIAN_POINT('Ctrl Pts',(89.651134916259,54.9154141523682,11.60260784203));
#76200=CARTESIAN_POINT('Ctrl Pts',(89.668596770749,54.9106680097827,11.6644125073856));
#76201=CARTESIAN_POINT('Ctrl Pts',(89.6825567612058,54.9059218671972,11.7271927524304));
#76202=CARTESIAN_POINT('Ctrl Pts',(89.6929286219364,54.9011757246117,11.7905168856154));
#76203=CARTESIAN_POINT('Ctrl Pts',(89.7029515272654,54.8965892633153,11.8517105140722));
#76204=CARTESIAN_POINT('Ctrl Pts',(89.7096239404532,54.8920028020189,11.913411479243));
#76205=CARTESIAN_POINT('Ctrl Pts',(89.7129208658942,54.8874163407225,11.9752244425295));
#76206=CARTESIAN_POINT('Ctrl Pts',(89.7163899689478,54.8825903574924,12.0402655068587));
#76207=CARTESIAN_POINT('Ctrl Pts',(89.7161213474005,54.8777643742623,12.1054299439649));
#76208=CARTESIAN_POINT('Ctrl Pts',(89.7121480636584,54.8729383910322,12.170259777053));
#76209=CARTESIAN_POINT('Ctrl Pts',(89.7081747799164,54.8681124078022,12.2350896101411));
#76210=CARTESIAN_POINT('Ctrl Pts',(89.7004969874147,54.8632864245721,12.2995842049145));
#76211=CARTESIAN_POINT('Ctrl Pts',(89.6892100178568,54.858460441342,12.3632977826439));
#76212=CARTESIAN_POINT('Ctrl Pts',(89.6784580694433,54.8538632177499,12.4239912307372));
#76213=CARTESIAN_POINT('Ctrl Pts',(89.6643872831714,54.8492659941579,12.4842252391071));
#76214=CARTESIAN_POINT('Ctrl Pts',(89.6470513488977,54.8446687705658,12.543609484171));
#76215=CARTESIAN_POINT('Ctrl Pts',(89.6294185762502,54.8399928299947,12.6040105491222));
#76216=CARTESIAN_POINT('Ctrl Pts',(89.6084077857015,54.8353168894235,12.6635319376246));
#76217=CARTESIAN_POINT('Ctrl Pts',(89.5841302871514,54.8306409488524,12.7217712522267));
#76218=CARTESIAN_POINT('Ctrl Pts',(89.5603271414321,54.82605637048,12.778872641367));
#76219=CARTESIAN_POINT('Ctrl Pts',(89.5333839998898,54.8214717921076,12.8347411140072));
#76220=CARTESIAN_POINT('Ctrl Pts',(89.5034559361524,54.8168872137352,12.8890128275083));
#76221=CARTESIAN_POINT('Ctrl Pts',(89.4735461639264,54.8123054373772,12.9432513710835));
#76222=CARTESIAN_POINT('Ctrl Pts',(89.440655332198,54.8077236610193,12.9958946457735));
#76223=CARTESIAN_POINT('Ctrl Pts',(89.4049851955275,54.8031418846613,13.0466019122202));
#76224=CARTESIAN_POINT('Ctrl Pts',(89.3693237583149,54.7985612257359,13.0972968118591));
#76225=CARTESIAN_POINT('Ctrl Pts',(89.3308846545162,54.7939805668104,13.1460562244108));
#76226=CARTESIAN_POINT('Ctrl Pts',(89.2899127121818,54.789399907885,13.1925687330206));
#76227=CARTESIAN_POINT('Ctrl Pts',(89.2474605926311,54.7846537652995,13.2407615807016));
#76228=CARTESIAN_POINT('Ctrl Pts',(89.2022894612093,54.779907622714,13.2865415914872));
#76229=CARTESIAN_POINT('Ctrl Pts',(89.1547152007213,54.7751614801285,13.3296021427803));
#76230=CARTESIAN_POINT('Ctrl Pts',(89.108741549382,54.7705750188321,13.3712139461235));
#76231=CARTESIAN_POINT('Ctrl Pts',(89.0605243709355,54.7659885575357,13.410286108892));
#76232=CARTESIAN_POINT('Ctrl Pts',(89.0103822401222,54.7614020962393,13.4465832005817));
#76233=CARTESIAN_POINT('Ctrl Pts',(88.9576215022053,54.7565761130092,13.4847758603415));
#76234=CARTESIAN_POINT('Ctrl Pts',(88.9027297790061,54.7517501297791,13.5198952957746));
#76235=CARTESIAN_POINT('Ctrl Pts',(88.8461097595345,54.7469241465491,13.5517208772613));
#76236=CARTESIAN_POINT('Ctrl Pts',(88.7894897400629,54.742098163319,13.583546458748));
#76237=CARTESIAN_POINT('Ctrl Pts',(88.7311420404278,54.7372721800889,13.6120779711507));
#76238=CARTESIAN_POINT('Ctrl Pts',(88.6714928765752,54.7324461968588,13.6371537148202));
#76239=CARTESIAN_POINT('Ctrl Pts',(88.6146711823758,54.7278489732668,13.661040826501));
#76240=CARTESIAN_POINT('Ctrl Pts',(88.5564353396656,54.7232517496747,13.6818905126966));
#76241=CARTESIAN_POINT('Ctrl Pts',(88.4971423888616,54.7186545260826,13.6995361683636));
#76242=CARTESIAN_POINT('Ctrl Pts',(88.4368341813766,54.7139785855115,13.7174839656775));
#76243=CARTESIAN_POINT('Ctrl Pts',(88.3754327759686,54.7093026449404,13.7321166832191));
#76244=CARTESIAN_POINT('Ctrl Pts',(88.3133366096077,54.7046267043692,13.7433095749118));
#76245=CARTESIAN_POINT('Ctrl Pts',(88.2524537269068,54.7000421259968,13.7542837710974));
#76246=CARTESIAN_POINT('Ctrl Pts',(88.1909035136092,54.6954575476244,13.7619512579306));
#76247=CARTESIAN_POINT('Ctrl Pts',(88.1290757533627,54.690872969252,13.7662449682525));
#76248=CARTESIAN_POINT('Ctrl Pts',(88.0672857811664,54.686291192894,13.7705360543333));
#76249=CARTESIAN_POINT('Ctrl Pts',(88.0052191051471,54.6817094165361,13.7714574173445));
#76250=CARTESIAN_POINT('Ctrl Pts',(87.9432714190773,54.6771276401781,13.7689937389568));
#76251=CARTESIAN_POINT('Ctrl Pts',(87.8813388411998,54.6725469812527,13.7665306614266));
#76252=CARTESIAN_POINT('Ctrl Pts',(87.8195257040799,54.6679663223272,13.7606842015897));
#76253=CARTESIAN_POINT('Ctrl Pts',(87.7582264300416,54.6633856634017,13.7514911325577));
#76254=CARTESIAN_POINT('Ctrl Pts',(87.6947126212843,54.6586395208162,13.7419659491431));
#76255=CARTESIAN_POINT('Ctrl Pts',(87.6317510992091,54.6538933782307,13.7288477465443));
#76256=CARTESIAN_POINT('Ctrl Pts',(87.569770798394,54.6491472356452,13.7122355928755));
#76257=CARTESIAN_POINT('Ctrl Pts',(87.5098757898254,54.6445607743488,13.6961823457429));
#76258=CARTESIAN_POINT('Ctrl Pts',(87.4508975007422,54.6399743130524,13.6768667660837));
#76259=CARTESIAN_POINT('Ctrl Pts',(87.3932065158404,54.635387851756,13.6544287980674));
#76260=CARTESIAN_POINT('Ctrl Pts',(87.3325026948182,54.630561868526,13.6308190365617));
#76261=CARTESIAN_POINT('Ctrl Pts',(87.2732249108346,54.6257358852959,13.6037520761322));
#76262=CARTESIAN_POINT('Ctrl Pts',(87.2157769375249,54.6209099020658,13.5734465551083));
#76263=CARTESIAN_POINT('Ctrl Pts',(87.1583289642153,54.6160839188357,13.5431410340843));
#76264=CARTESIAN_POINT('Ctrl Pts',(87.102711316498,54.6112579356057,13.5095973533818));
#76265=CARTESIAN_POINT('Ctrl Pts',(87.0492910206734,54.6064319523756,13.4730858803508));
#76266=CARTESIAN_POINT('Ctrl Pts',(86.9986250991325,54.6018547989938,13.4384569551571));
#76267=CARTESIAN_POINT('Ctrl Pts',(86.9497234381032,54.5972776456119,13.4010137474302));
#76268=CARTESIAN_POINT('Ctrl Pts',(86.9029180125317,54.5927004922301,13.3609629896828));
#76269=CARTESIAN_POINT('Ctrl Pts',(86.8561945285598,54.5881313520062,13.3209823482332));
#76270=CARTESIAN_POINT('Ctrl Pts',(86.8115603826973,54.5835622117823,13.2784035495247));
#76271=CARTESIAN_POINT('Ctrl Pts',(86.7693177776882,54.5789930715585,13.2334759502425));
#76272=CARTESIAN_POINT('Ctrl Pts',(86.7271165208912,54.5744284037335,13.1885923273181));
#76273=CARTESIAN_POINT('Ctrl Pts',(86.6873025169719,54.5698637359085,13.1413648317498));
#76274=CARTESIAN_POINT('Ctrl Pts',(86.6501428681452,54.5652990680836,13.0920812357118));
#76275=CARTESIAN_POINT('Ctrl Pts',(86.6130056287687,54.5607371530213,13.0428273605761));
#76276=CARTESIAN_POINT('Ctrl Pts',(86.5785198800985,54.5561752379591,12.9915202526092));
#76277=CARTESIAN_POINT('Ctrl Pts',(86.546912586667,54.5516133228969,12.9384808775668));
#76278=CARTESIAN_POINT('Ctrl Pts',(86.5153124778442,54.547052444797,12.8854535588291));
#76279=CARTESIAN_POINT('Ctrl Pts',(86.4865897883838,54.5424915666972,12.8306951961169));
#76280=CARTESIAN_POINT('Ctrl Pts',(86.4609271044993,54.5379306885974,12.7745540587944));
#76281=CARTESIAN_POINT('Ctrl Pts',(86.4352419934899,54.5333658246563,12.7183638586263));
#76282=CARTESIAN_POINT('Ctrl Pts',(86.4126224475418,54.5288009607153,12.6607889370642));
#76283=CARTESIAN_POINT('Ctrl Pts',(86.3932035947369,54.5242360967743,12.6021992416235));
#76284=CARTESIAN_POINT('Ctrl Pts',(86.3737769978184,54.5196694123949,12.5435861809895));
#76285=CARTESIAN_POINT('Ctrl Pts',(86.3575537741795,54.5151027280155,12.4839580367219));
#76286=CARTESIAN_POINT('Ctrl Pts',(86.3446187416312,54.5105360436361,12.4236986683751));
#76287=CARTESIAN_POINT('Ctrl Pts',(86.331659116281,54.5059606768229,12.3633247315716));
#76288=CARTESIAN_POINT('Ctrl Pts',(86.3220002556448,54.5013853100096,12.3023176819412));
#76289=CARTESIAN_POINT('Ctrl Pts',(86.3156753947611,54.4968099431963,12.2410694675598));
#76290=CARTESIAN_POINT('Ctrl Pts',(86.3096506201407,54.4924516570043,12.1827272060709));
#76291=CARTESIAN_POINT('Ctrl Pts',(86.3066505849826,54.4880933708122,12.1241665433601));
#76292=CARTESIAN_POINT('Ctrl Pts',(86.3066600222213,54.4837350846202,12.065724781343));
#76293=CARTESIAN_POINT('',(86.3066606861718,53.6899850846232,12.0675293592027));
#76294=CARTESIAN_POINT('Ctrl Pts',(86.3066600222214,54.4837350845702,12.065724780673));
#76295=CARTESIAN_POINT('Ctrl Pts',(86.3066624166605,54.4826292923442,12.0508968315069));
#76296=CARTESIAN_POINT('Ctrl Pts',(86.3068583141327,54.4815235001183,12.0360706484629));
#76297=CARTESIAN_POINT('Ctrl Pts',(86.3072476018017,54.4804177078924,12.0212495672259));
#76298=CARTESIAN_POINT('Ctrl Pts',(86.3088660274098,54.4758204843003,11.9596323639894));
#76299=CARTESIAN_POINT('Ctrl Pts',(86.3138347189205,54.4712232607082,11.8979765865206));
#76300=CARTESIAN_POINT('Ctrl Pts',(86.3221585533405,54.4666260371161,11.8366762034915));
#76301=CARTESIAN_POINT('Ctrl Pts',(86.3306249144588,54.461950096545,11.7743261910786));
#76302=CARTESIAN_POINT('Ctrl Pts',(86.3425624793092,54.4572741559739,11.7123443908936));
#76303=CARTESIAN_POINT('Ctrl Pts',(86.3579209371358,54.4525982154028,11.6511452693774));
#76304=CARTESIAN_POINT('Ctrl Pts',(86.3729793093529,54.4480136370303,11.5911419043546));
#76305=CARTESIAN_POINT('Ctrl Pts',(86.3913259667826,54.4434290586579,11.5318914252639));
#76306=CARTESIAN_POINT('Ctrl Pts',(86.4128615941009,54.4388444802855,11.473776671187));
#76307=CARTESIAN_POINT('Ctrl Pts',(86.434384059219,54.4342627039276,11.4156974358355));
#76308=CARTESIAN_POINT('Ctrl Pts',(86.4590914530389,54.4296809275696,11.3587530254644));
#76309=CARTESIAN_POINT('Ctrl Pts',(86.4868348657027,54.4250991512116,11.3033103652255));
#76310=CARTESIAN_POINT('Ctrl Pts',(86.514571512128,54.4205184922862,11.2478812266922));
#76311=CARTESIAN_POINT('Ctrl Pts',(86.5453424798089,54.4159378333607,11.1939535662459));
#76312=CARTESIAN_POINT('Ctrl Pts',(86.578951908098,54.4113571744353,11.1418717090793));
#76313=CARTESIAN_POINT('Ctrl Pts',(86.6137755309597,54.4066110318498,11.0879083111809));
#76314=CARTESIAN_POINT('Ctrl Pts',(86.651646367545,54.4018648892642,11.035927158464));
#76315=CARTESIAN_POINT('Ctrl Pts',(86.6922975784569,54.3971187466787,10.9862783881868));
#76316=CARTESIAN_POINT('Ctrl Pts',(86.7315811023166,54.3925322853823,10.9383000227696));
#76317=CARTESIAN_POINT('Ctrl Pts',(86.7734604617028,54.3879458240859,10.8924999195148));
#76318=CARTESIAN_POINT('Ctrl Pts',(86.8176555815901,54.3833593627895,10.8491582129751));
#76319=CARTESIAN_POINT('Ctrl Pts',(86.864158733725,54.3785333795595,10.803553042582));
#76320=CARTESIAN_POINT('Ctrl Pts',(86.9132256763394,54.3737073963294,10.7606705150984));
#76321=CARTESIAN_POINT('Ctrl Pts',(86.9644909547854,54.3688814130993,10.7207886211141));
#76322=CARTESIAN_POINT('Ctrl Pts',(87.0157562332315,54.3640554298693,10.6809067271298));
#76323=CARTESIAN_POINT('Ctrl Pts',(87.0692192701858,54.3592294466392,10.6440257709017));
#76324=CARTESIAN_POINT('Ctrl Pts',(87.1244825926361,54.3544034634091,10.610368960883));
#76325=CARTESIAN_POINT('Ctrl Pts',(87.177126341616,54.349806239817,10.5783075396812));
#76326=CARTESIAN_POINT('Ctrl Pts',(87.2316196777066,54.345209016225,10.5490398251764));
#76327=CARTESIAN_POINT('Ctrl Pts',(87.2876342647683,54.3406117926329,10.5227836027657));
#76328=CARTESIAN_POINT('Ctrl Pts',(87.3446079740018,54.3359358520618,10.4960778023722));
#76329=CARTESIAN_POINT('Ctrl Pts',(87.4031551169578,54.3312599114906,10.4724879515797));
#76330=CARTESIAN_POINT('Ctrl Pts',(87.462900203113,54.3265839709195,10.4521965893417));
#76331=CARTESIAN_POINT('Ctrl Pts',(87.5214779428595,54.3219993925471,10.432301695673));
#76332=CARTESIAN_POINT('Ctrl Pts',(87.5812067290269,54.3174148141747,10.4155777244258));
#76333=CARTESIAN_POINT('Ctrl Pts',(87.6417110618891,54.3128302358023,10.402148890138));
#76334=CARTESIAN_POINT('Ctrl Pts',(87.7021784155568,54.3082484594443,10.3887282633199));
#76335=CARTESIAN_POINT('Ctrl Pts',(87.7634198801215,54.3036666830864,10.3785988901978));
#76336=CARTESIAN_POINT('Ctrl Pts',(87.8250464254723,54.2990849067284,10.3718346881959));
#76337=CARTESIAN_POINT('Ctrl Pts',(87.8866579409526,54.294504247803,10.3650721358901));
#76338=CARTESIAN_POINT('Ctrl Pts',(87.9486538450002,54.2899235888775,10.3616731809678));
#76339=CARTESIAN_POINT('Ctrl Pts',(88.0106386281579,54.2853429299521,10.3616600383109));
#76340=CARTESIAN_POINT('Ctrl Pts',(88.0748627111526,54.2805967873665,10.3616464208545));
#76341=CARTESIAN_POINT('Ctrl Pts',(88.1390742729589,54.275850644781,10.3652679994941));
#76342=CARTESIAN_POINT('Ctrl Pts',(88.2028344224945,54.2711045021955,10.372490510819));
#76343=CARTESIAN_POINT('Ctrl Pts',(88.2644493977779,54.2665180408991,10.3794700248258));
#76344=CARTESIAN_POINT('Ctrl Pts',(88.3256423468815,54.2619315796027,10.3898118419173));
#76345=CARTESIAN_POINT('Ctrl Pts',(88.3860260104896,54.2573451183063,10.40343260977));
#76346=CARTESIAN_POINT('Ctrl Pts',(88.4495631318367,54.2525191350763,10.4177647043827));
#76347=CARTESIAN_POINT('Ctrl Pts',(88.5122035000195,54.2476931518462,10.4357274518014));
#76348=CARTESIAN_POINT('Ctrl Pts',(88.5735153471093,54.2428671686161,10.4571646075914));
#76349=CARTESIAN_POINT('Ctrl Pts',(88.634827194199,54.2380411853861,10.4786017633815));
#76350=CARTESIAN_POINT('Ctrl Pts',(88.6948099514436,54.233215202156,10.50351300755));
#76351=CARTESIAN_POINT('Ctrl Pts',(88.7530605078257,54.2283892189259,10.5316854825931));
#76352=CARTESIAN_POINT('Ctrl Pts',(88.8085498908767,54.2237919953339,10.5585225354259));
#76353=CARTESIAN_POINT('Ctrl Pts',(88.8626954355473,54.2191947717418,10.5884287686047));
#76354=CARTESIAN_POINT('Ctrl Pts',(88.9151360865985,54.2145975481497,10.6212464665174));
#76355=CARTESIAN_POINT('Ctrl Pts',(88.9684746643107,54.2099216075786,10.6546260927303));
#76356=CARTESIAN_POINT('Ctrl Pts',(89.0200488953005,54.2052456670075,10.691017681134));
#76357=CARTESIAN_POINT('Ctrl Pts',(89.0695017591331,54.2005697264363,10.7302047830928));
#76358=CARTESIAN_POINT('Ctrl Pts',(89.1179883740787,54.1959851480639,10.7686262166814));
#76359=CARTESIAN_POINT('Ctrl Pts',(89.1644353561218,54.1914005696915,10.809734573136));
#76360=CARTESIAN_POINT('Ctrl Pts',(89.208534679412,54.1868159913191,10.853281760999));
#76361=CARTESIAN_POINT('Ctrl Pts',(89.2526070499638,54.1822342149611,10.8968023335792));
#76362=CARTESIAN_POINT('Ctrl Pts',(89.2943342453998,54.1776524386032,10.9427584250462));
#76363=CARTESIAN_POINT('Ctrl Pts',(89.3334431566761,54.1730706622452,10.9908632956872));
#76364=CARTESIAN_POINT('Ctrl Pts',(89.3725425298244,54.1684900033198,11.038956434209));
#76365=CARTESIAN_POINT('Ctrl Pts',(89.4090245654839,54.1639093443943,11.0891969167641));
#76366=CARTESIAN_POINT('Ctrl Pts',(89.4426560766216,54.1593286854689,11.141264516809));
#76367=CARTESIAN_POINT('Ctrl Pts',(89.4775025801101,54.1545825428834,11.1952131425243));
#76368=CARTESIAN_POINT('Ctrl Pts',(89.5092882869207,54.1498364002978,11.2511229747902));
#76369=CARTESIAN_POINT('Ctrl Pts',(89.5378039284902,54.1450902577123,11.308606707485));
#76370=CARTESIAN_POINT('Ctrl Pts',(89.5653601773901,54.1405037964159,11.3641564324304));
#76371=CARTESIAN_POINT('Ctrl Pts',(89.5898627778076,54.1359173351195,11.4211753132817));
#76372=CARTESIAN_POINT('Ctrl Pts',(89.6111717068205,54.1313308738231,11.4792927950918));
#76373=CARTESIAN_POINT('Ctrl Pts',(89.6335934667398,54.1265048905931,11.5404453862649));
#76374=CARTESIAN_POINT('Ctrl Pts',(89.6524786405656,54.121678907363,11.6028138577107));
#76375=CARTESIAN_POINT('Ctrl Pts',(89.6677243021645,54.1168529241329,11.6659507252631));
#76376=CARTESIAN_POINT('Ctrl Pts',(89.6829699637634,54.1120269409029,11.7290875928155));
#76377=CARTESIAN_POINT('Ctrl Pts',(89.6945760734779,54.1072009576728,11.7929922050902));
#76378=CARTESIAN_POINT('Ctrl Pts',(89.7025028104862,54.1023749744427,11.8572104463405));
#76379=CARTESIAN_POINT('Ctrl Pts',(89.7100538069661,54.0977777508506,11.9183846360638));
#76380=CARTESIAN_POINT('Ctrl Pts',(89.7142974237847,54.0931805272586,11.9800945583366));
#76381=CARTESIAN_POINT('Ctrl Pts',(89.7151703252516,54.0885833036665,12.041951338256));
#76382=CARTESIAN_POINT('Ctrl Pts',(89.7160581731673,54.0839073630954,12.1048672745882));
#76383=CARTESIAN_POINT('Ctrl Pts',(89.7134586284006,54.0792314225243,12.1679346304526));
#76384=CARTESIAN_POINT('Ctrl Pts',(89.7073598865906,54.0745554819531,12.2307360639514));
#76385=CARTESIAN_POINT('Ctrl Pts',(89.7013803067872,54.0699709035807,12.2923104337271));
#76386=CARTESIAN_POINT('Ctrl Pts',(89.692037091836,54.0653863252083,12.3536286483593));
#76387=CARTESIAN_POINT('Ctrl Pts',(89.6793715957827,54.0608017468359,12.4142973643104));
#76388=CARTESIAN_POINT('Ctrl Pts',(89.66671384066,54.0562199704779,12.4749290005989));
#76389=CARTESIAN_POINT('Ctrl Pts',(89.6507379344762,54.05163819412,12.5349114280546));
#76390=CARTESIAN_POINT('Ctrl Pts',(89.6315366393272,54.047056417762,12.5938596747223));
#76391=CARTESIAN_POINT('Ctrl Pts',(89.6123400271112,54.0424757588366,12.65279354472));
#76392=CARTESIAN_POINT('Ctrl Pts',(89.589919745095,54.0378950999111,12.7106932508293));
#76393=CARTESIAN_POINT('Ctrl Pts',(89.5644183420192,54.0333144409857,12.767189197206));
#76394=CARTESIAN_POINT('Ctrl Pts',(89.5379956598028,54.0285682984001,12.8257261503761));
#76395=CARTESIAN_POINT('Ctrl Pts',(89.5082651541107,54.0238221558146,12.8827554194644));
#76396=CARTESIAN_POINT('Ctrl Pts',(89.4754387020055,54.0190760132291,12.9378911191591));
#76397=CARTESIAN_POINT('Ctrl Pts',(89.4437166773578,54.0144895519327,12.9911718093498));
#76398=CARTESIAN_POINT('Ctrl Pts',(89.4091040885707,54.0099030906363,13.042683933148));
#76399=CARTESIAN_POINT('Ctrl Pts',(89.3718362984402,54.0053166293399,13.0921088657875));
#76400=CARTESIAN_POINT('Ctrl Pts',(89.3326222467849,54.0004906461099,13.1441149507953));
#76401=CARTESIAN_POINT('Ctrl Pts',(89.2904684684486,53.9956646628798,13.193809366909));
#76402=CARTESIAN_POINT('Ctrl Pts',(89.2456950773454,53.9908386796497,13.240862928847));
#76403=CARTESIAN_POINT('Ctrl Pts',(89.2009216862423,53.9860126964196,13.2879164907849));
#76404=CARTESIAN_POINT('Ctrl Pts',(89.1535292081039,53.9811867131896,13.3323288119198));
#76405=CARTESIAN_POINT('Ctrl Pts',(89.1038775564186,53.9763607299595,13.3738201261169));
#76406=CARTESIAN_POINT('Ctrl Pts',(89.0565794756688,53.9717635063674,13.4133446829584));
#76407=CARTESIAN_POINT('Ctrl Pts',(89.0070373960248,53.9671662827753,13.4503812207983));
#76408=CARTESIAN_POINT('Ctrl Pts',(88.9555436663255,53.9625690591833,13.4846656047161));
#76409=CARTESIAN_POINT('Ctrl Pts',(88.9031682238357,53.9578931186121,13.51953703059));
#76410=CARTESIAN_POINT('Ctrl Pts',(88.848774013114,53.953217178041,13.5515607538071));
#76411=CARTESIAN_POINT('Ctrl Pts',(88.7927052492535,53.9485412374699,13.5805004915448));
#76412=CARTESIAN_POINT('Ctrl Pts',(88.7377320009299,53.9439566590975,13.6088747819613));
#76413=CARTESIAN_POINT('Ctrl Pts',(88.6811495224217,53.9393720807251,13.634284273046));
#76414=CARTESIAN_POINT('Ctrl Pts',(88.6233107003458,53.9347875023526,13.6565503581597));
#76415=CARTESIAN_POINT('Ctrl Pts',(88.5655072283506,53.9302057259947,13.67880283463));
#76416=CARTESIAN_POINT('Ctrl Pts',(88.5064494094089,53.9256239496367,13.6979155320779));
#76417=CARTESIAN_POINT('Ctrl Pts',(88.4465109806567,53.9210421732788,13.7137575735913));
#76418=CARTESIAN_POINT('Ctrl Pts',(88.3865871700665,53.9164615143533,13.7295957514477));
#76419=CARTESIAN_POINT('Ctrl Pts',(88.3257836679409,53.9118808554279,13.7421647268433));
#76420=CARTESIAN_POINT('Ctrl Pts',(88.2644882978339,53.9073001965024,13.7513837896637));
#76421=CARTESIAN_POINT('Ctrl Pts',(88.2009785340436,53.9025540539169,13.7609359059341));
#76422=CARTESIAN_POINT('Ctrl Pts',(88.1369412482078,53.8978079113314,13.7668912836917));
#76423=CARTESIAN_POINT('Ctrl Pts',(88.0728155526031,53.8930617687459,13.7692186216268));
#76424=CARTESIAN_POINT('Ctrl Pts',(88.0108473298419,53.8884753074495,13.7714676575904));
#76425=CARTESIAN_POINT('Ctrl Pts',(87.9487970787355,53.8838888461531,13.7703290012007));
#76426=CARTESIAN_POINT('Ctrl Pts',(87.8870601431849,53.8793023848567,13.7658275640466));
#76427=CARTESIAN_POINT('Ctrl Pts',(87.8220990770406,53.8744764016266,13.7610910452333));
#76428=CARTESIAN_POINT('Ctrl Pts',(87.7574855887589,53.8696504183965,13.7526309534498));
#76429=CARTESIAN_POINT('Ctrl Pts',(87.6936698632552,53.8648244351664,13.7405376734829));
#76430=CARTESIAN_POINT('Ctrl Pts',(87.6298541377515,53.8599984519364,13.728444393516));
#76431=CARTESIAN_POINT('Ctrl Pts',(87.5668367849956,53.8551724687063,13.7127181573378));
#76432=CARTESIAN_POINT('Ctrl Pts',(87.5050480590712,53.8503464854762,13.693509591084));
#76433=CARTESIAN_POINT('Ctrl Pts',(87.4461882216034,53.8457492618841,13.6752115428435));
#76434=CARTESIAN_POINT('Ctrl Pts',(87.3882014793481,53.8411520382921,13.6536787651955));
#76435=CARTESIAN_POINT('Ctrl Pts',(87.3314683072925,53.8365548147,13.6290136001347));
#76436=CARTESIAN_POINT('Ctrl Pts',(87.2737637089344,53.8318788741288,13.6039261003229));
#76437=CARTESIAN_POINT('Ctrl Pts',(87.2173565484748,53.8272029335577,13.5755980001816));
#76438=CARTESIAN_POINT('Ctrl Pts',(87.1626320339562,53.8225269929866,13.5441903225873));
#76439=CARTESIAN_POINT('Ctrl Pts',(87.1089767699752,53.8179424146142,13.5133963128609));
#76440=CARTESIAN_POINT('Ctrl Pts',(87.0569394522188,53.8133578362418,13.4796422512973));
#76441=CARTESIAN_POINT('Ctrl Pts',(87.0068615371703,53.8087732578693,13.443127729394));
#76442=CARTESIAN_POINT('Ctrl Pts',(86.9568142288713,53.8041914815114,13.4066355245306));
#76443=CARTESIAN_POINT('Ctrl Pts',(86.9087243591689,53.7996097051534,13.3673865039837));
#76444=CARTESIAN_POINT('Ctrl Pts',(86.8629045950878,53.7950279287955,13.3256236647585));
#76445=CARTESIAN_POINT('Ctrl Pts',(86.8170960058197,53.79044726987,13.2838710109178));
#76446=CARTESIAN_POINT('Ctrl Pts',(86.7735567991505,53.7858666109446,13.2396060982234));
#76447=CARTESIAN_POINT('Ctrl Pts',(86.7325651363716,53.7812859520191,13.1931109683875));
#76448=CARTESIAN_POINT('Ctrl Pts',(86.6900925839436,53.7765398094336,13.1449361273167));
#76449=CARTESIAN_POINT('Ctrl Pts',(86.6503556003815,53.7717936668481,13.0943672372871));
#76450=CARTESIAN_POINT('Ctrl Pts',(86.613618656534,53.7670475242626,13.0417562280268));
#76451=CARTESIAN_POINT('Ctrl Pts',(86.5781177064321,53.7624610629662,12.9909152864855));
#76452=CARTESIAN_POINT('Ctrl Pts',(86.5454183363236,53.7578746016698,12.9381679510526));
#76453=CARTESIAN_POINT('Ctrl Pts',(86.5157140514985,53.7532881403734,12.8838598705243));
#76454=CARTESIAN_POINT('Ctrl Pts',(86.4844584993063,53.7484621571433,12.8267156216255));
#76455=CARTESIAN_POINT('Ctrl Pts',(86.4565197254006,53.7436361739133,12.7678437188743));
#76456=CARTESIAN_POINT('Ctrl Pts',(86.4320659753496,53.7388101906832,12.7076713967456));
#76457=CARTESIAN_POINT('Ctrl Pts',(86.4076122252987,53.7339842074531,12.6474990746169));
#76458=CARTESIAN_POINT('Ctrl Pts',(86.3866436350648,53.7291582242231,12.5860269713807));
#76459=CARTESIAN_POINT('Ctrl Pts',(86.3692670297251,53.724332240993,12.5236982520312));
#76460=CARTESIAN_POINT('Ctrl Pts',(86.3485464875666,53.7185775503028,12.4493750553121));
#76461=CARTESIAN_POINT('Ctrl Pts',(86.3328622147382,53.7128228596126,12.3735907719497));
#76462=CARTESIAN_POINT('Ctrl Pts',(86.3223801757244,53.7070681689225,12.2969500479836));
#76463=CARTESIAN_POINT('Ctrl Pts',(86.3120080250888,53.7013738074894,12.2211127864775));
#76464=CARTESIAN_POINT('Ctrl Pts',(86.3067296976861,53.6956794460563,12.1444367572088));
#76465=CARTESIAN_POINT('Ctrl Pts',(86.3066606861718,53.6899850846232,12.0675293592027));
#76466=CARTESIAN_POINT('',(86.3066601233575,52.8962350845279,12.0653515508395));
#76467=CARTESIAN_POINT('Ctrl Pts',(86.3066606861711,53.6899850845702,12.0675293584867));
#76468=CARTESIAN_POINT('Ctrl Pts',(86.3066056477354,53.6854436845471,12.0061937261784));
#76469=CARTESIAN_POINT('Ctrl Pts',(86.3098658996797,53.6809022845239,11.9447845824161));
#76470=CARTESIAN_POINT('Ctrl Pts',(86.3164385719836,53.6763608845008,11.8836914640537));
#76471=CARTESIAN_POINT('Ctrl Pts',(86.3230076991165,53.6718219340199,11.822631298124));
#76472=CARTESIAN_POINT('Ctrl Pts',(86.3328856501294,53.6672829835391,11.7618873353594));
#76473=CARTESIAN_POINT('Ctrl Pts',(86.3460175785588,53.6627440330583,11.7018456757199));
#76474=CARTESIAN_POINT('Ctrl Pts',(86.3591474682364,53.6582057872564,11.6418133376396));
#76475=CARTESIAN_POINT('Ctrl Pts',(86.3755302206782,53.6536675414546,11.58248359339));
#76476=CARTESIAN_POINT('Ctrl Pts',(86.395059996133,53.6491292956528,11.5242318397116));
#76477=CARTESIAN_POINT('Ctrl Pts',(86.4146081007246,53.6445867906044,11.4659254154424));
#76478=CARTESIAN_POINT('Ctrl Pts',(86.4373089614595,53.640044285556,11.4086994959161));
#76479=CARTESIAN_POINT('Ctrl Pts',(86.463007420663,53.6355017805077,11.352912480885));
#76480=CARTESIAN_POINT('Ctrl Pts',(86.4887181511995,53.6309571063568,11.2970988268621));
#76481=CARTESIAN_POINT('Ctrl Pts',(86.5174290864942,53.626412432206,11.2427259048733));
#76482=CARTESIAN_POINT('Ctrl Pts',(86.548939071428,53.6218677580551,11.1901274768877));
#76483=CARTESIAN_POINT('Ctrl Pts',(86.5805074415662,53.6173146630266,11.1374315886849));
#76484=CARTESIAN_POINT('Ctrl Pts',(86.6148849254102,53.612761567998,11.0865171903036));
#76485=CARTESIAN_POINT('Ctrl Pts',(86.6518276286619,53.6082084729694,11.0376881306766));
#76486=CARTESIAN_POINT('Ctrl Pts',(86.6785772670636,53.6049116474829,11.0023317659945));
#76487=CARTESIAN_POINT('Ctrl Pts',(86.7066709528863,53.6016148219963,10.9680680892726));
#76488=CARTESIAN_POINT('Ctrl Pts',(86.7360040762212,53.5983179965098,10.93500034043));
#76489=CARTESIAN_POINT('Ctrl Pts',(86.7769073412483,53.5937207729177,10.8888893661803));
#76490=CARTESIAN_POINT('Ctrl Pts',(86.8203992414488,53.5891235493257,10.8449055349744));
#76491=CARTESIAN_POINT('Ctrl Pts',(86.8662299000522,53.5845263257336,10.8033534723188));
#76492=CARTESIAN_POINT('Ctrl Pts',(86.9128453042571,53.5798503851625,10.7610899252683));
#76493=CARTESIAN_POINT('Ctrl Pts',(86.9618800316775,53.5751744445913,10.7213426673058));
#76494=CARTESIAN_POINT('Ctrl Pts',(87.0130287778948,53.5704985040202,10.6843964839905));
#76495=CARTESIAN_POINT('Ctrl Pts',(87.0631781397433,53.5659139256478,10.6481721842172));
#76496=CARTESIAN_POINT('Ctrl Pts',(87.1153592202268,53.5613293472754,10.6146407966693));
#76497=CARTESIAN_POINT('Ctrl Pts',(87.1692495734302,53.556744768903,10.5840313583043));
#76498=CARTESIAN_POINT('Ctrl Pts',(87.2231069897883,53.552162992545,10.5534406278948));
#76499=CARTESIAN_POINT('Ctrl Pts',(87.2786711657099,53.5475812161871,10.5257685564865));
#76500=CARTESIAN_POINT('Ctrl Pts',(87.3355919471247,53.5429994398291,10.5012000774185));
#76501=CARTESIAN_POINT('Ctrl Pts',(87.3924988463404,53.5384187809037,10.4766375902661));
#76502=CARTESIAN_POINT('Ctrl Pts',(87.4507612270868,53.5338381219783,10.4551773944843));
#76503=CARTESIAN_POINT('Ctrl Pts',(87.5100075542628,53.5292574630528,10.436956905139));
#76504=CARTESIAN_POINT('Ctrl Pts',(87.5713942501557,53.5245113204673,10.4180781713547));
#76505=CARTESIAN_POINT('Ctrl Pts',(87.6338368100407,53.5197651778818,10.4026779370554));
#76506=CARTESIAN_POINT('Ctrl Pts',(87.6969056406633,53.5150190352963,10.3908523739584));
#76507=CARTESIAN_POINT('Ctrl Pts',(87.7578525560681,53.5104325739999,10.3794246752589));
#76508=CARTESIAN_POINT('Ctrl Pts',(87.8193837348227,53.5058461127035,10.3713349137168));
#76509=CARTESIAN_POINT('Ctrl Pts',(87.881104517804,53.5012596514071,10.3666171710574));
#76510=CARTESIAN_POINT('Ctrl Pts',(87.9460485878324,53.496433668177,10.361653050467));
#76511=CARTESIAN_POINT('Ctrl Pts',(88.0112019651358,53.4916076849469,10.3604228281746));
#76512=CARTESIAN_POINT('Ctrl Pts',(88.0761060336377,53.4867817017169,10.3629039839211));
#76513=CARTESIAN_POINT('Ctrl Pts',(88.1410101021396,53.4819557184868,10.3653851396675));
#76514=CARTESIAN_POINT('Ctrl Pts',(88.2056642241824,53.4771297352567,10.3715775346472));
#76515=CARTESIAN_POINT('Ctrl Pts',(88.2696205463436,53.4723037520266,10.3813961152221));
#76516=CARTESIAN_POINT('Ctrl Pts',(88.3305452323787,53.4677065284345,10.3907492787346));
#76517=CARTESIAN_POINT('Ctrl Pts',(88.3910869330253,53.4631093048424,10.4034309692159));
#76518=CARTESIAN_POINT('Ctrl Pts',(88.4508541930947,53.4585120812503,10.4193964883989));
#76519=CARTESIAN_POINT('Ctrl Pts',(88.5116448313103,53.4538361406792,10.4356353807198));
#76520=CARTESIAN_POINT('Ctrl Pts',(88.5716337197105,53.4491602001081,10.4552716297821));
#76521=CARTESIAN_POINT('Ctrl Pts',(88.6304160071788,53.4444842595369,10.4782032102153));
#76522=CARTESIAN_POINT('Ctrl Pts',(88.6880497601553,53.4398996811645,10.5006867354227));
#76523=CARTESIAN_POINT('Ctrl Pts',(88.7445231422343,53.4353151027921,10.5263377827289));
#76524=CARTESIAN_POINT('Ctrl Pts',(88.7994688403535,53.4307305244196,10.5550096878565));
#76525=CARTESIAN_POINT('Ctrl Pts',(88.854380956619,53.4261487480617,10.583664069215));
#76526=CARTESIAN_POINT('Ctrl Pts',(88.907766789943,53.4215669717037,10.6153354124485));
#76527=CARTESIAN_POINT('Ctrl Pts',(88.9592810507774,53.4169851953457,10.6498298533239));
#76528=CARTESIAN_POINT('Ctrl Pts',(89.0107827479892,53.4124045364202,10.6843158814777));
#76529=CARTESIAN_POINT('Ctrl Pts',(89.0604133560476,53.4078238774947,10.7216233573642));
#76530=CARTESIAN_POINT('Ctrl Pts',(89.1078559094675,53.4032432185693,10.7615146802412));
#76531=CARTESIAN_POINT('Ctrl Pts',(89.1570124013203,53.3984970759838,10.8028471412208));
#76532=CARTESIAN_POINT('Ctrl Pts',(89.2038192314359,53.3937509333983,10.8469533897118));
#76533=CARTESIAN_POINT('Ctrl Pts',(89.2479625930688,53.3890047908128,10.8935246787465));
#76534=CARTESIAN_POINT('Ctrl Pts',(89.2906207762093,53.3844183295164,10.9385291030415));
#76535=CARTESIAN_POINT('Ctrl Pts',(89.3307915913948,53.3798318682199,10.9858348723314));
#76536=CARTESIAN_POINT('Ctrl Pts',(89.3682323432263,53.3752454069235,11.0351289110172));
#76537=CARTESIAN_POINT('Ctrl Pts',(89.4076283892803,53.3704194236935,11.0869972663054));
#76538=CARTESIAN_POINT('Ctrl Pts',(89.4440010363312,53.3655934404635,11.1410667268849));
#76539=CARTESIAN_POINT('Ctrl Pts',(89.477120451333,53.3607674572334,11.1969397847196));
#76540=CARTESIAN_POINT('Ctrl Pts',(89.5102398663347,53.3559414740034,11.2528128425543));
#76541=CARTESIAN_POINT('Ctrl Pts',(89.540105820036,53.3511154907734,11.3104888866465));
#76542=CARTESIAN_POINT('Ctrl Pts',(89.5665468526566,53.3462895075433,11.3695455328667));
#76543=CARTESIAN_POINT('Ctrl Pts',(89.5917345363198,53.3416922839513,11.4258027957559));
#76544=CARTESIAN_POINT('Ctrl Pts',(89.6139181232076,53.3370950603592,11.4835436934228));
#76545=CARTESIAN_POINT('Ctrl Pts',(89.6329228404703,53.3324978367672,11.5424151117911));
#76546=CARTESIAN_POINT('Ctrl Pts',(89.6522529702132,53.327821896196,11.6022945690582));
#76547=CARTESIAN_POINT('Ctrl Pts',(89.6682940405242,53.3231459556249,11.6633431814259));
#76548=CARTESIAN_POINT('Ctrl Pts',(89.6809121743324,53.3184700150538,11.7251654864652));
#76549=CARTESIAN_POINT('Ctrl Pts',(89.6932837651337,53.3138854366814,11.7857798587618));
#76550=CARTESIAN_POINT('Ctrl Pts',(89.702364869821,53.309300858309,11.8471374389696));
#76551=CARTESIAN_POINT('Ctrl Pts',(89.7080794740081,53.3047162799366,11.9088500890859));
#76552=CARTESIAN_POINT('Ctrl Pts',(89.7137905855287,53.3001345035787,11.9705250215053));
#76553=CARTESIAN_POINT('Ctrl Pts',(89.7161392295267,53.2955527272207,12.0325540877018));
#76554=CARTESIAN_POINT('Ctrl Pts',(89.715100990825,53.2909709508628,12.094542050896));
#76555=CARTESIAN_POINT('Ctrl Pts',(89.7140630053354,53.2863902919374,12.1565148960749));
#76556=CARTESIAN_POINT('Ctrl Pts',(89.7096397854306,53.2818096330119,12.2184461494038));
#76557=CARTESIAN_POINT('Ctrl Pts',(89.7018590228373,53.2772289740865,12.2799406471193));
#76558=CARTESIAN_POINT('Ctrl Pts',(89.6937971676995,53.272482831501,12.3436567323232));
#76559=CARTESIAN_POINT('Ctrl Pts',(89.68213054133,53.2677366889154,12.4069033158724));
#76560=CARTESIAN_POINT('Ctrl Pts',(89.6669483202019,53.2629905463299,12.469249298103));
#76561=CARTESIAN_POINT('Ctrl Pts',(89.6522768963367,53.2584040850335,12.5294976849418));
#76562=CARTESIAN_POINT('Ctrl Pts',(89.6343229185176,53.2538176237372,12.5889046279803));
#76563=CARTESIAN_POINT('Ctrl Pts',(89.6132177704993,53.2492311624408,12.6470964218582));
#76564=CARTESIAN_POINT('Ctrl Pts',(89.5910104337698,53.2444051792107,12.7083272059501));
#76565=CARTESIAN_POINT('Ctrl Pts',(89.5653140140062,53.2395791959806,12.7682118453188));
#76566=CARTESIAN_POINT('Ctrl Pts',(89.536337804965,53.2347532127505,12.8263416444892));
#76567=CARTESIAN_POINT('Ctrl Pts',(89.5073615959238,53.2299272295204,12.8844714436596));
#76568=CARTESIAN_POINT('Ctrl Pts',(89.4751059865718,53.2251012462903,12.9408458786286));
#76569=CARTESIAN_POINT('Ctrl Pts',(89.4398328311856,53.2202752630601,12.9950918017754));
#76570=CARTESIAN_POINT('Ctrl Pts',(89.4062316820777,53.2156780394681,13.0467663778713));
#76571=CARTESIAN_POINT('Ctrl Pts',(89.3697546816081,53.2110808158761,13.096721870335));
#76572=CARTESIAN_POINT('Ctrl Pts',(89.3306036918106,53.206483592284,13.1446199201572));
#76573=CARTESIAN_POINT('Ctrl Pts',(89.2907823305195,53.2018076517129,13.1933381149453));
#76574=CARTESIAN_POINT('Ctrl Pts',(89.248194755509,53.1971317111418,13.2399272495526));
#76575=CARTESIAN_POINT('Ctrl Pts',(89.20310058838,53.1924557705706,13.2840603526854));
#76576=CARTESIAN_POINT('Ctrl Pts',(89.1588875064995,53.1878711921983,13.3273311485927));
#76577=CARTESIAN_POINT('Ctrl Pts',(89.1122652843203,53.1832866138259,13.3682406525049));
#76578=CARTESIAN_POINT('Ctrl Pts',(89.0635187746866,53.1787020354535,13.4065144775541));
#76579=CARTESIAN_POINT('Ctrl Pts',(89.0148020580706,53.1741202590956,13.4447649103081));
#76580=CARTESIAN_POINT('Ctrl Pts',(88.9639640279461,53.1695384827377,13.4803825446326));
#76581=CARTESIAN_POINT('Ctrl Pts',(88.911323488337,53.1649567063797,13.5131324928799));
#76582=CARTESIAN_POINT('Ctrl Pts',(88.8586957870345,53.1603760474543,13.5458744538633));
#76583=CARTESIAN_POINT('Ctrl Pts',(88.8042668809664,53.1557953885289,13.5757498483781));
#76584=CARTESIAN_POINT('Ctrl Pts',(88.7483837755344,53.1512147296035,13.6025676044934));
#76585=CARTESIAN_POINT('Ctrl Pts',(88.6904818031715,53.1464685870179,13.6303541951172));
#76586=CARTESIAN_POINT('Ctrl Pts',(88.6310190456313,53.1417224444324,13.654857683996));
#76587=CARTESIAN_POINT('Ctrl Pts',(88.5704060480769,53.1369763018468,13.6759191622485));
#76588=CARTESIAN_POINT('Ctrl Pts',(88.5118323406232,53.1323898405505,13.6962720389496));
#76589=CARTESIAN_POINT('Ctrl Pts',(88.4521850947159,53.1278033792541,13.7134107745029));
#76590=CARTESIAN_POINT('Ctrl Pts',(88.3918495305261,53.1232169179578,13.727243049857));
#76591=CARTESIAN_POINT('Ctrl Pts',(88.328363020525,53.1183909347276,13.7417976976737));
#76592=CARTESIAN_POINT('Ctrl Pts',(88.2641149608831,53.1135649514975,13.7526909457334));
#76593=CARTESIAN_POINT('Ctrl Pts',(88.1995622259961,53.1087389682673,13.759876950232));
#76594=CARTESIAN_POINT('Ctrl Pts',(88.1350094911091,53.1039129850372,13.7670629547306));
#76595=CARTESIAN_POINT('Ctrl Pts',(88.0701527321782,53.0990870018071,13.7705417582285));
#76596=CARTESIAN_POINT('Ctrl Pts',(88.0054474678553,53.0942610185769,13.7703309552393));
#76597=CARTESIAN_POINT('Ctrl Pts',(87.9438093407625,53.0896637949847,13.7701301446626));
#76598=CARTESIAN_POINT('Ctrl Pts',(87.8820555940026,53.0850665713925,13.7665808416365));
#76599=CARTESIAN_POINT('Ctrl Pts',(87.8205799798599,53.0804693478002,13.7596691092211));
#76600=CARTESIAN_POINT('Ctrl Pts',(87.7580517359021,53.0757934072291,13.752639029137));
#76601=CARTESIAN_POINT('Ctrl Pts',(87.6958117695767,53.071117466658,13.7421301947354));
#76602=CARTESIAN_POINT('Ctrl Pts',(87.634275594825,53.0664415260869,13.7281833707944));
#76603=CARTESIAN_POINT('Ctrl Pts',(87.5739417621752,53.0618569477144,13.714509050851));
#76604=CARTESIAN_POINT('Ctrl Pts',(87.5142849862034,53.0572723693418,13.6975299992812));
#76605=CARTESIAN_POINT('Ctrl Pts',(87.4556902889564,53.0526877909692,13.6773366998926));
#76606=CARTESIAN_POINT('Ctrl Pts',(87.3971314037679,53.0481060146111,13.6571557422968));
#76607=CARTESIAN_POINT('Ctrl Pts',(87.3396337904558,53.043524238253,13.6337645977005));
#76608=CARTESIAN_POINT('Ctrl Pts',(87.283567702014,53.0389424618949,13.6073036973442));
#76609=CARTESIAN_POINT('Ctrl Pts',(87.2275152873234,53.0343618029693,13.5808492504391));
#76610=CARTESIAN_POINT('Ctrl Pts',(87.1728941645742,53.0297811440437,13.5513267511701));
#76611=CARTESIAN_POINT('Ctrl Pts',(87.1200530726413,53.025200485118,13.5189240889428));
#76612=CARTESIAN_POINT('Ctrl Pts',(87.065303011405,53.0204543425327,13.4853508285072));
#76613=CARTESIAN_POINT('Ctrl Pts',(87.0124645855012,53.0157081999473,13.4486855690757));
#76614=CARTESIAN_POINT('Ctrl Pts',(86.961893976834,53.010962057362,13.4091870263507));
#76615=CARTESIAN_POINT('Ctrl Pts',(86.9130247877561,53.0063755960654,13.3710173898049));
#76616=CARTESIAN_POINT('Ctrl Pts',(86.8662735807736,53.0017891347689,13.3302025046934));
#76617=CARTESIAN_POINT('Ctrl Pts',(86.8219268580204,52.9972026734723,13.2870159288981));
#76618=CARTESIAN_POINT('Ctrl Pts',(86.7752641857629,52.9923766902426,13.2415739907536));
#76619=CARTESIAN_POINT('Ctrl Pts',(86.731264469373,52.9875507070128,13.1935063199345));
#76620=CARTESIAN_POINT('Ctrl Pts',(86.6902140313079,52.982724723783,13.14317188067));
#76621=CARTESIAN_POINT('Ctrl Pts',(86.6491635932428,52.9778987405532,13.0928374414054));
#76622=CARTESIAN_POINT('Ctrl Pts',(86.6110627509574,52.9730727573235,13.0402368038683));
#76623=CARTESIAN_POINT('Ctrl Pts',(86.5761437956817,52.9682467740937,12.9857622021639));
#76624=CARTESIAN_POINT('Ctrl Pts',(86.5421066500874,52.9635426615986,12.9326632496102));
#76625=CARTESIAN_POINT('Ctrl Pts',(86.5109575200296,52.9588385491035,12.8775741112516));
#76626=CARTESIAN_POINT('Ctrl Pts',(86.482928763992,52.9541344366084,12.8208331824218));
#76627=CARTESIAN_POINT('Ctrl Pts',(86.4541800394326,52.9493094906052,12.7626347617718));
#76628=CARTESIAN_POINT('Ctrl Pts',(86.4287145702846,52.9444845446021,12.7026988858379));
#76629=CARTESIAN_POINT('Ctrl Pts',(86.4067358730977,52.9396595985989,12.6414228416863));
#76630=CARTESIAN_POINT('Ctrl Pts',(86.385384982539,52.9349724739168,12.5818971063152));
#76631=CARTESIAN_POINT('Ctrl Pts',(86.3673245239217,52.9302853492346,12.5211072211321));
#76632=CARTESIAN_POINT('Ctrl Pts',(86.35269385782,52.9255982245525,12.4594406872809));
#76633=CARTESIAN_POINT('Ctrl Pts',(86.3374178863764,52.9207043678888,12.3950542674426));
#76634=CARTESIAN_POINT('Ctrl Pts',(86.3258815299883,52.9158105112251,12.3297125519769));
#76635=CARTESIAN_POINT('Ctrl Pts',(86.3181857479463,52.9109166545614,12.2638755761682));
#76636=CARTESIAN_POINT('Ctrl Pts',(86.3104899659043,52.9060227978976,12.1980386003594));
#76637=CARTESIAN_POINT('Ctrl Pts',(86.3066348771815,52.9011289412339,12.1317069497035));
#76638=CARTESIAN_POINT('Ctrl Pts',(86.3066601233573,52.8962350845702,12.0653515514135));
#76639=CARTESIAN_POINT('',(86.306660409711,52.1024850846248,12.0648182329483));
#76640=CARTESIAN_POINT('Ctrl Pts',(86.3066601233575,52.8962350845279,12.0653515508395));
#76641=CARTESIAN_POINT('Ctrl Pts',(86.3066858000485,52.8912577788647,11.9978646744587));
#76642=CARTESIAN_POINT('Ctrl Pts',(86.3107241159865,52.8862804732015,11.9305012550205));
#76643=CARTESIAN_POINT('Ctrl Pts',(86.3187061355887,52.8813031675382,11.8637221908469));
#76644=CARTESIAN_POINT('Ctrl Pts',(86.3267111976187,52.8763114934303,11.7967503494251));
#76645=CARTESIAN_POINT('Ctrl Pts',(86.3386826266837,52.8713198193224,11.7303665837433));
#76646=CARTESIAN_POINT('Ctrl Pts',(86.3545006531629,52.8663281452145,11.6650202629455));
#76647=CARTESIAN_POINT('Ctrl Pts',(86.3703867161387,52.8613150009176,11.5993928745479));
#76648=CARTESIAN_POINT('Ctrl Pts',(86.3901523795347,52.8563018566207,11.5348122054962));
#76649=CARTESIAN_POINT('Ctrl Pts',(86.4136279471483,52.8512887123237,11.4717127290877));
#76650=CARTESIAN_POINT('Ctrl Pts',(86.4277640539517,52.8482699847526,11.4337165897641));
#76651=CARTESIAN_POINT('Ctrl Pts',(86.4432444489851,52.8452512571815,11.396257107537));
#76652=CARTESIAN_POINT('Ctrl Pts',(86.4600240713583,52.8422325296104,11.3594248062846));
#76653=CARTESIAN_POINT('Ctrl Pts',(86.4855777770241,52.8376353060185,11.3033328535416));
#76654=CARTESIAN_POINT('Ctrl Pts',(86.5142307592316,52.8330380824266,11.2485137929798));
#76655=CARTESIAN_POINT('Ctrl Pts',(86.5458336483086,52.8284408588347,11.1953322117642));
#76656=CARTESIAN_POINT('Ctrl Pts',(86.5779776648541,52.8237649182636,11.1412400171441));
#76657=CARTESIAN_POINT('Ctrl Pts',(86.6131734265545,52.8190889776924,11.088842427819));
#76658=CARTESIAN_POINT('Ctrl Pts',(86.6512127534507,52.8144130371213,11.0385013480681));
#76659=CARTESIAN_POINT('Ctrl Pts',(86.6885088381055,52.8098284587491,10.9891438718666));
#76660=CARTESIAN_POINT('Ctrl Pts',(86.7285380461163,52.8052438803768,10.9417636901763));
#76661=CARTESIAN_POINT('Ctrl Pts',(86.7710594362043,52.8006593020046,10.8966744534331));
#76662=CARTESIAN_POINT('Ctrl Pts',(86.8135548379592,52.7960775256469,10.851612774446));
#76663=CARTESIAN_POINT('Ctrl Pts',(86.8585390530228,52.7914957492891,10.8088396336136));
#76664=CARTESIAN_POINT('Ctrl Pts',(86.9057316990031,52.7869139729314,10.7686346627062));
#76665=CARTESIAN_POINT('Ctrl Pts',(86.9529128353433,52.7823333140061,10.7284394972406));
#76666=CARTESIAN_POINT('Ctrl Pts',(87.0023009460659,52.7777526550809,10.6908115882876));
#76667=CARTESIAN_POINT('Ctrl Pts',(87.0535812526061,52.7731719961556,10.6559914263599));
#76668=CARTESIAN_POINT('Ctrl Pts',(87.1067141425788,52.7684258535699,10.6199133301595));
#76669=CARTESIAN_POINT('Ctrl Pts',(87.1618781181891,52.7636797109842,10.5868501134878));
#76670=CARTESIAN_POINT('Ctrl Pts',(87.2186907889171,52.7589335683985,10.5570198975357));
#76671=CARTESIAN_POINT('Ctrl Pts',(87.2735920293924,52.7543471071023,10.5281933023689));
#76672=CARTESIAN_POINT('Ctrl Pts',(87.3300322706156,52.7497606458062,10.5023857575206));
#76673=CARTESIAN_POINT('Ctrl Pts',(87.3876442761706,52.74517418451,10.4797457715835));
#76674=CARTESIAN_POINT('Ctrl Pts',(87.4482649932609,52.7403482012795,10.4559234420326));
#76675=CARTESIAN_POINT('Ctrl Pts',(87.5101826099621,52.7355222180491,10.4356087979634));
#76676=CARTESIAN_POINT('Ctrl Pts',(87.5729521277682,52.7306962348186,10.4189150303542));
#76677=CARTESIAN_POINT('Ctrl Pts',(87.6357216455744,52.7258702515882,10.4022212627449));
#76678=CARTESIAN_POINT('Ctrl Pts',(87.6993424141855,52.7210442683577,10.3891484262244));
#76679=CARTESIAN_POINT('Ctrl Pts',(87.7633613538561,52.7162182851273,10.3797467756781));
#76680=CARTESIAN_POINT('Ctrl Pts',(87.8243456892375,52.711621061534,10.3707907790152));
#76681=CARTESIAN_POINT('Ctrl Pts',(87.8859416847116,52.7070238379407,10.3651289653363));
#76682=CARTESIAN_POINT('Ctrl Pts',(87.9477620249569,52.7024266143474,10.3628335976445));
#76683=CARTESIAN_POINT('Ctrl Pts',(88.0106408976501,52.6977506737764,10.3604989270119));
#76684=CARTESIAN_POINT('Ctrl Pts',(88.0737513593552,52.6930747332054,10.3616472439076));
#76685=CARTESIAN_POINT('Ctrl Pts',(88.1366764500734,52.6883987926345,10.3662999483741));
#76686=CARTESIAN_POINT('Ctrl Pts',(88.1983720609748,52.6838142142608,10.3708617446486));
#76687=CARTESIAN_POINT('Ctrl Pts',(88.2598889476235,52.6792296358872,10.3787921778162));
#76688=CARTESIAN_POINT('Ctrl Pts',(88.3208329193961,52.6746450575136,10.390058951616));
#76689=CARTESIAN_POINT('Ctrl Pts',(88.3817396432744,52.6700632811544,10.4013188393598));
#76690=CARTESIAN_POINT('Ctrl Pts',(88.4420736470582,52.6654815047953,10.4159109321208));
#76691=CARTESIAN_POINT('Ctrl Pts',(88.501447927114,52.6608997284361,10.4337513466418));
#76692=CARTESIAN_POINT('Ctrl Pts',(88.560807726596,52.6563190695094,10.45158741013));
#76693=CARTESIAN_POINT('Ctrl Pts',(88.6192077797048,52.6517384105828,10.4726700762792));
#76694=CARTESIAN_POINT('Ctrl Pts',(88.676275309765,52.6471577516561,10.4968653347093));
#76695=CARTESIAN_POINT('Ctrl Pts',(88.735404495967,52.6424116090718,10.5219346856941));
#76696=CARTESIAN_POINT('Ctrl Pts',(88.7931024763872,52.6376654664874,10.5503456616479));
#76697=CARTESIAN_POINT('Ctrl Pts',(88.8489785946509,52.6329193239031,10.5818953168638));
#76698=CARTESIAN_POINT('Ctrl Pts',(88.902974792473,52.6283328626055,10.6123835017483));
#76699=CARTESIAN_POINT('Ctrl Pts',(88.9552693743075,52.6237464013079,10.6458021629032));
#76700=CARTESIAN_POINT('Ctrl Pts',(89.0055383863637,52.6191599400103,10.6819233281176));
#76701=CARTESIAN_POINT('Ctrl Pts',(89.0584326316906,52.6143339567826,10.719930873844));
#76702=CARTESIAN_POINT('Ctrl Pts',(89.1090834329309,52.6095079735549,10.7609305366531));
#76703=CARTESIAN_POINT('Ctrl Pts',(89.1571543293087,52.6046819903272,10.8046098585264));
#76704=CARTESIAN_POINT('Ctrl Pts',(89.2052252256866,52.5998560070995,10.8482891803997));
#76705=CARTESIAN_POINT('Ctrl Pts',(89.2507158185852,52.5950300238717,10.8946476446369));
#76706=CARTESIAN_POINT('Ctrl Pts',(89.2933381379182,52.590204040644,10.9433318675404));
#76707=CARTESIAN_POINT('Ctrl Pts',(89.333940088373,52.5856068170538,10.9897083772467));
#76708=CARTESIAN_POINT('Ctrl Pts',(89.3721062896434,52.5810095934636,11.0383855163199));
#76709=CARTESIAN_POINT('Ctrl Pts',(89.4075659526996,52.5764123698734,11.0890770883226));
#76710=CARTESIAN_POINT('Ctrl Pts',(89.4436327817057,52.571736429302,11.1406366380165));
#76711=CARTESIAN_POINT('Ctrl Pts',(89.4768990927446,52.5670604887307,11.1942799186709));
#76712=CARTESIAN_POINT('Ctrl Pts',(89.5071207485995,52.5623845481593,11.2496682407195));
#76713=CARTESIAN_POINT('Ctrl Pts',(89.536751909997,52.5577999697888,11.3039743422129));
#76714=CARTESIAN_POINT('Ctrl Pts',(89.5634560684134,52.5532153914182,11.3599574381604));
#76715=CARTESIAN_POINT('Ctrl Pts',(89.5870465481152,52.5486308130476,11.4172688432222));
#76716=CARTESIAN_POINT('Ctrl Pts',(89.6106226097266,52.5440490366915,11.4745452205516));
#76717=CARTESIAN_POINT('Ctrl Pts',(89.6310885726903,52.5394672603354,11.5331478274829));
#76718=CARTESIAN_POINT('Ctrl Pts',(89.6483049988145,52.5348854839793,11.5927060358961));
#76719=CARTESIAN_POINT('Ctrl Pts',(89.6655172260881,52.5303048250556,11.6522497188782));
#76720=CARTESIAN_POINT('Ctrl Pts',(89.6794813484911,52.525724166132,11.7127480518802));
#76721=CARTESIAN_POINT('Ctrl Pts',(89.6901077573731,52.5211435072084,11.7738151702612));
#76722=CARTESIAN_POINT('Ctrl Pts',(89.7011180623501,52.5163973646211,11.8370884364144));
#76723=CARTESIAN_POINT('Ctrl Pts',(89.7085447131949,52.5116512220338,11.9009718095415));
#76724=CARTESIAN_POINT('Ctrl Pts',(89.7123463173579,52.5069050794465,11.9650270134499));
#76725=CARTESIAN_POINT('Ctrl Pts',(89.7160200186911,52.5023186181519,12.026927116121));
#76726=CARTESIAN_POINT('Ctrl Pts',(89.716308810466,52.4977321568572,12.0889871418802));
#76727=CARTESIAN_POINT('Ctrl Pts',(89.7132285048279,52.4931456955626,12.1508112784445));
#76728=CARTESIAN_POINT('Ctrl Pts',(89.7099873342589,52.488319712329,12.2158640996341));
#76729=CARTESIAN_POINT('Ctrl Pts',(89.703015581476,52.4834937290953,12.2806550765543));
#76730=CARTESIAN_POINT('Ctrl Pts',(89.6923932531676,52.4786677458617,12.3447320645396));
#76731=CARTESIAN_POINT('Ctrl Pts',(89.6817709248592,52.4738417626281,12.408809052525));
#76732=CARTESIAN_POINT('Ctrl Pts',(89.6674982389069,52.4690157793944,12.4721714364314));
#76733=CARTESIAN_POINT('Ctrl Pts',(89.6497158858192,52.4641897961608,12.5343856116107));
#76734=CARTESIAN_POINT('Ctrl Pts',(89.632776445882,52.4595925725695,12.5936507312766));
#76735=CARTESIAN_POINT('Ctrl Pts',(89.6125830511616,52.4549953489782,12.6521173850085));
#76736=CARTESIAN_POINT('Ctrl Pts',(89.5892292657091,52.4503981253869,12.7094028446156));
#76737=CARTESIAN_POINT('Ctrl Pts',(89.5654755998887,52.4457221848157,12.7676691872022));
#76738=CARTESIAN_POINT('Ctrl Pts',(89.5384523500933,52.4410462442445,12.8247129684509));
#76739=CARTESIAN_POINT('Ctrl Pts',(89.5083116368733,52.4363703036732,12.8801453787155));
#76740=CARTESIAN_POINT('Ctrl Pts',(89.4787598365825,52.4317857253017,12.9344947070085));
#76741=CARTESIAN_POINT('Ctrl Pts',(89.44621155495,52.4272011469301,12.987294597847));
#76742=CARTESIAN_POINT('Ctrl Pts',(89.4108584772245,52.4226165685585,13.0381990944979));
#76743=CARTESIAN_POINT('Ctrl Pts',(89.3755270066846,52.4180347922014,13.0890724792069));
#76744=CARTESIAN_POINT('Ctrl Pts',(89.337394428918,52.4134530158443,13.1380523494934));
#76745=CARTESIAN_POINT('Ctrl Pts',(89.2966964853522,52.4088712394872,13.1848205321466));
#76746=CARTESIAN_POINT('Ctrl Pts',(89.2560084674577,52.4042905805626,13.2315773086804));
#76747=CARTESIAN_POINT('Ctrl Pts',(89.2127566598054,52.399709921638,13.2761230845364));
#76748=CARTESIAN_POINT('Ctrl Pts',(89.1672166318282,52.3951292627134,13.3181732850863));
#76749=CARTESIAN_POINT('Ctrl Pts',(89.1200313971876,52.3903831201271,13.361742616678));
#76750=CARTESIAN_POINT('Ctrl Pts',(89.0703898291941,52.3856369775408,13.4026321658333));
#76751=CARTESIAN_POINT('Ctrl Pts',(89.0186376816877,52.3808908349544,13.4405694373305));
#76752=CARTESIAN_POINT('Ctrl Pts',(88.9686267059997,52.376304373659,13.477230330722));
#76753=CARTESIAN_POINT('Ctrl Pts',(88.9166454047811,52.3717179123635,13.5111342320162));
#76754=CARTESIAN_POINT('Ctrl Pts',(88.8630348847986,52.367131451068,13.5420797372385));
#76755=CARTESIAN_POINT('Ctrl Pts',(88.8066246256006,52.3623054678362,13.5746413309551));
#76756=CARTESIAN_POINT('Ctrl Pts',(88.7484108841394,52.3574794846045,13.6039267595688));
#76757=CARTESIAN_POINT('Ctrl Pts',(88.688816912249,52.3526535013727,13.6297579956852));
#76758=CARTESIAN_POINT('Ctrl Pts',(88.6292229403586,52.347827518141,13.6555892318015));
#76759=CARTESIAN_POINT('Ctrl Pts',(88.5682493730131,52.3430015349092,13.6779661248141));
#76760=CARTESIAN_POINT('Ctrl Pts',(88.5063368010146,52.3381755516775,13.6967716851726));
#76761=CARTESIAN_POINT('Ctrl Pts',(88.4473589878856,52.3335783280763,13.7146858306975));
#76762=CARTESIAN_POINT('Ctrl Pts',(88.3872870418415,52.328981104475,13.7294331729696));
#76763=CARTESIAN_POINT('Ctrl Pts',(88.3264932499655,52.3243838808738,13.7408847258323));
#76764=CARTESIAN_POINT('Ctrl Pts',(88.2646585030634,52.3197079403038,13.7525323604187));
#76765=CARTESIAN_POINT('Ctrl Pts',(88.2020774375247,52.3150319997338,13.7607700325316));
#76766=CARTESIAN_POINT('Ctrl Pts',(88.1391592105617,52.3103560591638,13.7655146519957));
#76767=CARTESIAN_POINT('Ctrl Pts',(88.0774703291852,52.3057714807822,13.7701665673696));
#76768=CARTESIAN_POINT('Ctrl Pts',(88.0154578752452,52.3011869024006,13.7714606623572));
#76769=CARTESIAN_POINT('Ctrl Pts',(87.9535164641609,52.296602324019,13.7693703292906));
#76770=CARTESIAN_POINT('Ctrl Pts',(87.8916129105884,52.2920205476518,13.7672812737991));
#76771=CARTESIAN_POINT('Ctrl Pts',(87.8297808214775,52.2874387712846,13.7618119089304));
#76772=CARTESIAN_POINT('Ctrl Pts',(87.7684153667387,52.2828569949175,13.752987709293));
#76773=CARTESIAN_POINT('Ctrl Pts',(87.7070648781943,52.2782763359829,13.744165661757));
#76774=CARTESIAN_POINT('Ctrl Pts',(87.6461813017391,52.2736956770482,13.731990476122));
#76775=CARTESIAN_POINT('Ctrl Pts',(87.586153183064,52.2691150181136,13.7165393111766));
#76776=CARTESIAN_POINT('Ctrl Pts',(87.5239564524399,52.264368875537,13.7005299481457));
#76777=CARTESIAN_POINT('Ctrl Pts',(87.4626787516,52.2596227329604,13.6810034567997));
#76778=CARTESIAN_POINT('Ctrl Pts',(87.4027365460003,52.2548765903838,13.6581025111871));
#76779=CARTESIAN_POINT('Ctrl Pts',(87.3448110618613,52.2502901290784,13.6359720548821));
#76780=CARTESIAN_POINT('Ctrl Pts',(87.288133083026,52.245703667773,13.6106908972693));
#76781=CARTESIAN_POINT('Ctrl Pts',(87.2330568291272,52.2411172064676,13.5824363680987));
#76782=CARTESIAN_POINT('Ctrl Pts',(87.1751042903378,52.2362912232554,13.5527062833194));
#76783=CARTESIAN_POINT('Ctrl Pts',(87.1189259206474,52.2314652400432,13.5196840670374));
#76784=CARTESIAN_POINT('Ctrl Pts',(87.0649008559051,52.226639256831,13.483628740236));
#76785=CARTESIAN_POINT('Ctrl Pts',(87.0108757911629,52.2218132736188,13.4475734134345));
#76786=CARTESIAN_POINT('Ctrl Pts',(86.9590045023056,52.2169872904066,13.4084854278801));
#76787=CARTESIAN_POINT('Ctrl Pts',(86.9096242506336,52.2121613071944,13.3666714782402));
#76788=CARTESIAN_POINT('Ctrl Pts',(86.8628648716396,52.2075914645873,13.3270768173739));
#76789=CARTESIAN_POINT('Ctrl Pts',(86.8181334255304,52.2030216219802,13.2848640209387));
#76790=CARTESIAN_POINT('Ctrl Pts',(86.7757433169464,52.1984517793732,13.2402724396713));
#76791=CARTESIAN_POINT('Ctrl Pts',(86.733775453883,52.1939274567148,13.1961250326716));
#76792=CARTESIAN_POINT('Ctrl Pts',(86.6941028933692,52.1894031340565,13.1496463735899));
#76793=CARTESIAN_POINT('Ctrl Pts',(86.6569975161341,52.1848788113982,13.1011097088159));
#76794=CARTESIAN_POINT('Ctrl Pts',(86.6199281062314,52.1803588742988,13.0526200920573));
#76795=CARTESIAN_POINT('Ctrl Pts',(86.5854212685,52.1758389371994,13.0020768350406));
#76796=CARTESIAN_POINT('Ctrl Pts',(86.553710141661,52.1713190000999,12.9497879295297));
#76797=CARTESIAN_POINT('Ctrl Pts',(86.5220173283185,52.1668016733099,12.8975292213904));
#76798=CARTESIAN_POINT('Ctrl Pts',(86.4931172975748,52.1622843465199,12.843527310607));
#76799=CARTESIAN_POINT('Ctrl Pts',(86.4671998749245,52.1577670197298,12.7881191102698));
#76800=CARTESIAN_POINT('Ctrl Pts',(86.4407689541676,52.1531601918044,12.7316131153585));
#76801=CARTESIAN_POINT('Ctrl Pts',(86.4174404093148,52.148553363879,12.673644980549));
#76802=CARTESIAN_POINT('Ctrl Pts',(86.3973653048879,52.1439465359536,12.6145963054291));
#76803=CARTESIAN_POINT('Ctrl Pts',(86.3776695877166,52.1394267696826,12.5566635555033));
#76804=CARTESIAN_POINT('Ctrl Pts',(86.3611054955156,52.1349070034116,12.4976912889509));
#76805=CARTESIAN_POINT('Ctrl Pts',(86.3477652985263,52.1303872371406,12.4380553230553));
#76806=CARTESIAN_POINT('Ctrl Pts',(86.3340396547405,52.1257368783879,12.376696257266));
#76807=CARTESIAN_POINT('Ctrl Pts',(86.323727234676,52.1210865196353,12.3146351214984));
#76808=CARTESIAN_POINT('Ctrl Pts',(86.3168715966915,52.1164361608827,12.2522895292375));
#76809=CARTESIAN_POINT('Ctrl Pts',(86.3100159587071,52.11178580213,12.1899439369766));
#76810=CARTESIAN_POINT('Ctrl Pts',(86.3066170756141,52.1071354433774,12.1273144895588));
#76811=CARTESIAN_POINT('Ctrl Pts',(86.3066604097109,52.1024850846248,12.0648182329483));
#76812=CARTESIAN_POINT('',(86.3066605745511,51.3087350845309,12.0673994500905));
#76813=CARTESIAN_POINT('Ctrl Pts',(86.3066604097115,52.1024850845701,12.0648182322137));
#76814=CARTESIAN_POINT('Ctrl Pts',(86.3067111580443,52.0970390772838,11.9916292403597));
#76815=CARTESIAN_POINT('Ctrl Pts',(86.3114763800807,52.0915930699975,11.9186024518142));
#76816=CARTESIAN_POINT('Ctrl Pts',(86.3208935106417,52.0861470627112,11.8461935164083));
#76817=CARTESIAN_POINT('Ctrl Pts',(86.3288429408399,52.0815498391194,11.7850698254908));
#76818=CARTESIAN_POINT('Ctrl Pts',(86.340128826112,52.0769526155277,11.7242524630003));
#76819=CARTESIAN_POINT('Ctrl Pts',(86.3547154834296,52.0723553919359,11.6641338086265));
#76820=CARTESIAN_POINT('Ctrl Pts',(86.3695519040185,52.0676794513647,11.6029857592751));
#76821=CARTESIAN_POINT('Ctrl Pts',(86.38780322277,52.0630035107936,11.5425611089259));
#76822=CARTESIAN_POINT('Ctrl Pts',(86.4093767528214,52.0583275702224,11.4832669481684));
#76823=CARTESIAN_POINT('Ctrl Pts',(86.4305287622981,52.0537429918508,11.4251313232952));
#76824=CARTESIAN_POINT('Ctrl Pts',(86.454874144327,52.0491584134791,11.3680829098034));
#76825=CARTESIAN_POINT('Ctrl Pts',(86.4822747215772,52.0445738351075,11.3124922968469));
#76826=CARTESIAN_POINT('Ctrl Pts',(86.5096585520707,52.0399920587504,11.2569356599069));
#76827=CARTESIAN_POINT('Ctrl Pts',(86.5400936506463,52.0354102823934,11.2028355124607));
#76828=CARTESIAN_POINT('Ctrl Pts',(86.5733941459654,52.0308285060364,11.1505415115662));
#76829=CARTESIAN_POINT('Ctrl Pts',(86.6066865197486,52.026247847112,11.0982602644643));
#76830=CARTESIAN_POINT('Ctrl Pts',(86.6428426296857,52.0216671881876,11.0477847186531));
#76831=CARTESIAN_POINT('Ctrl Pts',(86.6816322280494,52.0170865292632,10.9994372205542));
#76832=CARTESIAN_POINT('Ctrl Pts',(86.7218231629647,52.012340386677,10.9493430914222));
#76833=CARTESIAN_POINT('Ctrl Pts',(86.7648411935247,52.0075942440907,10.9015342057474));
#76834=CARTESIAN_POINT('Ctrl Pts',(86.8103848719461,52.0028481015044,10.8563313884009));
#76835=CARTESIAN_POINT('Ctrl Pts',(86.8543962589852,51.9982616402095,10.812649394358));
#76836=CARTESIAN_POINT('Ctrl Pts',(86.9007655913499,51.9936751789146,10.7714011796717));
#76837=CARTESIAN_POINT('Ctrl Pts',(86.9491854582199,51.9890887176196,10.7328365762352));
#76838=CARTESIAN_POINT('Ctrl Pts',(87.0001339892513,51.9842627343877,10.6922579868686));
#76839=CARTESIAN_POINT('Ctrl Pts',(87.0533525810631,51.9794367511557,10.6546513716129));
#76840=CARTESIAN_POINT('Ctrl Pts',(87.1084491168998,51.9746107679237,10.6202556453456));
#76841=CARTESIAN_POINT('Ctrl Pts',(87.1635456527366,51.9697847846918,10.5858599190783));
#76842=CARTESIAN_POINT('Ctrl Pts',(87.2205195270349,51.9649588014598,10.5546753250427));
#76843=CARTESIAN_POINT('Ctrl Pts',(87.2789524109492,51.9601328182278,10.5268829924386));
#76844=CARTESIAN_POINT('Ctrl Pts',(87.3346154797033,51.9555355945679,10.5004080622803));
#76845=CARTESIAN_POINT('Ctrl Pts',(87.3918308845876,51.950938370908,10.4769023109299));
#76846=CARTESIAN_POINT('Ctrl Pts',(87.4502496246742,51.9463411472481,10.4565485865762));
#76847=CARTESIAN_POINT('Ctrl Pts',(87.5096686515911,51.9416652066855,10.4358463514125));
#76848=CARTESIAN_POINT('Ctrl Pts',(87.5703321721983,51.9369892661229,10.418405415213));
#76849=CARTESIAN_POINT('Ctrl Pts',(87.6318479078409,51.9323133255602,10.4043687152044));
#76850=CARTESIAN_POINT('Ctrl Pts',(87.6921617017417,51.9277287471196,10.3906062750333));
#76851=CARTESIAN_POINT('Ctrl Pts',(87.7532941876698,51.9231441686789,10.3801163569567));
#76852=CARTESIAN_POINT('Ctrl Pts',(87.8148590786071,51.9185595902382,10.3729838823699));
#76853=CARTESIAN_POINT('Ctrl Pts',(87.8763863421556,51.9139778138121,10.3658557670274));
#76854=CARTESIAN_POINT('Ctrl Pts',(87.9383449820718,51.9093960373859,10.3620810847948));
#76855=CARTESIAN_POINT('Ctrl Pts',(88.0003404276645,51.9048142609597,10.3616933347787));
#76856=CARTESIAN_POINT('Ctrl Pts',(88.0623207534155,51.9002336019662,10.3613056793296));
#76857=CARTESIAN_POINT('Ctrl Pts',(88.1243373582144,51.8956529429727,10.3643033194917));
#76858=CARTESIAN_POINT('Ctrl Pts',(88.185994545916,51.8910722839792,10.3706676595724));
#76859=CARTESIAN_POINT('Ctrl Pts',(88.2498791967054,51.8863261414596,10.3772619214698));
#76860=CARTESIAN_POINT('Ctrl Pts',(88.3133773792603,51.8815799989401,10.3874707993819));
#76861=CARTESIAN_POINT('Ctrl Pts',(88.3760560569369,51.8768338564206,10.4012150556622));
#76862=CARTESIAN_POINT('Ctrl Pts',(88.4366259475975,51.8722473950572,10.4144968945741));
#76863=CARTESIAN_POINT('Ctrl Pts',(88.4964301152985,51.8676609336939,10.4310797722773));
#76864=CARTESIAN_POINT('Ctrl Pts',(88.5550919317186,51.8630744723306,10.4508409349421));
#76865=CARTESIAN_POINT('Ctrl Pts',(88.6168172820691,51.8582484892329,10.4716340975691));
#76866=CARTESIAN_POINT('Ctrl Pts',(88.677277092279,51.8534225061353,10.4959463811966));
#76867=CARTESIAN_POINT('Ctrl Pts',(88.7360579612984,51.8485965230376,10.5235779473964));
#76868=CARTESIAN_POINT('Ctrl Pts',(88.7948388303178,51.84377053994,10.5512095135962));
#76869=CARTESIAN_POINT('Ctrl Pts',(88.8519402253361,51.8389445568423,10.5821599855566));
#76870=CARTESIAN_POINT('Ctrl Pts',(88.9069830748624,51.8341185737447,10.6161761606457));
#76871=CARTESIAN_POINT('Ctrl Pts',(88.9594168014754,51.8295213502986,10.6485799122753));
#76872=CARTESIAN_POINT('Ctrl Pts',(89.0101980435192,51.8249241268526,10.6838982930395));
#76873=CARTESIAN_POINT('Ctrl Pts',(89.0589838887052,51.8203269034065,10.7219372765327));
#76874=CARTESIAN_POINT('Ctrl Pts',(89.108605082099,51.8156509628171,10.7606275923245));
#76875=CARTESIAN_POINT('Ctrl Pts',(89.1561614010464,51.8109750222277,10.8021323582303));
#76876=CARTESIAN_POINT('Ctrl Pts',(89.2013199894643,51.8062990816384,10.8461995416128));
#76877=CARTESIAN_POINT('Ctrl Pts',(89.2455962323468,51.801714503411,10.8894057042266));
#76878=CARTESIAN_POINT('Ctrl Pts',(89.2875672179041,51.7971299251836,10.9350746791043));
#76879=CARTESIAN_POINT('Ctrl Pts',(89.3269520802885,51.7925453469563,10.9829279996305));
#76880=CARTESIAN_POINT('Ctrl Pts',(89.3663128713366,51.7879635707426,11.0307520730475));
#76881=CARTESIAN_POINT('Ctrl Pts',(89.403090350482,51.783381794529,11.0807574527049));
#76882=CARTESIAN_POINT('Ctrl Pts',(89.4370423597757,51.7788000183153,11.1326308213117));
#76883=CARTESIAN_POINT('Ctrl Pts',(89.4709860886462,51.7742193595332,11.1844915387248));
#76884=CARTESIAN_POINT('Ctrl Pts',(89.5021054369677,51.7696387007511,11.2382189149636));
#76885=CARTESIAN_POINT('Ctrl Pts',(89.5302014022898,51.7650580419689,11.2934704310639));
#76886=CARTESIAN_POINT('Ctrl Pts',(89.5593123812506,51.7603118992433,11.3507180003967));
#76887=CARTESIAN_POINT('Ctrl Pts',(89.5851770245851,51.7555657565177,11.409601453028));
#76888=CARTESIAN_POINT('Ctrl Pts',(89.6076270229513,51.7508196137921,11.4697140072234));
#76889=CARTESIAN_POINT('Ctrl Pts',(89.6293217024915,51.746233152635,11.5278041049746));
#76890=CARTESIAN_POINT('Ctrl Pts',(89.6478277825351,51.7416466914778,11.5870413819114));
#76891=CARTESIAN_POINT('Ctrl Pts',(89.6630441084574,51.7370602303207,11.6470428431076));
#76892=CARTESIAN_POINT('Ctrl Pts',(89.6790550884844,51.7322342468108,11.7101778076001));
#76893=CARTESIAN_POINT('Ctrl Pts',(89.6914231524119,51.727408263301,11.7741583320411));
#76894=CARTESIAN_POINT('Ctrl Pts',(89.7000919605218,51.7225822797911,11.8385287171955));
#76895=CARTESIAN_POINT('Ctrl Pts',(89.7087607686316,51.7177562962812,11.90289910235));
#76896=CARTESIAN_POINT('Ctrl Pts',(89.7137303484956,51.7129303127714,11.9676586962098));
#76897=CARTESIAN_POINT('Ctrl Pts',(89.7150078131359,51.7081043292615,12.0323516958568));
#76898=CARTESIAN_POINT('Ctrl Pts',(89.7162247237674,51.7035071056239,12.0939781366755));
#76899=CARTESIAN_POINT('Ctrl Pts',(89.71409668693,51.6989098819864,12.1557971814345));
#76900=CARTESIAN_POINT('Ctrl Pts',(89.7086007131203,51.6943126583488,12.2174155025532));
#76901=CARTESIAN_POINT('Ctrl Pts',(89.703010633344,51.6896367177834,12.2800888963248));
#76902=CARTESIAN_POINT('Ctrl Pts',(89.6939360891808,51.6849607772179,12.3425540995861));
#76903=CARTESIAN_POINT('Ctrl Pts',(89.6814082778584,51.6802848366525,12.4043947707369));
#76904=CARTESIAN_POINT('Ctrl Pts',(89.6691252446246,51.6757002582384,12.465027150919));
#76905=CARTESIAN_POINT('Ctrl Pts',(89.6535227817232,51.6711156798242,12.5250586618879));
#76906=CARTESIAN_POINT('Ctrl Pts',(89.6346824935692,51.6665311014101,12.5841023023275));
#76907=CARTESIAN_POINT('Ctrl Pts',(89.6158537202772,51.661949325012,12.6431098563032));
#76908=CARTESIAN_POINT('Ctrl Pts',(89.5937912000363,51.6573675486138,12.7011302529871));
#76909=CARTESIAN_POINT('Ctrl Pts',(89.5686268111683,51.6527857722156,12.757790107424));
#76910=CARTESIAN_POINT('Ctrl Pts',(89.5434685595586,51.6482051132515,12.8144361432792));
#76911=CARTESIAN_POINT('Ctrl Pts',(89.5152101476267,51.6436244542874,12.8697218305777));
#76912=CARTESIAN_POINT('Ctrl Pts',(89.4840313941275,51.6390437953233,12.9232942012605));
#76913=CARTESIAN_POINT('Ctrl Pts',(89.4517262586315,51.6342976527779,12.9788019589325));
#76914=CARTESIAN_POINT('Ctrl Pts',(89.4162859747846,51.6295515102325,13.0324697025458));
#76915=CARTESIAN_POINT('Ctrl Pts',(89.3779609977017,51.6248053676871,13.0839353940022));
#76916=CARTESIAN_POINT('Ctrl Pts',(89.3409254422562,51.6202189063563,13.1336695521035));
#76917=CARTESIAN_POINT('Ctrl Pts',(89.3011966246599,51.6156324450255,13.1813471287117));
#76918=CARTESIAN_POINT('Ctrl Pts',(89.2590414409187,51.6110459836947,13.2266754056796));
#76919=CARTESIAN_POINT('Ctrl Pts',(89.2146847589663,51.606220000542,13.2743708914178));
#76920=CARTESIAN_POINT('Ctrl Pts',(89.1676417913895,51.6013940173892,13.319464517301));
#76921=CARTESIAN_POINT('Ctrl Pts',(89.1182648220577,51.5965680342365,13.3616617804943));
#76922=CARTESIAN_POINT('Ctrl Pts',(89.0688878527258,51.5917420510837,13.4038590436876));
#76923=CARTESIAN_POINT('Ctrl Pts',(89.0171774443592,51.586916067931,13.4431596137063));
#76924=CARTESIAN_POINT('Ctrl Pts',(88.963520384612,51.5820900847782,13.479322239441));
#76925=CARTESIAN_POINT('Ctrl Pts',(88.9124067525923,51.5774928607006,13.5137707007131));
#76926=CARTESIAN_POINT('Ctrl Pts',(88.8593170143169,51.572895636623,13.5455134682698));
#76927=CARTESIAN_POINT('Ctrl Pts',(88.804569143224,51.5682984125454,13.5743178877553));
#76928=CARTESIAN_POINT('Ctrl Pts',(88.7488838461878,51.563622472035,13.6036155138181));
#76929=CARTESIAN_POINT('Ctrl Pts',(88.6914834854479,51.5589465315246,13.6298728452724));
#76930=CARTESIAN_POINT('Ctrl Pts',(88.6327347597007,51.5542705910141,13.6528902684748));
#76931=CARTESIAN_POINT('Ctrl Pts',(88.5751339057874,51.5496860121518,13.6754579618924));
#76932=CARTESIAN_POINT('Ctrl Pts',(88.5162374001639,51.5451014332895,13.6949110208099));
#76933=CARTESIAN_POINT('Ctrl Pts',(88.4564146330363,51.5405168544272,13.7111080937972));
#76934=CARTESIAN_POINT('Ctrl Pts',(88.3966284285346,51.535935077579,13.7272952674177));
#76935=CARTESIAN_POINT('Ctrl Pts',(88.3359175753889,51.5313533007309,13.7402302682345));
#76936=CARTESIAN_POINT('Ctrl Pts',(88.2746672929125,51.5267715238828,13.74982136649));
#76937=CARTESIAN_POINT('Ctrl Pts',(88.2134319485466,51.5221908644677,13.7594101256071));
#76938=CARTESIAN_POINT('Ctrl Pts',(88.1516579387086,51.5176102050526,13.7656565224022));
#76939=CARTESIAN_POINT('Ctrl Pts',(88.0897393328737,51.5130295456375,13.7685201769902));
#76940=CARTESIAN_POINT('Ctrl Pts',(88.0255838312244,51.5082834035256,13.7714872850857));
#76941=CARTESIAN_POINT('Ctrl Pts',(87.9612736639141,51.5035372614137,13.7708224680467));
#76942=CARTESIAN_POINT('Ctrl Pts',(87.8972488331793,51.4987911193018,13.7665397694988));
#76943=CARTESIAN_POINT('Ctrl Pts',(87.8353780690605,51.4942046575228,13.7624011590782));
#76944=CARTESIAN_POINT('Ctrl Pts',(87.7737742606188,51.4896181957437,13.7548843942375));
#76945=CARTESIAN_POINT('Ctrl Pts',(87.7128280906952,51.4850317339646,13.7440549300013));
#76946=CARTESIAN_POINT('Ctrl Pts',(87.6486991062743,51.4802057516863,13.7326599146268));
#76947=CARTESIAN_POINT('Ctrl Pts',(87.5852989611591,51.475379769408,13.717596849635));
#76948=CARTESIAN_POINT('Ctrl Pts',(87.523066151467,51.4705537871298,13.6990019580686));
#76949=CARTESIAN_POINT('Ctrl Pts',(87.4608333417749,51.4657278048515,13.6804070665021));
#76950=CARTESIAN_POINT('Ctrl Pts',(87.3997684503712,51.4609018225733,13.6582806418593));
#76951=CARTESIAN_POINT('Ctrl Pts',(87.3402839503183,51.456075840295,13.6328167781522));
#76952=CARTESIAN_POINT('Ctrl Pts',(87.2836191186344,51.4514786179385,13.6085599457052));
#76953=CARTESIAN_POINT('Ctrl Pts',(87.2281555585013,51.4468813955821,13.5811753816928));
#76954=CARTESIAN_POINT('Ctrl Pts',(87.1742611959948,51.4422841732256,13.5508040306626));
#76955=CARTESIAN_POINT('Ctrl Pts',(87.1194439987869,51.4376082325,13.5199126301253));
#76956=CARTESIAN_POINT('Ctrl Pts',(87.06625076872,51.4329322917744,13.4859313155132));
#76957=CARTESIAN_POINT('Ctrl Pts',(87.0150481026579,51.4282563510489,13.4490598879949));
#76958=CARTESIAN_POINT('Ctrl Pts',(86.9648458896195,51.4236717739064,13.4129088942742));
#76959=CARTESIAN_POINT('Ctrl Pts',(86.9165575854691,51.419087196764,13.3739800239028));
#76960=CARTESIAN_POINT('Ctrl Pts',(86.8705022991761,51.4145026196216,13.332506940374));
#76961=CARTESIAN_POINT('Ctrl Pts',(86.8244751610249,51.4099208444882,13.2910592044291));
#76962=CARTESIAN_POINT('Ctrl Pts',(86.7806787120628,51.4053390693548,13.2470706785538));
#76963=CARTESIAN_POINT('Ctrl Pts',(86.7393989587362,51.4007572942213,13.2008152393482));
#76964=CARTESIAN_POINT('Ctrl Pts',(86.6981292729125,51.3961766365131,13.1545710811394));
#76965=CARTESIAN_POINT('Ctrl Pts',(86.659375403062,51.3915959788048,13.1060614867506));
#76966=CARTESIAN_POINT('Ctrl Pts',(86.6233850158349,51.3870153210966,13.0555956200997));
#76967=CARTESIAN_POINT('Ctrl Pts',(86.586094398825,51.3822691773228,13.0033065659844));
#76968=CARTESIAN_POINT('Ctrl Pts',(86.5517711506645,51.3775230335491,12.9489176203987));
#76969=CARTESIAN_POINT('Ctrl Pts',(86.5206421299862,51.3727768897754,12.8928060563928));
#76970=CARTESIAN_POINT('Ctrl Pts',(86.4905604429464,51.368190429664,12.8385823618802));
#76971=CARTESIAN_POINT('Ctrl Pts',(86.463461609385,51.3636039695526,12.7827506368254));
#76972=CARTESIAN_POINT('Ctrl Pts',(86.4395025448572,51.3590175094412,12.7256746046951));
#76973=CARTESIAN_POINT('Ctrl Pts',(86.4142922306473,51.3541915238363,12.6656178064765));
#76974=CARTESIAN_POINT('Ctrl Pts',(86.3925588490335,51.3493655382314,12.604183774149));
#76975=CARTESIAN_POINT('Ctrl Pts',(86.3744257960406,51.3445395526265,12.5418147859562));
#76976=CARTESIAN_POINT('Ctrl Pts',(86.3562927430476,51.3397135670216,12.4794457977634));
#76977=CARTESIAN_POINT('Ctrl Pts',(86.3417600882466,51.3348875814167,12.4161425025795));
#76978=CARTESIAN_POINT('Ctrl Pts',(86.3308884938938,51.3300615958118,12.3523567052638));
#76979=CARTESIAN_POINT('Ctrl Pts',(86.3148742743359,51.3229527587313,12.2583981073123));
#76980=CARTESIAN_POINT('Ctrl Pts',(86.3067391222564,51.3158439216507,12.163059810845));
#76981=CARTESIAN_POINT('Ctrl Pts',(86.3066605745515,51.3087350845701,12.0673994506177));
#76982=CARTESIAN_POINT('',(86.3066600260026,50.5149850846118,12.0662977153839));
#76983=CARTESIAN_POINT('Ctrl Pts',(86.3066605745511,51.3087350845309,12.0673994500905));
#76984=CARTESIAN_POINT('Ctrl Pts',(86.3066106156482,51.3042136305189,12.0065563171497));
#76985=CARTESIAN_POINT('Ctrl Pts',(86.3098229390638,51.2996921765069,11.9455970361689));
#76986=CARTESIAN_POINT('Ctrl Pts',(86.3163083194618,51.2951707224949,11.8849062576601));
#76987=CARTESIAN_POINT('Ctrl Pts',(86.3227871823644,51.2906538123267,11.8242764704651));
#76988=CARTESIAN_POINT('Ctrl Pts',(86.3325325346701,51.2861369021586,11.7639151711377));
#76989=CARTESIAN_POINT('Ctrl Pts',(86.3455031304503,51.2816199919904,11.7042058415065));
#76990=CARTESIAN_POINT('Ctrl Pts',(86.3584657883159,51.2771058461399,11.6445330535706));
#76991=CARTESIAN_POINT('Ctrl Pts',(86.3746496682963,51.2725917002894,11.5855119574642));
#76992=CARTESIAN_POINT('Ctrl Pts',(86.3939621494986,51.268077554439,11.5275174787927));
#76993=CARTESIAN_POINT('Ctrl Pts',(86.4132703985603,51.2635643978192,11.4695357090415));
#76994=CARTESIAN_POINT('Ctrl Pts',(86.4357057221016,51.2590512411994,11.4125806087351));
#76995=CARTESIAN_POINT('Ctrl Pts',(86.4611258432148,51.2545380845797,11.3570113303237));
#76996=CARTESIAN_POINT('Ctrl Pts',(86.4865680009035,51.250021015527,11.3013938791837));
#76997=CARTESIAN_POINT('Ctrl Pts',(86.5149999056639,51.2455039464744,11.2471651287774));
#76998=CARTESIAN_POINT('Ctrl Pts',(86.5462319704495,51.2409868774218,11.1946622611142));
#76999=CARTESIAN_POINT('Ctrl Pts',(86.5774776671001,51.2364678368033,11.1421364775147));
#77000=CARTESIAN_POINT('Ctrl Pts',(86.6115256631514,51.2319487961847,11.091338513034));
#77001=CARTESIAN_POINT('Ctrl Pts',(86.6481431777198,51.2274297555662,11.0425762766262));
#77002=CARTESIAN_POINT('Ctrl Pts',(86.6848270397391,51.2229025268761,10.9937256876876));
#77003=CARTESIAN_POINT('Ctrl Pts',(86.7240893763254,51.2183752981861,10.9469185934149));
#77004=CARTESIAN_POINT('Ctrl Pts',(86.7656580695585,51.2138480694961,10.9024286391097));
#77005=CARTESIAN_POINT('Ctrl Pts',(86.7956545696152,51.2105811634403,10.8703241197457));
#77006=CARTESIAN_POINT('Ctrl Pts',(86.8268512280379,51.2073142573844,10.8394254501484));
#77007=CARTESIAN_POINT('Ctrl Pts',(86.8591352487777,51.2040473513286,10.8098222934268));
#77008=CARTESIAN_POINT('Ctrl Pts',(86.9045656857548,51.1994501243947,10.7681643984389));
#77009=CARTESIAN_POINT('Ctrl Pts',(86.9523521679268,51.1948528974607,10.7288886987404));
#77010=CARTESIAN_POINT('Ctrl Pts',(87.0022148020363,51.1902556705268,10.6922724942809));
#77011=CARTESIAN_POINT('Ctrl Pts',(87.0529311787428,51.1855797303734,10.6550293511518));
#77012=CARTESIAN_POINT('Ctrl Pts',(87.1057951451597,51.18090379022,10.620538059968));
#77013=CARTESIAN_POINT('Ctrl Pts',(87.1604737166441,51.1762278500666,10.5890504826092));
#77014=CARTESIAN_POINT('Ctrl Pts',(87.2140839796211,51.1716432683103,10.5581781087179));
#77015=CARTESIAN_POINT('Ctrl Pts',(87.2694381156879,51.167058686554,10.5301933974363));
#77016=CARTESIAN_POINT('Ctrl Pts',(87.3261918247247,51.1624741047977,10.5052909948757));
#77017=CARTESIAN_POINT('Ctrl Pts',(87.3829108469857,51.1578923250496,10.4804038121848));
#77018=CARTESIAN_POINT('Ctrl Pts',(87.4410272809177,51.1533105453016,10.4585954069282));
#77019=CARTESIAN_POINT('Ctrl Pts',(87.5001738029954,51.1487287655535,10.4400137048382));
#77020=CARTESIAN_POINT('Ctrl Pts',(87.5593059000659,51.1441481032372,10.4214365345649));
#77021=CARTESIAN_POINT('Ctrl Pts',(87.6194671011378,51.139567440921,10.4060846577511));
#77022=CARTESIAN_POINT('Ctrl Pts',(87.6802737041403,51.1349867786048,10.3940565342013));
#77023=CARTESIAN_POINT('Ctrl Pts',(87.7432769532544,51.1302406392915,10.3815938931893));
#77024=CARTESIAN_POINT('Ctrl Pts',(87.8069725695866,51.1254944999782,10.3726999207212));
#77025=CARTESIAN_POINT('Ctrl Pts',(87.8709233462469,51.1207483606649,10.3674260785373));
#77026=CARTESIAN_POINT('Ctrl Pts',(87.9327226229017,51.1161618960153,10.362329664558));
#77027=CARTESIAN_POINT('Ctrl Pts',(87.9947596329381,51.1115754313658,10.3606135911176));
#77028=CARTESIAN_POINT('Ctrl Pts',(88.0566383046152,51.1069889667162,10.3622711539826));
#77029=CARTESIAN_POINT('Ctrl Pts',(88.1217483724266,51.1021629900711,10.3640152772421));
#77030=CARTESIAN_POINT('Ctrl Pts',(88.1866824684781,51.0973370134259,10.3694950077655));
#77031=CARTESIAN_POINT('Ctrl Pts',(88.2509867298057,51.0925110367808,10.37864075991));
#77032=CARTESIAN_POINT('Ctrl Pts',(88.3152909911333,51.0876850601356,10.3877865120545));
#77033=CARTESIAN_POINT('Ctrl Pts',(88.3789647977517,51.0828590834905,10.4005980821477));
#77034=CARTESIAN_POINT('Ctrl Pts',(88.4415714258755,51.0780331068453,10.4169447908516));
#77035=CARTESIAN_POINT('Ctrl Pts',(88.5012103445833,51.0734358934599,10.4325166250287));
#77036=CARTESIAN_POINT('Ctrl Pts',(88.5601258555124,51.0688386800745,10.4513599045846));
#77037=CARTESIAN_POINT('Ctrl Pts',(88.6179331809773,51.0642414666891,10.4733898940956));
#77038=CARTESIAN_POINT('Ctrl Pts',(88.6767304717578,51.0595655248421,10.4957971528427));
#77039=CARTESIAN_POINT('Ctrl Pts',(88.734380726769,51.0548895829952,10.5215012533864));
#77040=CARTESIAN_POINT('Ctrl Pts',(88.7904917387102,51.0502136411482,10.5503590580607));
#77041=CARTESIAN_POINT('Ctrl Pts',(88.8455062724811,51.0456290729547,10.5786529457466));
#77042=CARTESIAN_POINT('Ctrl Pts',(88.8990407051215,51.0410445047613,10.6099781477268));
#77043=CARTESIAN_POINT('Ctrl Pts',(88.9507447637455,51.0364599365678,10.6441509874065));
#77044=CARTESIAN_POINT('Ctrl Pts',(89.0024172221083,51.0318781703507,10.6783029414792));
#77045=CARTESIAN_POINT('Ctrl Pts',(89.0522611008404,51.0272964041336,10.7152988021777));
#77046=CARTESIAN_POINT('Ctrl Pts',(89.0999528899065,51.0227146379165,10.7549102093432));
#77047=CARTESIAN_POINT('Ctrl Pts',(89.1476330481359,51.0181339890778,10.7945119562756));
#77048=CARTESIAN_POINT('Ctrl Pts',(89.193161767169,51.0135533402391,10.8367276583122));
#77049=CARTESIAN_POINT('Ctrl Pts',(89.2362482106196,51.0089726914004,10.8812883650553));
#77050=CARTESIAN_POINT('Ctrl Pts',(89.2808914118443,51.0042265389805,10.9274590962302));
#77051=CARTESIAN_POINT('Ctrl Pts',(89.322912024005,50.9994803865607,10.9761471583441));
#77052=CARTESIAN_POINT('Ctrl Pts',(89.3620296693481,50.9947342341408,11.0270131530471));
#77053=CARTESIAN_POINT('Ctrl Pts',(89.3998310641828,50.9901477826815,11.0761675827823));
#77054=CARTESIAN_POINT('Ctrl Pts',(89.4349215240421,50.9855613312222,11.1273552188832));
#77055=CARTESIAN_POINT('Ctrl Pts',(89.4670918540817,50.9809748797629,11.1802396779733));
#77056=CARTESIAN_POINT('Ctrl Pts',(89.5009424480424,50.9761488768628,11.2358863048274));
#77057=CARTESIAN_POINT('Ctrl Pts',(89.5315591962283,50.9713228739626,11.293411303298));
#77058=CARTESIAN_POINT('Ctrl Pts',(89.5587543818358,50.9664968710625,11.3523956214344));
#77059=CARTESIAN_POINT('Ctrl Pts',(89.5859495674434,50.9616708681624,11.4113799395709));
#77060=CARTESIAN_POINT('Ctrl Pts',(89.6097230252991,50.9568448652623,11.4718229460076));
#77061=CARTESIAN_POINT('Ctrl Pts',(89.6299476630851,50.9520188623621,11.5332868503675));
#77062=CARTESIAN_POINT('Ctrl Pts',(89.64921357763,50.9474216299938,11.5918371364854));
#77063=CARTESIAN_POINT('Ctrl Pts',(89.6653386807364,50.9428243976255,11.6515541042634));
#77064=CARTESIAN_POINT('Ctrl Pts',(89.6781854577588,50.9382271652571,11.7120685305917));
#77065=CARTESIAN_POINT('Ctrl Pts',(89.6912521785553,50.933551225783,11.7736189966437));
#77066=CARTESIAN_POINT('Ctrl Pts',(89.7009270074487,50.9288752863089,11.8359940100405));
#77067=CARTESIAN_POINT('Ctrl Pts',(89.7071174661682,50.9241993468348,11.898786434285));
#77068=CARTESIAN_POINT('Ctrl Pts',(89.7131869835846,50.9196147599146,11.9603521000679));
#77069=CARTESIAN_POINT('Ctrl Pts',(89.7159070005629,50.9150301729943,12.0223184828421));
#77070=CARTESIAN_POINT('Ctrl Pts',(89.7152418402189,50.9104455860741,12.0842916824639));
#77071=CARTESIAN_POINT('Ctrl Pts',(89.7145770864241,50.9058638012758,12.1462270037628));
#77072=CARTESIAN_POINT('Ctrl Pts',(89.7105312633608,50.9012820164775,12.208168625688));
#77073=CARTESIAN_POINT('Ctrl Pts',(89.703120749887,50.8967002316792,12.2697208958398));
#77074=CARTESIAN_POINT('Ctrl Pts',(89.695712043927,50.8921195644336,12.331258152649));
#77075=CARTESIAN_POINT('Ctrl Pts',(89.6849403375673,50.887538897188,12.3924057410408));
#77076=CARTESIAN_POINT('Ctrl Pts',(89.6708738325338,50.8829582299424,12.4527734423014));
#77077=CARTESIAN_POINT('Ctrl Pts',(89.6562992042134,50.8782120956037,12.5153218014233));
#77078=CARTESIAN_POINT('Ctrl Pts',(89.6381872542293,50.8734659612651,12.5770322703839));
#77079=CARTESIAN_POINT('Ctrl Pts',(89.6166710385845,50.8687198269265,12.6374852154264));
#77080=CARTESIAN_POINT('Ctrl Pts',(89.5958786517995,50.8641333577011,12.6959044577488));
#77081=CARTESIAN_POINT('Ctrl Pts',(89.571907694026,50.8595468884757,12.7531489879837));
#77082=CARTESIAN_POINT('Ctrl Pts',(89.5449273008262,50.8549604192503,12.808860600234));
#77083=CARTESIAN_POINT('Ctrl Pts',(89.5165380371022,50.850134452355,12.8674813786989));
#77084=CARTESIAN_POINT('Ctrl Pts',(89.48481672904,50.8453084854598,12.924404189032));
#77085=CARTESIAN_POINT('Ctrl Pts',(89.4500136048722,50.8404825185646,12.9792440421884));
#77086=CARTESIAN_POINT('Ctrl Pts',(89.4152104807044,50.8356565516694,13.0340838953448));
#77087=CARTESIAN_POINT('Ctrl Pts',(89.3773259812303,50.8308305847741,13.0868403101328));
#77088=CARTESIAN_POINT('Ctrl Pts',(89.3366589580983,50.8260046178789,13.1371690634133));
#77089=CARTESIAN_POINT('Ctrl Pts',(89.2979193047422,50.8214073724887,13.18511253962));
#77090=CARTESIAN_POINT('Ctrl Pts',(89.2564959118719,50.8168101270984,13.2310501401612));
#77091=CARTESIAN_POINT('Ctrl Pts',(89.212624387168,50.8122128817082,13.2746660695838));
#77092=CARTESIAN_POINT('Ctrl Pts',(89.1680019001511,50.8075369438618,13.3190285862168));
#77093=CARTESIAN_POINT('Ctrl Pts',(89.1208469412602,50.8028610060155,13.3609887302104));
#77094=CARTESIAN_POINT('Ctrl Pts',(89.0714513947245,50.7981850681691,13.400247981084));
#77095=CARTESIAN_POINT('Ctrl Pts',(89.0230207146095,50.7936004676138,13.438740362563));
#77096=CARTESIAN_POINT('Ctrl Pts',(88.9724366103187,50.7890158670586,13.4746360859703));
#77097=CARTESIAN_POINT('Ctrl Pts',(88.9200106573475,50.7844312665033,13.5076915274873));
#77098=CARTESIAN_POINT('Ctrl Pts',(88.8676167451246,50.7798494678816,13.5407267667758));
#77099=CARTESIAN_POINT('Ctrl Pts',(88.8133836459609,50.7752676692598,13.5709248952249));
#77100=CARTESIAN_POINT('Ctrl Pts',(88.757652642223,50.770685870638,13.5980850718748));
#77101=CARTESIAN_POINT('Ctrl Pts',(88.7019352299095,50.7661051894045,13.6252386248239));
#77102=CARTESIAN_POINT('Ctrl Pts',(88.6447210955907,50.761524508171,13.6493554738316));
#77103=CARTESIAN_POINT('Ctrl Pts',(88.5863750651557,50.7569438269374,13.6702812627457));
#77104=CARTESIAN_POINT('Ctrl Pts',(88.5259217583888,50.752197705809,13.6919628257781));
#77105=CARTESIAN_POINT('Ctrl Pts',(88.4642537550222,50.7474515846805,13.7102181578227));
#77106=CARTESIAN_POINT('Ctrl Pts',(88.4017957626031,50.742705463552,13.7249314354522));
#77107=CARTESIAN_POINT('Ctrl Pts',(88.3414385696333,50.7381189800978,13.7391498261289));
#77108=CARTESIAN_POINT('Ctrl Pts',(88.2803442229204,50.7335324966437,13.750060649943));
#77109=CARTESIAN_POINT('Ctrl Pts',(88.218905399802,50.7289460131895,13.7576117108643));
#77110=CARTESIAN_POINT('Ctrl Pts',(88.1542589064933,50.7241200732239,13.765557006437));
#77111=CARTESIAN_POINT('Ctrl Pts',(88.0892316229153,50.7192941332582,13.7697820481331));
#77112=CARTESIAN_POINT('Ctrl Pts',(88.0242827004128,50.7144681932926,13.7702882401371));
#77113=CARTESIAN_POINT('Ctrl Pts',(87.9593337779103,50.7096422533269,13.7707944321412));
#77114=CARTESIAN_POINT('Ctrl Pts',(87.8944638597993,50.7048163133613,13.7675818837741));
#77115=CARTESIAN_POINT('Ctrl Pts',(87.8301242227846,50.6999903733956,13.7607149579846));
#77116=CARTESIAN_POINT('Ctrl Pts',(87.7688349409761,50.69539323222,13.7541735945359));
#77117=CARTESIAN_POINT('Ctrl Pts',(87.7077751321042,50.6907960910443,13.7442897274374));
#77118=CARTESIAN_POINT('Ctrl Pts',(87.6473378815273,50.6861989498687,13.7310899973239));
#77119=CARTESIAN_POINT('Ctrl Pts',(87.5858645432479,50.6815229989955,13.7176639816345));
#77120=CARTESIAN_POINT('Ctrl Pts',(87.5250358470893,50.6768470481223,13.7008073044624));
#77121=CARTESIAN_POINT('Ctrl Pts',(87.4652609216621,50.6721710972492,13.6806032620972));
#77122=CARTESIAN_POINT('Ctrl Pts',(87.4066551073436,50.6675866012138,13.6607943815863));
#77123=CARTESIAN_POINT('Ctrl Pts',(87.3490627197813,50.6630021051784,13.6377680671013));
#77124=CARTESIAN_POINT('Ctrl Pts',(87.2928574184861,50.6584176091431,13.6116539289947));
#77125=CARTESIAN_POINT('Ctrl Pts',(87.2366864663903,50.6538359148677,13.585555750232));
#77126=CARTESIAN_POINT('Ctrl Pts',(87.1819013804066,50.6492542205924,13.5563737037183));
#77127=CARTESIAN_POINT('Ctrl Pts',(87.1288559908015,50.6446725263171,13.5242855627878));
#77128=CARTESIAN_POINT('Ctrl Pts',(87.0758235340169,50.6400919490895,13.4922052451604));
#77129=CARTESIAN_POINT('Ctrl Pts',(87.0245303669891,50.6355113718619,13.4572205030133));
#77130=CARTESIAN_POINT('Ctrl Pts',(86.9753040373237,50.6309307946342,13.4195541025375));
#77131=CARTESIAN_POINT('Ctrl Pts',(86.9242975627487,50.6261845724907,13.3805255925661));
#77132=CARTESIAN_POINT('Ctrl Pts',(86.8755107748959,50.6214383503473,13.3386180591));
#77133=CARTESIAN_POINT('Ctrl Pts',(86.8292713698261,50.6166921282038,13.2941255148507));
#77134=CARTESIAN_POINT('Ctrl Pts',(86.784589189961,50.6121057467143,13.25113136599));
#77135=CARTESIAN_POINT('Ctrl Pts',(86.7422858376984,50.6075193652249,13.2057239984065));
#77136=CARTESIAN_POINT('Ctrl Pts',(86.7026181382662,50.6029329837355,13.1582049896819));
#77137=CARTESIAN_POINT('Ctrl Pts',(86.6608767416166,50.598106841265,13.1082018430421));
#77138=CARTESIAN_POINT('Ctrl Pts',(86.6220545207183,50.5932806987945,13.0558607267832));
#77139=CARTESIAN_POINT('Ctrl Pts',(86.5863993683685,50.5884545563239,13.0015682102098));
#77140=CARTESIAN_POINT('Ctrl Pts',(86.5507442160188,50.5836284138534,12.9472756936364));
#77141=CARTESIAN_POINT('Ctrl Pts',(86.5182563893731,50.5788022713829,12.8910323767418));
#77142=CARTESIAN_POINT('Ctrl Pts',(86.4891266012826,50.5739761289124,12.8332523664847));
#77143=CARTESIAN_POINT('Ctrl Pts',(86.459454928889,50.569060208554,12.7743975087041));
#77144=CARTESIAN_POINT('Ctrl Pts',(86.433157332778,50.5641442881956,12.7137323715273));
#77145=CARTESIAN_POINT('Ctrl Pts',(86.4104420441128,50.5592283678373,12.6516526832911));
#77146=CARTESIAN_POINT('Ctrl Pts',(86.3878424418835,50.5543374837139,12.589889159995));
#77147=CARTESIAN_POINT('Ctrl Pts',(86.3687889427545,50.5494465995905,12.5267258171671));
#77148=CARTESIAN_POINT('Ctrl Pts',(86.3534411451279,50.5445557154672,12.4625772033731));
#77149=CARTESIAN_POINT('Ctrl Pts',(86.3379755003825,50.5396272769913,12.3979360283986));
#77150=CARTESIAN_POINT('Ctrl Pts',(86.3262729414904,50.5346988385154,12.3322947441721));
#77151=CARTESIAN_POINT('Ctrl Pts',(86.3184469541847,50.5297704000395,12.2660975329719));
#77152=CARTESIAN_POINT('Ctrl Pts',(86.310620966879,50.5248419615636,12.1999003217717));
#77153=CARTESIAN_POINT('Ctrl Pts',(86.3066717033888,50.5199135230877,12.1331475901878));
#77154=CARTESIAN_POINT('Ctrl Pts',(86.3066600260026,50.5149850846118,12.0662977153839));
#77155=CARTESIAN_POINT('',(86.3066605689282,49.7212350845238,12.0646074147082));
#77156=CARTESIAN_POINT('Ctrl Pts',(86.3066600260025,50.5149850845702,12.06629771482));
#77157=CARTESIAN_POINT('Ctrl Pts',(86.3066487968142,50.5102457989619,12.0020135300569));
#77158=CARTESIAN_POINT('Ctrl Pts',(86.3102788918965,50.5055065133535,11.9377784889388));
#77159=CARTESIAN_POINT('Ctrl Pts',(86.3175077249544,50.5007672277452,11.8740136724633));
#77160=CARTESIAN_POINT('Ctrl Pts',(86.3247527769692,50.4960173088482,11.8101057901849));
#77161=CARTESIAN_POINT('Ctrl Pts',(86.3356126403743,50.4912673899512,11.7466706948135));
#77162=CARTESIAN_POINT('Ctrl Pts',(86.3499931349081,50.4865174710542,11.6841217082398));
#77163=CARTESIAN_POINT('Ctrl Pts',(86.3643903902438,50.4817620160159,11.6214998193629));
#77164=CARTESIAN_POINT('Ctrl Pts',(86.3823163239311,50.4770065609776,11.5597665355359));
#77165=CARTESIAN_POINT('Ctrl Pts',(86.4036270091007,50.4722511059393,11.4993193988433));
#77166=CARTESIAN_POINT('Ctrl Pts',(86.4249924565275,50.467483430766,11.4387169306058));
#77167=CARTESIAN_POINT('Ctrl Pts',(86.449759860851,50.4627157555925,11.3794076368747));
#77168=CARTESIAN_POINT('Ctrl Pts',(86.4777373601943,50.4579480804192,11.3217685084759));
#77169=CARTESIAN_POINT('Ctrl Pts',(86.4972709051324,50.4546193484225,11.2815255800086));
#77170=CARTESIAN_POINT('Ctrl Pts',(86.5183682753801,50.4512906164259,11.2420963079173));
#77171=CARTESIAN_POINT('Ctrl Pts',(86.5409516333099,50.4479618844293,11.2036006521386));
#77172=CARTESIAN_POINT('Ctrl Pts',(86.5721417994069,50.4433645298556,11.1504338068234));
#77173=CARTESIAN_POINT('Ctrl Pts',(86.606283984092,50.4387671752819,11.0988521303865));
#77174=CARTESIAN_POINT('Ctrl Pts',(86.6431920725684,50.4341698207082,11.0492029163814));
#77175=CARTESIAN_POINT('Ctrl Pts',(86.680730926981,50.4294938965098,10.9987051882904));
#77176=CARTESIAN_POINT('Ctrl Pts',(86.7211309265507,50.4248179723114,10.950207100825));
#77177=CARTESIAN_POINT('Ctrl Pts',(86.7641477588114,50.420142048113,10.9040471936248));
#77178=CARTESIAN_POINT('Ctrl Pts',(86.8063254783426,50.4155573353616,10.8587877099031));
#77179=CARTESIAN_POINT('Ctrl Pts',(86.851018492454,50.4109726226102,10.8157763956407));
#77180=CARTESIAN_POINT('Ctrl Pts',(86.8979548455414,50.4063879098588,10.7753004533447));
#77181=CARTESIAN_POINT('Ctrl Pts',(86.9448625218334,50.4018059982384,10.7348492407143));
#77182=CARTESIAN_POINT('Ctrl Pts',(86.9940104346816,50.3972240866179,10.6969306602472));
#77183=CARTESIAN_POINT('Ctrl Pts',(87.0450908979768,50.3926421749974,10.6617940171653));
#77184=CARTESIAN_POINT('Ctrl Pts',(87.0961589111338,50.3880613801529,10.6266659381416));
#77185=CARTESIAN_POINT('Ctrl Pts',(87.1491581204776,50.3834805853084,10.594318738798));
#77186=CARTESIAN_POINT('Ctrl Pts',(87.2037506543892,50.3788997904638,10.5649592511824));
#77187=CARTESIAN_POINT('Ctrl Pts',(87.2603122030945,50.3741537779207,10.5345408410126));
#77188=CARTESIAN_POINT('Ctrl Pts',(87.318583726246,50.3694077653775,10.5073301125322));
#77189=CARTESIAN_POINT('Ctrl Pts',(87.3781624688156,50.3646617528344,10.4835046620213));
#77190=CARTESIAN_POINT('Ctrl Pts',(87.4357400024264,50.3600751555862,10.4604794919955));
#77191=CARTESIAN_POINT('Ctrl Pts',(87.4945378015802,50.355488558338,10.4406158728676));
#77192=CARTESIAN_POINT('Ctrl Pts',(87.5541752808107,50.3509019610898,10.424023748181));
#77193=CARTESIAN_POINT('Ctrl Pts',(87.6169219690562,50.3460762408991,10.4065665905601));
#77194=CARTESIAN_POINT('Ctrl Pts',(87.680597661316,50.3412505207085,10.3927315331494));
#77195=CARTESIAN_POINT('Ctrl Pts',(87.7447481675762,50.3364248005179,10.3825853756929));
#77196=CARTESIAN_POINT('Ctrl Pts',(87.8088986738363,50.3315990803272,10.3724392182365));
#77197=CARTESIAN_POINT('Ctrl Pts',(87.8735233419441,50.3267733601366,10.3659819481964));
#77198=CARTESIAN_POINT('Ctrl Pts',(87.9381664171364,50.321947639946,10.3632169531008));
#77199=CARTESIAN_POINT('Ctrl Pts',(87.9997399437425,50.3173510670004,10.3605832526065));
#77200=CARTESIAN_POINT('Ctrl Pts',(88.061583113388,50.3127544940547,10.3612882410334));
#77201=CARTESIAN_POINT('Ctrl Pts',(88.1233033296202,50.3081579211091,10.3653640019816));
#77202=CARTESIAN_POINT('Ctrl Pts',(88.1860903420984,50.3034818992072,10.3695102099687));
#77203=CARTESIAN_POINT('Ctrl Pts',(88.2487495844209,50.2988058773052,10.3771449384457));
#77204=CARTESIAN_POINT('Ctrl Pts',(88.310864002806,50.2941298554033,10.3882466166265));
#77205=CARTESIAN_POINT('Ctrl Pts',(88.3717550718666,50.2895459281934,10.3991296462092));
#77206=CARTESIAN_POINT('Ctrl Pts',(88.4321220576025,50.2849620009836,10.413344206161));
#77207=CARTESIAN_POINT('Ctrl Pts',(88.4915762679907,50.2803780737737,10.4308176596342));
#77208=CARTESIAN_POINT('Ctrl Pts',(88.5509941564265,50.275796946991,10.4482804381706));
#77209=CARTESIAN_POINT('Ctrl Pts',(88.6094998876824,50.2712158202084,10.4689980192556));
#77210=CARTESIAN_POINT('Ctrl Pts',(88.66671722287,50.2666346934257,10.4928471913919));
#77211=CARTESIAN_POINT('Ctrl Pts',(88.7239206342945,50.2620546814541,10.5166905598636));
#77212=CARTESIAN_POINT('Ctrl Pts',(88.7798358022469,50.2574746694826,10.5436638107564));
#77213=CARTESIAN_POINT('Ctrl Pts',(88.8341057955293,50.2528946575111,10.5735953347145));
#77214=CARTESIAN_POINT('Ctrl Pts',(88.8903517785809,50.2481478856737,10.6046166761119));
#77215=CARTESIAN_POINT('Ctrl Pts',(88.9448299322576,50.2434011138363,10.6388156448567));
#77216=CARTESIAN_POINT('Ctrl Pts',(88.997172346362,50.238654341999,10.6759500228874));
#77217=CARTESIAN_POINT('Ctrl Pts',(89.0477400437914,50.2340685137344,10.7118253263981));
#77218=CARTESIAN_POINT('Ctrl Pts',(89.0963141523153,50.2294826854698,10.7504397723638));
#77219=CARTESIAN_POINT('Ctrl Pts',(89.1425959842488,50.2248968572052,10.7915333021095));
#77220=CARTESIAN_POINT('Ctrl Pts',(89.1913142670116,50.2200696135814,10.8347901508174));
#77221=CARTESIAN_POINT('Ctrl Pts',(89.2374917905969,50.2152423699577,10.8807938651008));
#77222=CARTESIAN_POINT('Ctrl Pts',(89.2808257891941,50.210415126334,10.9291986538108));
#77223=CARTESIAN_POINT('Ctrl Pts',(89.3241597877912,50.2055878827102,10.9776034425208));
#77224=CARTESIAN_POINT('Ctrl Pts',(89.3646499174546,50.2007606390865,11.0284087492997));
#77225=CARTESIAN_POINT('Ctrl Pts',(89.4020459495463,50.1959333954627,11.0812330215473));
#77226=CARTESIAN_POINT('Ctrl Pts',(89.4376669307682,50.1913352831803,11.1315499216178));
#77227=CARTESIAN_POINT('Ctrl Pts',(89.4706273049234,50.1867371708979,11.1839051611084));
#77228=CARTESIAN_POINT('Ctrl Pts',(89.5006871383485,50.1821390586154,11.2379860717119));
#77229=CARTESIAN_POINT('Ctrl Pts',(89.5312550424806,50.1774632291306,11.2929810567915));
#77230=CARTESIAN_POINT('Ctrl Pts',(89.558823061198,50.1727873996458,11.3497602120251));
#77231=CARTESIAN_POINT('Ctrl Pts',(89.5831833051602,50.168111570161,11.4079616344198));
#77232=CARTESIAN_POINT('Ctrl Pts',(89.6070727119168,50.1635261155711,11.4650381339636));
#77233=CARTESIAN_POINT('Ctrl Pts',(89.6278770357406,50.1589406609812,11.5234819186271));
#77234=CARTESIAN_POINT('Ctrl Pts',(89.6454464357721,50.1543552063913,11.5829268335005));
#77235=CARTESIAN_POINT('Ctrl Pts',(89.6630050729331,50.1497725608134,11.642335332906));
#77236=CARTESIAN_POINT('Ctrl Pts',(89.6773325718359,50.1451899152354,11.7027432594939));
#77237=CARTESIAN_POINT('Ctrl Pts',(89.6883283361337,50.1406072696574,11.7637674928092));
#77238=CARTESIAN_POINT('Ctrl Pts',(89.6993213992027,50.1360257498561,11.8247767348592));
#77239=CARTESIAN_POINT('Ctrl Pts',(89.7069842622872,50.1314442300548,11.8864014825308));
#77240=CARTESIAN_POINT('Ctrl Pts',(89.7112674612321,50.1268627102534,11.9482485844018));
#77241=CARTESIAN_POINT('Ctrl Pts',(89.7157037728269,50.1221174136473,12.012306551045));
#77242=CARTESIAN_POINT('Ctrl Pts',(89.7165141093847,50.1173721170411,12.0766024957849));
#77243=CARTESIAN_POINT('Ctrl Pts',(89.7137023404252,50.112626820435,12.1406965562169));
#77244=CARTESIAN_POINT('Ctrl Pts',(89.7109841953776,50.1080395287142,12.2026564666653));
#77245=CARTESIAN_POINT('Ctrl Pts',(89.7048815061111,50.1034522369935,12.2644272088208));
#77246=CARTESIAN_POINT('Ctrl Pts',(89.6954506739318,50.0988649452727,12.3256165685985));
#77247=CARTESIAN_POINT('Ctrl Pts',(89.6855325877313,50.0940406462239,12.3899673420278));
#77248=CARTESIAN_POINT('Ctrl Pts',(89.6719332443629,50.089216347175,12.4536743970219));
#77249=CARTESIAN_POINT('Ctrl Pts',(89.654778475292,50.0843920481261,12.5162967463427));
#77250=CARTESIAN_POINT('Ctrl Pts',(89.637623706221,50.0795677490773,12.5789190956634));
#77251=CARTESIAN_POINT('Ctrl Pts',(89.6169137902823,50.0747434500284,12.6404561514783));
#77252=CARTESIAN_POINT('Ctrl Pts',(89.5928329021536,50.0699191509795,12.7004915328548));
#77253=CARTESIAN_POINT('Ctrl Pts',(89.5698820994029,50.0653212501343,12.7577095303252));
#77254=CARTESIAN_POINT('Ctrl Pts',(89.5437758042981,50.0607233492891,12.8137977326738));
#77255=CARTESIAN_POINT('Ctrl Pts',(89.5146466153835,50.0561254484439,12.8683850021316));
#77256=CARTESIAN_POINT('Ctrl Pts',(89.4850235558929,50.0514495925294,12.9238977709671));
#77257=CARTESIAN_POINT('Ctrl Pts',(89.4522742532069,50.0467737366149,12.9778577101907));
#77258=CARTESIAN_POINT('Ctrl Pts',(89.4165900779081,50.0420978807004,13.0298938574792));
#77259=CARTESIAN_POINT('Ctrl Pts',(89.381597103485,50.0375125959054,13.0809220669277));
#77260=CARTESIAN_POINT('Ctrl Pts',(89.3437822413148,50.0329273111103,13.1300999082551));
#77261=CARTESIAN_POINT('Ctrl Pts',(89.3033718855931,50.0283420263153,13.1771029407434));
#77262=CARTESIAN_POINT('Ctrl Pts',(89.2629861465548,50.0237595347276,13.2240773405024));
#77263=CARTESIAN_POINT('Ctrl Pts',(89.220008380139,50.01917704314,13.2688791733253));
#77264=CARTESIAN_POINT('Ctrl Pts',(89.1747059368798,50.0145945515523,13.3112161772442));
#77265=CARTESIAN_POINT('Ctrl Pts',(89.1294144657396,50.0100131698307,13.3535429272649));
#77266=CARTESIAN_POINT('Ctrl Pts',(89.0817998070938,50.0054317881091,13.3934056861967));
#77267=CARTESIAN_POINT('Ctrl Pts',(89.0321654642234,50.0008504063874,13.4305497170413));
#77268=CARTESIAN_POINT('Ctrl Pts',(88.9807535278566,49.9961049480632,13.46902401608));
#77269=CARTESIAN_POINT('Ctrl Pts',(88.9271749221276,49.9913594897389,13.5045807549041));
#77270=CARTESIAN_POINT('Ctrl Pts',(88.8718013827731,49.9866140314147,13.5369846413257));
#77271=CARTESIAN_POINT('Ctrl Pts',(88.818274586487,49.9820268371705,13.5683078373428));
#77272=CARTESIAN_POINT('Ctrl Pts',(88.7630712069238,49.9774396429263,13.5966850075563));
#77273=CARTESIAN_POINT('Ctrl Pts',(88.7065513627189,49.9728524486821,13.6219508788583));
#77274=CARTESIAN_POINT('Ctrl Pts',(88.6471065079281,49.9680278583178,13.6485243075688));
#77275=CARTESIAN_POINT('Ctrl Pts',(88.5862058221421,49.9632032679535,13.6716554140613));
#77276=CARTESIAN_POINT('Ctrl Pts',(88.5242881493081,49.9583786775892,13.69121078983));
#77277=CARTESIAN_POINT('Ctrl Pts',(88.4623704764741,49.9535540872249,13.7107661655987));
#77278=CARTESIAN_POINT('Ctrl Pts',(88.3994364620039,49.9487294968606,13.7267457263269));
#77279=CARTESIAN_POINT('Ctrl Pts',(88.3359359037635,49.9439049064963,13.739078448264));
#77280=CARTESIAN_POINT('Ctrl Pts',(88.275493887077,49.9393126953507,13.7508171574307));
#77281=CARTESIAN_POINT('Ctrl Pts',(88.2142892124175,49.9347204842051,13.7593007386264));
#77282=CARTESIAN_POINT('Ctrl Pts',(88.152704642768,49.9301282730595,13.7644388802127));
#77283=CARTESIAN_POINT('Ctrl Pts',(88.0899888039669,49.9254517059325,13.7696714061732));
#77284=CARTESIAN_POINT('Ctrl Pts',(88.0268794771053,49.9207751388056,13.771434151298));
#77285=CARTESIAN_POINT('Ctrl Pts',(87.96379294189,49.9160985716787,13.7696861005668));
#77286=CARTESIAN_POINT('Ctrl Pts',(87.9020151183292,49.911519018564,13.7679743126349));
#77287=CARTESIAN_POINT('Ctrl Pts',(87.8402596861978,49.9069394654494,13.7628960104431));
#77288=CARTESIAN_POINT('Ctrl Pts',(87.778921210903,49.9023599123347,13.7544650636751));
#77289=CARTESIAN_POINT('Ctrl Pts',(87.717620147725,49.8977831524225,13.7460392591863));
#77290=CARTESIAN_POINT('Ctrl Pts',(87.6567360416306,49.8932063925102,13.7342649337972));
#77291=CARTESIAN_POINT('Ctrl Pts',(87.5966586802207,49.888629632598,13.7192078230893));
#77292=CARTESIAN_POINT('Ctrl Pts',(87.5365957676149,49.8840539734116,13.7041543336663));
#77293=CARTESIAN_POINT('Ctrl Pts',(87.4773397093041,49.8794783142252,13.6858197501331));
#77294=CARTESIAN_POINT('Ctrl Pts',(87.4192683985301,49.8749026550389,13.6643205396359));
#77295=CARTESIAN_POINT('Ctrl Pts',(87.3589717827859,49.8701516556201,13.6419974748233));
#77296=CARTESIAN_POINT('Ctrl Pts',(87.2999531278244,49.8654006562012,13.6162624728202));
#77297=CARTESIAN_POINT('Ctrl Pts',(87.2426137837962,49.8606496567824,13.5873012385284));
#77298=CARTESIAN_POINT('Ctrl Pts',(87.1873193869315,49.8560680967416,13.5593728760791));
#77299=CARTESIAN_POINT('Ctrl Pts',(87.1335869555861,49.8514865367007,13.5284448610906));
#77300=CARTESIAN_POINT('Ctrl Pts',(87.0817498541583,49.8469049766599,13.4947298562196));
#77301=CARTESIAN_POINT('Ctrl Pts',(87.0298755271838,49.8423201264837,13.4609906397424));
#77302=CARTESIAN_POINT('Ctrl Pts',(86.9798996477705,49.8377352763076,13.4244607546482));
#77303=CARTESIAN_POINT('Ctrl Pts',(86.9321238428729,49.8331504261314,13.3853942068929));
#77304=CARTESIAN_POINT('Ctrl Pts',(86.884267715068,49.8285578676917,13.3462619786389));
#77305=CARTESIAN_POINT('Ctrl Pts',(86.838619409982,49.823965309252,13.3045849297218));
#77306=CARTESIAN_POINT('Ctrl Pts',(86.7954439568676,49.8193727508123,13.2606540677553));
#77307=CARTESIAN_POINT('Ctrl Pts',(86.7907994973359,49.8188787212126,13.2559283475629));
#77308=CARTESIAN_POINT('Ctrl Pts',(86.7861836137786,49.8183846916129,13.2511765776306));
#77309=CARTESIAN_POINT('Ctrl Pts',(86.7815966074234,49.8178906620131,13.2463991417826));
#77310=CARTESIAN_POINT('Ctrl Pts',(86.7393784611865,49.8133436846882,13.2024283099049));
#77311=CARTESIAN_POINT('Ctrl Pts',(86.6994265036506,49.8087967073632,13.1560896518755));
#77312=CARTESIAN_POINT('Ctrl Pts',(86.6620215912074,49.8042497300383,13.1076487355204));
#77313=CARTESIAN_POINT('Ctrl Pts',(86.6246693612079,49.7997091568421,13.0592760451198));
#77314=CARTESIAN_POINT('Ctrl Pts',(86.5898573866485,49.795168583646,13.008807368977));
#77315=CARTESIAN_POINT('Ctrl Pts',(86.5578291487055,49.7906280104498,12.9565443911159));
#77316=CARTESIAN_POINT('Ctrl Pts',(86.5258336294948,49.7860920757167,12.9043348029664));
#77317=CARTESIAN_POINT('Ctrl Pts',(86.4966164826327,49.7815561409836,12.8503349873008));
#77318=CARTESIAN_POINT('Ctrl Pts',(86.4703790443116,49.7770202062506,12.7948771545973));
#77319=CARTESIAN_POINT('Ctrl Pts',(86.4434889842422,49.7723714461105,12.7380398812909));
#77320=CARTESIAN_POINT('Ctrl Pts',(86.4197291914862,49.7677226859705,12.6796715411922));
#77321=CARTESIAN_POINT('Ctrl Pts',(86.3992664835047,49.7630739258305,12.6201569339147));
#77322=CARTESIAN_POINT('Ctrl Pts',(86.3793118303186,49.7585405866251,12.5621199747398));
#77323=CARTESIAN_POINT('Ctrl Pts',(86.3624925481563,49.7540072474198,12.5029935460392));
#77324=CARTESIAN_POINT('Ctrl Pts',(86.3489136999958,49.7494739082145,12.4431524452241));
#77325=CARTESIAN_POINT('Ctrl Pts',(86.3348162661056,49.7447674376071,12.3810259708212));
#77326=CARTESIAN_POINT('Ctrl Pts',(86.3242119685148,49.7400609669997,12.3181297082135));
#77327=CARTESIAN_POINT('Ctrl Pts',(86.3171600745083,49.7353544963923,12.2548945272111));
#77328=CARTESIAN_POINT('Ctrl Pts',(86.3101081805018,49.730648025785,12.1916593462086));
#77329=CARTESIAN_POINT('Ctrl Pts',(86.3066087018371,49.7259415551776,12.1280858736035));
#77330=CARTESIAN_POINT('Ctrl Pts',(86.3066605689277,49.7212350845702,12.0646074153347));
#77331=CARTESIAN_POINT('',(87.4571200021394,49.5646,10.4541712921126));
#77332=CARTESIAN_POINT('Ctrl Pts',(86.3066605689282,49.7212350845237,12.0646074147082));
#77333=CARTESIAN_POINT('Ctrl Pts',(86.3067280594444,49.7151109317192,11.9820079870988));
#77334=CARTESIAN_POINT('Ctrl Pts',(86.3128039761533,49.7089867789146,11.8996672994486));
#77335=CARTESIAN_POINT('Ctrl Pts',(86.3247540055513,49.70286262611,11.8183121282626));
#77336=CARTESIAN_POINT('Ctrl Pts',(86.3318997838979,49.6992005565833,11.7696640453768));
#77337=CARTESIAN_POINT('Ctrl Pts',(86.3411450603446,49.6955384870566,11.7213677890819));
#77338=CARTESIAN_POINT('Ctrl Pts',(86.352453256211,49.6918764175298,11.6735748042403));
#77339=CARTESIAN_POINT('Ctrl Pts',(86.3666577103926,49.6872764177229,11.6135410666397));
#77340=CARTESIAN_POINT('Ctrl Pts',(86.3841544769797,49.682676417916,11.5541587182232));
#77341=CARTESIAN_POINT('Ctrl Pts',(86.4048668634738,49.6780764181091,11.4958147815381));
#77342=CARTESIAN_POINT('Ctrl Pts',(86.4259196253528,49.6734008245648,11.4365120543286));
#77343=CARTESIAN_POINT('Ctrl Pts',(86.4502946188797,49.6687252310205,11.3782827131778));
#77344=CARTESIAN_POINT('Ctrl Pts',(86.4778572181742,49.6640496374763,11.3215216281614));
#77345=CARTESIAN_POINT('Ctrl Pts',(86.5049010407252,49.659462046851,11.2658288869006));
#77346=CARTESIAN_POINT('Ctrl Pts',(86.5350132812281,49.6548744562257,11.2115500870572));
#77347=CARTESIAN_POINT('Ctrl Pts',(86.5680176299229,49.6502868656004,11.1590398491407));
#77348=CARTESIAN_POINT('Ctrl Pts',(86.6010023848879,49.6457019984954,11.1065607850378));
#77349=CARTESIAN_POINT('Ctrl Pts',(86.6368755734356,49.6411171313903,11.0558486302588));
#77350=CARTESIAN_POINT('Ctrl Pts',(86.6754156395653,49.6365322642853,11.0072322012063));
#77351=CARTESIAN_POINT('Ctrl Pts',(86.7139469229305,49.63194844201,10.9586268511866));
#77352=CARTESIAN_POINT('Ctrl Pts',(86.7551435616937,49.6273646197347,10.9121166767737));
#77353=CARTESIAN_POINT('Ctrl Pts',(86.798742713684,49.6227807974595,10.8679987031002));
#77354=CARTESIAN_POINT('Ctrl Pts',(86.8438579691743,49.6180375787584,10.822346584581));
#77355=CARTESIAN_POINT('Ctrl Pts',(86.8915455481405,49.6132943600573,10.7792565633214));
#77356=CARTESIAN_POINT('Ctrl Pts',(86.9414732651338,49.6085511413563,10.7390156749206));
#77357=CARTESIAN_POINT('Ctrl Pts',(86.9897857092911,49.6039613763435,10.7000766688778));
#77358=CARTESIAN_POINT('Ctrl Pts',(87.0401950753472,49.5993716113308,10.6638054910064));
#77359=CARTESIAN_POINT('Ctrl Pts',(87.0923693508009,49.5947818463181,10.6304190841503));
#77360=CARTESIAN_POINT('Ctrl Pts',(87.1471602095597,49.5899619007728,10.5953583212242));
#77361=CARTESIAN_POINT('Ctrl Pts',(87.203897118866,49.5851419552276,10.5634796281792));
#77362=CARTESIAN_POINT('Ctrl Pts',(87.2621673652706,49.5803220096824,10.5349792552796));
#77363=CARTESIAN_POINT('Ctrl Pts',(87.3204376116753,49.5755020641371,10.50647888238));
#77364=CARTESIAN_POINT('Ctrl Pts',(87.3802405748965,49.5706821185919,10.4813570068324));
#77365=CARTESIAN_POINT('Ctrl Pts',(87.4411435901739,49.5658621730467,10.4597501726755));
#77366=CARTESIAN_POINT('Ctrl Pts',(87.4464597044757,49.5654414486978,10.4578641511122));
#77367=CARTESIAN_POINT('Ctrl Pts',(87.4517852306617,49.5650207243489,10.4560045037934));
#77368=CARTESIAN_POINT('Ctrl Pts',(87.4571200021394,49.5646,10.4541712921126));
#77369=CARTESIAN_POINT('',(86.3679792906019,49.5646,11.6129461576271));
#77370=CARTESIAN_POINT('Origin',(88.011,49.5646,12.066));
#77371=CARTESIAN_POINT('',(86.3092266939895,49.5985899145734,12.0662160011593));
#77372=CARTESIAN_POINT('Ctrl Pts',(86.3679792906019,49.5646,11.6129461576271));
#77373=CARTESIAN_POINT('Ctrl Pts',(86.3470351830164,49.5704400412141,11.6889009322794));
#77374=CARTESIAN_POINT('Ctrl Pts',(86.3313737199885,49.5762800824281,11.7662671947601));
#77375=CARTESIAN_POINT('Ctrl Pts',(86.3211280276762,49.5821201236421,11.8443977600419));
#77376=CARTESIAN_POINT('Ctrl Pts',(86.3114965890295,49.5876100404708,11.9178442117801));
#77377=CARTESIAN_POINT('Ctrl Pts',(86.3066506132027,49.5930999572995,11.9919661813803));
#77378=CARTESIAN_POINT('Ctrl Pts',(86.3066600136595,49.5985898741282,12.0662157799485));
#77379=CARTESIAN_POINT('',(86.3073293460377,50.3923399468998,12.0666353777397));
#77380=CARTESIAN_POINT('Ctrl Pts',(86.3092810471104,49.5985899154299,12.0662160058438));
#77381=CARTESIAN_POINT('Ctrl Pts',(86.3121893889261,49.629264691781,12.4804454596203));
#77382=CARTESIAN_POINT('Ctrl Pts',(86.6701468888325,49.7019442162931,13.4633634721033));
#77383=CARTESIAN_POINT('Ctrl Pts',(88.3227306481849,49.8166284889665,14.0573743541845));
#77384=CARTESIAN_POINT('Ctrl Pts',(89.8516815299995,49.9426427334496,12.8834028378848));
#77385=CARTESIAN_POINT('Ctrl Pts',(89.696794108141,50.0686569779329,10.9633757853075));
#77386=CARTESIAN_POINT('Ctrl Pts',(87.9986885115237,50.1946712224162,10.0514601738819));
#77387=CARTESIAN_POINT('Ctrl Pts',(86.5545658312753,50.3025655349151,10.8497041618736));
#77388=CARTESIAN_POINT('Ctrl Pts',(86.310277298106,50.368455099253,11.7432630818391));
#77389=CARTESIAN_POINT('Ctrl Pts',(86.3092109631531,50.3923399154298,12.0666342497661));
#77390=CARTESIAN_POINT('',(86.3066604225581,51.1860899153758,12.0672001521734));
#77391=CARTESIAN_POINT('Ctrl Pts',(86.306660118584,50.3923399580925,12.0666357789217));
#77392=CARTESIAN_POINT('Ctrl Pts',(86.3066852637277,50.3973113147805,12.1340426553562));
#77393=CARTESIAN_POINT('Ctrl Pts',(86.3107135546021,50.4022826714685,12.2013277506436));
#77394=CARTESIAN_POINT('Ctrl Pts',(86.3186766764168,50.4072540281564,12.26803119575));
#77395=CARTESIAN_POINT('Ctrl Pts',(86.3266622759845,50.4122394176485,12.3349229267581));
#77396=CARTESIAN_POINT('Ctrl Pts',(86.3386048135703,50.4172248071405,12.4012293743328));
#77397=CARTESIAN_POINT('Ctrl Pts',(86.354385126363,50.4222101966325,12.4665021798249));
#77398=CARTESIAN_POINT('Ctrl Pts',(86.3702327072629,50.4272168377765,12.5320532293634));
#77399=CARTESIAN_POINT('Ctrl Pts',(86.3899506940518,50.4322234789205,12.5965614717567));
#77400=CARTESIAN_POINT('Ctrl Pts',(86.4133699848707,50.4372301200645,12.6595934386076));
#77401=CARTESIAN_POINT('Ctrl Pts',(86.4281351142681,50.4403866505038,12.6993331196222));
#77402=CARTESIAN_POINT('Ctrl Pts',(86.4443705175168,50.4435431809432,12.738486425967));
#77403=CARTESIAN_POINT('Ctrl Pts',(86.4620244619462,50.4466997113825,12.7769497999936));
#77404=CARTESIAN_POINT('Ctrl Pts',(86.4877325305886,50.4512963215923,12.8329610253403));
#77405=CARTESIAN_POINT('Ctrl Pts',(86.5165354926491,50.455892931802,12.8876913198559));
#77406=CARTESIAN_POINT('Ctrl Pts',(86.5482830806852,50.4604895420117,12.940776571217));
#77407=CARTESIAN_POINT('Ctrl Pts',(86.580579112399,50.4651655592556,12.9947788771415));
#77408=CARTESIAN_POINT('Ctrl Pts',(86.615922338754,50.4698415764995,13.0470782417727));
#77409=CARTESIAN_POINT('Ctrl Pts',(86.6541035914268,50.4745175937435,13.0973132269109));
#77410=CARTESIAN_POINT('Ctrl Pts',(86.6915330282512,50.4791015369032,13.1465590496897));
#77411=CARTESIAN_POINT('Ctrl Pts',(86.7316894162553,50.483685480063,13.1938206290306));
#77412=CARTESIAN_POINT('Ctrl Pts',(86.774331041167,50.4882694232228,13.2387850279821));
#77413=CARTESIAN_POINT('Ctrl Pts',(86.8169465414334,50.4928505580025,13.2837218792269));
#77414=CARTESIAN_POINT('Ctrl Pts',(86.8620439098941,50.4974316927822,13.3263639719743));
#77415=CARTESIAN_POINT('Ctrl Pts',(86.9093420809422,50.5020128275619,13.3664324915109));
#77416=CARTESIAN_POINT('Ctrl Pts',(86.9566286600696,50.5065928395888,13.4064911909827));
#77417=CARTESIAN_POINT('Ctrl Pts',(87.006114582701,50.5111728516158,13.4439772403373));
#77418=CARTESIAN_POINT('Ctrl Pts',(87.0574844918447,50.5157528636428,13.4786510578722));
#77419=CARTESIAN_POINT('Ctrl Pts',(87.110724638286,50.520499621328,13.5145872538671));
#77420=CARTESIAN_POINT('Ctrl Pts',(87.1659881523694,50.5252463790133,13.5475021178737));
#77421=CARTESIAN_POINT('Ctrl Pts',(87.2228918182155,50.5299931366985,13.5771784571666));
#77422=CARTESIAN_POINT('Ctrl Pts',(87.2778660422669,50.5345789453038,13.6058485560266));
#77423=CARTESIAN_POINT('Ctrl Pts',(87.3343704549797,50.539164753909,13.6314960940994));
#77424=CARTESIAN_POINT('Ctrl Pts',(87.3920374879344,50.5437505625142,13.6539736283256));
#77425=CARTESIAN_POINT('Ctrl Pts',(87.4527404486939,50.5485777947395,13.6776345106043));
#77426=CARTESIAN_POINT('Ctrl Pts',(87.5147312163883,50.5534050269647,13.6977821803525));
#77427=CARTESIAN_POINT('Ctrl Pts',(87.5775640365029,50.55823225919,13.7143046141862));
#77428=CARTESIAN_POINT('Ctrl Pts',(87.6403968566176,50.5630594914153,13.7308270480198));
#77429=CARTESIAN_POINT('Ctrl Pts',(87.7040710771906,50.5678867236405,13.743724193095));
#77430=CARTESIAN_POINT('Ctrl Pts',(87.7681330346237,50.5727139558658,13.7529470865231));
#77431=CARTESIAN_POINT('Ctrl Pts',(87.829144338054,50.5773113135149,13.76173078237));
#77432=CARTESIAN_POINT('Ctrl Pts',(87.8907579602646,50.5819086711641,13.7672183676022));
#77433=CARTESIAN_POINT('Ctrl Pts',(87.9525863601549,50.5865060288132,13.769338686897));
#77434=CARTESIAN_POINT('Ctrl Pts',(88.0154713713922,50.5911819526272,13.7714952412137));
#77435=CARTESIAN_POINT('Ctrl Pts',(88.0785780588376,50.5958578764412,13.7701681896364));
#77436=CARTESIAN_POINT('Ctrl Pts',(88.141489423131,50.6005338002552,13.7653373255628));
#77437=CARTESIAN_POINT('Ctrl Pts',(88.2031736195302,50.6051185141003,13.7606006937691));
#77438=CARTESIAN_POINT('Ctrl Pts',(88.2646695126617,50.6097032279454,13.7524957559121));
#77439=CARTESIAN_POINT('Ctrl Pts',(88.3255829859497,50.6142879417905,13.7410559335589));
#77440=CARTESIAN_POINT('Ctrl Pts',(88.3864592330113,50.6188698537662,13.7296231024574));
#77441=CARTESIAN_POINT('Ctrl Pts',(88.4467532667713,50.6234517657419,13.7148595218008));
#77442=CARTESIAN_POINT('Ctrl Pts',(88.5060783046827,50.6280336777176,13.6968501794563));
#77443=CARTESIAN_POINT('Ctrl Pts',(88.565388873419,50.6326144721806,13.6788452295291));
#77444=CARTESIAN_POINT('Ctrl Pts',(88.6237304286219,50.6371952666436,13.657596237216));
#77445=CARTESIAN_POINT('Ctrl Pts',(88.6807305571034,50.6417760611065,13.6332382768686));
#77446=CARTESIAN_POINT('Ctrl Pts',(88.73978652946,50.6465220727101,13.6080017893157));
#77447=CARTESIAN_POINT('Ctrl Pts',(88.7974019023001,50.6512680843136,13.5794279517199));
#77448=CARTESIAN_POINT('Ctrl Pts',(88.853186642118,50.6560140959171,13.5477207886231));
#77449=CARTESIAN_POINT('Ctrl Pts',(88.9070975956646,50.6606006909595,13.5170786559829));
#77450=CARTESIAN_POINT('Ctrl Pts',(88.9592985498954,50.6651872860019,13.4835107147741));
#77451=CARTESIAN_POINT('Ctrl Pts',(89.0094661784179,50.6697738810443,13.4472458601406));
#77452=CARTESIAN_POINT('Ctrl Pts',(89.0622493258862,50.6745996009284,13.40909031589));
#77453=CARTESIAN_POINT('Ctrl Pts',(89.1127808199414,50.6794253208125,13.3679493471259));
#77454=CARTESIAN_POINT('Ctrl Pts',(89.1607251442831,50.6842510406966,13.324136291585));
#77455=CARTESIAN_POINT('Ctrl Pts',(89.2086694686247,50.6890767605807,13.2803232360441));
#77456=CARTESIAN_POINT('Ctrl Pts',(89.2540262262617,50.6939024804649,13.2338386112796));
#77457=CARTESIAN_POINT('Ctrl Pts',(89.2965084889806,50.698728200349,13.1850365321824));
#77458=CARTESIAN_POINT('Ctrl Pts',(89.3369799397171,50.7033255045427,13.1385444007935));
#77459=CARTESIAN_POINT('Ctrl Pts',(89.3750090047662,50.7079228087365,13.0897584870719));
#77460=CARTESIAN_POINT('Ctrl Pts',(89.4103257087688,50.7125201129303,13.0389657734878));
#77461=CARTESIAN_POINT('Ctrl Pts',(89.4462464236706,50.7171960434262,12.9873043674968));
#77462=CARTESIAN_POINT('Ctrl Pts',(89.4793607081385,50.7218719739221,12.9335672105246));
#77463=CARTESIAN_POINT('Ctrl Pts',(89.5094254032387,50.726547904418,12.8780936808823));
#77464=CARTESIAN_POINT('Ctrl Pts',(89.538903282671,50.7311325680886,12.8237029074841));
#77465=CARTESIAN_POINT('Ctrl Pts',(89.5654492955193,50.7357172317592,12.7676434039417));
#77466=CARTESIAN_POINT('Ctrl Pts',(89.5888777580777,50.7403018954297,12.7102643992676));
#77467=CARTESIAN_POINT('Ctrl Pts',(89.6122919095732,50.7448837586003,12.6529204440358));
#77468=CARTESIAN_POINT('Ctrl Pts',(89.6325920947704,50.7494656217708,12.5942590561464));
#77469=CARTESIAN_POINT('Ctrl Pts',(89.6496399301992,50.7540474849414,12.5346512720102));
#77470=CARTESIAN_POINT('Ctrl Pts',(89.6666836130879,50.758628232054,12.4750580072374));
#77471=CARTESIAN_POINT('Ctrl Pts',(89.6804763789678,50.7632089791667,12.4145192930305));
#77472=CARTESIAN_POINT('Ctrl Pts',(89.6909297172832,50.7677897262794,12.3534212598063));
#77473=CARTESIAN_POINT('Ctrl Pts',(89.7017603019815,50.7725357861588,12.2901182838805));
#77474=CARTESIAN_POINT('Ctrl Pts',(89.709005657291,50.7772818460382,12.2262154088906));
#77475=CARTESIAN_POINT('Ctrl Pts',(89.7126256410867,50.7820279059176,12.1621509916559));
#77476=CARTESIAN_POINT('Ctrl Pts',(89.7161239626396,50.7866144578209,12.1002396836941));
#77477=CARTESIAN_POINT('Ctrl Pts',(89.7162368207152,50.7912010097241,12.0381780483506));
#77478=CARTESIAN_POINT('Ctrl Pts',(89.7129811514963,50.7957875616274,11.9763618632993));
#77479=CARTESIAN_POINT('Ctrl Pts',(89.7095556471097,50.8006133754949,11.911320976518));
#77480=CARTESIAN_POINT('Ctrl Pts',(89.7024006033697,50.8054391893624,11.8465524909059));
#77481=CARTESIAN_POINT('Ctrl Pts',(89.6915972956155,50.8102650032298,11.7825082619017));
#77482=CARTESIAN_POINT('Ctrl Pts',(89.6807939878612,50.8150908170973,11.7184640328975));
#77483=CARTESIAN_POINT('Ctrl Pts',(89.6663426356459,50.8199166309648,11.6551446748319));
#77484=CARTESIAN_POINT('Ctrl Pts',(89.6483851321419,50.8247424448323,11.5929833357685));
#77485=CARTESIAN_POINT('Ctrl Pts',(89.6312785310761,50.8293395912357,11.533767463761));
#77486=CARTESIAN_POINT('Ctrl Pts',(89.6109203559465,50.8339367376392,11.475359179951));
#77487=CARTESIAN_POINT('Ctrl Pts',(89.5874052368878,50.8385338840426,11.4181409376162));
#77488=CARTESIAN_POINT('Ctrl Pts',(89.5634870240488,50.8432098342623,11.3599418659886));
#77489=CARTESIAN_POINT('Ctrl Pts',(89.5363026713531,50.847885784482,11.3029745552547));
#77490=CARTESIAN_POINT('Ctrl Pts',(89.5060053913801,50.8525617347017,11.2476273982199));
#77491=CARTESIAN_POINT('Ctrl Pts',(89.4763006636678,50.8571462329866,11.1933627173364));
#77492=CARTESIAN_POINT('Ctrl Pts',(89.4436039334705,50.8617307312715,11.1406558549161));
#77493=CARTESIAN_POINT('Ctrl Pts',(89.4081078498387,50.8663152295564,11.0898522184018));
#77494=CARTESIAN_POINT('Ctrl Pts',(89.3726334678097,50.8708969249698,11.0390796422251));
#77495=CARTESIAN_POINT('Ctrl Pts',(89.3343634168964,50.8754786203832,10.9902084011517));
#77496=CARTESIAN_POINT('Ctrl Pts',(89.2935343242799,50.8800603157966,10.9435559957647));
#77497=CARTESIAN_POINT('Ctrl Pts',(89.2527151959571,50.8846408930524,10.8969149758442));
#77498=CARTESIAN_POINT('Ctrl Pts',(89.2093386008289,50.8892214703083,10.8524920995507));
#77499=CARTESIAN_POINT('Ctrl Pts',(89.1636808995905,50.8938020475641,10.810571157206));
#77500=CARTESIAN_POINT('Ctrl Pts',(89.1163721240079,50.89854826771,10.7671342692373));
#77501=CARTESIAN_POINT('Ctrl Pts',(89.0666144868449,50.903294487856,10.7263841734061));
#77502=CARTESIAN_POINT('Ctrl Pts',(89.0147545343136,50.9080407080019,10.6885924094717));
#77503=CARTESIAN_POINT('Ctrl Pts',(88.9646411013919,50.9126270867645,10.6520733820822));
#77504=CARTESIAN_POINT('Ctrl Pts',(88.9125651954624,50.917213465527,10.618316808786));
#77505=CARTESIAN_POINT('Ctrl Pts',(88.8588684810597,50.9217998442895,10.5875231234728));
#77506=CARTESIAN_POINT('Ctrl Pts',(88.8023646640735,50.9266259851272,10.555119636991));
#77507=CARTESIAN_POINT('Ctrl Pts',(88.7440664965507,50.9314521259648,10.525997620887));
#77508=CARTESIAN_POINT('Ctrl Pts',(88.6843977849398,50.9362782668025,10.500333924862));
#77509=CARTESIAN_POINT('Ctrl Pts',(88.6247290733289,50.9411044076401,10.4746702288369));
#77510=CARTESIAN_POINT('Ctrl Pts',(88.5636904532144,50.9459305484778,10.4524650017373));
#77511=CARTESIAN_POINT('Ctrl Pts',(88.5017229000459,50.9507566893155,10.4338339940525));
#77512=CARTESIAN_POINT('Ctrl Pts',(88.4426943609331,50.9553539346258,10.4160866228946));
#77513=CARTESIAN_POINT('Ctrl Pts',(88.3825806479584,50.9599511799362,10.4015091716729));
#77514=CARTESIAN_POINT('Ctrl Pts',(88.3217544155937,50.9645484252466,10.3902295715734));
#77515=CARTESIAN_POINT('Ctrl Pts',(88.2598870007897,50.9692243631029,10.3787568948836));
#77516=CARTESIAN_POINT('Ctrl Pts',(88.1972829246974,50.9739003009593,10.3706962760495));
#77517=CARTESIAN_POINT('Ctrl Pts',(88.1343515751703,50.9785762388156,10.3661296447955));
#77518=CARTESIAN_POINT('Ctrl Pts',(88.0726494942767,50.9831608393054,10.3616522157691));
#77519=CARTESIAN_POINT('Ctrl Pts',(88.0106333425797,50.9877454397952,10.3605335406842));
#77520=CARTESIAN_POINT('Ctrl Pts',(87.9486978124994,50.992330040285,10.3627991096078));
#77521=CARTESIAN_POINT('Ctrl Pts',(87.8868001349848,50.9969118388469,10.3650632939047));
#77522=CARTESIAN_POINT('Ctrl Pts',(87.824983489032,51.0014936374087,10.370707602465));
#77523=CARTESIAN_POINT('Ctrl Pts',(87.7636429740228,51.0060754359706,10.3797054417156));
#77524=CARTESIAN_POINT('Ctrl Pts',(87.7023174183853,51.0106561171498,10.3887010866249));
#77525=CARTESIAN_POINT('Ctrl Pts',(87.6414682666095,51.015236798329,10.401048564842));
#77526=CARTESIAN_POINT('Ctrl Pts',(87.5814838475592,51.0198174795082,10.4166696175743));
#77527=CARTESIAN_POINT('Ctrl Pts',(87.5193329771451,51.0245636006991,10.4328548543319));
#77528=CARTESIAN_POINT('Ctrl Pts',(87.4581110767645,51.0293097218899,10.4525545699957));
#77529=CARTESIAN_POINT('Ctrl Pts',(87.3982341983022,51.0340558430808,10.4756249159806));
#77530=CARTESIAN_POINT('Ctrl Pts',(87.3403713037556,51.0386423264952,10.4979192812041));
#77531=CARTESIAN_POINT('Ctrl Pts',(87.2837648329454,51.0432288099096,10.523360834546));
#77532=CARTESIAN_POINT('Ctrl Pts',(87.2287685056506,51.047815293324,10.5517712442144));
#77533=CARTESIAN_POINT('Ctrl Pts',(87.1709008636871,51.0526412334031,10.5816649388591));
#77534=CARTESIAN_POINT('Ctrl Pts',(87.1148166627409,51.0574671734822,10.6148456730932));
#77535=CARTESIAN_POINT('Ctrl Pts',(87.0608942929944,51.0622931135613,10.6510533645697));
#77536=CARTESIAN_POINT('Ctrl Pts',(87.006971923248,51.0671190536405,10.6872610560462));
#77537=CARTESIAN_POINT('Ctrl Pts',(86.9552118543247,51.0719449937196,10.7264952517081));
#77538=CARTESIAN_POINT('Ctrl Pts',(86.9059504698246,51.0767709337987,10.7684483164594));
#77539=CARTESIAN_POINT('Ctrl Pts',(86.8594551730849,51.0813258913644,10.808045664657));
#77540=CARTESIAN_POINT('Ctrl Pts',(86.814981848768,51.0858808489301,10.8502384811275));
#77541=CARTESIAN_POINT('Ctrl Pts',(86.7728402917496,51.0904358064958,10.894788929157));
#77542=CARTESIAN_POINT('Ctrl Pts',(86.7309866254985,51.094959646791,10.939035030039));
#77543=CARTESIAN_POINT('Ctrl Pts',(86.691433367289,51.0994834870863,10.9856063034794));
#77544=CARTESIAN_POINT('Ctrl Pts',(86.6544517062852,51.1040073273815,11.0342289195663));
#77545=CARTESIAN_POINT('Ctrl Pts',(86.6175059510488,51.1085267754468,11.0828043275966));
#77546=CARTESIAN_POINT('Ctrl Pts',(86.5831271644513,51.1130462235121,11.1334267183578));
#77547=CARTESIAN_POINT('Ctrl Pts',(86.5515477123081,51.1175656715774,11.1857876077042));
#77548=CARTESIAN_POINT('Ctrl Pts',(86.5199865423486,51.1220825032142,11.2381181839411));
#77549=CARTESIAN_POINT('Ctrl Pts',(86.4912217654906,51.126599334851,11.2921848154484));
#77550=CARTESIAN_POINT('Ctrl Pts',(86.4654423658546,51.1311161664877,11.3476502000175));
#77551=CARTESIAN_POINT('Ctrl Pts',(86.4392958994072,51.1356973122284,11.403905343159));
#77552=CARTESIAN_POINT('Ctrl Pts',(86.4162207877119,51.1402784579691,11.4615989149807));
#77553=CARTESIAN_POINT('Ctrl Pts',(86.3963648395834,51.1448596037098,11.5203553039326));
#77554=CARTESIAN_POINT('Ctrl Pts',(86.3767772798433,51.149378827133,11.5783174959802));
#77555=CARTESIAN_POINT('Ctrl Pts',(86.3603224833752,51.1538980505563,11.6373134175068));
#77556=CARTESIAN_POINT('Ctrl Pts',(86.34709206766,51.1584172739796,11.696967171791));
#77557=CARTESIAN_POINT('Ctrl Pts',(86.3335897275704,51.163029380879,11.7578469880641));
#77558=CARTESIAN_POINT('Ctrl Pts',(86.3234459251632,51.1676414877784,11.8194114230928));
#77559=CARTESIAN_POINT('Ctrl Pts',(86.3167026929446,51.1722535946777,11.8812529542731));
#77560=CARTESIAN_POINT('Ctrl Pts',(86.309959460726,51.1768657015771,11.9430944854533));
#77561=CARTESIAN_POINT('Ctrl Pts',(86.3066167724698,51.1814778084765,12.0052125352787));
#77562=CARTESIAN_POINT('Ctrl Pts',(86.3066604225581,51.1860899153758,12.0672001521734));
#77563=CARTESIAN_POINT('',(86.3066605642293,51.9798399154705,12.0646131774589));
#77564=CARTESIAN_POINT('Ctrl Pts',(86.3066604225586,51.1860899154298,12.0672001528987));
#77565=CARTESIAN_POINT('Ctrl Pts',(86.3067130919174,51.1916550030472,12.1419960166398));
#77566=CARTESIAN_POINT('Ctrl Pts',(86.3116895962548,51.1972200906646,12.2166201618318));
#77567=CARTESIAN_POINT('Ctrl Pts',(86.3215218299453,51.202785178282,12.2905848358831));
#77568=CARTESIAN_POINT('Ctrl Pts',(86.3296440530645,51.2073823923769,12.3516856604259));
#77569=CARTESIAN_POINT('Ctrl Pts',(86.3411018368618,51.2119796064718,12.4124707301463));
#77570=CARTESIAN_POINT('Ctrl Pts',(86.355858390661,51.2165768205668,12.4725477691915));
#77571=CARTESIAN_POINT('Ctrl Pts',(86.370867651638,51.221252762325,12.5336536323914));
#77572=CARTESIAN_POINT('Ctrl Pts',(86.3892897538642,51.2259287040833,12.5940264482924));
#77573=CARTESIAN_POINT('Ctrl Pts',(86.4110308607976,51.2306046458416,12.6532593883454));
#77574=CARTESIAN_POINT('Ctrl Pts',(86.4323471215974,51.2351892143417,12.7113348488997));
#77575=CARTESIAN_POINT('Ctrl Pts',(86.4568536557395,51.2397737828418,12.7683140811023));
#77576=CARTESIAN_POINT('Ctrl Pts',(86.4844112400724,51.2443583513419,12.8238268889811));
#77577=CARTESIAN_POINT('Ctrl Pts',(86.5119519809785,51.2489401177153,12.8793057669658));
#77578=CARTESIAN_POINT('Ctrl Pts',(86.5425398485158,51.2535218840886,12.9333195428286));
#77579=CARTESIAN_POINT('Ctrl Pts',(86.575987984843,51.258103650462,12.9855190873251));
#77580=CARTESIAN_POINT('Ctrl Pts',(86.6094279629091,51.2626842993068,13.0377058999458));
#77581=CARTESIAN_POINT('Ctrl Pts',(86.645726550323,51.2672649481516,13.0880789312246));
#77582=CARTESIAN_POINT('Ctrl Pts',(86.6846525901919,51.2718455969964,13.1363164878181));
#77583=CARTESIAN_POINT('Ctrl Pts',(86.7249850657803,51.2765917491438,13.1862969142964));
#77584=CARTESIAN_POINT('Ctrl Pts',(86.7681381789869,51.2813379012912,13.2339841049719));
#77585=CARTESIAN_POINT('Ctrl Pts',(86.8138095736111,51.2860840534386,13.2790580854034));
#77586=CARTESIAN_POINT('Ctrl Pts',(86.8579441928296,51.2906705045312,13.3226153925403));
#77587=CARTESIAN_POINT('Ctrl Pts',(86.9044298579653,51.2952569556239,13.3637322733405));
#77588=CARTESIAN_POINT('Ctrl Pts',(86.9529584541405,51.2998434067166,13.4021597669572));
#77589=CARTESIAN_POINT('Ctrl Pts',(87.0040217120299,51.3046694093913,13.4425943389673));
#77590=CARTESIAN_POINT('Ctrl Pts',(87.0573466385354,51.3094954120661,13.4800505052685));
#77591=CARTESIAN_POINT('Ctrl Pts',(87.1125404367764,51.3143214147408,13.5142904573503));
#77592=CARTESIAN_POINT('Ctrl Pts',(87.1677342350173,51.3191474174155,13.5485304094321));
#77593=CARTESIAN_POINT('Ctrl Pts',(87.2247962987226,51.3239734200903,13.5795539057566));
#77594=CARTESIAN_POINT('Ctrl Pts',(87.2833077818663,51.328799422765,13.6071809988667));
#77595=CARTESIAN_POINT('Ctrl Pts',(87.3390455384296,51.3333966496307,13.6334984344808));
#77596=CARTESIAN_POINT('Ctrl Pts',(87.3963272293104,51.3379938764964,13.6568423081311));
#77597=CARTESIAN_POINT('Ctrl Pts',(87.4548033372498,51.3425911033621,13.677030759466));
#77598=CARTESIAN_POINT('Ctrl Pts',(87.5142806677395,51.347267043524,13.6975648756108));
#77599=CARTESIAN_POINT('Ctrl Pts',(87.5749932626738,51.3519429836859,13.7148341864651));
#77600=CARTESIAN_POINT('Ctrl Pts',(87.6365484410715,51.3566189238478,13.7286968652211));
#77601=CARTESIAN_POINT('Ctrl Pts',(87.6969009554397,51.3612035055703,13.7422886951951));
#77602=CARTESIAN_POINT('Ctrl Pts',(87.7580629042249,51.3657880872928,13.7526056961669));
#77603=CARTESIAN_POINT('Ctrl Pts',(87.8196477612758,51.3703726690154,13.7595640396322));
#77604=CARTESIAN_POINT('Ctrl Pts',(87.8811949790187,51.3749544487425,13.7665181303112));
#77605=CARTESIAN_POINT('Ctrl Pts',(87.943164087736,51.3795362284697,13.770117576732));
#77606=CARTESIAN_POINT('Ctrl Pts',(88.005160423092,51.3841180081969,13.770329995905));
#77607=CARTESIAN_POINT('Ctrl Pts',(88.0671416385854,51.3886986705051,13.7705423632726));
#77608=CARTESIAN_POINT('Ctrl Pts',(88.1291495587205,51.3932793328133,13.7673693414617));
#77609=CARTESIAN_POINT('Ctrl Pts',(88.1907885410593,51.3978599951215,13.7608306452574));
#77610=CARTESIAN_POINT('Ctrl Pts',(88.2546542398407,51.4026061344654,13.7540557377823));
#77611=CARTESIAN_POINT('Ctrl Pts',(88.3181232497171,51.4073522738093,13.7436673270672));
#77612=CARTESIAN_POINT('Ctrl Pts',(88.3807627611592,51.4120984131532,13.7297458748439));
#77613=CARTESIAN_POINT('Ctrl Pts',(88.4412948875003,51.4166848778268,13.7162927829305));
#77614=CARTESIAN_POINT('Ctrl Pts',(88.5010519575863,51.4212713425004,13.6995408265212));
#77615=CARTESIAN_POINT('Ctrl Pts',(88.5596576912754,51.4258578071739,13.6796138241241));
#77616=CARTESIAN_POINT('Ctrl Pts',(88.6213239035269,51.430683783853,13.6586462040295));
#77617=CARTESIAN_POINT('Ctrl Pts',(88.6817146322155,51.4355097605321,13.634163065632));
#77618=CARTESIAN_POINT('Ctrl Pts',(88.7404170450196,51.4403357372112,13.6063654144504));
#77619=CARTESIAN_POINT('Ctrl Pts',(88.7991194578237,51.4451617138903,13.5785677632688));
#77620=CARTESIAN_POINT('Ctrl Pts',(88.8561330230062,51.4499876905693,13.5474559776151));
#77621=CARTESIAN_POINT('Ctrl Pts',(88.9110793882464,51.4548136672484,13.513284329513));
#77622=CARTESIAN_POINT('Ctrl Pts',(88.9634212821718,51.4594108914382,13.4807324259905));
#77623=CARTESIAN_POINT('Ctrl Pts',(89.0141024548446,51.464008115628,13.4452705771532));
#77624=CARTESIAN_POINT('Ctrl Pts',(89.0627805440023,51.4686053398177,13.4070937785473));
#77625=CARTESIAN_POINT('Ctrl Pts',(89.1122921272935,51.4732812803141,13.3682632949215));
#77626=CARTESIAN_POINT('Ctrl Pts',(89.1597308850862,51.4779572208106,13.326624211991));
#77627=CARTESIAN_POINT('Ctrl Pts',(89.2047646755216,51.482633161307,13.2824295027155));
#77628=CARTESIAN_POINT('Ctrl Pts',(89.2489185673613,51.4872177403293,13.239098297539));
#77629=CARTESIAN_POINT('Ctrl Pts',(89.2907602454635,51.4918023193517,13.1933108083627));
#77630=CARTESIAN_POINT('Ctrl Pts',(89.3300096325757,51.496386898374,13.1453462951123));
#77631=CARTESIAN_POINT('Ctrl Pts',(89.369235031301,51.5009686753996,13.0974110967477));
#77632=CARTESIAN_POINT('Ctrl Pts',(89.4058709588722,51.5055504524252,13.047301905739));
#77633=CARTESIAN_POINT('Ctrl Pts',(89.4396761443467,51.5101322294508,12.9953327230732));
#77634=CARTESIAN_POINT('Ctrl Pts',(89.4734730853234,51.5147128890605,12.9433762147888));
#77635=CARTESIAN_POINT('Ctrl Pts',(89.5044403772444,51.5192935486702,12.8895610418726));
#77636=CARTESIAN_POINT('Ctrl Pts',(89.5323799870813,51.5238742082799,12.8342302848161));
#77637=CARTESIAN_POINT('Ctrl Pts',(89.561328952019,51.5286203502342,12.7769006314902));
#77638=CARTESIAN_POINT('Ctrl Pts',(89.5870269692947,51.5333664921885,12.7179442826247));
#77639=CARTESIAN_POINT('Ctrl Pts',(89.609306880766,51.5381126341428,12.6577684940041));
#77640=CARTESIAN_POINT('Ctrl Pts',(89.6308372034223,51.5426990961573,12.5996172689975));
#77641=CARTESIAN_POINT('Ctrl Pts',(89.6491756941917,51.5472855581717,12.5403278862145));
#77642=CARTESIAN_POINT('Ctrl Pts',(89.6642222819317,51.5518720201862,12.4802836252188));
#77643=CARTESIAN_POINT('Ctrl Pts',(89.6800546512452,51.5566980021104,12.4171036583279));
#77644=CARTESIAN_POINT('Ctrl Pts',(89.692241730495,51.5615239840347,12.3530884374176));
#77645=CARTESIAN_POINT('Ctrl Pts',(89.7007284689377,51.5663499659589,12.2886938186422));
#77646=CARTESIAN_POINT('Ctrl Pts',(89.7092152073804,51.5711759478831,12.2242991998668));
#77647=CARTESIAN_POINT('Ctrl Pts',(89.7140016344315,51.5760019298073,12.1595258351518));
#77648=CARTESIAN_POINT('Ctrl Pts',(89.715096151996,51.5808279117316,12.0948295048961));
#77649=CARTESIAN_POINT('Ctrl Pts',(89.7161387876291,51.5854251341817,12.0331998870144));
#77650=CARTESIAN_POINT('Ctrl Pts',(89.7138359464523,51.5900223566319,11.9713871243631));
#77651=CARTESIAN_POINT('Ctrl Pts',(89.7081657511357,51.594619579082,11.9097846077624));
#77652=CARTESIAN_POINT('Ctrl Pts',(89.7023984650355,51.5992955197959,11.8471272709525));
#77653=CARTESIAN_POINT('Ctrl Pts',(89.6931473169984,51.6039714605098,11.784687976654));
#77654=CARTESIAN_POINT('Ctrl Pts',(89.6804446813148,51.6086474012236,11.7228829767708));
#77655=CARTESIAN_POINT('Ctrl Pts',(89.6679902433133,51.6132319784067,11.6622855890788));
#77656=CARTESIAN_POINT('Ctrl Pts',(89.6522180897161,51.6178165555898,11.6022984541811));
#77657=CARTESIAN_POINT('Ctrl Pts',(89.6332109188214,51.6224011327728,11.5433083409346));
#77658=CARTESIAN_POINT('Ctrl Pts',(89.6142153648411,51.6269829079271,11.484354281612));
#77659=CARTESIAN_POINT('Ctrl Pts',(89.591988869851,51.6315646830813,11.4263965191688));
#77660=CARTESIAN_POINT('Ctrl Pts',(89.5666643673551,51.6361464582355,11.3698080640071));
#77661=CARTESIAN_POINT('Ctrl Pts',(89.5413460412288,51.6407271159449,11.3132334101515));
#77662=CARTESIAN_POINT('Ctrl Pts',(89.5129314153614,51.6453077736542,11.2580278650513));
#77663=CARTESIAN_POINT('Ctrl Pts',(89.4816013057684,51.6498884313635,11.2045438867405));
#77664=CARTESIAN_POINT('Ctrl Pts',(89.449139329153,51.6546345751011,11.1491276856553));
#77665=CARTESIAN_POINT('Ctrl Pts',(89.4135474179629,51.6593807188387,11.0955603575894));
#77666=CARTESIAN_POINT('Ctrl Pts',(89.3750770503391,51.6641268625764,11.0442032313917));
#77667=CARTESIAN_POINT('Ctrl Pts',(89.3379010155446,51.6687133226397,10.9945740121148));
#77668=CARTESIAN_POINT('Ctrl Pts',(89.2980375462268,51.6732997827031,10.9470089810368));
#77669=CARTESIAN_POINT('Ctrl Pts',(89.2557543649582,51.6778862427664,10.901800100276));
#77670=CARTESIAN_POINT('Ctrl Pts',(89.2112629663549,51.6827122283411,10.8542302090333));
#77671=CARTESIAN_POINT('Ctrl Pts',(89.1640926474987,51.6875382139159,10.8092697662519));
#77672=CARTESIAN_POINT('Ctrl Pts',(89.1145965243496,51.6923641994907,10.7672122779132));
#77673=CARTESIAN_POINT('Ctrl Pts',(89.0651004012004,51.6971901850654,10.7251547895744));
#77674=CARTESIAN_POINT('Ctrl Pts',(89.0132790374135,51.7020161706401,10.6860005845717));
#77675=CARTESIAN_POINT('Ctrl Pts',(88.9595199021039,51.7068421562149,10.6499898196295));
#77676=CARTESIAN_POINT('Ctrl Pts',(88.9083090589371,51.7114393802768,10.6156860380462));
#77677=CARTESIAN_POINT('Ctrl Pts',(88.8551297687583,51.7160366043387,10.5840935275524));
#77678=CARTESIAN_POINT('Ctrl Pts',(88.8003006616581,51.7206338284007,10.5554440423784));
#77679=CARTESIAN_POINT('Ctrl Pts',(88.7445327374292,51.7253097689131,10.5263040033941));
#77680=CARTESIAN_POINT('Ctrl Pts',(88.6870583538989,51.7299857094255,10.5002090968762));
#77681=CARTESIAN_POINT('Ctrl Pts',(88.6282447727882,51.7346616499378,10.4773578986865));
#77682=CARTESIAN_POINT('Ctrl Pts',(88.5705803308158,51.7392462287928,10.4549531825118));
#77683=CARTESIAN_POINT('Ctrl Pts',(88.511629050097,51.7438308076477,10.4356667523341));
#77684=CARTESIAN_POINT('Ctrl Pts',(88.4517607190889,51.7484153865026,10.4196389144212));
#77685=CARTESIAN_POINT('Ctrl Pts',(88.3919289785141,51.7529971633465,10.4036208724309));
#77686=CARTESIAN_POINT('Ctrl Pts',(88.3311817897196,51.7575789401903,10.3908576050375));
#77687=CARTESIAN_POINT('Ctrl Pts',(88.2699046298808,51.7621607170341,10.3814397522717));
#77688=CARTESIAN_POINT('Ctrl Pts',(88.2086424146661,51.7667413764481,10.3720241963857));
#77689=CARTESIAN_POINT('Ctrl Pts',(88.1468509879067,51.7713220358619,10.3659525127385));
#77690=CARTESIAN_POINT('Ctrl Pts',(88.0849245316919,51.7759026952759,10.363263966666));
#77691=CARTESIAN_POINT('Ctrl Pts',(88.0207608959499,51.7806488373944,10.36047829312));
#77692=CARTESIAN_POINT('Ctrl Pts',(87.9564528657858,51.7853949795129,10.3613249675671));
#77693=CARTESIAN_POINT('Ctrl Pts',(87.8924404019637,51.7901411216314,10.3657887021569));
#77694=CARTESIAN_POINT('Ctrl Pts',(87.8305815886813,51.794727583417,10.3701022577997));
#77695=CARTESIAN_POINT('Ctrl Pts',(87.768999282998,51.7993140452026,10.3777931994341));
#77696=CARTESIAN_POINT('Ctrl Pts',(87.7080839810922,51.8039005069881,10.3887949674864));
#77697=CARTESIAN_POINT('Ctrl Pts',(87.6439874767223,51.8087264892731,10.4003712849629));
#77698=CARTESIAN_POINT('Ctrl Pts',(87.5806301815173,51.8135524715581,10.4156135763098));
#77699=CARTESIAN_POINT('Ctrl Pts',(87.5184502046144,51.8183784538431,10.4343843790078));
#77700=CARTESIAN_POINT('Ctrl Pts',(87.4562702277115,51.8232044361281,10.4531551817058));
#77701=CARTESIAN_POINT('Ctrl Pts',(87.3952681511434,51.8280304184131,10.4754542006095));
#77702=CARTESIAN_POINT('Ctrl Pts',(87.3358558974417,51.832856400698,10.5010861760529));
#77703=CARTESIAN_POINT('Ctrl Pts',(87.2792598719986,51.8374536243207,10.5255031581393));
#77704=CARTESIAN_POINT('Ctrl Pts',(87.2238739591252,51.8420508479433,10.5530444637661));
#77705=CARTESIAN_POINT('Ctrl Pts',(87.1700656849818,51.8466480715659,10.5835681083352));
#77706=CARTESIAN_POINT('Ctrl Pts',(87.1153360671562,51.8513240121332,10.6146144005367));
#77707=CARTESIAN_POINT('Ctrl Pts',(87.0622391480133,51.8559999527005,10.6487460015799));
#77708=CARTESIAN_POINT('Ctrl Pts',(87.0111409577233,51.8606758932678,10.6857620744316));
#77709=CARTESIAN_POINT('Ctrl Pts',(86.9610411635716,51.8652604716757,10.7220548984953));
#77710=CARTESIAN_POINT('Ctrl Pts',(86.9128631272666,51.8698450500836,10.7611201770715));
#77711=CARTESIAN_POINT('Ctrl Pts',(86.8669252958447,51.8744296284915,10.8027233450617));
#77712=CARTESIAN_POINT('Ctrl Pts',(86.8210155408074,51.8790114048868,10.8443010859365));
#77713=CARTESIAN_POINT('Ctrl Pts',(86.7773436523091,51.883593181282,10.8884132995929));
#77714=CARTESIAN_POINT('Ctrl Pts',(86.7361948612738,51.8881749576772,10.9347853015995));
#77715=CARTESIAN_POINT('Ctrl Pts',(86.6950561058497,51.8927556166417,10.9811459941273));
#77716=CARTESIAN_POINT('Ctrl Pts',(86.6564395640461,51.8973362756061,11.029765000343));
#77717=CARTESIAN_POINT('Ctrl Pts',(86.6205920273553,51.9019169345705,11.0803324570597));
#77718=CARTESIAN_POINT('Ctrl Pts',(86.5834494414185,51.9066630771214,11.1327267435319));
#77719=CARTESIAN_POINT('Ctrl Pts',(86.5492801490811,51.9114092196723,11.1872125204093));
#77720=CARTESIAN_POINT('Ctrl Pts',(86.5183099409665,51.9161553622232,11.2434118750781));
#77721=CARTESIAN_POINT('Ctrl Pts',(86.4883817075303,51.9207418235624,11.2977204350745));
#77722=CARTESIAN_POINT('Ctrl Pts',(86.4614408643829,51.9253282849016,11.3536285849229));
#77723=CARTESIAN_POINT('Ctrl Pts',(86.4376432980279,51.9299147462408,11.4107721587422));
#77724=CARTESIAN_POINT('Ctrl Pts',(86.4126029355551,51.9347407293975,11.4708999793805));
#77725=CARTESIAN_POINT('Ctrl Pts',(86.391043382755,51.9395667125543,11.5323951949942));
#77726=CARTESIAN_POINT('Ctrl Pts',(86.3730867843619,51.944392695711,11.5948151810192));
#77727=CARTESIAN_POINT('Ctrl Pts',(86.3551301859688,51.9492186788678,11.6572351670442));
#77728=CARTESIAN_POINT('Ctrl Pts',(86.3407766097187,51.9540446620245,11.7205792744149));
#77729=CARTESIAN_POINT('Ctrl Pts',(86.3300854400862,51.9588706451812,11.7843955293858));
#77730=CARTESIAN_POINT('Ctrl Pts',(86.3146007869758,51.9658604019308,11.8768243846938));
#77731=CARTESIAN_POINT('Ctrl Pts',(86.3067370918222,51.9728501586803,11.9705644153934));
#77732=CARTESIAN_POINT('Ctrl Pts',(86.3066605642297,51.9798399154299,12.064613176913));
#77733=CARTESIAN_POINT('',(86.3066600304637,52.7735899153848,12.0656777559288));
#77734=CARTESIAN_POINT('Ctrl Pts',(86.3066605642293,51.9798399154705,12.0646131774589));
#77735=CARTESIAN_POINT('Ctrl Pts',(86.3066110592266,51.9843615272388,12.1254524887725));
#77736=CARTESIAN_POINT('Ctrl Pts',(86.3098234268039,51.9888831390072,12.1864087974373));
#77737=CARTESIAN_POINT('Ctrl Pts',(86.3163087196424,51.9934047507755,12.2470974872272));
#77738=CARTESIAN_POINT('Ctrl Pts',(86.3227874283413,51.9979217720151,12.3077245633292));
#77739=CARTESIAN_POINT('Ctrl Pts',(86.3325324283883,52.0024387932547,12.3680840389148));
#77740=CARTESIAN_POINT('Ctrl Pts',(86.345502752508,52.0069558144942,12.4277924186555));
#77741=CARTESIAN_POINT('Ctrl Pts',(86.3584650054124,52.0114700248672,12.4874636428725));
#77742=CARTESIAN_POINT('Ctrl Pts',(86.3746484952788,52.0159842352402,12.5464840613476));
#77743=CARTESIAN_POINT('Ctrl Pts',(86.393960872915,52.0204984456132,12.6044786876713));
#77744=CARTESIAN_POINT('Ctrl Pts',(86.4132688196422,52.0250116202745,12.662460008077));
#77745=CARTESIAN_POINT('Ctrl Pts',(86.435704063534,52.0295247949358,12.7194155048757));
#77746=CARTESIAN_POINT('Ctrl Pts',(86.4611245850067,52.0340379695971,12.7749859191827));
#77747=CARTESIAN_POINT('Ctrl Pts',(86.4865669549605,52.0385550232509,12.8306040952616));
#77748=CARTESIAN_POINT('Ctrl Pts',(86.5149995091763,52.0430720769047,12.8848343315321));
#77749=CARTESIAN_POINT('Ctrl Pts',(86.5462328952534,52.0475891305585,12.9373392935316));
#77750=CARTESIAN_POINT('Ctrl Pts',(86.5774796251288,52.0521081140271,12.9898666871568));
#77751=CARTESIAN_POINT('Ctrl Pts',(86.6115292756043,52.0566270974958,13.0406669021523));
#77752=CARTESIAN_POINT('Ctrl Pts',(86.6481492710332,52.0611460809645,13.0894318375713));
#77753=CARTESIAN_POINT('Ctrl Pts',(86.6848359186587,52.0656732894526,13.1382855302397));
#77754=CARTESIAN_POINT('Ctrl Pts',(86.7241019130956,52.0702004979407,13.185096144303));
#77755=CARTESIAN_POINT('Ctrl Pts',(86.7656752921718,52.0747277064288,13.2295897935582));
#77756=CARTESIAN_POINT('Ctrl Pts',(86.7967664476536,52.078113434174,13.2628649084919));
#77757=CARTESIAN_POINT('Ctrl Pts',(86.8291472898651,52.0814991619193,13.2948448699306));
#77758=CARTESIAN_POINT('Ctrl Pts',(86.862692146513,52.0848848896645,13.325429993775));
#77759=CARTESIAN_POINT('Ctrl Pts',(86.9082401705004,52.0894821133216,13.3669592204204));
#77760=CARTESIAN_POINT('Ctrl Pts',(86.9561374912916,52.0940793369787,13.4060996032432));
#77761=CARTESIAN_POINT('Ctrl Pts',(87.0061034332076,52.0986765606358,13.4425746349722));
#77762=CARTESIAN_POINT('Ctrl Pts',(87.0569249272226,52.1033525011988,13.4796742179207));
#77763=CARTESIAN_POINT('Ctrl Pts',(87.1098862220447,52.1080284417618,13.5140158871587));
#77764=CARTESIAN_POINT('Ctrl Pts',(87.1646536219269,52.1127043823248,13.5453487228921));
#77765=CARTESIAN_POINT('Ctrl Pts',(87.2183509342208,52.1172889607641,13.5760693535784));
#77766=CARTESIAN_POINT('Ctrl Pts',(87.2737839451832,52.1218735392034,13.6038974062373));
#77767=CARTESIAN_POINT('Ctrl Pts',(87.3306078061622,52.1264581176428,13.6286392092113));
#77768=CARTESIAN_POINT('Ctrl Pts',(87.3873969373941,52.1310398940682,13.6533658904294));
#77769=CARTESIAN_POINT('Ctrl Pts',(87.4455747673341,52.1356216704936,13.6750098593511));
#77770=CARTESIAN_POINT('Ctrl Pts',(87.5047735561091,52.140203446919,13.693424229605));
#77771=CARTESIAN_POINT('Ctrl Pts',(87.5639579071159,52.1447841059124,13.711834108848));
#77772=CARTESIAN_POINT('Ctrl Pts',(87.6241622368029,52.1493647649057,13.7270158019066));
#77773=CARTESIAN_POINT('Ctrl Pts',(87.6850025666825,52.153945423899,13.73887193445));
#77774=CARTESIAN_POINT('Ctrl Pts',(87.7480408493917,52.1586915664197,13.7511563884723));
#77775=CARTESIAN_POINT('Ctrl Pts',(87.811761406716,52.1634377089405,13.7598702251828));
#77776=CARTESIAN_POINT('Ctrl Pts',(87.8757268866723,52.1681838514612,13.7649632192636));
#77777=CARTESIAN_POINT('Ctrl Pts',(87.9375402859127,52.1727703128257,13.7698848625728));
#77778=CARTESIAN_POINT('Ctrl Pts',(87.9995818583249,52.1773567741903,13.7714255110949));
#77779=CARTESIAN_POINT('Ctrl Pts',(88.0614555531867,52.1819432355548,13.769592989171));
#77780=CARTESIAN_POINT('Ctrl Pts',(88.1265605179797,52.1867692186536,13.7676647662711));
#77781=CARTESIAN_POINT('Ctrl Pts',(88.1914789475542,52.1915952017524,13.7620014384124));
#77782=CARTESIAN_POINT('Ctrl Pts',(88.2557571753501,52.1964211848512,13.7526738750317));
#77783=CARTESIAN_POINT('Ctrl Pts',(88.320035403146,52.20124716795,13.7433463116511));
#77784=CARTESIAN_POINT('Ctrl Pts',(88.3836728097494,52.2060731510488,13.7303547181766));
#77785=CARTESIAN_POINT('Ctrl Pts',(88.4462330406866,52.2108991341476,13.7138310095075));
#77786=CARTESIAN_POINT('Ctrl Pts',(88.5058278141434,52.2154963577379,13.6980905517112));
#77787=CARTESIAN_POINT('Ctrl Pts',(88.5646899250684,52.2200935813282,13.6790806940928));
#77788=CARTESIAN_POINT('Ctrl Pts',(88.6224348357162,52.2246908049185,13.656887261019));
#77789=CARTESIAN_POINT('Ctrl Pts',(88.6811684964101,52.2293667454899,13.6343138159627));
#77790=CARTESIAN_POINT('Ctrl Pts',(88.738745800749,52.2340426860612,13.6084467899394));
#77791=CARTESIAN_POINT('Ctrl Pts',(88.7947749495291,52.2387186266326,13.5794304292205));
#77792=CARTESIAN_POINT('Ctrl Pts',(88.8497093567838,52.2433032050036,13.5509810129526));
#77793=CARTESIAN_POINT('Ctrl Pts',(88.9031550888766,52.2478877833747,13.5195044688184));
#77794=CARTESIAN_POINT('Ctrl Pts',(88.9547623926716,52.2524723617457,13.4851854641937));
#77795=CARTESIAN_POINT('Ctrl Pts',(89.0063381549831,52.2570541381025,13.4508874347458));
#77796=CARTESIAN_POINT('Ctrl Pts',(89.0560772939649,52.2616359144592,13.4137506708428));
#77797=CARTESIAN_POINT('Ctrl Pts',(89.1036569456197,52.266217690816,13.3740044475418));
#77798=CARTESIAN_POINT('Ctrl Pts',(89.1512249932506,52.2707983497404,13.3342679177989));
#77799=CARTESIAN_POINT('Ctrl Pts',(89.1966342085771,52.2753790086648,13.2919235182363));
#77800=CARTESIAN_POINT('Ctrl Pts',(89.2395945159105,52.2799596675893,13.2472410215848));
#77801=CARTESIAN_POINT('Ctrl Pts',(89.2841068333612,52.2847058101761,13.2009442979601));
#77802=CARTESIAN_POINT('Ctrl Pts',(89.325989464459,52.2894519527629,13.1521376824791));
#77803=CARTESIAN_POINT('Ctrl Pts',(89.3649629946575,52.2941980953497,13.1011613616717));
#77804=CARTESIAN_POINT('Ctrl Pts',(89.4026252824094,52.2987845566454,13.0519001104328));
#77805=CARTESIAN_POINT('Ctrl Pts',(89.4375708857887,52.3033710179412,13.000613318739));
#77806=CARTESIAN_POINT('Ctrl Pts',(89.4695915607741,52.307957479237,12.947637961092));
#77807=CARTESIAN_POINT('Ctrl Pts',(89.5032844735889,52.3127834624693,12.8918960347477));
#77808=CARTESIAN_POINT('Ctrl Pts',(89.5337382689994,52.3176094457016,12.8342849041646));
#77809=CARTESIAN_POINT('Ctrl Pts',(89.5607664177231,52.3224354289339,12.7752241437639));
#77810=CARTESIAN_POINT('Ctrl Pts',(89.5877945664468,52.3272614121663,12.7161633833633));
#77811=CARTESIAN_POINT('Ctrl Pts',(89.6113969050988,52.3320873953986,12.6556536249518));
#77812=CARTESIAN_POINT('Ctrl Pts',(89.631447580047,52.3369133786309,12.5941330096858));
#77813=CARTESIAN_POINT('Ctrl Pts',(89.6505478195558,52.3415106022077,12.535528574207));
#77814=CARTESIAN_POINT('Ctrl Pts',(89.6665039718338,52.3461078257845,12.4757663456097));
#77815=CARTESIAN_POINT('Ctrl Pts',(89.6791795669483,52.3507050493613,12.4152159332221));
#77816=CARTESIAN_POINT('Ctrl Pts',(89.6920722027953,52.3553809899344,12.3536287327593));
#77817=CARTESIAN_POINT('Ctrl Pts',(89.70157062529,52.3600569305074,12.2912265774969));
#77818=CARTESIAN_POINT('Ctrl Pts',(89.7075835073716,52.3647328710804,12.2284168652413));
#77819=CARTESIAN_POINT('Ctrl Pts',(89.7134789050183,52.3693174494369,12.1668343787055));
#77820=CARTESIAN_POINT('Ctrl Pts',(89.7160236929141,52.3739020277933,12.1048606492721));
#77821=CARTESIAN_POINT('Ctrl Pts',(89.71518330836,52.3784866061497,12.0428896753089));
#77822=CARTESIAN_POINT('Ctrl Pts',(89.7143434374343,52.3830683824915,11.9809565769287));
#77823=CARTESIAN_POINT('Ctrl Pts',(89.710122503393,52.3876501588333,11.9190267386236));
#77824=CARTESIAN_POINT('Ctrl Pts',(89.70253800403,52.392231935175,11.8574957637787));
#77825=CARTESIAN_POINT('Ctrl Pts',(89.6949553544229,52.3968125940841,11.7959797954986));
#77826=CARTESIAN_POINT('Ctrl Pts',(89.6840108302165,52.4013932529931,11.7348630025654));
#77827=CARTESIAN_POINT('Ctrl Pts',(89.669773736496,52.4059739119022,11.6745354081002));
#77828=CARTESIAN_POINT('Ctrl Pts',(89.6550223047996,52.4107200545032,11.6120283819732));
#77829=CARTESIAN_POINT('Ctrl Pts',(89.6367359211655,52.4154661971042,11.5503692487821));
#77830=CARTESIAN_POINT('Ctrl Pts',(89.6150488293952,52.4202123397052,11.489977267362));
#77831=CARTESIAN_POINT('Ctrl Pts',(89.5940913877346,52.4247988009849,11.4316171404813));
#77832=CARTESIAN_POINT('Ctrl Pts',(89.5699587204277,52.4293852622646,11.3744407070064));
#77833=CARTESIAN_POINT('Ctrl Pts',(89.5428209755857,52.4339717235443,11.3188056917002));
#77834=CARTESIAN_POINT('Ctrl Pts',(89.5142659972748,52.438797706806,11.2602652099966));
#77835=CARTESIAN_POINT('Ctrl Pts',(89.4823837675879,52.4436236900676,11.2034321253496));
#77836=CARTESIAN_POINT('Ctrl Pts',(89.4474256066323,52.4484496733293,11.148690721615));
#77837=CARTESIAN_POINT('Ctrl Pts',(89.4124674456766,52.4532756565909,11.0939493178805));
#77838=CARTESIAN_POINT('Ctrl Pts',(89.3744337956266,52.4581016398525,11.0413000750128));
#77839=CARTESIAN_POINT('Ctrl Pts',(89.3336244852963,52.4629276231142,10.9910863725421));
#77840=CARTESIAN_POINT('Ctrl Pts',(89.2947496043837,52.467524846715,10.9432528833718));
#77841=CARTESIAN_POINT('Ctrl Pts',(89.2531966879137,52.4721220703158,10.8974328229279));
#77842=CARTESIAN_POINT('Ctrl Pts',(89.2092022313909,52.4767192939166,10.8539413181327));
#77843=CARTESIAN_POINT('Ctrl Pts',(89.1644544701387,52.4813952344866,10.8097051205094));
#77844=CARTESIAN_POINT('Ctrl Pts',(89.1171810309949,52.4860711750567,10.7678784429161));
#77845=CARTESIAN_POINT('Ctrl Pts',(89.0676746417971,52.4907471156267,10.7287589832109));
#77846=CARTESIAN_POINT('Ctrl Pts',(89.0191355472001,52.4953316940081,10.6904038701442));
#77847=CARTESIAN_POINT('Ctrl Pts',(88.9684503945638,52.4999162723895,10.6546514656367));
#77848=CARTESIAN_POINT('Ctrl Pts',(88.9159314434978,52.5045008507709,10.6217445107707));
#77849=CARTESIAN_POINT('Ctrl Pts',(88.8634445910991,52.509082627138,10.5888576680617));
#77850=CARTESIAN_POINT('Ctrl Pts',(88.8091265930975,52.513664403505,10.558813096353));
#77851=CARTESIAN_POINT('Ctrl Pts',(88.7533192950585,52.5182461798721,10.5318106701636));
#77852=CARTESIAN_POINT('Ctrl Pts',(88.6975256076543,52.5228268388067,10.5048148294958));
#77853=CARTESIAN_POINT('Ctrl Pts',(88.6402437992809,52.5274074977413,10.480859883103));
#77854=CARTESIAN_POINT('Ctrl Pts',(88.5818391276159,52.5319881566759,10.4600991543739));
#77855=CARTESIAN_POINT('Ctrl Pts',(88.5213244936232,52.5367342992527,10.4385884110609));
#77856=CARTESIAN_POINT('Ctrl Pts',(88.4596048389029,52.5414804418294,10.420507351753));
#77857=CARTESIAN_POINT('Ctrl Pts',(88.397105205341,52.5462265844062,10.4059706008602));
#77858=CARTESIAN_POINT('Ctrl Pts',(88.3367083364506,52.5508130457118,10.3919229306942));
#77859=CARTESIAN_POINT('Ctrl Pts',(88.2755836749861,52.5553995070174,10.3811848686896));
#77860=CARTESIAN_POINT('Ctrl Pts',(88.2141240412226,52.559985968323,10.3738074992846));
#77861=CARTESIAN_POINT('Ctrl Pts',(88.1494547589547,52.5648119515354,10.3660448564696));
#77862=CARTESIAN_POINT('Ctrl Pts',(88.0844152000847,52.5696379347478,10.3620035979478));
#77863=CARTESIAN_POINT('Ctrl Pts',(88.0194645253132,52.5744639179602,10.3616810194652));
#77864=CARTESIAN_POINT('Ctrl Pts',(87.9545138505416,52.5792899011726,10.3613584409825));
#77865=CARTESIAN_POINT('Ctrl Pts',(87.8896527029231,52.584115884385,10.3647544313855));
#77866=CARTESIAN_POINT('Ctrl Pts',(87.8253321896315,52.5889418675974,10.3718033467767));
#77867=CARTESIAN_POINT('Ctrl Pts',(87.7640605755197,52.5935390911885,10.3785181318687));
#77868=CARTESIAN_POINT('Ctrl Pts',(87.7030279223271,52.5981363147797,10.3885748725647));
#77869=CARTESIAN_POINT('Ctrl Pts',(87.6426272497201,52.6027335383709,10.4019458084391));
#77870=CARTESIAN_POINT('Ctrl Pts',(87.5811923532064,52.6074094789421,10.4155456911273));
#77871=CARTESIAN_POINT('Ctrl Pts',(87.5204118209124,52.6120854195133,10.4325743699693));
#77872=CARTESIAN_POINT('Ctrl Pts',(87.46069453033,52.6167613600846,10.4529473890628));
#77873=CARTESIAN_POINT('Ctrl Pts',(87.4021440430775,52.6213459384561,10.4729223441067));
#77874=CARTESIAN_POINT('Ctrl Pts',(87.3446161271531,52.6259305168276,10.4961119538344));
#77875=CARTESIAN_POINT('Ctrl Pts',(87.2884840837042,52.6305150951992,10.522385544801));
#77876=CARTESIAN_POINT('Ctrl Pts',(87.2323863471824,52.6350968715562,10.5486430778065));
#77877=CARTESIAN_POINT('Ctrl Pts',(87.1776832515823,52.6396786479133,10.5779806392638));
#77878=CARTESIAN_POINT('Ctrl Pts',(87.1247281323297,52.6442604242704,10.6102194491696));
#77879=CARTESIAN_POINT('Ctrl Pts',(87.0717859281054,52.648841083195,10.6424503964711));
#77880=CARTESIAN_POINT('Ctrl Pts',(87.020591288557,52.6534217421196,10.6775809229875));
#77881=CARTESIAN_POINT('Ctrl Pts',(86.9714711392208,52.6580024010442,10.7153873304285));
#77882=CARTESIAN_POINT('Ctrl Pts',(86.9205764455857,52.6627485436305,10.7545595550686));
#77883=CARTESIAN_POINT('Ctrl Pts',(86.8719095003477,52.6674946862169,10.7966043995105));
#77884=CARTESIAN_POINT('Ctrl Pts',(86.8257971440967,52.6722408288033,10.841226949203));
#77885=CARTESIAN_POINT('Ctrl Pts',(86.7812362120673,52.6768272900989,10.8843481983753));
#77886=CARTESIAN_POINT('Ctrl Pts',(86.739060998119,52.6814137513944,10.9298760088617));
#77887=CARTESIAN_POINT('Ctrl Pts',(86.6995274846004,52.68600021269,10.9775080721698));
#77888=CARTESIAN_POINT('Ctrl Pts',(86.6579293850988,52.6908261959218,11.0276276576205));
#77889=CARTESIAN_POINT('Ctrl Pts',(86.6192568617795,52.6956521791536,11.0800767945419));
#77890=CARTESIAN_POINT('Ctrl Pts',(86.5837566909408,52.7004781623853,11.1344682655187));
#77891=CARTESIAN_POINT('Ctrl Pts',(86.5482565201021,52.7053041456171,11.1888597364954));
#77892=CARTESIAN_POINT('Ctrl Pts',(86.5159289571537,52.7101301288489,11.2451929409941));
#77893=CARTESIAN_POINT('Ctrl Pts',(86.4869635332425,52.7149561120806,11.3030532891523));
#77894=CARTESIAN_POINT('Ctrl Pts',(86.4574999237459,52.7198650989407,11.3619087959349));
#77895=CARTESIAN_POINT('Ctrl Pts',(86.4314063174814,52.7247740858009,11.4225592194157));
#77896=CARTESIAN_POINT('Ctrl Pts',(86.4088885715127,52.729683072661,11.4846104521835));
#77897=CARTESIAN_POINT('Ctrl Pts',(86.3864229191759,52.7345807028357,11.5465181326575));
#77898=CARTESIAN_POINT('Ctrl Pts',(86.3675168111418,52.7394783330105,11.6098198038362));
#77899=CARTESIAN_POINT('Ctrl Pts',(86.3523292230594,52.7443759631853,11.6740993884629));
#77900=CARTESIAN_POINT('Ctrl Pts',(86.3371938783017,52.7492567461502,11.738157859691));
#77901=CARTESIAN_POINT('Ctrl Pts',(86.325751674089,52.7541375291151,11.803187158091));
#77902=CARTESIAN_POINT('Ctrl Pts',(86.3181120088452,52.75901831208,11.8687562801913));
#77903=CARTESIAN_POINT('Ctrl Pts',(86.3105092552082,52.7638755131816,11.9340086002363));
#77904=CARTESIAN_POINT('Ctrl Pts',(86.3066724870618,52.7687327142832,11.9997951539516));
#77905=CARTESIAN_POINT('Ctrl Pts',(86.3066600304638,52.7735899153848,12.0656777559288));
#77906=CARTESIAN_POINT('',(86.3066607114372,53.5673399154776,12.0675572608337));
#77907=CARTESIAN_POINT('Ctrl Pts',(86.3066600304636,52.7735899154298,12.0656777565391));
#77908=CARTESIAN_POINT('Ctrl Pts',(86.3066478884484,52.7783244602588,12.129896660799));
#77909=CARTESIAN_POINT('Ctrl Pts',(86.3102696895027,52.7830590050878,12.1940683671357));
#77910=CARTESIAN_POINT('Ctrl Pts',(86.3174835015953,52.7877935499168,12.2577725351328));
#77911=CARTESIAN_POINT('Ctrl Pts',(86.3247131691019,52.7925385009175,12.3216167200773));
#77912=CARTESIAN_POINT('Ctrl Pts',(86.3355505626445,52.7972834519183,12.3849908574272));
#77913=CARTESIAN_POINT('Ctrl Pts',(86.3499021437454,52.8020284029191,12.4474823030581));
#77914=CARTESIAN_POINT('Ctrl Pts',(86.3642700270975,52.8067787438056,12.5100447339854));
#77915=CARTESIAN_POINT('Ctrl Pts',(86.3821599224672,52.8115290846921,12.5717220352282));
#77916=CARTESIAN_POINT('Ctrl Pts',(86.4034285223832,52.8162794255786,12.6321172846264));
#77917=CARTESIAN_POINT('Ctrl Pts',(86.4247516027314,52.8210419346674,12.6926672390503));
#77918=CARTESIAN_POINT('Ctrl Pts',(86.4494705067647,52.8258044437561,12.7519281542938));
#77919=CARTESIAN_POINT('Ctrl Pts',(86.4773939614703,52.8305669528449,12.8095236070127));
#77920=CARTESIAN_POINT('Ctrl Pts',(86.4977263091968,52.8340347540845,12.851461497023));
#77921=CARTESIAN_POINT('Ctrl Pts',(86.5197567014376,52.8375025553242,12.8925168392184));
#77922=CARTESIAN_POINT('Ctrl Pts',(86.5433968215242,52.8409703565639,12.9325539487693));
#77923=CARTESIAN_POINT('Ctrl Pts',(86.5747362525636,52.8455675801571,12.985630677195));
#77924=CARTESIAN_POINT('Ctrl Pts',(86.6090230548098,52.8501648037503,13.037114053001));
#77925=CARTESIAN_POINT('Ctrl Pts',(86.6460701587727,52.8547620273435,13.0866573196364));
#77926=CARTESIAN_POINT('Ctrl Pts',(86.6837516099672,52.8594379679145,13.1370489018124));
#77927=CARTESIAN_POINT('Ctrl Pts',(86.7242885925132,52.8641139084855,13.185432804658));
#77928=CARTESIAN_POINT('Ctrl Pts',(86.7674358396594,52.8687898490565,13.2314711556776));
#77929=CARTESIAN_POINT('Ctrl Pts',(86.8097400420211,52.8733744274301,13.2766099732558));
#77930=CARTESIAN_POINT('Ctrl Pts',(86.8545530587904,52.8779590058036,13.3194936839307));
#77931=CARTESIAN_POINT('Ctrl Pts',(86.901602145811,52.8825435841772,13.359835861584));
#77932=CARTESIAN_POINT('Ctrl Pts',(86.9486224772492,52.8871253605364,13.400153382801));
#77933=CARTESIAN_POINT('Ctrl Pts',(86.9978757834375,52.8917071368955,13.4379321203825));
#77934=CARTESIAN_POINT('Ctrl Pts',(87.049053695795,52.8962889132547,13.4729236452013));
#77935=CARTESIAN_POINT('Ctrl Pts',(87.1002191265607,52.9008695721813,13.5079066360665));
#77936=CARTESIAN_POINT('Ctrl Pts',(87.1533078116675,52.905450231108,13.5401034764192));
#77937=CARTESIAN_POINT('Ctrl Pts',(87.2079813162425,52.9100308900346,13.569308294774));
#77938=CARTESIAN_POINT('Ctrl Pts',(87.2646299889455,52.914777032619,13.5995681840786));
#77939=CARTESIAN_POINT('Ctrl Pts',(87.3229796991594,52.9195231752034,13.6266153986706));
#77940=CARTESIAN_POINT('Ctrl Pts',(87.3826271432278,52.9242693177877,13.6502734576051));
#77941=CARTESIAN_POINT('Ctrl Pts',(87.4402677827277,52.9288557790853,13.6731355545081));
#77942=CARTESIAN_POINT('Ctrl Pts',(87.4991196905869,52.9334422403829,13.6928328422381));
#77943=CARTESIAN_POINT('Ctrl Pts',(87.5588019903555,52.9380287016805,13.7092564607126));
#77944=CARTESIAN_POINT('Ctrl Pts',(87.6216011200086,52.9428546849083,13.7265377811367));
#77945=CARTESIAN_POINT('Ctrl Pts',(87.6853191247605,52.947680668136,13.740193984382));
#77946=CARTESIAN_POINT('Ctrl Pts',(87.749501534727,52.9525066513638,13.7501595495261));
#77947=CARTESIAN_POINT('Ctrl Pts',(87.8136839446935,52.9573326345915,13.7601251146701));
#77948=CARTESIAN_POINT('Ctrl Pts',(87.8783301074432,52.9621586178193,13.7664000561262));
#77949=CARTESIAN_POINT('Ctrl Pts',(87.9429841694157,52.9669846010471,13.7689822906859));
#77950=CARTESIAN_POINT('Ctrl Pts',(88.0045735212603,52.9715818246389,13.7714421230305));
#77951=CARTESIAN_POINT('Ctrl Pts',(88.066422914334,52.9761790482308,13.7705615739378));
#77952=CARTESIAN_POINT('Ctrl Pts',(88.1281395648571,52.9807762718227,13.7663097241224));
#77953=CARTESIAN_POINT('Ctrl Pts',(88.1909129723994,52.9854522123939,13.7619850710666));
#77954=CARTESIAN_POINT('Ctrl Pts',(88.2535485227054,52.990128152965,13.7541724628825));
#77955=CARTESIAN_POINT('Ctrl Pts',(88.3156293295559,52.9948040935361,13.7428946917366));
#77956=CARTESIAN_POINT('Ctrl Pts',(88.3764971528496,52.9993886719084,13.7318372745399));
#77957=CARTESIAN_POINT('Ctrl Pts',(88.4368311909235,53.0039732502806,13.7174489820524));
#77958=CARTESIAN_POINT('Ctrl Pts',(88.4962428750387,53.0085578286528,13.6998035952415));
#77959=CARTESIAN_POINT('Ctrl Pts',(88.5556182477674,53.0131396050106,13.6821689929838));
#77960=CARTESIAN_POINT('Ctrl Pts',(88.614071897359,53.0177213813683,13.6612813882623));
#77961=CARTESIAN_POINT('Ctrl Pts',(88.6712278545075,53.0223031577261,13.6372651003992));
#77962=CARTESIAN_POINT('Ctrl Pts',(88.7283698721008,53.0268838166513,13.6132546697797));
#77963=CARTESIAN_POINT('Ctrl Pts',(88.7842143564401,53.0314644755766,13.5861172678811));
#77964=CARTESIAN_POINT('Ctrl Pts',(88.8384047838757,53.0360451345018,13.5560255565659));
#77965=CARTESIAN_POINT('Ctrl Pts',(88.894552927535,53.0407912770875,13.5248467338506));
#77966=CARTESIAN_POINT('Ctrl Pts',(88.948924675794,53.0455374196733,13.4904962827174));
#77967=CARTESIAN_POINT('Ctrl Pts',(89.0011530118701,53.050283562259,13.4532173040604));
#77968=CARTESIAN_POINT('Ctrl Pts',(89.0516241550464,53.0548700235552,13.4171925556073));
#77969=CARTESIAN_POINT('Ctrl Pts',(89.1000934654956,53.0594564848514,13.3784336063825));
#77970=CARTESIAN_POINT('Ctrl Pts',(89.1462629006426,53.0640429461476,13.3372013931807));
#77971=CARTESIAN_POINT('Ctrl Pts',(89.1948434740714,53.068868929378,13.2938158816469));
#77972=CARTESIAN_POINT('Ctrl Pts',(89.2408769065255,53.0736949126085,13.247692144612));
#77973=CARTESIAN_POINT('Ctrl Pts',(89.2840616485871,53.0785208958389,13.1991764533808));
#77974=CARTESIAN_POINT('Ctrl Pts',(89.3272463906486,53.0833468790694,13.1506607621496));
#77975=CARTESIAN_POINT('Ctrl Pts',(89.3675821005486,53.0881728622998,13.0997536726613));
#77976=CARTESIAN_POINT('Ctrl Pts',(89.4048197737318,53.0929988455303,13.0468370272141));
#77977=CARTESIAN_POINT('Ctrl Pts',(89.4402923192196,53.0975960691222,12.9964287188472));
#77978=CARTESIAN_POINT('Ctrl Pts',(89.473099585584,53.1021932927141,12.9439901255787));
#77979=CARTESIAN_POINT('Ctrl Pts',(89.5030025514424,53.106790516306,12.8898344627953));
#77980=CARTESIAN_POINT('Ctrl Pts',(89.5334175374574,53.1114664568771,12.8347515076803));
#77981=CARTESIAN_POINT('Ctrl Pts',(89.5608274449313,53.1161423974483,12.7778925068007));
#77982=CARTESIAN_POINT('Ctrl Pts',(89.5850253034763,53.1208183380194,12.7196200575383));
#77983=CARTESIAN_POINT('Ctrl Pts',(89.6087503652583,53.1254029163916,12.6624861811512));
#77984=CARTESIAN_POINT('Ctrl Pts',(89.6293875637479,53.1299874947638,12.6039940863905));
#77985=CARTESIAN_POINT('Ctrl Pts',(89.6467881246946,53.1345720731361,12.5445102367852));
#77986=CARTESIAN_POINT('Ctrl Pts',(89.6641780507214,53.1391538494938,12.4850627426728));
#77987=CARTESIAN_POINT('Ctrl Pts',(89.67833511902,53.1437356258516,12.424625183169));
#77988=CARTESIAN_POINT('Ctrl Pts',(89.6891598475981,53.1483174022094,12.3635808486939));
#77989=CARTESIAN_POINT('Ctrl Pts',(89.6999819361733,53.1528980611346,12.3025514020959));
#77990=CARTESIAN_POINT('Ctrl Pts',(89.7074732095439,53.1574787200599,12.2409159753006));
#77991=CARTESIAN_POINT('Ctrl Pts',(89.7115853466096,53.1620593789851,12.1790677429547));
#77992=CARTESIAN_POINT('Ctrl Pts',(89.715846041231,53.1668055215708,12.1149851438841));
#77993=CARTESIAN_POINT('Ctrl Pts',(89.7164786690044,53.1715516641565,12.0506746448662));
#77994=CARTESIAN_POINT('Ctrl Pts',(89.7134883946887,53.1762978067422,11.9865764420948));
#77995=CARTESIAN_POINT('Ctrl Pts',(89.7105987264652,53.1808842680384,11.9246347871911));
#77996=CARTESIAN_POINT('Ctrl Pts',(89.7043262066928,53.1854707293346,11.8628918872255));
#77997=CARTESIAN_POINT('Ctrl Pts',(89.6947283959729,53.1900571906308,11.8017396658699));
#77998=CARTESIAN_POINT('Ctrl Pts',(89.6846293521585,53.1948831738613,11.7373938498458));
#77999=CARTESIAN_POINT('Ctrl Pts',(89.670848301016,53.1997091570917,11.6737027307551));
#78000=CARTESIAN_POINT('Ctrl Pts',(89.6535125923678,53.2045351403222,11.6111074637751));
#78001=CARTESIAN_POINT('Ctrl Pts',(89.6361768837197,53.2093611235526,11.5485121967951));
#78002=CARTESIAN_POINT('Ctrl Pts',(89.6152867992471,53.214187106783,11.487013370594));
#78003=CARTESIAN_POINT('Ctrl Pts',(89.5910280729863,53.2190130900135,11.4270272899605));
#78004=CARTESIAN_POINT('Ctrl Pts',(89.5679192507301,53.2236103136057,11.369884649399));
#78005=CARTESIAN_POINT('Ctrl Pts',(89.541659099045,53.2282075371979,11.3138799422366));
#78006=CARTESIAN_POINT('Ctrl Pts',(89.512381111906,53.2328047607902,11.2593838630353));
#78007=CARTESIAN_POINT('Ctrl Pts',(89.4826018059495,53.2374807013613,11.2039546626513));
#78008=CARTESIAN_POINT('Ctrl Pts',(89.4497004554622,53.2421566419324,11.1500867673443));
#78009=CARTESIAN_POINT('Ctrl Pts',(89.4138694256987,53.2468325825035,11.09815072969));
#78010=CARTESIAN_POINT('Ctrl Pts',(89.3787384907302,53.2514171608761,11.0472294591209));
#78011=CARTESIAN_POINT('Ctrl Pts',(89.3407916345206,53.2560017392486,10.9981656719112));
#78012=CARTESIAN_POINT('Ctrl Pts',(89.3002560358696,53.2605863176212,10.9512831258235));
#78013=CARTESIAN_POINT('Ctrl Pts',(89.2597452118706,53.2651680939793,10.9044292335314));
#78014=CARTESIAN_POINT('Ctrl Pts',(89.2166491149424,53.2697498703374,10.8597543232163));
#78015=CARTESIAN_POINT('Ctrl Pts',(89.1712357965721,53.2743316466955,10.8175498680553));
#78016=CARTESIAN_POINT('Ctrl Pts',(89.1258335538883,53.2789123056211,10.7753557059831));
#78017=CARTESIAN_POINT('Ctrl Pts',(89.0781155843645,53.2834929645467,10.7356311493715));
#78018=CARTESIAN_POINT('Ctrl Pts',(89.0283859930401,53.2880736234723,10.6986300512423));
#78019=CARTESIAN_POINT('Ctrl Pts',(88.9768598403684,53.2928197660577,10.660292229023));
#78020=CARTESIAN_POINT('Ctrl Pts',(88.923174365156,53.2975659086431,10.6248788099224));
#78021=CARTESIAN_POINT('Ctrl Pts',(88.8677021869033,53.3023120512284,10.5926242167881));
#78022=CARTESIAN_POINT('Ctrl Pts',(88.8140963387823,53.306898512525,10.5614548112371));
#78023=CARTESIAN_POINT('Ctrl Pts',(88.7588226143968,53.3114849738215,10.5332352153234));
#78024=CARTESIAN_POINT('Ctrl Pts',(88.7022414979199,53.3160714351181,10.508129650082));
#78025=CARTESIAN_POINT('Ctrl Pts',(88.6427055067527,53.3208974183479,10.4817129795827));
#78026=CARTESIAN_POINT('Ctrl Pts',(88.58172242412,53.3257234015777,10.4587447481971));
#78027=CARTESIAN_POINT('Ctrl Pts',(88.5197319482119,53.3305493848074,10.4393572486657));
#78028=CARTESIAN_POINT('Ctrl Pts',(88.4577414723038,53.3353753680372,10.4199697491342));
#78029=CARTESIAN_POINT('Ctrl Pts',(88.3947442504564,53.340201351267,10.4041630641035));
#78030=CARTESIAN_POINT('Ctrl Pts',(88.3311907710474,53.3450273344968,10.3920069576799));
#78031=CARTESIAN_POINT('Ctrl Pts',(88.2706498323445,53.3496245580888,10.3804270709342));
#78032=CARTESIAN_POINT('Ctrl Pts',(88.2093556183969,53.3542217816809,10.3721118964261));
#78033=CARTESIAN_POINT('Ctrl Pts',(88.1476919645212,53.3588190052729,10.3671503473128));
#78034=CARTESIAN_POINT('Ctrl Pts',(88.0849724610756,53.363494945844,10.3621038429761));
#78035=CARTESIAN_POINT('Ctrl Pts',(88.0218712499876,53.3681708864152,10.3605270842887));
#78036=CARTESIAN_POINT('Ctrl Pts',(87.9588039789972,53.3728468269863,10.3624594483865));
#78037=CARTESIAN_POINT('Ctrl Pts',(87.8969689658722,53.3774314053587,10.3643540564372));
#78038=CARTESIAN_POINT('Ctrl Pts',(87.8351671116439,53.382015983731,10.3696218762146));
#78039=CARTESIAN_POINT('Ctrl Pts',(87.7737936335629,53.3866005621034,10.3782476558091));
#78040=CARTESIAN_POINT('Ctrl Pts',(87.7124576658829,53.3911823384613,10.3868681634774));
#78041=CARTESIAN_POINT('Ctrl Pts',(87.6515500582537,53.3957641148193,10.3988424907949));
#78042=CARTESIAN_POINT('Ctrl Pts',(87.5914610742573,53.4003458911772,10.4141035367231));
#78043=CARTESIAN_POINT('Ctrl Pts',(87.5313867451412,53.4049265501026,10.4293608606913));
#78044=CARTESIAN_POINT('Ctrl Pts',(87.4721311364827,53.409507209028,10.4479031867508));
#78045=CARTESIAN_POINT('Ctrl Pts',(87.4140724617767,53.4140878679534,10.4696127193846));
#78046=CARTESIAN_POINT('Ctrl Pts',(87.353916324206,53.418834010539,10.4921065437499));
#78047=CARTESIAN_POINT('Ctrl Pts',(87.2950458257325,53.4235801531245,10.518000653331));
#78048=CARTESIAN_POINT('Ctrl Pts',(87.2378600183096,53.4283262957101,10.5471091532596));
#78049=CARTESIAN_POINT('Ctrl Pts',(87.1825981951091,53.4329127570064,10.5752383141332));
#78050=CARTESIAN_POINT('Ctrl Pts',(87.1289099154122,53.4374992183028,10.6063686662655));
#78051=CARTESIAN_POINT('Ctrl Pts',(87.0771286709566,53.4420856795992,10.6402864325571));
#78052=CARTESIAN_POINT('Ctrl Pts',(87.0226432188333,53.4469116628293,10.6759755097672));
#78053=CARTESIAN_POINT('Ctrl Pts',(86.9702699727955,53.4517376460594,10.714750748264));
#78054=CARTESIAN_POINT('Ctrl Pts',(86.9203585665297,53.4565636292896,10.756314503708));
#78055=CARTESIAN_POINT('Ctrl Pts',(86.8704471602638,53.4613896125197,10.7978782591519));
#78056=CARTESIAN_POINT('Ctrl Pts',(86.8229980143172,53.4662155957499,10.8422300325295));
#78057=CARTESIAN_POINT('Ctrl Pts',(86.7783140833319,53.47104157898,10.8890291989824));
#78058=CARTESIAN_POINT('Ctrl Pts',(86.7362981532647,53.4755794110246,10.9330340674335));
#78059=CARTESIAN_POINT('Ctrl Pts',(86.6965446275607,53.4801172430691,10.9793934087281));
#78060=CARTESIAN_POINT('Ctrl Pts',(86.6593331863823,53.4846550751137,11.0278421793559));
#78061=CARTESIAN_POINT('Ctrl Pts',(86.6221740909261,53.4891865237426,11.0762227965929));
#78062=CARTESIAN_POINT('Ctrl Pts',(86.5875503140188,53.4937179723716,11.1266866120252));
#78063=CARTESIAN_POINT('Ctrl Pts',(86.5557041194029,53.4982494210005,11.1789325079132));
#78064=CARTESIAN_POINT('Ctrl Pts',(86.5238903094915,53.5027762615553,11.2311252744424));
#78065=CARTESIAN_POINT('Ctrl Pts',(86.4948487563883,53.5073031021101,11.2850960865296));
#78066=CARTESIAN_POINT('Ctrl Pts',(86.4687795277154,53.511829942665,11.3405133698914));
#78067=CARTESIAN_POINT('Ctrl Pts',(86.4421402312034,53.5164557737287,11.3971424885313));
#78068=CARTESIAN_POINT('Ctrl Pts',(86.4186051288118,53.5210816047925,11.4552816346984));
#78069=CARTESIAN_POINT('Ctrl Pts',(86.3983382336703,53.5257074358562,11.5145502171383));
#78070=CARTESIAN_POINT('Ctrl Pts',(86.378515920084,53.5302317931049,11.5725186636484));
#78071=CARTESIAN_POINT('Ctrl Pts',(86.3618200008801,53.5347561503536,11.631566963447));
#78072=CARTESIAN_POINT('Ctrl Pts',(86.3483543202793,53.5392805076024,11.6913212318451));
#78073=CARTESIAN_POINT('Ctrl Pts',(86.3344356204183,53.5439570755736,11.7530857836639));
#78074=CARTESIAN_POINT('Ctrl Pts',(86.3239685799923,53.5486336435449,11.8156040867182));
#78075=CARTESIAN_POINT('Ctrl Pts',(86.3170104412882,53.5533102115161,11.8784521112473));
#78076=CARTESIAN_POINT('Ctrl Pts',(86.3100523025842,53.5579867794874,11.9413001357764));
#78077=CARTESIAN_POINT('Ctrl Pts',(86.306603075047,53.5626633474586,12.0044772662455));
#78078=CARTESIAN_POINT('Ctrl Pts',(86.3066607114366,53.5673399154299,12.0675572601897));
#78079=CARTESIAN_POINT('',(86.3066601203479,54.3610899154771,12.0653595099723));
#78080=CARTESIAN_POINT('Ctrl Pts',(86.3066607114372,53.5673399154776,12.0675572608336));
#78081=CARTESIAN_POINT('Ctrl Pts',(86.3067358739435,53.5734385352263,12.1498186326717));
#78082=CARTESIAN_POINT('Ctrl Pts',(86.3127703680478,53.579537154975,12.231815876902));
#78083=CARTESIAN_POINT('Ctrl Pts',(86.324628267231,53.5856357747237,12.312830335489));
#78084=CARTESIAN_POINT('Ctrl Pts',(86.332029821036,53.5894424576368,12.363398557141));
#78085=CARTESIAN_POINT('Ctrl Pts',(86.3416992924877,53.59324914055,12.4135844802534));
#78086=CARTESIAN_POINT('Ctrl Pts',(86.3535945960656,53.5970558234632,12.4632180290585));
#78087=CARTESIAN_POINT('Ctrl Pts',(86.3679602187063,53.6016530470553,12.5231590661058));
#78088=CARTESIAN_POINT('Ctrl Pts',(86.3856112274446,53.6062502706474,12.5824428301661));
#78089=CARTESIAN_POINT('Ctrl Pts',(86.4064706649311,53.6108474942395,12.6406829112678));
#78090=CARTESIAN_POINT('Ctrl Pts',(86.4276872727553,53.6155234348106,12.6999202210557));
#78091=CARTESIAN_POINT('Ctrl Pts',(86.4522231863206,53.6201993753817,12.7580772322774));
#78092=CARTESIAN_POINT('Ctrl Pts',(86.4799432088402,53.6248753159529,12.8147589317287));
#78093=CARTESIAN_POINT('Ctrl Pts',(86.5071216157924,53.6294598943253,12.8703331396263));
#78094=CARTESIAN_POINT('Ctrl Pts',(86.5373605891585,53.6340444726977,12.9244886896752));
#78095=CARTESIAN_POINT('Ctrl Pts',(86.5704835546859,53.6386290510701,12.9768716739365));
#78096=CARTESIAN_POINT('Ctrl Pts',(86.6035862760337,53.6432108274281,13.02922264263));
#78097=CARTESIAN_POINT('Ctrl Pts',(86.639569222979,53.6477926037861,13.0798027643285));
#78098=CARTESIAN_POINT('Ctrl Pts',(86.6782106069416,53.652374380144,13.128283987148));
#78099=CARTESIAN_POINT('Ctrl Pts',(86.7168425667998,53.6569550390695,13.1767533860611));
#78100=CARTESIAN_POINT('Ctrl Pts',(86.758131359452,53.6615356979949,13.2231245043846));
#78101=CARTESIAN_POINT('Ctrl Pts',(86.8018139552308,53.6661163569204,13.267101138429));
#78102=CARTESIAN_POINT('Ctrl Pts',(86.8470746549347,53.6708624995059,13.3126664990031));
#78103=CARTESIAN_POINT('Ctrl Pts',(86.8949050649616,53.6756086420914,13.3556605960175));
#78104=CARTESIAN_POINT('Ctrl Pts',(86.9449715152674,53.6803547846769,13.395796264598));
#78105=CARTESIAN_POINT('Ctrl Pts',(86.9933535081046,53.6849412459733,13.4345815912572));
#78106=CARTESIAN_POINT('Ctrl Pts',(87.0438229889342,53.6895277072697,13.4706975393349));
#78107=CARTESIAN_POINT('Ctrl Pts',(87.0960478619781,53.6941141685661,13.5039281695305));
#78108=CARTESIAN_POINT('Ctrl Pts',(87.1510001106102,53.6989401517961,13.5388942258609));
#78109=CARTESIAN_POINT('Ctrl Pts',(87.207895568258,53.7037661350262,13.5706650130704));
#78110=CARTESIAN_POINT('Ctrl Pts',(87.266319061639,53.7085921182562,13.5990444010667));
#78111=CARTESIAN_POINT('Ctrl Pts',(87.3247425550201,53.7134181014862,13.6274237890629));
#78112=CARTESIAN_POINT('Ctrl Pts',(87.3846934562525,53.7182440847163,13.6524115999727));
#78113=CARTESIAN_POINT('Ctrl Pts',(87.4457366346986,53.7230700679463,13.6738719362711));
#78114=CARTESIAN_POINT('Ctrl Pts',(87.5038862648798,53.7276672915384,13.6943150169081));
#78115=CARTESIAN_POINT('Ctrl Pts',(87.563265695465,53.7322645151305,13.7116414710749));
#78116=CARTESIAN_POINT('Ctrl Pts',(87.6235085536853,53.7368617387226,13.7257063639792));
#78117=CARTESIAN_POINT('Ctrl Pts',(87.6847829335868,53.7415376792937,13.740012086127));
#78118=CARTESIAN_POINT('Ctrl Pts',(87.74695011912,53.7462136198648,13.7509432366428));
#78119=CARTESIAN_POINT('Ctrl Pts',(87.8096049207595,53.7508895604359,13.7583991425363));
#78120=CARTESIAN_POINT('Ctrl Pts',(87.8710355236841,53.7554741388083,13.7657093690856));
#78121=CARTESIAN_POINT('Ctrl Pts',(87.9329343295529,53.7600587171808,13.7696788707333));
#78122=CARTESIAN_POINT('Ctrl Pts',(87.9949082391577,53.7646432955532,13.7702640320188));
#78123=CARTESIAN_POINT('Ctrl Pts',(88.0568442713882,53.7692250719111,13.7708488356639));
#78124=CARTESIAN_POINT('Ctrl Pts',(88.1188548083692,53.7738068482691,13.7680533955879));
#78125=CARTESIAN_POINT('Ctrl Pts',(88.1805439489161,53.7783886246271,13.7618861061362));
#78126=CARTESIAN_POINT('Ctrl Pts',(88.2422180443265,53.7829692835525,13.755720320802));
#78127=CARTESIAN_POINT('Ctrl Pts',(88.303570392612,53.787549942478,13.7461843691937));
#78128=CARTESIAN_POINT('Ctrl Pts',(88.3642094798163,53.7921306014034,13.7333385675885));
#78129=CARTESIAN_POINT('Ctrl Pts',(88.4270392514299,53.7968767439889,13.7200286907704));
#78130=CARTESIAN_POINT('Ctrl Pts',(88.4891026577919,53.8016228865744,13.7031652957325));
#78131=CARTESIAN_POINT('Ctrl Pts',(88.5499774633923,53.80636902916,13.6828729478704));
#78132=CARTESIAN_POINT('Ctrl Pts',(88.608804170509,53.8109554904564,13.6632633246015));
#78133=CARTESIAN_POINT('Ctrl Pts',(88.6665205270712,53.8155419517528,13.6404520908354));
#78134=CARTESIAN_POINT('Ctrl Pts',(88.7227649895615,53.8201284130492,13.6146011220564));
#78135=CARTESIAN_POINT('Ctrl Pts',(88.7819467454341,53.8249543962792,13.5874001202937));
#78136=CARTESIAN_POINT('Ctrl Pts',(88.8394980822379,53.8297803795093,13.5568334774783));
#78137=CARTESIAN_POINT('Ctrl Pts',(88.8950290374551,53.8346063627394,13.5231436087552));
#78138=CARTESIAN_POINT('Ctrl Pts',(88.9505599926724,53.8394323459695,13.4894537400321));
#78139=CARTESIAN_POINT('Ctrl Pts',(89.0040700763058,53.8442583291995,13.4526410764199));
#78140=CARTESIAN_POINT('Ctrl Pts',(89.0552091036478,53.8490843124296,13.41299746973));
#78141=CARTESIAN_POINT('Ctrl Pts',(89.1039240559726,53.8536815360217,13.3752330359843));
#78142=CARTESIAN_POINT('Ctrl Pts',(89.1506877066357,53.8582787596138,13.3347449665407));
#78143=CARTESIAN_POINT('Ctrl Pts',(89.1951795727132,53.8628759832058,13.291762446467));
#78144=CARTESIAN_POINT('Ctrl Pts',(89.2404332606208,53.867551923777,13.2480439486744));
#78145=CARTESIAN_POINT('Ctrl Pts',(89.283336156128,53.8722278643481,13.2017450224899));
#78146=CARTESIAN_POINT('Ctrl Pts',(89.3235839074266,53.8769038049192,13.1531514713069));
#78147=CARTESIAN_POINT('Ctrl Pts',(89.3630452665553,53.8814883832916,13.1055073790856));
#78148=CARTESIAN_POINT('Ctrl Pts',(89.3999539646657,53.886072961664,13.0556579346042));
#78149=CARTESIAN_POINT('Ctrl Pts',(89.4340601429617,53.8906575400365,13.003909731858));
#78150=CARTESIAN_POINT('Ctrl Pts',(89.4681454761555,53.8952393163944,12.9521931567121));
#78151=CARTESIAN_POINT('Ctrl Pts',(89.4994314063208,53.8998210927524,12.8985805485348));
#78152=CARTESIAN_POINT('Ctrl Pts',(89.5277102494122,53.9044028691103,12.8434090653755));
#78153=CARTESIAN_POINT('Ctrl Pts',(89.5559821956811,53.9089835280358,12.7882510377853));
#78154=CARTESIAN_POINT('Ctrl Pts',(89.581248278671,53.9135641869612,12.731535342748));
#78155=CARTESIAN_POINT('Ctrl Pts',(89.6033468146777,53.9181448458867,12.6736236149013));
#78156=CARTESIAN_POINT('Ctrl Pts',(89.6262436957873,53.9228909884722,12.6136197328818));
#78157=CARTESIAN_POINT('Ctrl Pts',(89.6457395154445,53.9276371310577,12.552332266648));
#78158=CARTESIAN_POINT('Ctrl Pts',(89.6617099036571,53.9323832736432,12.4901835093074));
#78159=CARTESIAN_POINT('Ctrl Pts',(89.6771429771701,53.9369697349396,12.430125711838));
#78160=CARTESIAN_POINT('Ctrl Pts',(89.6892840571562,53.941556196236,12.369264193803));
#78161=CARTESIAN_POINT('Ctrl Pts',(89.69807303788,53.9461426575324,12.3079904966283));
#78162=CARTESIAN_POINT('Ctrl Pts',(89.7073210116099,53.9509686407625,12.2435168608772));
#78163=CARTESIAN_POINT('Ctrl Pts',(89.7128571017517,53.9557946239926,12.1785874551594));
#78164=CARTESIAN_POINT('Ctrl Pts',(89.7146734512133,53.9606206072226,12.1136613809167));
#78165=CARTESIAN_POINT('Ctrl Pts',(89.7164898006749,53.9654465904527,12.0487353066739));
#78166=CARTESIAN_POINT('Ctrl Pts',(89.7145865057904,53.9702725736828,11.9838132093474));
#78167=CARTESIAN_POINT('Ctrl Pts',(89.709018817693,53.9750985569129,11.919347586585));
#78168=CARTESIAN_POINT('Ctrl Pts',(89.7037150472789,53.979695780505,11.8579377416451));
#78169=CARTESIAN_POINT('Ctrl Pts',(89.6950647092455,53.984293004097,11.7966899299085));
#78170=CARTESIAN_POINT('Ctrl Pts',(89.6830865172788,53.9888902276891,11.7359977055616));
#78171=CARTESIAN_POINT('Ctrl Pts',(89.6709032260674,53.9935661682602,11.6742662651626));
#78172=CARTESIAN_POINT('Ctrl Pts',(89.6552769954437,53.9982421088314,11.6131101540597));
#78173=CARTESIAN_POINT('Ctrl Pts',(89.6362828548449,54.0029180494025,11.5529400840574));
#78174=CARTESIAN_POINT('Ctrl Pts',(89.6176598366806,54.0075026277749,11.493945664132));
#78175=CARTESIAN_POINT('Ctrl Pts',(89.5957994952143,54.0120872061473,11.4358996084322));
#78176=CARTESIAN_POINT('Ctrl Pts',(89.5708238834506,54.0166717845197,11.3791781248263));
#78177=CARTESIAN_POINT('Ctrl Pts',(89.5458635363458,54.0212535608777,11.3224913084034));
#78178=CARTESIAN_POINT('Ctrl Pts',(89.5177918990106,54.0258353372356,11.2671279237597));
#78179=CARTESIAN_POINT('Ctrl Pts',(89.4867795774909,54.0304171135936,11.2134453247675));
#78180=CARTESIAN_POINT('Ctrl Pts',(89.4557748194517,54.0349977725191,11.1597758182261));
#78181=CARTESIAN_POINT('Ctrl Pts',(89.4218310554884,54.0395784314445,11.1077867241655));
#78182=CARTESIAN_POINT('Ctrl Pts',(89.3851644054752,54.04415909037,11.0578100266691));
#78183=CARTESIAN_POINT('Ctrl Pts',(89.3471731138449,54.0489052329555,11.0060278407147));
#78184=CARTESIAN_POINT('Ctrl Pts',(89.3062587244168,54.053651375541,10.956406744));
#78185=CARTESIAN_POINT('Ctrl Pts',(89.2627085564407,54.0583975181265,10.9092802736474));
#78186=CARTESIAN_POINT('Ctrl Pts',(89.2206236092914,54.0629839794229,10.8637393467971));
#78187=CARTESIAN_POINT('Ctrl Pts',(89.1760778662624,54.0675704407193,10.8205281563628));
#78188=CARTESIAN_POINT('Ctrl Pts',(89.1293676683184,54.0721569020157,10.7799095700301));
#78189=CARTESIAN_POINT('Ctrl Pts',(89.0802180914697,54.0769828852457,10.7371697312301));
#78190=CARTESIAN_POINT('Ctrl Pts',(89.028672291556,54.0818088684758,10.6973011153504));
#78191=CARTESIAN_POINT('Ctrl Pts',(88.9751117077413,54.0866348517059,10.6605593393543));
#78192=CARTESIAN_POINT('Ctrl Pts',(88.9215511239265,54.091460834936,10.6238175633582));
#78193=CARTESIAN_POINT('Ctrl Pts',(88.8659763507109,54.096286818166,10.5902028964001));
#78194=CARTESIAN_POINT('Ctrl Pts',(88.8087975090945,54.1011128013961,10.5599143549975));
#78195=CARTESIAN_POINT('Ctrl Pts',(88.7543290397454,54.1057100249882,10.531061540873));
#78196=CARTESIAN_POINT('Ctrl Pts',(88.6981815237835,54.1103072485803,10.5051081356642));
#78197=CARTESIAN_POINT('Ctrl Pts',(88.6406957446929,54.1149044721723,10.4822518809117));
#78198=CARTESIAN_POINT('Ctrl Pts',(88.5822256526191,54.1195804127435,10.4590042648755));
#78199=CARTESIAN_POINT('Ctrl Pts',(88.5223714607889,54.1242563533146,10.4389611930283));
#78200=CARTESIAN_POINT('Ctrl Pts',(88.4615189127579,54.1289322938857,10.4222824011262));
#78201=CARTESIAN_POINT('Ctrl Pts',(88.4018553495955,54.1335168722581,10.4059294925575));
#78202=CARTESIAN_POINT('Ctrl Pts',(88.3412326071423,54.1381014506306,10.3928107194147));
#78203=CARTESIAN_POINT('Ctrl Pts',(88.2800329469916,54.142686029003,10.3830275970673));
#78204=CARTESIAN_POINT('Ctrl Pts',(88.2188706910073,54.1472678053609,10.3732504539939));
#78205=CARTESIAN_POINT('Ctrl Pts',(88.1571327181066,54.1518495817189,10.366804999472));
#78206=CARTESIAN_POINT('Ctrl Pts',(88.0952117853512,54.1564313580769,10.3637417320489));
#78207=CARTESIAN_POINT('Ctrl Pts',(88.0333059542634,54.1610120170023,10.3606792117147));
#78208=CARTESIAN_POINT('Ctrl Pts',(87.9712177600988,54.1655926759278,10.36099726613));
#78209=CARTESIAN_POINT('Ctrl Pts',(87.9093433328666,54.1701733348532,10.3646943961688));
#78210=CARTESIAN_POINT('Ctrl Pts',(87.8452335925824,54.1749194774387,10.3685250909678));
#78211=CARTESIAN_POINT('Ctrl Pts',(87.7813539444909,54.1796656200243,10.3759837142419));
#78212=CARTESIAN_POINT('Ctrl Pts',(87.7181404417955,54.1844117626098,10.3870097931291));
#78213=CARTESIAN_POINT('Ctrl Pts',(87.6570537217279,54.1889982239062,10.3976649058141));
#78214=CARTESIAN_POINT('Ctrl Pts',(87.5965895299048,54.1935846852026,10.4116510313652));
#78215=CARTESIAN_POINT('Ctrl Pts',(87.5371294420067,54.198171146499,10.4288617865717));
#78216=CARTESIAN_POINT('Ctrl Pts',(87.4745641289013,54.202997129729,10.4469713509256));
#78217=CARTESIAN_POINT('Ctrl Pts',(87.4131112825313,54.2078231129591,10.468651380767));
#78218=CARTESIAN_POINT('Ctrl Pts',(87.3531925442499,54.2126490961892,10.4937200673037));
#78219=CARTESIAN_POINT('Ctrl Pts',(87.2932738059684,54.2174750794192,10.5187887538404));
#78220=CARTESIAN_POINT('Ctrl Pts',(87.2348897243538,54.2223010626493,10.5472457436092));
#78221=CARTESIAN_POINT('Ctrl Pts',(87.1784299465193,54.2271270458794,10.5788544315881));
#78222=CARTESIAN_POINT('Ctrl Pts',(87.1246464561318,54.2317242694714,10.608964815144));
#78223=CARTESIAN_POINT('Ctrl Pts',(87.0723881077518,54.2363214930635,10.6420584371157));
#78224=CARTESIAN_POINT('Ctrl Pts',(87.0220058687739,54.2409187166556,10.6779562528507));
#78225=CARTESIAN_POINT('Ctrl Pts',(86.9707609487516,54.2455946572267,10.7144687368853));
#78226=CARTESIAN_POINT('Ctrl Pts',(86.9214575001497,54.2502705977978,10.7538821732325));
#78227=CARTESIAN_POINT('Ctrl Pts',(86.8744389471863,54.254946538369,10.7959591310407));
#78228=CARTESIAN_POINT('Ctrl Pts',(86.8283390796325,54.2595311167414,10.8372139562058));
#78229=CARTESIAN_POINT('Ctrl Pts',(86.7844360200587,54.2641156951138,10.8810287992545));
#78230=CARTESIAN_POINT('Ctrl Pts',(86.7430223918915,54.2687002734862,10.9271375759402));
#78231=CARTESIAN_POINT('Ctrl Pts',(86.7016340750124,54.2732820498441,10.9732181717446));
#78232=CARTESIAN_POINT('Ctrl Pts',(86.6627325120772,54.2778638262021,11.0215895432681));
#78233=CARTESIAN_POINT('Ctrl Pts',(86.6265731589287,54.28244560256,11.0719491173378));
#78234=CARTESIAN_POINT('Ctrl Pts',(86.5904226245513,54.2870262614855,11.1222964093971));
#78235=CARTESIAN_POINT('Ctrl Pts',(86.5570132690835,54.2916069204109,11.1746305281004));
#78236=CARTESIAN_POINT('Ctrl Pts',(86.5265586935049,54.2961875793364,11.2286178631168));
#78237=CARTESIAN_POINT('Ctrl Pts',(86.4950038974746,54.3009337219219,11.2845555773123));
#78238=CARTESIAN_POINT('Ctrl Pts',(86.4666218026833,54.3056798645074,11.3422677701031));
#78239=CARTESIAN_POINT('Ctrl Pts',(86.441598119318,54.3104260070929,11.4013553035554));
#78240=CARTESIAN_POINT('Ctrl Pts',(86.4174163436591,54.3150124683893,11.4584548702869));
#78241=CARTESIAN_POINT('Ctrl Pts',(86.3963706809794,54.3195989296857,11.5168381751189));
#78242=CARTESIAN_POINT('Ctrl Pts',(86.3785787226685,54.3241853909821,11.5761269461223));
#78243=CARTESIAN_POINT('Ctrl Pts',(86.3598576026394,54.3290113742121,11.6385119955326));
#78244=CARTESIAN_POINT('Ctrl Pts',(86.3447395068377,54.3338373574422,11.7018990541506));
#78245=CARTESIAN_POINT('Ctrl Pts',(86.3333003915963,54.3386633406723,11.7658352792848));
#78246=CARTESIAN_POINT('Ctrl Pts',(86.3218612763549,54.3434893239023,11.8297715044191));
#78247=CARTESIAN_POINT('Ctrl Pts',(86.3141011422701,54.3483153071324,11.8942562434794));
#78248=CARTESIAN_POINT('Ctrl Pts',(86.3100325565661,54.3531412903625,11.9588338114055));
#78249=CARTESIAN_POINT('Ctrl Pts',(86.3077988381869,54.3557908320516,11.9942879251569));
#78250=CARTESIAN_POINT('Ctrl Pts',(86.3066734788713,54.3584403737407,12.0298125996632));
#78251=CARTESIAN_POINT('Ctrl Pts',(86.3066601203481,54.3610899154298,12.0653595093375));
#78252=CARTESIAN_POINT('',(86.3066603887547,55.1548399153721,12.0648488527018));
#78253=CARTESIAN_POINT('Ctrl Pts',(86.3066601203479,54.3610899154771,12.0653595099723));
#78254=CARTESIAN_POINT('Ctrl Pts',(86.306637159949,54.3656439064994,12.1264569851298));
#78255=CARTESIAN_POINT('Ctrl Pts',(86.3099038103981,54.3701978975217,12.1876878311977));
#78256=CARTESIAN_POINT('Ctrl Pts',(86.3164768878567,54.374751888544,12.2486643315267));
#78257=CARTESIAN_POINT('Ctrl Pts',(86.3230390949028,54.379298348275,12.3095399902466));
#78258=CARTESIAN_POINT('Ctrl Pts',(86.3328968232668,54.383844808006,12.3701616257491));
#78259=CARTESIAN_POINT('Ctrl Pts',(86.3460148865128,54.3883912677371,12.4301420155186));
#78260=CARTESIAN_POINT('Ctrl Pts',(86.3591209808625,54.3929335792868,12.4900676792935));
#78261=CARTESIAN_POINT('Ctrl Pts',(86.3754814072012,54.3974758908366,12.5493527512415));
#78262=CARTESIAN_POINT('Ctrl Pts',(86.3950094588118,54.4020182023863,12.6076173985299));
#78263=CARTESIAN_POINT('Ctrl Pts',(86.4145271930971,54.4065581140803,12.6658512626488));
#78264=CARTESIAN_POINT('Ctrl Pts',(86.4372090708181,54.4110980257744,12.7230652790075));
#78265=CARTESIAN_POINT('Ctrl Pts',(86.4629183718369,54.4156379374684,12.7788941773812));
#78266=CARTESIAN_POINT('Ctrl Pts',(86.4886239629771,54.4201771940485,12.8347150195872));
#78267=CARTESIAN_POINT('Ctrl Pts',(86.5173558919771,54.4247164506286,12.8891506693967));
#78268=CARTESIAN_POINT('Ctrl Pts',(86.5489299526732,54.4292557072087,12.9418573013396));
#78269=CARTESIAN_POINT('Ctrl Pts',(86.5805334836223,54.4337992005906,12.9946131280248));
#78270=CARTESIAN_POINT('Ctrl Pts',(86.6149841758236,54.4383426939726,13.0456362678403));
#78271=CARTESIAN_POINT('Ctrl Pts',(86.6520533418262,54.4428861873546,13.0946101379231));
#78272=CARTESIAN_POINT('Ctrl Pts',(86.6891405886908,54.4474318968716,13.1436078955082));
#78273=CARTESIAN_POINT('Ctrl Pts',(86.7288485154797,54.4519776063886,13.1905539970893));
#78274=CARTESIAN_POINT('Ctrl Pts',(86.770908834505,54.4565233159056,13.2351658294961));
#78275=CARTESIAN_POINT('Ctrl Pts',(86.813045320444,54.4610772572352,13.2798584493449));
#78276=CARTESIAN_POINT('Ctrl Pts',(86.8575423259244,54.4656311985648,13.3222080033695));
#78277=CARTESIAN_POINT('Ctrl Pts',(86.904096329719,54.4701851398943,13.3619703315734));
#78278=CARTESIAN_POINT('Ctrl Pts',(86.9346638294139,54.4731752715448,13.3880783965339));
#78279=CARTESIAN_POINT('Ctrl Pts',(86.9661174748064,54.4761654031953,13.4130718722357));
#78280=CARTESIAN_POINT('Ctrl Pts',(86.998364778829,54.4791555348458,13.4368919521407));
#78281=CARTESIAN_POINT('Ctrl Pts',(87.0479438891033,54.4837527584379,13.4735144979362));
#78282=CARTESIAN_POINT('Ctrl Pts',(87.0996140482451,54.4883499820299,13.5075191659228));
#78283=CARTESIAN_POINT('Ctrl Pts',(87.1530676211808,54.492947205622,13.5386597940372));
#78284=CARTESIAN_POINT('Ctrl Pts',(87.2074364647569,54.4976231461931,13.5703336344529));
#78285=CARTESIAN_POINT('Ctrl Pts',(87.2636500006559,54.5022990867642,13.5990440400659));
#78286=CARTESIAN_POINT('Ctrl Pts',(87.321350487704,54.5069750273354,13.6245757555505));
#78287=CARTESIAN_POINT('Ctrl Pts',(87.3779235773261,54.5115596057078,13.6496086123289));
#78288=CARTESIAN_POINT('Ctrl Pts',(87.4359255464466,54.5161441840802,13.6715856614817));
#78289=CARTESIAN_POINT('Ctrl Pts',(87.4949934502638,54.5207287624526,13.6903497395048));
#78290=CARTESIAN_POINT('Ctrl Pts',(87.554025252807,54.5253105388106,13.7091023492503));
#78291=CARTESIAN_POINT('Ctrl Pts',(87.6141212141056,54.5298923151685,13.7246457278236));
#78292=CARTESIAN_POINT('Ctrl Pts',(87.6749004332037,54.5344740915265,13.7368716039239));
#78293=CARTESIAN_POINT('Ctrl Pts',(87.7356648290827,54.5390547504519,13.7490944983005));
#78294=CARTESIAN_POINT('Ctrl Pts',(87.7971116531336,54.5436354093774,13.7580013960368));
#78295=CARTESIAN_POINT('Ctrl Pts',(87.8588489460954,54.5482160683028,13.7635349458541));
#78296=CARTESIAN_POINT('Ctrl Pts',(87.9228165979135,54.5529622108883,13.7692684040451));
#78297=CARTESIAN_POINT('Ctrl Pts',(87.9870955344131,54.5577083534738,13.7713799967936));
#78298=CARTESIAN_POINT('Ctrl Pts',(88.0512455570579,54.5624544960594,13.7698647630423));
#78299=CARTESIAN_POINT('Ctrl Pts',(88.1132372883896,54.5670409573558,13.7684005084755));
#78300=CARTESIAN_POINT('Ctrl Pts',(88.1751081224645,54.5716274186521,13.7635497258958));
#78301=CARTESIAN_POINT('Ctrl Pts',(88.2364649154011,54.5762138799485,13.7553609464893));
#78302=CARTESIAN_POINT('Ctrl Pts',(88.3010259864812,54.5810398631786,13.7467445188043));
#78303=CARTESIAN_POINT('Ctrl Pts',(88.3650172194607,54.5858658464087,13.7344319998631));
#78304=CARTESIAN_POINT('Ctrl Pts',(88.4279946468341,54.5906918296387,13.718540559294));
#78305=CARTESIAN_POINT('Ctrl Pts',(88.4909720742074,54.5955178128688,13.7026491187249));
#78306=CARTESIAN_POINT('Ctrl Pts',(88.5529351009836,54.6003437960989,13.6831790245952));
#78307=CARTESIAN_POINT('Ctrl Pts',(88.6134632606434,54.605169779329,13.6603063868576));
#78308=CARTESIAN_POINT('Ctrl Pts',(88.6711222847858,54.609767002921,13.6385179502204));
#78309=CARTESIAN_POINT('Ctrl Pts',(88.7277161566771,54.6143642265131,13.6135528454747));
#78310=CARTESIAN_POINT('Ctrl Pts',(88.7828712094735,54.6189614501052,13.5855360053602));
#78311=CARTESIAN_POINT('Ctrl Pts',(88.8389706668758,54.6236373906763,13.5570394406963));
#78312=CARTESIAN_POINT('Ctrl Pts',(88.8935810387959,54.6283133312474,13.5253857475867));
#78313=CARTESIAN_POINT('Ctrl Pts',(88.9463274463073,54.6329892718186,13.4907587177428));
#78314=CARTESIAN_POINT('Ctrl Pts',(88.9980432530891,54.637573850191,13.4568082579993));
#78315=CARTESIAN_POINT('Ctrl Pts',(89.0479668336628,54.6421584285634,13.4199999000623));
#78316=CARTESIAN_POINT('Ctrl Pts',(89.0957692908299,54.6467430069358,13.3805533162532));
#78317=CARTESIAN_POINT('Ctrl Pts',(89.1435425319678,54.6513247832938,13.3411308415091));
#78318=CARTESIAN_POINT('Ctrl Pts',(89.1891968284483,54.6559065596517,13.2990736614473));
#78319=CARTESIAN_POINT('Ctrl Pts',(89.2324346190519,54.6604883360097,13.254643052805));
#78320=CARTESIAN_POINT('Ctrl Pts',(89.2756618645504,54.6650689949351,13.2102232801798));
#78321=CARTESIAN_POINT('Ctrl Pts',(89.3164734192652,54.6696496538606,13.1634315927237));
#78322=CARTESIAN_POINT('Ctrl Pts',(89.3546085029542,54.674230312786,13.1145661764473));
#78323=CARTESIAN_POINT('Ctrl Pts',(89.3941212777851,54.6789764553715,13.0639354185317));
#78324=CARTESIAN_POINT('Ctrl Pts',(89.4307600872057,54.6837225979571,13.011078648429));
#78325=CARTESIAN_POINT('Ctrl Pts',(89.4642820001852,54.6884687405426,12.9563629953776));
#78326=CARTESIAN_POINT('Ctrl Pts',(89.4966760873183,54.693055201839,12.9034882195979));
#78327=CARTESIAN_POINT('Ctrl Pts',(89.5261595060493,54.6976416631354,12.848878163558));
#78328=CARTESIAN_POINT('Ctrl Pts',(89.5525597877001,54.7022281244318,12.7928894390111));
#78329=CARTESIAN_POINT('Ctrl Pts',(89.58033878948,54.7070541076618,12.733976776661));
#78330=CARTESIAN_POINT('Ctrl Pts',(89.604703547265,54.7118800908919,12.6735380920378));
#78331=CARTESIAN_POINT('Ctrl Pts',(89.6255116903145,54.716706074122,12.6120099243034));
#78332=CARTESIAN_POINT('Ctrl Pts',(89.646319833364,54.721532057352,12.550481756569));
#78333=CARTESIAN_POINT('Ctrl Pts',(89.6635712641648,54.7263580405821,12.4878647509873));
#78334=CARTESIAN_POINT('Ctrl Pts',(89.6771858758965,54.7311840238122,12.4246076722034));
#78335=CARTESIAN_POINT('Ctrl Pts',(89.6901551323704,54.7357812474042,12.3643490842458));
#78336=CARTESIAN_POINT('Ctrl Pts',(89.69987786545,54.7403784709963,12.3032623323918));
#78337=CARTESIAN_POINT('Ctrl Pts',(89.7062563573408,54.7449756945884,12.2417291054314));
#78338=CARTESIAN_POINT('Ctrl Pts',(89.7127440663715,54.7496516351595,12.1791422621653));
#78339=CARTESIAN_POINT('Ctrl Pts',(89.7157717268321,54.7543275757306,12.1160940085744));
#78340=CARTESIAN_POINT('Ctrl Pts',(89.7152904121643,54.7590035163018,12.0529989767782));
#78341=CARTESIAN_POINT('Ctrl Pts',(89.7148185018005,54.7635880946742,11.9911367452594));
#78342=CARTESIAN_POINT('Ctrl Pts',(89.7109735093815,54.7681726730466,11.9292300804759));
#78343=CARTESIAN_POINT('Ctrl Pts',(89.7037615928417,54.772757251419,11.8676744459228));
#78344=CARTESIAN_POINT('Ctrl Pts',(89.6965540840997,54.777339027777,11.8061564331013));
#78345=CARTESIAN_POINT('Ctrl Pts',(89.68598379068,54.7819208041349,11.7449895296412));
#78346=CARTESIAN_POINT('Ctrl Pts',(89.6721088198636,54.7865025804929,11.6845654392017));
#78347=CARTESIAN_POINT('Ctrl Pts',(89.6582372329626,54.7910832394183,11.6241560853704));
#78348=CARTESIAN_POINT('Ctrl Pts',(89.6410626825035,54.7956638983438,11.5644896808385));
#78349=CARTESIAN_POINT('Ctrl Pts',(89.6206942339859,54.8002445572692,11.5059470483316));
#78350=CARTESIAN_POINT('Ctrl Pts',(89.5995899425547,54.8049906998547,11.4452894692081));
#78351=CARTESIAN_POINT('Ctrl Pts',(89.5750566958746,54.8097368424403,11.3858389830133));
#78352=CARTESIAN_POINT('Ctrl Pts',(89.5472711615009,54.8144829850258,11.3279988116943));
#78353=CARTESIAN_POINT('Ctrl Pts',(89.5204204557523,54.8190694463222,11.272104640301));
#78354=CARTESIAN_POINT('Ctrl Pts',(89.4905331613785,54.8236559076186,11.2177145691873));
#78355=CARTESIAN_POINT('Ctrl Pts',(89.4578153286656,54.8282423689149,11.1651669187146));
#78356=CARTESIAN_POINT('Ctrl Pts',(89.4233888499944,54.833068352145,11.1098750360249));
#78357=CARTESIAN_POINT('Ctrl Pts',(89.3858284459847,54.8378943353751,11.0566238194046));
#78358=CARTESIAN_POINT('Ctrl Pts',(89.3454236407146,54.8427203186052,11.0057696558286));
#78359=CARTESIAN_POINT('Ctrl Pts',(89.3050188354446,54.8475463018352,10.9549154922525));
#78360=CARTESIAN_POINT('Ctrl Pts',(89.2617701181232,54.8523722850653,10.906458813634));
#78361=CARTESIAN_POINT('Ctrl Pts',(89.2160110555889,54.8571982682954,10.8607103287971));
#78362=CARTESIAN_POINT('Ctrl Pts',(89.1724210487852,54.8617954918875,10.8171303982902));
#78363=CARTESIAN_POINT('Ctrl Pts',(89.1263743736857,54.8663927154796,10.7758287457457));
#78364=CARTESIAN_POINT('Ctrl Pts',(89.078138693113,54.8709899390716,10.7370944934793));
#78365=CARTESIAN_POINT('Ctrl Pts',(89.0290770864174,54.8756658796428,10.6976970054004));
#78366=CARTESIAN_POINT('Ctrl Pts',(88.9777511130749,54.8803418202139,10.6609561089882));
#78367=CARTESIAN_POINT('Ctrl Pts',(88.9244825766025,54.885017760785,10.6271378044289));
#78368=CARTESIAN_POINT('Ctrl Pts',(88.8722548426254,54.8896023391574,10.5939802684603));
#78369=CARTESIAN_POINT('Ctrl Pts',(88.8181602237876,54.8941869175299,10.5636324295897));
#78370=CARTESIAN_POINT('Ctrl Pts',(88.7625342973995,54.8987714959023,10.5363036133166));
#78371=CARTESIAN_POINT('Ctrl Pts',(88.7069423686088,54.9033532722602,10.5089914999401));
#78372=CARTESIAN_POINT('Ctrl Pts',(88.6498214439763,54.9079350486182,10.4846949744478));
#78373=CARTESIAN_POINT('Ctrl Pts',(88.5915321193561,54.9125168249761,10.4635776792631));
#78374=CARTESIAN_POINT('Ctrl Pts',(88.5332570107039,54.9170974839016,10.4424655342974));
#78375=CARTESIAN_POINT('Ctrl Pts',(88.4738145461388,54.9216781428271,10.4245312537248));
#78376=CARTESIAN_POINT('Ctrl Pts',(88.413583819887,54.9262588017525,10.4098897670852));
#78377=CARTESIAN_POINT('Ctrl Pts',(88.3511771619209,54.931004944338,10.3947193332269));
#78378=CARTESIAN_POINT('Ctrl Pts',(88.287924747194,54.9357510869235,10.3830843629789));
#78379=CARTESIAN_POINT('Ctrl Pts',(88.2242611552639,54.9404972295091,10.3750551412729));
#78380=CARTESIAN_POINT('Ctrl Pts',(88.16273948896,54.9450836908055,10.3672960582005));
#78381=CARTESIAN_POINT('Ctrl Pts',(88.1008344072298,54.9496701521019,10.3629038996506));
#78382=CARTESIAN_POINT('Ctrl Pts',(88.038941901592,54.9542566133983,10.3618890629612));
#78383=CARTESIAN_POINT('Ctrl Pts',(87.9738171409165,54.9590825966283,10.3608212277549));
#78384=CARTESIAN_POINT('Ctrl Pts',(87.9087069497816,54.9639085798584,10.3634931243255));
#78385=CARTESIAN_POINT('Ctrl Pts',(87.8440677739317,54.9687345630885,10.3698548212196));
#78386=CARTESIAN_POINT('Ctrl Pts',(87.7794285980819,54.9735605463185,10.3762165181138));
#78387=CARTESIAN_POINT('Ctrl Pts',(87.7152610657229,54.9783865295486,10.386267838606));
#78388=CARTESIAN_POINT('Ctrl Pts',(87.6520071361564,54.9832125127787,10.399897074215));
#78389=CARTESIAN_POINT('Ctrl Pts',(87.591751548138,54.9878097363708,10.4128802613702));
#78390=CARTESIAN_POINT('Ctrl Pts',(87.5320774958243,54.9924069599628,10.4291630827193));
#78391=CARTESIAN_POINT('Ctrl Pts',(87.4733730569773,54.9970041835549,10.4486774886449));
#78392=CARTESIAN_POINT('Ctrl Pts',(87.4136634383757,55.0016801241261,10.4685260343075));
#78393=CARTESIAN_POINT('Ctrl Pts',(87.3549574890073,55.0063560646972,10.491717854363));
#78394=CARTESIAN_POINT('Ctrl Pts',(87.2976532270897,55.0110320052683,10.5181268730356));
#78395=CARTESIAN_POINT('Ctrl Pts',(87.2414686208403,55.0156165836407,10.5440198915635));
#78396=CARTESIAN_POINT('Ctrl Pts',(87.1866319045675,55.0202011620131,10.573005295817));
#78397=CARTESIAN_POINT('Ctrl Pts',(87.1335009537733,55.0247857403855,10.6049146980853));
#78398=CARTESIAN_POINT('Ctrl Pts',(87.0804024756907,55.0293675167435,10.6368045978827));
#78399=CARTESIAN_POINT('Ctrl Pts',(87.0290081313791,55.0339492931015,10.6716146905955));
#78400=CARTESIAN_POINT('Ctrl Pts',(86.9796509870481,55.0385310694594,10.7091307914603));
#78401=CARTESIAN_POINT('Ctrl Pts',(86.9303058802488,55.0431117283849,10.7466377426618));
#78402=CARTESIAN_POINT('Ctrl Pts',(86.8829973922011,55.0476923873103,10.7868490839957));
#78403=CARTESIAN_POINT('Ctrl Pts',(86.8380276978842,55.0522730462358,10.829508668017));
#78404=CARTESIAN_POINT('Ctrl Pts',(86.7914334011402,55.0570191888213,10.8737093980209));
#78405=CARTESIAN_POINT('Ctrl Pts',(86.7473505848034,55.0617653314068,10.920538297274));
#78406=CARTESIAN_POINT('Ctrl Pts',(86.7060740121473,55.0665114739923,10.9696683887497));
#78407=CARTESIAN_POINT('Ctrl Pts',(86.6661861664865,55.0710979352887,11.0171455260211));
#78408=CARTESIAN_POINT('Ctrl Pts',(86.628918981345,55.0756843965851,11.0667709944056));
#78409=CARTESIAN_POINT('Ctrl Pts',(86.5944959770564,55.0802708578815,11.1182177525482));
#78410=CARTESIAN_POINT('Ctrl Pts',(86.5582752764576,55.0850968411115,11.1723512502478));
#78411=CARTESIAN_POINT('Ctrl Pts',(86.5252043061989,55.0899228243416,11.2285009336578));
#78412=CARTESIAN_POINT('Ctrl Pts',(86.4954886934164,55.0947488075717,11.2862562502865));
#78413=CARTESIAN_POINT('Ctrl Pts',(86.4657730806339,55.0995747908017,11.3440115669152));
#78414=CARTESIAN_POINT('Ctrl Pts',(86.4394130175949,55.1044007740318,11.4033718931378));
#78415=CARTESIAN_POINT('Ctrl Pts',(86.416554373818,55.1092267572618,11.4639053390463));
#78416=CARTESIAN_POINT('Ctrl Pts',(86.3916467123487,55.1144853350552,11.5298649205931));
#78417=CARTESIAN_POINT('Ctrl Pts',(86.3708096801981,55.1197439128485,11.5974413574462));
#78418=CARTESIAN_POINT('Ctrl Pts',(86.3542262509689,55.1250024906418,11.666155555095));
#78419=CARTESIAN_POINT('Ctrl Pts',(86.3377777976361,55.1302182678031,11.7343104739421));
#78420=CARTESIAN_POINT('Ctrl Pts',(86.3255140956074,55.1354340449644,11.8035845018164));
#78421=CARTESIAN_POINT('Ctrl Pts',(86.317567286777,55.1406498221257,11.8734890097));
#78422=CARTESIAN_POINT('Ctrl Pts',(86.3103605653991,55.1453798532078,11.9368833006832));
#78423=CARTESIAN_POINT('Ctrl Pts',(86.3067036515886,55.1501098842899,12.0007957452571));
#78424=CARTESIAN_POINT('Ctrl Pts',(86.3066603887547,55.154839915372,12.0648488527018));
#78425=CARTESIAN_POINT('',(86.3066604846332,55.9485899154847,12.0672852856579));
#78426=CARTESIAN_POINT('Ctrl Pts',(86.3066603887541,55.1548399154298,12.0648488534838));
#78427=CARTESIAN_POINT('Ctrl Pts',(86.3066182940265,55.1594422377324,12.1271725549211));
#78428=CARTESIAN_POINT('Ctrl Pts',(86.3099990779096,55.164044560035,12.1895184871938));
#78429=CARTESIAN_POINT('Ctrl Pts',(86.3167835349057,55.1686468823377,12.2514869402501));
#78430=CARTESIAN_POINT('Ctrl Pts',(86.3235683082009,55.1732494192058,12.313458282347));
#78431=CARTESIAN_POINT('Ctrl Pts',(86.3337570130611,55.177851956074,12.3750516114809));
#78432=CARTESIAN_POINT('Ctrl Pts',(86.3472786724264,55.1824544929422,12.435873194185));
#78433=CARTESIAN_POINT('Ctrl Pts',(86.3608164302688,55.1870625094511,12.4967671892192));
#78434=CARTESIAN_POINT('Ctrl Pts',(86.3776949568103,55.1916705259599,12.5568871118524));
#78435=CARTESIAN_POINT('Ctrl Pts',(86.3977925109203,55.1962785424688,12.6158512824183));
#78436=CARTESIAN_POINT('Ctrl Pts',(86.4179021109743,55.2008893209012,12.6748507945534));
#78437=CARTESIAN_POINT('Ctrl Pts',(86.4412343924767,55.2055000993337,12.7326927090471));
#78438=CARTESIAN_POINT('Ctrl Pts',(86.4676193647064,55.2101108777661,12.7890152489407));
#78439=CARTESIAN_POINT('Ctrl Pts',(86.4940582244476,55.2147310730505,12.8454528195224));
#78440=CARTESIAN_POINT('Ctrl Pts',(86.5235619915821,55.2193512683348,12.9003643732525));
#78441=CARTESIAN_POINT('Ctrl Pts',(86.5559149500569,55.2239714636191,12.9534132819787));
#78442=CARTESIAN_POINT('Ctrl Pts',(86.5822199636318,55.2277279763278,12.9965454198097));
#78443=CARTESIAN_POINT('Ctrl Pts',(86.6104075793017,55.2314844890364,13.0384466472158));
#78444=CARTESIAN_POINT('Ctrl Pts',(86.6403421930249,55.2352410017451,13.078952127091));
#78445=CARTESIAN_POINT('Ctrl Pts',(86.6769761999087,55.2398382253372,13.1285227693683));
#78446=CARTESIAN_POINT('Ctrl Pts',(86.7163780016629,55.2444354489293,13.1762052693987));
#78447=CARTESIAN_POINT('Ctrl Pts',(86.7583258449082,55.2490326725214,13.2216739578121));
#78448=CARTESIAN_POINT('Ctrl Pts',(86.8009919493891,55.2537086130925,13.2679211939122));
#78449=CARTESIAN_POINT('Ctrl Pts',(86.8462918675474,55.2583845536636,13.3118776089568));
#78450=CARTESIAN_POINT('Ctrl Pts',(86.8939468716422,55.2630604942347,13.3532323582112));
#78451=CARTESIAN_POINT('Ctrl Pts',(86.9406707548454,55.2676450726072,13.3937790859005));
#78452=CARTESIAN_POINT('Ctrl Pts',(86.9896581177633,55.2722296509796,13.4318245506194));
#78453=CARTESIAN_POINT('Ctrl Pts',(87.040608194221,55.276814229352,13.4671119080491));
#78454=CARTESIAN_POINT('Ctrl Pts',(87.0915271308794,55.28139600571,13.5023776984606));
#78455=CARTESIAN_POINT('Ctrl Pts',(87.1444059848795,55.2859777820679,13.5348884348643));
#78456=CARTESIAN_POINT('Ctrl Pts',(87.1989124640647,55.2905595584259,13.5644287335668));
#78457=CARTESIAN_POINT('Ctrl Pts',(87.253405649866,55.2951402173513,13.593961827795));
#78458=CARTESIAN_POINT('Ctrl Pts',(87.3095252254899,55.2997208762768,13.62052568002));
#78459=CARTESIAN_POINT('Ctrl Pts',(87.3669133706643,55.3043015352022,13.643950331763));
#78460=CARTESIAN_POINT('Ctrl Pts',(87.4263747547465,55.3090476777877,13.6682212366693));
#78461=CARTESIAN_POINT('Ctrl Pts',(87.4871976074236,55.3137938203733,13.6891215020663));
#78462=CARTESIAN_POINT('Ctrl Pts',(87.5489626077904,55.3185399629588,13.70651707818));
#78463=CARTESIAN_POINT('Ctrl Pts',(87.608649559573,55.3231264242552,13.7233273899514));
#78464=CARTESIAN_POINT('Ctrl Pts',(87.6692157346942,55.3277128855516,13.7368650644912));
#78465=CARTESIAN_POINT('Ctrl Pts',(87.7302710777268,55.332299346848,13.7470610065668));
#78466=CARTESIAN_POINT('Ctrl Pts',(87.7945149560764,55.337125330078,13.7577894183622));
#78467=CARTESIAN_POINT('Ctrl Pts',(87.8592998566214,55.3419513133081,13.7648174111248));
#78468=CARTESIAN_POINT('Ctrl Pts',(87.924166980079,55.3467772965382,13.7681265705732));
#78469=CARTESIAN_POINT('Ctrl Pts',(87.9890341035366,55.3516032797682,13.7714357300217));
#78470=CARTESIAN_POINT('Ctrl Pts',(88.0539828024207,55.3564292629983,13.7710261376193));
#78471=CARTESIAN_POINT('Ctrl Pts',(88.1185594280151,55.3612552462284,13.7669426225023));
#78472=CARTESIAN_POINT('Ctrl Pts',(88.1800750140681,55.3658524698204,13.7630526727989));
#78473=CARTESIAN_POINT('Ctrl Pts',(88.2415055803598,55.3704496934125,13.755813314009));
#78474=CARTESIAN_POINT('Ctrl Pts',(88.3024572463992,55.3750469170046,13.7452342031776));
#78475=CARTESIAN_POINT('Ctrl Pts',(88.3644525708386,55.3797228575757,13.7344739491781));
#78476=CARTESIAN_POINT('Ctrl Pts',(88.4259519052912,55.3843987981468,13.7202584340412));
#78477=CARTESIAN_POINT('Ctrl Pts',(88.4865429209327,55.389074738718,13.7026532210431));
#78478=CARTESIAN_POINT('Ctrl Pts',(88.5459500617308,55.3936593170904,13.6853919925213));
#78479=CARTESIAN_POINT('Ctrl Pts',(88.6044835471508,55.3982438954628,13.6648724848301));
#78480=CARTESIAN_POINT('Ctrl Pts',(88.661764461642,55.4028284738352,13.6412080659595));
#78481=CARTESIAN_POINT('Ctrl Pts',(88.7190103670358,55.4074102501932,13.6175581103696));
#78482=CARTESIAN_POINT('Ctrl Pts',(88.7750047499725,55.4119920265511,13.5907672488416));
#78483=CARTESIAN_POINT('Ctrl Pts',(88.8293864271967,55.4165738029091,13.5609978232025));
#78484=CARTESIAN_POINT('Ctrl Pts',(88.8837548414746,55.4211544618345,13.5312356579186));
#78485=CARTESIAN_POINT('Ctrl Pts',(88.936510884512,55.42573512076,13.498496614923));
#78486=CARTESIAN_POINT('Ctrl Pts',(88.9873176893197,55.4303157796854,13.4629891213326));
#78487=CARTESIAN_POINT('Ctrl Pts',(89.039959971545,55.4350619222709,13.4261988625124));
#78488=CARTESIAN_POINT('Ctrl Pts',(89.0905089670408,55.4398080648565,13.3864365744015));
#78489=CARTESIAN_POINT('Ctrl Pts',(89.1386246186138,55.444554207442,13.3439818289381));
#78490=CARTESIAN_POINT('Ctrl Pts',(89.1851214462405,55.4491406687384,13.3029554494294));
#78491=CARTESIAN_POINT('Ctrl Pts',(89.2293457516953,55.4537271300347,13.2594153413936));
#78492=CARTESIAN_POINT('Ctrl Pts',(89.2710279210297,55.4583135913311,13.2136517214842));
#78493=CARTESIAN_POINT('Ctrl Pts',(89.3148868870606,55.4631395745612,13.165498156468));
#78494=CARTESIAN_POINT('Ctrl Pts',(89.3559305024903,55.4679655577913,13.1148829645452));
#78495=CARTESIAN_POINT('Ctrl Pts',(89.3938944449276,55.4727915410214,13.0621816048233));
#78496=CARTESIAN_POINT('Ctrl Pts',(89.431858387365,55.4776175242514,13.0094802451013));
#78497=CARTESIAN_POINT('Ctrl Pts',(89.4667423740536,55.4824435074815,12.9546933057325));
#78498=CARTESIAN_POINT('Ctrl Pts',(89.4983380083971,55.4872694907116,12.8982262218755));
#78499=CARTESIAN_POINT('Ctrl Pts',(89.5284359570816,55.4918667143036,12.8444357717834));
#78500=CARTESIAN_POINT('Ctrl Pts',(89.555673881669,55.4964639378957,12.788900033247));
#78501=CARTESIAN_POINT('Ctrl Pts',(89.5798462549563,55.5010611614878,12.7319551515752));
#78502=CARTESIAN_POINT('Ctrl Pts',(89.6044325250584,55.5057371020589,12.674035218556));
#78503=CARTESIAN_POINT('Ctrl Pts',(89.6258469327725,55.51041304263,12.6146578478582));
#78504=CARTESIAN_POINT('Ctrl Pts',(89.6439209125508,55.5150889832012,12.5542050070967));
#78505=CARTESIAN_POINT('Ctrl Pts',(89.6616417487194,55.5196735615736,12.4949333414091));
#78506=CARTESIAN_POINT('Ctrl Pts',(89.6761513659806,55.524258139946,12.4346283655096));
#78507=CARTESIAN_POINT('Ctrl Pts',(89.6873394838569,55.5288427183184,12.3736699050319));
#78508=CARTESIAN_POINT('Ctrl Pts',(89.6985207637504,55.5334244946764,12.3127487013035));
#78509=CARTESIAN_POINT('Ctrl Pts',(89.7063844778368,55.5380062710343,12.2511753045915));
#78510=CARTESIAN_POINT('Ctrl Pts',(89.7108711075708,55.5425880473923,12.1893412066015));
#78511=CARTESIAN_POINT('Ctrl Pts',(89.7153566430773,55.5471687063177,12.1275221891014));
#78512=CARTESIAN_POINT('Ctrl Pts',(89.7164666924284,55.5517493652432,12.065443104027));
#78513=CARTESIAN_POINT('Ctrl Pts',(89.7141936434196,55.5563300241686,12.0035000110784));
#78514=CARTESIAN_POINT('Ctrl Pts',(89.7118384768648,55.5610761667541,11.9393191244186));
#78515=CARTESIAN_POINT('Ctrl Pts',(89.7058510494495,55.5658223093397,11.8752848272459));
#78516=CARTESIAN_POINT('Ctrl Pts',(89.6962817888767,55.5705684519252,11.8118344482814));
#78517=CARTESIAN_POINT('Ctrl Pts',(89.6870344806762,55.5751549132216,11.7505188215132));
#78518=CARTESIAN_POINT('Ctrl Pts',(89.674442722707,55.5797413745179,11.689748945489));
#78519=CARTESIAN_POINT('Ctrl Pts',(89.6586040938518,55.5843278358143,11.6299087417493));
#78520=CARTESIAN_POINT('Ctrl Pts',(89.6419383133507,55.5891538190444,11.5669434617502));
#78521=CARTESIAN_POINT('Ctrl Pts',(89.6216774252868,55.5939798022745,11.5050082340056));
#78522=CARTESIAN_POINT('Ctrl Pts',(89.597993492667,55.5988057855046,11.4445287699076));
#78523=CARTESIAN_POINT('Ctrl Pts',(89.5743095600472,55.6036317687346,11.3840493058095));
#78524=CARTESIAN_POINT('Ctrl Pts',(89.547202923624,55.6084577519647,11.3250261619207));
#78525=CARTESIAN_POINT('Ctrl Pts',(89.5169011640017,55.6132837351948,11.2678543241623));
#78526=CARTESIAN_POINT('Ctrl Pts',(89.488035758223,55.6178809587869,11.2133925266766));
#78527=CARTESIAN_POINT('Ctrl Pts',(89.4561528251404,55.6224781823789,11.1603868536909));
#78528=CARTESIAN_POINT('Ctrl Pts',(89.4214232898435,55.627075405971,11.1091922977594));
#78529=CARTESIAN_POINT('Ctrl Pts',(89.3860990903874,55.6317513465421,11.0571211517064));
#78530=CARTESIAN_POINT('Ctrl Pts',(89.3478300524464,55.6364272871133,11.0069242420028));
#78531=CARTESIAN_POINT('Ctrl Pts',(89.3068456453556,55.6411032276844,10.9589503628957));
#78532=CARTESIAN_POINT('Ctrl Pts',(89.266662023794,55.6456878060568,10.9119138351105));
#78533=CARTESIAN_POINT('Ctrl Pts',(89.2238685352838,55.6502723844292,10.867014654133));
#78534=CARTESIAN_POINT('Ctrl Pts',(89.1787244633868,55.6548569628016,10.8245514858811));
#78535=CARTESIAN_POINT('Ctrl Pts',(89.1336079827603,55.6594387391596,10.7821142703782));
#78536=CARTESIAN_POINT('Ctrl Pts',(89.0861441374107,55.6640205155175,10.7421104634781));
#78537=CARTESIAN_POINT('Ctrl Pts',(89.0366295450226,55.6686022918755,10.7048024125878));
#78538=CARTESIAN_POINT('Ctrl Pts',(88.9871270285655,55.6731829508009,10.6675034606202));
#78539=CARTESIAN_POINT('Ctrl Pts',(88.9355751643183,55.6777636097264,10.6328992657033));
#78540=CARTESIAN_POINT('Ctrl Pts',(88.8823025615691,55.6823442686518,10.6012110453027));
#78541=CARTESIAN_POINT('Ctrl Pts',(88.8271054004916,55.6870904112373,10.5683780370499));
#78542=CARTESIAN_POINT('Ctrl Pts',(88.7700612585478,55.6918365538228,10.538676078001));
#78543=CARTESIAN_POINT('Ctrl Pts',(88.7115648967786,55.6965826964084,10.5123000093321));
#78544=CARTESIAN_POINT('Ctrl Pts',(88.6550366120927,55.7011691577048,10.48681134861));
#78545=CARTESIAN_POINT('Ctrl Pts',(88.5971527987433,55.7057556190011,10.4644284454721));
#78546=CARTESIAN_POINT('Ctrl Pts',(88.5382889240096,55.7103420802975,10.4452775604019));
#78547=CARTESIAN_POINT('Ctrl Pts',(88.4763509605202,55.7151680635276,10.4251265454436));
#78548=CARTESIAN_POINT('Ctrl Pts',(88.4133283838417,55.7199940467577,10.4085545555291));
#78549=CARTESIAN_POINT('Ctrl Pts',(88.3496721698896,55.7248200299878,10.3956479422163));
#78550=CARTESIAN_POINT('Ctrl Pts',(88.2860159559375,55.7296460132178,10.3827413289034));
#78551=CARTESIAN_POINT('Ctrl Pts',(88.2217267571155,55.7344719964479,10.3735001077978));
#78552=CARTESIAN_POINT('Ctrl Pts',(88.1572598488965,55.739297979678,10.3679473234906));
#78553=CARTESIAN_POINT('Ctrl Pts',(88.0958487794327,55.74389520327,10.3626577504022));
#78554=CARTESIAN_POINT('Ctrl Pts',(88.0340243279118,55.7484924268621,10.3606930660133));
#78555=CARTESIAN_POINT('Ctrl Pts',(87.9721774406511,55.7530896504542,10.3621022200597));
#78556=CARTESIAN_POINT('Ctrl Pts',(87.9092715663668,55.7577655910253,10.3635355026583));
#78557=CARTESIAN_POINT('Ctrl Pts',(87.8463430009672,55.7624415315965,10.3684593898906));
#78558=CARTESIAN_POINT('Ctrl Pts',(87.7838092377672,55.7671174721676,10.3768702852782));
#78559=CARTESIAN_POINT('Ctrl Pts',(87.7224973083379,55.77170205054,10.385116841987));
#78560=CARTESIAN_POINT('Ctrl Pts',(87.6615654206068,55.7762866289124,10.3967152974373));
#78561=CARTESIAN_POINT('Ctrl Pts',(87.6014051252175,55.7808712072848,10.4116098180441));
#78562=CARTESIAN_POINT('Ctrl Pts',(87.5412815987531,55.7854529836428,10.4264952353793));
#78563=CARTESIAN_POINT('Ctrl Pts',(87.4819292226512,55.7900347600007,10.4446726013306));
#78564=CARTESIAN_POINT('Ctrl Pts',(87.4237292855877,55.7946165363587,10.4660350180102));
#78565=CARTESIAN_POINT('Ctrl Pts',(87.3655435426919,55.7991971952841,10.4873922246889));
#78566=CARTESIAN_POINT('Ctrl Pts',(87.3085101585382,55.8037778542096,10.5119327647239));
#78567=CARTESIAN_POINT('Ctrl Pts',(87.2529932198747,55.808358513135,10.5395005545746));
#78568=CARTESIAN_POINT('Ctrl Pts',(87.1954706426435,55.8131046557205,10.5680642751067));
#78569=CARTESIAN_POINT('Ctrl Pts',(87.1395767259984,55.817850798306,10.5998779605821));
#78570=CARTESIAN_POINT('Ctrl Pts',(87.0856892780369,55.8225969408916,10.6347156455057));
#78571=CARTESIAN_POINT('Ctrl Pts',(87.0336148428542,55.827183402188,10.6683812361785));
#78572=CARTESIAN_POINT('Ctrl Pts',(86.9834143832994,55.8317698634844,10.7048701942512));
#78573=CARTESIAN_POINT('Ctrl Pts',(86.9353976264655,55.8363563247808,10.7439355652439));
#78574=CARTESIAN_POINT('Ctrl Pts',(86.8848732574003,55.8411823080108,10.7850410740672));
#78575=CARTESIAN_POINT('Ctrl Pts',(86.8367674101936,55.8460082912409,10.8289990481498));
#78576=CARTESIAN_POINT('Ctrl Pts',(86.7913972393957,55.850834274471,10.8754774500554));
#78577=CARTESIAN_POINT('Ctrl Pts',(86.7460270685979,55.8556602577011,10.9219558519611));
#78578=CARTESIAN_POINT('Ctrl Pts',(86.7033929411827,55.8604862409311,10.9709541420561));
#78579=CARTESIAN_POINT('Ctrl Pts',(86.6637611582523,55.8653122241612,11.022102333135));
#78580=CARTESIAN_POINT('Ctrl Pts',(86.6259913092781,55.8699114787058,11.0708475398733));
#78581=CARTESIAN_POINT('Ctrl Pts',(86.5907903728854,55.8745107332503,11.1217484975243));
#78582=CARTESIAN_POINT('Ctrl Pts',(86.5584127681868,55.8791099877949,11.1745039710839));
#78583=CARTESIAN_POINT('Ctrl Pts',(86.5260846539442,55.883702212196,11.2271788058047));
#78584=CARTESIAN_POINT('Ctrl Pts',(86.4965715781281,55.8882944365972,11.281702107454));
#78585=CARTESIAN_POINT('Ctrl Pts',(86.4700867789411,55.8928866609983,11.3377409246938));
#78586=CARTESIAN_POINT('Ctrl Pts',(86.4433152665828,55.8975285988676,11.3943863943342));
#78587=CARTESIAN_POINT('Ctrl Pts',(86.4196383236701,55.9021705367369,11.4525799769534));
#78588=CARTESIAN_POINT('Ctrl Pts',(86.3992298158745,55.9068124746062,11.5119497232524));
#78589=CARTESIAN_POINT('Ctrl Pts',(86.3790787614473,55.9113958544196,11.5705705200782));
#78590=CARTESIAN_POINT('Ctrl Pts',(86.3621143073747,55.915979234233,11.6303374781457));
#78591=CARTESIAN_POINT('Ctrl Pts',(86.3484555539935,55.9205626140464,11.6908722875434));
#78592=CARTESIAN_POINT('Ctrl Pts',(86.334535040707,55.9252338309437,11.752567201786));
#78593=CARTESIAN_POINT('Ctrl Pts',(86.3240484533583,55.9299050478409,11.8150591982026));
#78594=CARTESIAN_POINT('Ctrl Pts',(86.3170678817167,55.9345762647382,11.8779340162383));
#78595=CARTESIAN_POINT('Ctrl Pts',(86.3100873100751,55.9392474816354,11.9408088342741));
#78596=CARTESIAN_POINT('Ctrl Pts',(86.3066128093318,55.9439186985327,12.0040659176332));
#78597=CARTESIAN_POINT('Ctrl Pts',(86.3066604846326,55.9485899154299,12.067285284916));
#78598=CARTESIAN_POINT('',(86.3066600510811,56.7423399153589,12.0664172756536));
#78599=CARTESIAN_POINT('Ctrl Pts',(86.3066604846332,55.9485899154847,12.0672852856579));
#78600=CARTESIAN_POINT('Ctrl Pts',(86.3067146504435,55.9538970682025,12.1391112882315));
#78601=CARTESIAN_POINT('Ctrl Pts',(86.3113132460109,55.9592042209202,12.2107507526871));
#78602=CARTESIAN_POINT('Ctrl Pts',(86.3203621123175,55.964511373638,12.2816811728741));
#78603=CARTESIAN_POINT('Ctrl Pts',(86.3295034461463,55.9698727584823,12.3533364087442));
#78604=CARTESIAN_POINT('Ctrl Pts',(86.3431863562652,55.9752341433265,12.4242678780687));
#78605=CARTESIAN_POINT('Ctrl Pts',(86.3612643699134,55.9805955281708,12.4939569913238));
#78606=CARTESIAN_POINT('Ctrl Pts',(86.3733255626821,55.9841725083287,12.5404518023802));
#78607=CARTESIAN_POINT('Ctrl Pts',(86.3873420993332,55.9877494884866,12.586394033035));
#78608=CARTESIAN_POINT('Ctrl Pts',(86.4032587884797,55.9913264686445,12.6316350699695));
#78609=CARTESIAN_POINT('Ctrl Pts',(86.4237153120338,55.9959236922366,12.6897799724135));
#78610=CARTESIAN_POINT('Ctrl Pts',(86.4473721617171,56.0005209158287,12.7469330672877));
#78611=CARTESIAN_POINT('Ctrl Pts',(86.4741130321229,56.0051181394207,12.8027179131592));
#78612=CARTESIAN_POINT('Ctrl Pts',(86.5013117790042,56.0097940799919,12.8594579474081));
#78613=CARTESIAN_POINT('Ctrl Pts',(86.5317010679247,56.014470020563,12.9147819035902));
#78614=CARTESIAN_POINT('Ctrl Pts',(86.5651057779538,56.0191459611341,12.968310774763));
#78615=CARTESIAN_POINT('Ctrl Pts',(86.597857800527,56.0237305395065,13.0207937568169));
#78616=CARTESIAN_POINT('Ctrl Pts',(86.6335081862367,56.0283151178789,13.0715507180151));
#78617=CARTESIAN_POINT('Ctrl Pts',(86.6718448854607,56.0328996962513,13.1202477957308));
#78618=CARTESIAN_POINT('Ctrl Pts',(86.7101581539617,56.0374814726093,13.1689151106407));
#78619=CARTESIAN_POINT('Ctrl Pts',(86.751154166243,56.0420632489673,13.2155246392687));
#78620=CARTESIAN_POINT('Ctrl Pts',(86.7945785585489,56.0466450253252,13.2597728897818));
#78621=CARTESIAN_POINT('Ctrl Pts',(86.8379923602402,56.0512256842507,13.3040103487527));
#78622=CARTESIAN_POINT('Ctrl Pts',(86.88383300986,56.0558063431762,13.3458873096701));
#78623=CARTESIAN_POINT('Ctrl Pts',(86.9318083981857,56.0603870021016,13.3851362030411));
#78624=CARTESIAN_POINT('Ctrl Pts',(86.9815169744614,56.0651331446871,13.4258030257173));
#78625=CARTESIAN_POINT('Ctrl Pts',(87.0335170748689,56.0698792872726,13.4636478412017));
#78626=CARTESIAN_POINT('Ctrl Pts',(87.0874472546661,56.0746254298581,13.4984193388063));
#78627=CARTESIAN_POINT('Ctrl Pts',(87.1395629839962,56.0792118911545,13.5320209689951));
#78628=CARTESIAN_POINT('Ctrl Pts',(87.193480479509,56.0837983524509,13.5627526119449));
#78629=CARTESIAN_POINT('Ctrl Pts',(87.2488471905413,56.0883848137473,13.5904336425815));
#78630=CARTESIAN_POINT('Ctrl Pts',(87.3071053555355,56.0932107969774,13.6195602787853));
#78631=CARTESIAN_POINT('Ctrl Pts',(87.3669676662476,56.0980367802074,13.6453086724651));
#78632=CARTESIAN_POINT('Ctrl Pts',(87.4280009735009,56.1028627634375,13.6675264502034));
#78633=CARTESIAN_POINT('Ctrl Pts',(87.4890342807541,56.1076887466675,13.6897442279417));
#78634=CARTESIAN_POINT('Ctrl Pts',(87.5512379416981,56.1125147298976,13.7084312774101));
#78635=CARTESIAN_POINT('Ctrl Pts',(87.6141651528457,56.1173407131277,13.7234971914558));
#78636=CARTESIAN_POINT('Ctrl Pts',(87.6741095094423,56.1219379367197,13.7378489560986));
#78637=CARTESIAN_POINT('Ctrl Pts',(87.7349564804357,56.1265351603118,13.7489741038072));
#78638=CARTESIAN_POINT('Ctrl Pts',(87.7963267255002,56.1311323839039,13.7567661638487));
#78639=CARTESIAN_POINT('Ctrl Pts',(87.8587477961767,56.135808324475,13.7646916451638));
#78640=CARTESIAN_POINT('Ctrl Pts',(87.9217097357451,56.1404842650461,13.7691686055733));
#78641=CARTESIAN_POINT('Ctrl Pts',(87.9847991470731,56.1451602056173,13.7701385949816));
#78642=CARTESIAN_POINT('Ctrl Pts',(88.046655867941,56.1497447839897,13.7710896319752));
#78643=CARTESIAN_POINT('Ctrl Pts',(88.1086345907267,56.1543293623621,13.7686695011596));
#78644=CARTESIAN_POINT('Ctrl Pts',(88.1703398149164,56.1589139407345,13.762875263236));
#78645=CARTESIAN_POINT('Ctrl Pts',(88.2320073259479,56.1634957170924,13.7570845666498));
#78646=CARTESIAN_POINT('Ctrl Pts',(88.2934011640666,56.1680774934504,13.7479238994837));
#78647=CARTESIAN_POINT('Ctrl Pts',(88.3541283927722,56.1726592698084,13.7354423445191));
#78648=CARTESIAN_POINT('Ctrl Pts',(88.4148408109383,56.1772399287338,13.7229638336349));
#78649=CARTESIAN_POINT('Ctrl Pts',(88.4748864440305,56.1818205876593,13.707166145203));
#78650=CARTESIAN_POINT('Ctrl Pts',(88.5338820615718,56.1864012465847,13.6881495570034));
#78651=CARTESIAN_POINT('Ctrl Pts',(88.5950089905418,56.1911473891702,13.6684459640151));
#78652=CARTESIAN_POINT('Ctrl Pts',(88.6550080113801,56.1958935317557,13.6452865598798));
#78653=CARTESIAN_POINT('Ctrl Pts',(88.7134719454762,56.2006396743412,13.618838691371));
#78654=CARTESIAN_POINT('Ctrl Pts',(88.7699688934998,56.2052261356376,13.5932806464742));
#78655=CARTESIAN_POINT('Ctrl Pts',(88.8250319802325,56.209812596934,13.5646522221337));
#78656=CARTESIAN_POINT('Ctrl Pts',(88.8783182356818,56.2143990582304,13.5331516328089));
#78657=CARTESIAN_POINT('Ctrl Pts',(88.9343872960256,56.2192250414605,13.5000059664672));
#78658=CARTESIAN_POINT('Ctrl Pts',(88.9884883099577,56.2240510246906,13.4636802687804));
#78659=CARTESIAN_POINT('Ctrl Pts',(89.0402583257664,56.2288770079207,13.4244557903887));
#78660=CARTESIAN_POINT('Ctrl Pts',(89.0920283415751,56.2337029911507,13.385231311997));
#78661=CARTESIAN_POINT('Ctrl Pts',(89.1414669162095,56.2385289743808,13.343108532046));
#78662=CARTESIAN_POINT('Ctrl Pts',(89.1882557510482,56.2433549576109,13.2984137828765));
#78663=CARTESIAN_POINT('Ctrl Pts',(89.2328267172351,56.2479521812029,13.2558376392124));
#78664=CARTESIAN_POINT('Ctrl Pts',(89.2751765111576,56.252549404795,13.2107530770504));
#78665=CARTESIAN_POINT('Ctrl Pts',(89.3150099307752,56.2571466283871,13.1634210386354));
#78666=CARTESIAN_POINT('Ctrl Pts',(89.3555254069417,56.2618225689582,13.1152785469105));
#78667=CARTESIAN_POINT('Ctrl Pts',(89.3934370743049,56.2664985095293,13.0648111863052));
#78668=CARTESIAN_POINT('Ctrl Pts',(89.428471601609,56.2711744501005,13.0123345572428));
#78669=CARTESIAN_POINT('Ctrl Pts',(89.4628215968074,56.2757590284729,12.9608832577669));
#78670=CARTESIAN_POINT('Ctrl Pts',(89.4944055762479,56.2803436068453,12.9075009446471));
#78671=CARTESIAN_POINT('Ctrl Pts',(89.5230065515739,56.2849281852177,12.8525182919663));
#78672=CARTESIAN_POINT('Ctrl Pts',(89.5515900464819,56.2895099615757,12.7975692437251));
#78673=CARTESIAN_POINT('Ctrl Pts',(89.5771939179111,56.2940917379336,12.7410222460178));
#78674=CARTESIAN_POINT('Ctrl Pts',(89.5996462730734,56.2986735142916,12.683234035557));
#78675=CARTESIAN_POINT('Ctrl Pts',(89.6220931524138,56.303254173217,12.6254599188493));
#78676=CARTESIAN_POINT('Ctrl Pts',(89.6413898570269,56.3078348321425,12.5664456646026));
#78677=CARTESIAN_POINT('Ctrl Pts',(89.6574127686622,56.3124154910679,12.5065676233974));
#78678=CARTESIAN_POINT('Ctrl Pts',(89.6740145337125,56.3171616336534,12.4445263917917));
#78679=CARTESIAN_POINT('Ctrl Pts',(89.6871012226801,56.321907776239,12.3815583119947));
#78680=CARTESIAN_POINT('Ctrl Pts',(89.6965925739576,56.3266539188245,12.3180962320605));
#78681=CARTESIAN_POINT('Ctrl Pts',(89.7057645940771,56.3312403801209,12.256769297995));
#78682=CARTESIAN_POINT('Ctrl Pts',(89.7115793988327,56.3358268414173,12.194981611144));
#78683=CARTESIAN_POINT('Ctrl Pts',(89.7140174858883,56.3404133027136,12.1331288191363));
#78684=CARTESIAN_POINT('Ctrl Pts',(89.7165828988469,56.3452392859437,12.0680458460833));
#78685=CARTESIAN_POINT('Ctrl Pts',(89.7154092342088,56.3500652691738,12.002891425418));
#78686=CARTESIAN_POINT('Ctrl Pts',(89.7105359120319,56.3548912524039,11.9381230305569));
#78687=CARTESIAN_POINT('Ctrl Pts',(89.705662589855,56.3597172356339,11.8733546356957));
#78688=CARTESIAN_POINT('Ctrl Pts',(89.6970897723693,56.364543218864,11.8089728987431));
#78689=CARTESIAN_POINT('Ctrl Pts',(89.6849189735046,56.3693692020941,11.7454222313675));
#78690=CARTESIAN_POINT('Ctrl Pts',(89.6733250907644,56.3739664256862,11.6848839714062));
#78691=CARTESIAN_POINT('Ctrl Pts',(89.6584190714499,56.3785636492783,11.6248512021979));
#78692=CARTESIAN_POINT('Ctrl Pts',(89.6402600214436,56.3831608728703,11.5657134639774));
#78693=CARTESIAN_POINT('Ctrl Pts',(89.6217900390822,56.3878368134415,11.5055631267377));
#78694=CARTESIAN_POINT('Ctrl Pts',(89.5999545824805,56.3925127540126,11.4463392983937));
#78695=CARTESIAN_POINT('Ctrl Pts',(89.5748705397008,56.3971886945837,11.3884427915993));
#78696=CARTESIAN_POINT('Ctrl Pts',(89.5502766086465,56.4017732729561,11.3316775122184));
#78697=CARTESIAN_POINT('Ctrl Pts',(89.5225601086229,56.4063578513286,11.276188641823));
#78698=CARTESIAN_POINT('Ctrl Pts',(89.4918811517115,56.410942429701,11.2223378341387));
#78699=CARTESIAN_POINT('Ctrl Pts',(89.4612209452442,56.4155242060589,11.1685199391302));
#78700=CARTESIAN_POINT('Ctrl Pts',(89.4276021235109,56.4201059824169,11.1163385630737));
#78701=CARTESIAN_POINT('Ctrl Pts',(89.391231154141,56.4246877587749,11.0661316102913));
#78702=CARTESIAN_POINT('Ctrl Pts',(89.3548690551524,56.4292684177003,11.0159369022971));
#78703=CARTESIAN_POINT('Ctrl Pts',(89.3157564394869,56.4338490766258,10.9677160737162));
#78704=CARTESIAN_POINT('Ctrl Pts',(89.2741424368487,56.4384297355512,10.9217771109474));
#78705=CARTESIAN_POINT('Ctrl Pts',(89.2310250615346,56.4431758781367,10.8741785293722));
#78706=CARTESIAN_POINT('Ctrl Pts',(89.1852224485135,56.4479220207223,10.8290303163191));
#78707=CARTESIAN_POINT('Ctrl Pts',(89.1370547088028,56.4526681633078,10.7866346775127));
#78708=CARTESIAN_POINT('Ctrl Pts',(89.0905075455144,56.4572546246042,10.7456654160507));
#78709=CARTESIAN_POINT('Ctrl Pts',(89.0417523445954,56.4618410859006,10.7072667105503));
#78710=CARTESIAN_POINT('Ctrl Pts',(88.9911109199524,56.466427547197,10.6716695441216));
#78711=CARTESIAN_POINT('Ctrl Pts',(88.9378248132396,56.471253530427,10.6342133623027));
#78712=CARTESIAN_POINT('Ctrl Pts',(88.8824506108117,56.4760795136571,10.599859705636));
#78713=CARTESIAN_POINT('Ctrl Pts',(88.8253940271616,56.4809054968872,10.5688235895114));
#78714=CARTESIAN_POINT('Ctrl Pts',(88.7683374435115,56.4857314801172,10.5377874733868));
#78715=CARTESIAN_POINT('Ctrl Pts',(88.7095990976767,56.4905574633473,10.5100691043642));
#78716=CARTESIAN_POINT('Ctrl Pts',(88.6496074103387,56.4953834465774,10.4858242467813));
#78717=CARTESIAN_POINT('Ctrl Pts',(88.5924594288372,56.4999806701695,10.4627286358035));
#78718=CARTESIAN_POINT('Ctrl Pts',(88.5339396220379,56.5045778937615,10.4426897984422));
#78719=CARTESIAN_POINT('Ctrl Pts',(88.4744073098968,56.5091751173536,10.4258693647352));
#78720=CARTESIAN_POINT('Ctrl Pts',(88.4138556425571,56.5138510579247,10.408760919427));
#78721=CARTESIAN_POINT('Ctrl Pts',(88.3522569258906,56.5185269984959,10.3949824175572));
#78722=CARTESIAN_POINT('Ctrl Pts',(88.290011291034,56.523202939067,10.3846530592779));
#78723=CARTESIAN_POINT('Ctrl Pts',(88.2289818602702,56.5277875174394,10.3745255241119));
#78724=CARTESIAN_POINT('Ctrl Pts',(88.1673310901714,56.5323720958118,10.3677136478994));
#78725=CARTESIAN_POINT('Ctrl Pts',(88.1054496582838,56.5369566741842,10.3642790776246));
#78726=CARTESIAN_POINT('Ctrl Pts',(88.0436060472497,56.5415384505422,10.3608466064994));
#78727=CARTESIAN_POINT('Ctrl Pts',(87.9815325611732,56.5461202269001,10.3607873765511));
#78728=CARTESIAN_POINT('Ctrl Pts',(87.9196250684157,56.5507020032581,10.3641112088394));
#78729=CARTESIAN_POINT('Ctrl Pts',(87.8577326740479,56.5552826621835,10.3674342304906));
#78730=CARTESIAN_POINT('Ctrl Pts',(87.7960067007206,56.559863321109,10.3741386491852));
#78731=CARTESIAN_POINT('Ctrl Pts',(87.7348410219715,56.5644439800344,10.3841822172262));
#78732=CARTESIAN_POINT('Ctrl Pts',(87.6714656348476,56.56919012262,10.3945886252922));
#78733=CARTESIAN_POINT('Ctrl Pts',(87.6086923845848,56.5739362652055,10.4085800352604));
#78734=CARTESIAN_POINT('Ctrl Pts',(87.5469487884302,56.578682407791,10.4260514310989));
#78735=CARTESIAN_POINT('Ctrl Pts',(87.4872825207273,56.5832688690874,10.4429350116834));
#78736=CARTESIAN_POINT('Ctrl Pts',(87.4285781946293,56.5878553303838,10.4630678778013));
#78737=CARTESIAN_POINT('Ctrl Pts',(87.3712044154017,56.5924417916802,10.4863049517301));
#78738=CARTESIAN_POINT('Ctrl Pts',(87.3108343657043,56.5972677749102,10.5107555514079));
#78739=CARTESIAN_POINT('Ctrl Pts',(87.2519382325376,56.6020937581403,10.5386432103078));
#78740=CARTESIAN_POINT('Ctrl Pts',(87.1949167139219,56.6069197413704,10.5697437031765));
#78741=CARTESIAN_POINT('Ctrl Pts',(87.1378951953061,56.6117457246004,10.6008441960452));
#78742=CARTESIAN_POINT('Ctrl Pts',(87.0827488005417,56.6165717078305,10.6351571148539));
#78743=CARTESIAN_POINT('Ctrl Pts',(87.0298407653942,56.6213976910606,10.6724070207023));
#78744=CARTESIAN_POINT('Ctrl Pts',(86.9797608584156,56.6259657078196,10.7076657827155));
#78745=CARTESIAN_POINT('Ctrl Pts',(86.9314747164261,56.6305337245787,10.7457045104822));
#78746=CARTESIAN_POINT('Ctrl Pts',(86.8853106759136,56.6351017413377,10.7863131706398));
#78747=CARTESIAN_POINT('Ctrl Pts',(86.8392274476728,56.6396617615738,10.826850743474));
#78748=CARTESIAN_POINT('Ctrl Pts',(86.7952593321464,56.6442217818098,10.8699489816961));
#78749=CARTESIAN_POINT('Ctrl Pts',(86.7537043789943,56.6487818020459,10.9153555905494));
#78750=CARTESIAN_POINT('Ctrl Pts',(86.7121899853957,56.6533373714916,10.9607178804554));
#78751=CARTESIAN_POINT('Ctrl Pts',(86.6730844345984,56.6578929409373,11.0083836984446));
#78752=CARTESIAN_POINT('Ctrl Pts',(86.6366501883998,56.6624485103831,11.0580627842199));
#78753=CARTESIAN_POINT('Ctrl Pts',(86.6002376828568,56.6670013614779,11.1077122260199));
#78754=CARTESIAN_POINT('Ctrl Pts',(86.566493627052,56.6715542125726,11.1593721388688));
#78755=CARTESIAN_POINT('Ctrl Pts',(86.5356399060811,56.6761070636674,11.212719607121));
#78756=CARTESIAN_POINT('Ctrl Pts',(86.5047928926333,56.6806589249836,11.2660554777648));
#78757=CARTESIAN_POINT('Ctrl Pts',(86.4768352248621,56.6852107862998,11.3210777286816));
#78758=CARTESIAN_POINT('Ctrl Pts',(86.4519440347309,56.6897626476159,11.3774367619756));
#78759=CARTESIAN_POINT('Ctrl Pts',(86.4270313025592,56.6943184483331,11.433844571104));
#78760=CARTESIAN_POINT('Ctrl Pts',(86.405190560342,56.6988742490503,11.4915910011074));
#78761=CARTESIAN_POINT('Ctrl Pts',(86.3865511661085,56.7034300497675,11.5503054957936));
#78762=CARTESIAN_POINT('Ctrl Pts',(86.3679040418857,56.7079877398321,11.6090443401136));
#78763=CARTESIAN_POINT('Ctrl Pts',(86.3524610408587,56.7125454298968,11.6687515484091));
#78764=CARTESIAN_POINT('Ctrl Pts',(86.3403010154367,56.7171031199614,11.7290434173679));
#78765=CARTESIAN_POINT('Ctrl Pts',(86.3281186032256,56.7216692008018,11.7894462845612));
#78766=CARTESIAN_POINT('Ctrl Pts',(86.3192313151102,56.7262352816421,11.8504354504348));
#78767=CARTESIAN_POINT('Ctrl Pts',(86.3136663080636,56.7308013624825,11.9116200342736));
#78768=CARTESIAN_POINT('Ctrl Pts',(86.3089786900743,56.7346475467746,11.9631581461708));
#78769=CARTESIAN_POINT('Ctrl Pts',(86.3066474220475,56.7384937310667,12.0148346679399));
#78770=CARTESIAN_POINT('Ctrl Pts',(86.3066600510811,56.7423399153589,12.0664172756536));
#78771=CARTESIAN_POINT('',(86.3066607042565,57.5360899153607,12.064450618022));
#78772=CARTESIAN_POINT('Ctrl Pts',(86.3066600510813,56.7423399154299,12.0664172766061));
#78773=CARTESIAN_POINT('Ctrl Pts',(86.3066656024584,56.7440305888012,12.0890915258513));
#78774=CARTESIAN_POINT('Ctrl Pts',(86.3071236157404,56.7457212621725,12.1117596676896));
#78775=CARTESIAN_POINT('Ctrl Pts',(86.3080334792289,56.7474119355438,12.1344095368553));
#78776=CARTESIAN_POINT('Ctrl Pts',(86.3105075501914,56.7520091591358,12.1959983183745));
#78777=CARTESIAN_POINT('Ctrl Pts',(86.316332099658,56.7566063827279,12.2575791385552));
#78778=CARTESIAN_POINT('Ctrl Pts',(86.3255065323334,56.7612036063199,12.3187579989896));
#78779=CARTESIAN_POINT('Ctrl Pts',(86.334838056264,56.765879546891,12.3809844080103));
#78780=CARTESIAN_POINT('Ctrl Pts',(86.3476353350051,56.7705554874621,12.4427944287638));
#78781=CARTESIAN_POINT('Ctrl Pts',(86.363842306128,56.7752314280333,12.5037743335537));
#78782=CARTESIAN_POINT('Ctrl Pts',(86.3797326127225,56.7798160064057,12.5635627650787));
#78783=CARTESIAN_POINT('Ctrl Pts',(86.3989004305176,56.7844005847781,12.6225527122926));
#78784=CARTESIAN_POINT('Ctrl Pts',(86.4212411365165,56.7889851631505,12.6803627524318));
#78785=CARTESIAN_POINT('Ctrl Pts',(86.4435681882649,56.7935669395084,12.7381374600814));
#78786=CARTESIAN_POINT('Ctrl Pts',(86.4690640999206,56.7981487158664,12.7947332167309));
#78787=CARTESIAN_POINT('Ctrl Pts',(86.4975748797646,56.8027304922244,12.8497852008303));
#78788=CARTESIAN_POINT('Ctrl Pts',(86.5260787062199,56.8073111511498,12.9048237585048));
#78789=CARTESIAN_POINT('Ctrl Pts',(86.5575957072175,56.8118918100753,12.9583188392258));
#78790=CARTESIAN_POINT('Ctrl Pts',(86.5919252586688,56.8164724690008,13.0099288713223));
#78791=CARTESIAN_POINT('Ctrl Pts',(86.6274950202983,56.8212186115863,13.0634033987121));
#78792=CARTESIAN_POINT('Ctrl Pts',(86.6660841703194,56.8259647541718,13.1148535493639));
#78793=CARTESIAN_POINT('Ctrl Pts',(86.7074210320166,56.8307108967573,13.1639329259255));
#78794=CARTESIAN_POINT('Ctrl Pts',(86.7473671383277,56.8352973580538,13.2113610545574));
#78795=CARTESIAN_POINT('Ctrl Pts',(86.7898785758916,56.8398838193502,13.2565750775701));
#78796=CARTESIAN_POINT('Ctrl Pts',(86.8346714059086,56.8444702806466,13.2992987773946));
#78797=CARTESIAN_POINT('Ctrl Pts',(86.8818034828019,56.8492962638767,13.3442536664812));
#78798=CARTESIAN_POINT('Ctrl Pts',(86.9314612880865,56.8541222471067,13.3864505667847));
#78799=CARTESIAN_POINT('Ctrl Pts',(86.9832755413533,56.8589482303368,13.4256165903296));
#78800=CARTESIAN_POINT('Ctrl Pts',(87.0350897946201,56.8637742135669,13.4647826138744));
#78801=CARTESIAN_POINT('Ctrl Pts',(87.0890599143759,56.868600196797,13.5009174644516));
#78802=CARTESIAN_POINT('Ctrl Pts',(87.1447853658042,56.8734261800271,13.5338034756414));
#78803=CARTESIAN_POINT('Ctrl Pts',(87.1978693380795,56.8780234036192,13.5651306351619));
#78804=CARTESIAN_POINT('Ctrl Pts',(87.2527639172621,56.8826206272113,13.5936386685382));
#78805=CARTESIAN_POINT('Ctrl Pts',(87.3091377740607,56.8872178508033,13.6191143716416));
#78806=CARTESIAN_POINT('Ctrl Pts',(87.3664769047068,56.8918937913745,13.6450262881131));
#78807=CARTESIAN_POINT('Ctrl Pts',(87.4253460398766,56.8965697319456,13.667800702114));
#78808=CARTESIAN_POINT('Ctrl Pts',(87.4853671899815,56.9012456725167,13.6872603074868));
#78809=CARTESIAN_POINT('Ctrl Pts',(87.5442155997233,56.9058302508891,13.7063396958088));
#78810=CARTESIAN_POINT('Ctrl Pts',(87.6041709039119,56.9104148292616,13.7222324806806));
#78811=CARTESIAN_POINT('Ctrl Pts',(87.6648559138243,56.914999407634,13.7348196748617));
#78812=CARTESIAN_POINT('Ctrl Pts',(87.7255038341156,56.9195811839919,13.7473991759689));
#78813=CARTESIAN_POINT('Ctrl Pts',(87.7868800784062,56.9241629603499,13.7566769892163));
#78814=CARTESIAN_POINT('Ctrl Pts',(87.8485946274706,56.9287447367078,13.7625846075494));
#78815=CARTESIAN_POINT('Ctrl Pts',(87.9102941252017,56.9333253956333,13.7684907850954));
#78816=CARTESIAN_POINT('Ctrl Pts',(87.9723312574121,56.9379060545587,13.7710283509263));
#78817=CARTESIAN_POINT('Ctrl Pts',(88.0343102442518,56.9424867134842,13.7701805855346));
#78818=CARTESIAN_POINT('Ctrl Pts',(88.0985283215272,56.9472328560697,13.7693021932565));
#78819=CARTESIAN_POINT('Ctrl Pts',(88.162683389576,56.9519789986552,13.7647891294288));
#78820=CARTESIAN_POINT('Ctrl Pts',(88.2263370755343,56.9567251412407,13.7566817499164));
#78821=CARTESIAN_POINT('Ctrl Pts',(88.2878491691474,56.9613116025371,13.7488471386128));
#78822=CARTESIAN_POINT('Ctrl Pts',(88.3488925782536,56.9658980638335,13.7376564100642));
#78823=CARTESIAN_POINT('Ctrl Pts',(88.4090812385715,56.9704845251299,13.7231982871996));
#78824=CARTESIAN_POINT('Ctrl Pts',(88.472413172837,56.9753105083599,13.7079851078063));
#78825=CARTESIAN_POINT('Ctrl Pts',(88.5347980142919,56.98013649159,13.6891540808148));
#78826=CARTESIAN_POINT('Ctrl Pts',(88.5958062067336,56.98496247482,13.6668674324146));
#78827=CARTESIAN_POINT('Ctrl Pts',(88.6568143991754,56.9897884580501,13.6445807840144));
#78828=CARTESIAN_POINT('Ctrl Pts',(88.7164453783511,56.9946144412802,13.618838842067));
#78829=CARTESIAN_POINT('Ctrl Pts',(88.7742990285047,56.9994404245102,13.5898600423542));
#78830=CARTESIAN_POINT('Ctrl Pts',(88.8294103193431,57.0040376481023,13.5622548859833));
#78831=CARTESIAN_POINT('Ctrl Pts',(88.8831352735712,57.0086348716944,13.5315995098839));
#78832=CARTESIAN_POINT('Ctrl Pts',(88.935115061289,57.0132320952865,13.4980566291522));
#78833=CARTESIAN_POINT('Ctrl Pts',(88.9879848844333,57.0179080358576,13.4639394030169));
#78834=CARTESIAN_POINT('Ctrl Pts',(89.0390486978894,57.0225839764287,13.4268350102305));
#78835=CARTESIAN_POINT('Ctrl Pts',(89.0879525219152,57.0272599169998,13.3869648372082));
#78836=CARTESIAN_POINT('Ctrl Pts',(89.1359008246249,57.0318444953722,13.3478736789349));
#78837=CARTESIAN_POINT('Ctrl Pts',(89.1817723724914,57.0364290737447,13.3061241854332));
#78838=CARTESIAN_POINT('Ctrl Pts',(89.2252626151182,57.0410136521171,13.2619687024024));
#78839=CARTESIAN_POINT('Ctrl Pts',(89.2687262772663,57.045595428475,13.2178402064339));
#78840=CARTESIAN_POINT('Ctrl Pts',(89.3098111635798,57.050177204833,13.1713089986429));
#78841=CARTESIAN_POINT('Ctrl Pts',(89.3482481738866,57.054758981191,13.1226655842966));
#78842=CARTESIAN_POINT('Ctrl Pts',(89.386675809933,57.0593396401164,13.0740340334129));
#78843=CARTESIAN_POINT('Ctrl Pts',(89.422456536485,57.0639202990419,13.0232916978276));
#78844=CARTESIAN_POINT('Ctrl Pts',(89.455361636629,57.0685009579673,12.9707620119314));
#78845=CARTESIAN_POINT('Ctrl Pts',(89.4894554863603,57.0732471005528,12.9163346067715));
#78846=CARTESIAN_POINT('Ctrl Pts',(89.5204615954466,57.0779932431384,12.859988695644));
#78847=CARTESIAN_POINT('Ctrl Pts',(89.5481760948056,57.0827393857239,12.8021144538441));
#78848=CARTESIAN_POINT('Ctrl Pts',(89.5749581554726,57.0873258470203,12.7461873582519));
#78849=CARTESIAN_POINT('Ctrl Pts',(89.5986664570931,57.0919123083167,12.6888336605941));
#78850=CARTESIAN_POINT('Ctrl Pts',(89.6191661368895,57.0964987696131,12.6304258248537));
#78851=CARTESIAN_POINT('Ctrl Pts',(89.640736385612,57.1013247528431,12.5689677163967));
#78852=CARTESIAN_POINT('Ctrl Pts',(89.6587535020052,57.1061507360732,12.5063429645986));
#78853=CARTESIAN_POINT('Ctrl Pts',(89.6731207849723,57.1109767193033,12.4430004400036));
#78854=CARTESIAN_POINT('Ctrl Pts',(89.6874880679395,57.1158027025334,12.3796579154086));
#78855=CARTESIAN_POINT('Ctrl Pts',(89.6982054868738,57.1206286857634,12.3155982698893));
#78856=CARTESIAN_POINT('Ctrl Pts',(89.7052395320091,57.1254546689935,12.251276128461));
#78857=CARTESIAN_POINT('Ctrl Pts',(89.7119401516968,57.1300518925856,12.1900029636012));
#78858=CARTESIAN_POINT('Ctrl Pts',(89.7153262699519,57.1346491161777,12.1282400540699));
#78859=CARTESIAN_POINT('Ctrl Pts',(89.7153399582779,57.1392463397698,12.0663771169298));
#78860=CARTESIAN_POINT('Ctrl Pts',(89.7153538809853,57.1439222803409,12.0034549179486));
#78861=CARTESIAN_POINT('Ctrl Pts',(89.711878644327,57.148598220912,11.9404297504446));
#78862=CARTESIAN_POINT('Ctrl Pts',(89.7049082415433,57.1532741614831,11.8777190800113));
#78863=CARTESIAN_POINT('Ctrl Pts',(89.6980740319627,57.1578587398555,11.8162336999011));
#78864=CARTESIAN_POINT('Ctrl Pts',(89.6878800694191,57.162443318228,11.7550511677618));
#78865=CARTESIAN_POINT('Ctrl Pts',(89.6743731671188,57.1670278966004,11.6945642148242));
#78866=CARTESIAN_POINT('Ctrl Pts',(89.6608745200019,57.1716096729583,11.6341142304588));
#78867=CARTESIAN_POINT('Ctrl Pts',(89.6440670587452,57.1761914493163,11.5743594781124));
#78868=CARTESIAN_POINT('Ctrl Pts',(89.6240488833731,57.1807732256743,11.5156836042342));
#78869=CARTESIAN_POINT('Ctrl Pts',(89.6040355901599,57.1853538845997,11.4570220405981));
#78870=CARTESIAN_POINT('Ctrl Pts',(89.580813301596,57.1899345435252,11.3994393146546));
#78871=CARTESIAN_POINT('Ctrl Pts',(89.5545296859893,57.1945152024506,11.3433030067382));
#78872=CARTESIAN_POINT('Ctrl Pts',(89.5272965325583,57.1992613450361,11.2851386845454));
#78873=CARTESIAN_POINT('Ctrl Pts',(89.4967768149411,57.2040074876216,11.228527843375));
#78874=CARTESIAN_POINT('Ctrl Pts',(89.4631877493251,57.2087536302072,11.1738533885566));
#78875=CARTESIAN_POINT('Ctrl Pts',(89.4307287688681,57.2133400915035,11.1210184249186));
#78876=CARTESIAN_POINT('Ctrl Pts',(89.3954040667084,57.2179265527999,11.0699920041341));
#78877=CARTESIAN_POINT('Ctrl Pts',(89.35745340832,57.2225130140963,11.0210894512813));
#78878=CARTESIAN_POINT('Ctrl Pts',(89.3175208265065,57.2273389973264,10.9696330266604));
#78879=CARTESIAN_POINT('Ctrl Pts',(89.2746809083428,57.2321649805565,10.9205288778271));
#78880=CARTESIAN_POINT('Ctrl Pts',(89.2292583089208,57.2369909637865,10.8741017122483));
#78881=CARTESIAN_POINT('Ctrl Pts',(89.1838357094989,57.2418169470166,10.8276745466695));
#78882=CARTESIAN_POINT('Ctrl Pts',(89.1358309598696,57.2466429302467,10.7839247436333));
#78883=CARTESIAN_POINT('Ctrl Pts',(89.0856078244774,57.2514689134767,10.7431270434498));
#78884=CARTESIAN_POINT('Ctrl Pts',(89.0377653492997,57.2560661370688,10.7042632221631));
#78885=CARTESIAN_POINT('Ctrl Pts',(88.9877136477779,57.2606633606609,10.6679183467968));
#78886=CARTESIAN_POINT('Ctrl Pts',(88.9357487091222,57.265260584253,10.6343524663603));
#78887=CARTESIAN_POINT('Ctrl Pts',(88.8828939892964,57.2699365248241,10.6002118467025));
#78888=CARTESIAN_POINT('Ctrl Pts',(88.8280602477108,57.2746124653952,10.5689466936973));
#78889=CARTESIAN_POINT('Ctrl Pts',(88.7715949479891,57.2792884059663,10.5407884865719));
#78890=CARTESIAN_POINT('Ctrl Pts',(88.7162329116333,57.2838729843387,10.513180456609));
#78891=CARTESIAN_POINT('Ctrl Pts',(88.6593029784183,57.2884575627112,10.4885592906041));
#78892=CARTESIAN_POINT('Ctrl Pts',(88.6011604815904,57.2930421410836,10.4670986767255));
#78893=CARTESIAN_POINT('Ctrl Pts',(88.5430535204439,57.2976239174415,10.4456511792003));
#78894=CARTESIAN_POINT('Ctrl Pts',(88.4837359417387,57.3022056937995,10.4273605794718));
#78895=CARTESIAN_POINT('Ctrl Pts',(88.4235832643108,57.3067874701574,10.412352550992));
#78896=CARTESIAN_POINT('Ctrl Pts',(88.3634452572971,57.3113681290829,10.3973481827648));
#78897=CARTESIAN_POINT('Ctrl Pts',(88.3024730495601,57.3159487880083,10.3856249196992));
#78898=CARTESIAN_POINT('Ctrl Pts',(88.2410555482283,57.3205294469338,10.377258077642));
#78899=CARTESIAN_POINT('Ctrl Pts',(88.1774192410267,57.3252755895193,10.3685889699787));
#78900=CARTESIAN_POINT('Ctrl Pts',(88.1133054177713,57.3300217321048,10.3635235806528));
#78901=CARTESIAN_POINT('Ctrl Pts',(88.0491535831273,57.3347678746903,10.3620871091237));
#78902=CARTESIAN_POINT('Ctrl Pts',(87.98716010076,57.3393543359867,10.3606989668686));
#78903=CARTESIAN_POINT('Ctrl Pts',(87.9251316496256,57.3439407972831,10.3626993294924));
#78904=CARTESIAN_POINT('Ctrl Pts',(87.8634631894947,57.3485272585795,10.3680577968771));
#78905=CARTESIAN_POINT('Ctrl Pts',(87.7985741748093,57.3533532418095,10.3736961032022));
#78906=CARTESIAN_POINT('Ctrl Pts',(87.7340844211728,57.3581792250396,10.3830527958237));
#78907=CARTESIAN_POINT('Ctrl Pts',(87.6704428147227,57.3630052082697,10.396031246054));
#78908=CARTESIAN_POINT('Ctrl Pts',(87.6068012082727,57.3678311914997,10.4090096962842));
#78909=CARTESIAN_POINT('Ctrl Pts',(87.5440083556983,57.3726571747298,10.4256096637016));
#78910=CARTESIAN_POINT('Ctrl Pts',(87.4824923775355,57.3774831579599,10.4456745608993));
#78911=CARTESIAN_POINT('Ctrl Pts',(87.4238923591315,57.382080381552,10.4647883485716));
#78912=CARTESIAN_POINT('Ctrl Pts',(87.3662102788873,57.386677605144,10.4871244272184));
#78913=CARTESIAN_POINT('Ctrl Pts',(87.3098251536625,57.3912748287361,10.5125751802988));
#78914=CARTESIAN_POINT('Ctrl Pts',(87.2524745616443,57.3959507693072,10.5384617195351));
#78915=CARTESIAN_POINT('Ctrl Pts',(87.1964662910824,57.4006267098784,10.567570526405));
#78916=CARTESIAN_POINT('Ctrl Pts',(87.1421832764163,57.4053026504495,10.5997352434089));
#78917=CARTESIAN_POINT('Ctrl Pts',(87.0889608859171,57.4098872288219,10.6312715009142));
#78918=CARTESIAN_POINT('Ctrl Pts',(87.0373973977466,57.4144718071943,10.6657450530811));
#78919=CARTESIAN_POINT('Ctrl Pts',(86.9878314633255,57.4190563855668,10.7029515851741));
#78920=CARTESIAN_POINT('Ctrl Pts',(86.9382958227402,57.4236381619247,10.7401353772827));
#78921=CARTESIAN_POINT('Ctrl Pts',(86.890755721362,57.4282199382827,10.7800485322924));
#78922=CARTESIAN_POINT('Ctrl Pts',(86.8455204210706,57.4328017146406,10.8224437340038));
#78923=CARTESIAN_POINT('Ctrl Pts',(86.8002961530495,57.4373823735661,10.864828596106));
#78924=CARTESIAN_POINT('Ctrl Pts',(86.7573759414981,57.4419630324916,10.9096939552778));
#78925=CARTESIAN_POINT('Ctrl Pts',(86.7170340035995,57.446543691417,10.9567539336291));
#78926=CARTESIAN_POINT('Ctrl Pts',(86.6752346484066,57.4512898340025,11.005514029275));
#78927=CARTESIAN_POINT('Ctrl Pts',(86.6362038491661,57.456035976588,11.0566299486358));
#78928=CARTESIAN_POINT('Ctrl Pts',(86.600201163264,57.4607821191736,11.1097461226931));
#78929=CARTESIAN_POINT('Ctrl Pts',(86.5654097674134,57.46536858047,11.1610752330469));
#78930=CARTESIAN_POINT('Ctrl Pts',(86.5334461592334,57.4699550417664,11.2142716422571));
#78931=CARTESIAN_POINT('Ctrl Pts',(86.504499024632,57.4745415030628,11.2689870472726));
#78932=CARTESIAN_POINT('Ctrl Pts',(86.4740401638422,57.4793674862928,11.3265598926465));
#78933=CARTESIAN_POINT('Ctrl Pts',(86.4469217568009,57.4841934695229,11.3858141584882));
#78934=CARTESIAN_POINT('Ctrl Pts',(86.4233060989873,57.489019452753,11.4463203147696));
#78935=CARTESIAN_POINT('Ctrl Pts',(86.3996904411738,57.493845435983,11.5068264710511));
#78936=CARTESIAN_POINT('Ctrl Pts',(86.3795776596723,57.4986714192131,11.5685838776753));
#78937=CARTESIAN_POINT('Ctrl Pts',(86.3630684141364,57.5034974024432,11.6311479287007));
#78938=CARTESIAN_POINT('Ctrl Pts',(86.3429813041155,57.5093692671442,11.7072707880753));
#78939=CARTESIAN_POINT('Ctrl Pts',(86.3281593659612,57.5152411318451,11.7848369403936));
#78940=CARTESIAN_POINT('Ctrl Pts',(86.3187675222516,57.5211129965461,11.8632092781867));
#78941=CARTESIAN_POINT('Ctrl Pts',(86.3107825017104,57.5261053028176,11.929842065794));
#78942=CARTESIAN_POINT('Ctrl Pts',(86.3067219701062,57.5310976090892,11.9970574272591));
#78943=CARTESIAN_POINT('Ctrl Pts',(86.3066607042565,57.5360899153607,12.064450618022));
#78944=CARTESIAN_POINT('',(86.3066600816788,58.3298399155007,12.0665276521619));
#78945=CARTESIAN_POINT('Ctrl Pts',(86.3066607042556,57.5360899154299,12.064450618956));
#78946=CARTESIAN_POINT('Ctrl Pts',(86.3066050417779,57.5406256283189,12.1256800683038));
#78947=CARTESIAN_POINT('Ctrl Pts',(86.3098532065461,57.5451613412079,12.1869899608666));
#78948=CARTESIAN_POINT('Ctrl Pts',(86.3164045293079,57.5496970540969,12.2479918303384));
#78949=CARTESIAN_POINT('Ctrl Pts',(86.3229518351935,57.5542299859601,12.3089562971408));
#78950=CARTESIAN_POINT('Ctrl Pts',(86.3327982305187,57.5587629178234,12.369612598124));
#78951=CARTESIAN_POINT('Ctrl Pts',(86.3458910537401,57.5632958496866,12.4295753466414));
#78952=CARTESIAN_POINT('Ctrl Pts',(86.3589809092653,57.5678277540889,12.4895245036498));
#78953=CARTESIAN_POINT('Ctrl Pts',(86.3753156211357,57.5723596584911,12.5487799113382));
#78954=CARTESIAN_POINT('Ctrl Pts',(86.3947914680293,57.5768915628934,12.6069665579176));
#78955=CARTESIAN_POINT('Ctrl Pts',(86.4142844559702,57.5814274559072,12.6652044156236));
#78956=CARTESIAN_POINT('Ctrl Pts',(86.4369239375402,57.5859633489211,12.7223711372686));
#78957=CARTESIAN_POINT('Ctrl Pts',(86.4625567634577,57.5904992419349,12.7781084038307));
#78958=CARTESIAN_POINT('Ctrl Pts',(86.4882003017455,57.5950370305714,12.8338689638932));
#78959=CARTESIAN_POINT('Ctrl Pts',(86.5168394326287,57.5995748192078,12.8881984172555));
#78960=CARTESIAN_POINT('Ctrl Pts',(86.5482748589299,57.6041126078443,12.9407628234451));
#78961=CARTESIAN_POINT('Ctrl Pts',(86.5797695730835,57.6086589548423,12.9934263671721));
#78962=CARTESIAN_POINT('Ctrl Pts',(86.6140708247473,57.6132053018403,13.0443177814376));
#78963=CARTESIAN_POINT('Ctrl Pts',(86.6509363382424,57.6177516488383,13.0931327429143));
#78964=CARTESIAN_POINT('Ctrl Pts',(86.6827229109502,57.621671648201,13.1352224949642));
#78965=CARTESIAN_POINT('Ctrl Pts',(86.7164150464297,57.6255916475637,13.1757689032637));
#78966=CARTESIAN_POINT('Ctrl Pts',(86.7518355149009,57.6295116469264,13.2145989879262));
#78967=CARTESIAN_POINT('Ctrl Pts',(86.7933752699446,57.6341088705185,13.2601374089248));
#78968=CARTESIAN_POINT('Ctrl Pts',(86.8374738665761,57.6387060941105,13.3035129384981));
#78969=CARTESIAN_POINT('Ctrl Pts',(86.8838772211828,57.6433033177026,13.3444244510613));
#78970=CARTESIAN_POINT('Ctrl Pts',(86.9310751275051,57.6479792582738,13.3860364800585));
#78971=CARTESIAN_POINT('Ctrl Pts',(86.9806571749383,57.6526551988449,13.425098860696));
#78972=CARTESIAN_POINT('Ctrl Pts',(87.0323141331252,57.657331139416,13.4613310752576));
#78973=CARTESIAN_POINT('Ctrl Pts',(87.0829617770989,57.6619157177884,13.4968553563595));
#78974=CARTESIAN_POINT('Ctrl Pts',(87.135603541871,57.6665002961608,13.5296587664414));
#78975=CARTESIAN_POINT('Ctrl Pts',(87.1899138315338,57.6710848745332,13.5595167690901));
#78976=CARTESIAN_POINT('Ctrl Pts',(87.2441909276934,57.6756666508912,13.5893565230477));
#78977=CARTESIAN_POINT('Ctrl Pts',(87.3001340815269,57.6802484272491,13.6162541943417));
#78978=CARTESIAN_POINT('Ctrl Pts',(87.3573906041994,57.6848302036071,13.6400297307615));
#78979=CARTESIAN_POINT('Ctrl Pts',(87.4146331627901,57.6894108625325,13.6637994686536));
#78980=CARTESIAN_POINT('Ctrl Pts',(87.4731879844347,57.693991521458,13.6844483881265));
#78981=CARTESIAN_POINT('Ctrl Pts',(87.5326816613113,57.6985721803834,13.7018442476208));
#78982=CARTESIAN_POINT('Ctrl Pts',(87.5943246428098,57.703318322969,13.7198685604764));
#78983=CARTESIAN_POINT('Ctrl Pts',(87.6569750735685,57.7080644655545,13.7344000444749));
#78984=CARTESIAN_POINT('Ctrl Pts',(87.720202066041,57.71281060814,13.745348503797));
#78985=CARTESIAN_POINT('Ctrl Pts',(87.7813018220297,57.7173970694364,13.7559286083832));
#78986=CARTESIAN_POINT('Ctrl Pts',(87.842939424396,57.7219835307328,13.763162982944));
#78987=CARTESIAN_POINT('Ctrl Pts',(87.9047197787231,57.7265699920292,13.7670230304629));
#78988=CARTESIAN_POINT('Ctrl Pts',(87.9697265311326,57.7313959752592,13.7710846639075));
#78989=CARTESIAN_POINT('Ctrl Pts',(88.0348907105068,57.7362219584893,13.7714098521451));
#78990=CARTESIAN_POINT('Ctrl Pts',(88.0997540577899,57.7410479417194,13.7680274829819));
#78991=CARTESIAN_POINT('Ctrl Pts',(88.164617405073,57.7458739249494,13.7646451138188));
#78992=CARTESIAN_POINT('Ctrl Pts',(88.2291792845965,57.7506999081795,13.7575553349039));
#78993=CARTESIAN_POINT('Ctrl Pts',(88.292993067447,57.7555258914096,13.7468494119081));
#78994=CARTESIAN_POINT('Ctrl Pts',(88.3537819707718,57.7601231150016,13.7366509674824));
#78995=CARTESIAN_POINT('Ctrl Pts',(88.4141416957318,57.7647203385937,13.7231296364321));
#78996=CARTESIAN_POINT('Ctrl Pts',(88.4736814457111,57.7693175621858,13.7063355496345));
#78997=CARTESIAN_POINT('Ctrl Pts',(88.534240678245,57.7739935027569,13.6892539023665));
#78998=CARTESIAN_POINT('Ctrl Pts',(88.5939510524028,57.778669443328,13.6687863615603));
#78999=CARTESIAN_POINT('Ctrl Pts',(88.6524091731495,57.7833453838992,13.6450405657233));
#79000=CARTESIAN_POINT('Ctrl Pts',(88.7097250932282,57.7879299622716,13.6217587338919));
#79001=CARTESIAN_POINT('Ctrl Pts',(88.7658367606141,57.792514540644,13.5953258018849));
#79002=CARTESIAN_POINT('Ctrl Pts',(88.8203789346954,57.7970991190164,13.5658935214446));
#79003=CARTESIAN_POINT('Ctrl Pts',(88.8748877735497,57.8016808953744,13.5364792295014));
#79004=CARTESIAN_POINT('Ctrl Pts',(88.9278285740933,57.8062626717323,13.5040694652369));
#79005=CARTESIAN_POINT('Ctrl Pts',(88.9788587726644,57.8108444480903,13.4688628699116));
#79006=CARTESIAN_POINT('Ctrl Pts',(89.0298765256688,57.8154251070157,13.4336648609928));
#79007=CARTESIAN_POINT('Ctrl Pts',(89.078984182906,57.8200057659412,13.3956716640504));
#79008=CARTESIAN_POINT('Ctrl Pts',(89.1258681095012,57.8245864248666,13.3551252592425));
#79009=CARTESIAN_POINT('Ctrl Pts',(89.1744457932388,57.8293325674521,13.3131140504448));
#79010=CARTESIAN_POINT('Ctrl Pts',(89.2206355167396,57.8340787100377,13.2683619561433));
#79011=CARTESIAN_POINT('Ctrl Pts',(89.2641277917142,57.8388248526232,13.2211820519873));
#79012=CARTESIAN_POINT('Ctrl Pts',(89.3061567936393,57.8434113139196,13.1755894890836));
#79013=CARTESIAN_POINT('Ctrl Pts',(89.3456667041477,57.847997775216,13.1277303502242));
#79014=CARTESIAN_POINT('Ctrl Pts',(89.3824191995577,57.8525842365124,13.0779210516066));
#79015=CARTESIAN_POINT('Ctrl Pts',(89.4210910459005,57.8574102197424,13.0255105276109));
#79016=CARTESIAN_POINT('Ctrl Pts',(89.4567092137119,57.8622362029725,12.9709411026307));
#79017=CARTESIAN_POINT('Ctrl Pts',(89.4890494131044,57.8670621862026,12.9146134385111));
#79018=CARTESIAN_POINT('Ctrl Pts',(89.521389612497,57.8718881694327,12.8582857743915));
#79019=CARTESIAN_POINT('Ctrl Pts',(89.5504516227279,57.8767141526627,12.8002004852554));
#79020=CARTESIAN_POINT('Ctrl Pts',(89.5760698670492,57.8815401358928,12.7407822958958));
#79021=CARTESIAN_POINT('Ctrl Pts',(89.600473763948,57.8861373594849,12.6841806276139));
#79022=CARTESIAN_POINT('Ctrl Pts',(89.6218532476306,57.890734583077,12.6261371915674));
#79023=CARTESIAN_POINT('Ctrl Pts',(89.6400384665074,57.895331806669,12.5670074951927));
#79024=CARTESIAN_POINT('Ctrl Pts',(89.6585350658217,57.9000077472402,12.5068653374971));
#79025=CARTESIAN_POINT('Ctrl Pts',(89.6737266845588,57.9046836878113,12.4455998192272));
#79026=CARTESIAN_POINT('Ctrl Pts',(89.6854849511396,57.9093596283824,12.3836082240857));
#79027=CARTESIAN_POINT('Ctrl Pts',(89.6970134754747,57.9139442067548,12.3228278694097));
#79028=CARTESIAN_POINT('Ctrl Pts',(89.7052415086695,57.9185287851273,12.2613500800785));
#79029=CARTESIAN_POINT('Ctrl Pts',(89.7100984345194,57.9231133634997,12.1995640124199));
#79030=CARTESIAN_POINT('Ctrl Pts',(89.7149523919008,57.9276951398576,12.1378157073297));
#79031=CARTESIAN_POINT('Ctrl Pts',(89.7164392875279,57.9322769162156,12.0757600039394));
#79032=CARTESIAN_POINT('Ctrl Pts',(89.7145401980228,57.9368586925736,12.0137924400075));
#79033=CARTESIAN_POINT('Ctrl Pts',(89.7126415716797,57.941439351499,11.9518399891159));
#79034=CARTESIAN_POINT('Ctrl Pts',(89.7073586151196,57.9460200104245,11.8899761435903));
#79035=CARTESIAN_POINT('Ctrl Pts',(89.6987245058285,57.9506006693499,11.8285956444673));
#79036=CARTESIAN_POINT('Ctrl Pts',(89.6897784754732,57.9553468119354,11.7649976762386));
#79037=CARTESIAN_POINT('Ctrl Pts',(89.6772345425004,57.9600929545209,11.701919231053));
#79038=CARTESIAN_POINT('Ctrl Pts',(89.6611878623258,57.9648390971065,11.6397901284197));
#79039=CARTESIAN_POINT('Ctrl Pts',(89.6456810636508,57.9694255584029,11.579751324386));
#79040=CARTESIAN_POINT('Ctrl Pts',(89.6269037144614,57.9740120196993,11.5205994743882));
#79041=CARTESIAN_POINT('Ctrl Pts',(89.6049923762338,57.9785984809957,11.462706422951));
#79042=CARTESIAN_POINT('Ctrl Pts',(89.5819367470676,57.9834244642257,11.4017899827332));
#79043=CARTESIAN_POINT('Ctrl Pts',(89.5554110680201,57.9882504474558,11.3422680172752));
#79044=CARTESIAN_POINT('Ctrl Pts',(89.5256302890324,57.9930764306859,11.2845462757491));
#79045=CARTESIAN_POINT('Ctrl Pts',(89.4958495100446,57.9979024139159,11.226824534223));
#79046=CARTESIAN_POINT('Ctrl Pts',(89.4628140273237,58.002728397146,11.170903535179));
#79047=CARTESIAN_POINT('Ctrl Pts',(89.4267908525366,58.0075543803761,11.1171527533508));
#79048=CARTESIAN_POINT('Ctrl Pts',(89.3924752361952,58.0121516039682,11.0659498480499));
#79049=CARTESIAN_POINT('Ctrl Pts',(89.3553079222439,58.0167488275602,11.0165058032694));
#79050=CARTESIAN_POINT('Ctrl Pts',(89.3154954527141,58.0213460511523,10.9691561417193));
#79051=CARTESIAN_POINT('Ctrl Pts',(89.2750012853581,58.0260219917234,10.9209957251034));
#79052=CARTESIAN_POINT('Ctrl Pts',(89.231770741624,58.0306979322946,10.8750025832539));
#79053=CARTESIAN_POINT('Ctrl Pts',(89.1860679593757,58.0353738728657,10.8315000500411));
#79054=CARTESIAN_POINT('Ctrl Pts',(89.1412581539756,58.0399584512381,10.788847503483));
#79055=CARTESIAN_POINT('Ctrl Pts',(89.0940722366443,58.0445430296105,10.748589481712));
#79056=CARTESIAN_POINT('Ctrl Pts',(89.0447988437096,58.0491276079829,10.7109963888075));
#79057=CARTESIAN_POINT('Ctrl Pts',(88.9955555658145,58.0537093843409,10.6734262721466));
#79058=CARTESIAN_POINT('Ctrl Pts',(88.9442277459688,58.0582911606988,10.6385181628915));
#79059=CARTESIAN_POINT('Ctrl Pts',(88.8911374198007,58.0628729370568,10.6065024981637));
#79060=CARTESIAN_POINT('Ctrl Pts',(88.8380600416362,58.0674535959822,10.574494641618));
#79061=CARTESIAN_POINT('Ctrl Pts',(88.7832214461921,58.0720342549077,10.5453780919779));
#79062=CARTESIAN_POINT('Ctrl Pts',(88.7269712591976,58.0766149138331,10.519339083185));
#79063=CARTESIAN_POINT('Ctrl Pts',(88.668688943862,58.0813610564187,10.4923593733817));
#79064=CARTESIAN_POINT('Ctrl Pts',(88.6088915929045,58.0861071990042,10.4686841263943));
#79065=CARTESIAN_POINT('Ctrl Pts',(88.5479919189739,58.0908533415897,10.4484665337135));
#79066=CARTESIAN_POINT('Ctrl Pts',(88.4891411802082,58.0954398028861,10.4289291505301));
#79067=CARTESIAN_POINT('Ctrl Pts',(88.429261647752,58.1000262641824,10.4126205088464));
#79068=CARTESIAN_POINT('Ctrl Pts',(88.3687397868389,58.1046127254788,10.3996275684852));
#79069=CARTESIAN_POINT('Ctrl Pts',(88.3050572510133,58.1094387087089,10.3859560888323));
#79070=CARTESIAN_POINT('Ctrl Pts',(88.2406640921925,58.114264691939,10.3759562329338));
#79071=CARTESIAN_POINT('Ctrl Pts',(88.1760177774279,58.119090675169,10.3696674946424));
#79072=CARTESIAN_POINT('Ctrl Pts',(88.1113714626634,58.1239166583991,10.363378756351));
#79073=CARTESIAN_POINT('Ctrl Pts',(88.0464726425025,58.1287426416292,10.3608010840659));
#79074=CARTESIAN_POINT('Ctrl Pts',(87.981776547289,58.1335686248593,10.3619105582712));
#79075=CARTESIAN_POINT('Ctrl Pts',(87.9201471546758,58.1381658484513,10.3629674415524));
#79076=CARTESIAN_POINT('Ctrl Pts',(87.8584486607663,58.1427630720434,10.3673741001395));
#79077=CARTESIAN_POINT('Ctrl Pts',(87.7970749734348,58.1473602956355,10.3751390008019));
#79078=CARTESIAN_POINT('Ctrl Pts',(87.7346504015503,58.1520362362066,10.3830368576956));
#79079=CARTESIAN_POINT('Ctrl Pts',(87.6725623959176,58.1567121767777,10.3944091294685));
#79080=CARTESIAN_POINT('Ctrl Pts',(87.6112258642168,58.1613881173488,10.4092092842007));
#79081=CARTESIAN_POINT('Ctrl Pts',(87.5510877738377,58.1659726957213,10.4237202618877));
#79082=CARTESIAN_POINT('Ctrl Pts',(87.491672574254,58.1705572740937,10.4415262487952));
#79083=CARTESIAN_POINT('Ctrl Pts',(87.433363993645,58.1751418524661,10.4625314222716));
#79084=CARTESIAN_POINT('Ctrl Pts',(87.3750910502248,58.179723628824,10.4835237577519));
#79085=CARTESIAN_POINT('Ctrl Pts',(87.3179238626078,58.184305405182,10.5077112305808));
#79086=CARTESIAN_POINT('Ctrl Pts',(87.2622306976248,58.18888718154,10.5349482806187));
#79087=CARTESIAN_POINT('Ctrl Pts',(87.206551115442,58.1934678404654,10.5621786879131));
#79088=CARTESIAN_POINT('Ctrl Pts',(87.1523452993283,58.1980484993908,10.5924569724198));
#79089=CARTESIAN_POINT('Ctrl Pts',(87.0999593449239,58.2026291583163,10.6255904192215));
#79090=CARTESIAN_POINT('Ctrl Pts',(87.0456808637864,58.2073753009018,10.6599208650002));
#79091=CARTESIAN_POINT('Ctrl Pts',(86.9933567783718,58.2121214434873,10.6973164608235));
#79092=CARTESIAN_POINT('Ctrl Pts',(86.9433396429249,58.2168675860728,10.7375135689326));
#79093=CARTESIAN_POINT('Ctrl Pts',(86.8950053057762,58.2214540473692,10.776358268022));
#79094=CARTESIAN_POINT('Ctrl Pts',(86.8488254862918,58.2260405086656,10.8178185438669));
#79095=CARTESIAN_POINT('Ctrl Pts',(86.8050828595243,58.230626969962,10.8616168857432));
#79096=CARTESIAN_POINT('Ctrl Pts',(86.7590558313697,58.2354529531921,10.9077025386552));
#79097=CARTESIAN_POINT('Ctrl Pts',(86.7157279710292,58.2402789364222,10.9563766851729));
#79098=CARTESIAN_POINT('Ctrl Pts',(86.6753805876875,58.2451049196523,11.0072764189582));
#79099=CARTESIAN_POINT('Ctrl Pts',(86.6350332043458,58.2499309028823,11.0581761527434));
#79100=CARTESIAN_POINT('Ctrl Pts',(86.5976666075079,58.2547568861124,11.1113008992694));
#79101=CARTESIAN_POINT('Ctrl Pts',(86.5635076182577,58.2595828693425,11.1662552359708));
#79102=CARTESIAN_POINT('Ctrl Pts',(86.5300585882811,58.2643085495008,11.2200674036025));
#79103=CARTESIAN_POINT('Ctrl Pts',(86.4995535605494,58.2690342296592,11.2758443580691));
#79104=CARTESIAN_POINT('Ctrl Pts',(86.4722214614649,58.2737599098175,11.3332412095758));
#79105=CARTESIAN_POINT('Ctrl Pts',(86.4449541705362,58.2784743847401,11.3905019652753));
#79106=CARTESIAN_POINT('Ctrl Pts',(86.4208450455069,58.2831888596626,11.4493745572213));
#79107=CARTESIAN_POINT('Ctrl Pts',(86.4000781682881,58.2879033345851,11.5094879267131));
#79108=CARTESIAN_POINT('Ctrl Pts',(86.3793403262532,58.2926112179704,11.5695172487714));
#79109=CARTESIAN_POINT('Ctrl Pts',(86.3619356072016,58.2973191013556,11.6307834624679));
#79110=CARTESIAN_POINT('Ctrl Pts',(86.3480005576707,58.3020269847408,11.6928945317842));
#79111=CARTESIAN_POINT('Ctrl Pts',(86.3340839774588,58.3067286283635,11.7549232799614));
#79112=CARTESIAN_POINT('Ctrl Pts',(86.3236280275323,58.3114302719862,11.8177942005056));
#79113=CARTESIAN_POINT('Ctrl Pts',(86.3167192903354,58.3161319156089,11.8811008046035));
#79114=CARTESIAN_POINT('Ctrl Pts',(86.310004973963,58.3207012488826,11.9426258787601));
#79115=CARTESIAN_POINT('Ctrl Pts',(86.3066408975656,58.3252705821562,12.0045620015264));
#79116=CARTESIAN_POINT('Ctrl Pts',(86.3066600816785,58.3298399154298,12.0665276512002));
#79117=CARTESIAN_POINT('',(86.3066604718792,59.1235899153792,12.0672682606086));
#79118=CARTESIAN_POINT('Ctrl Pts',(86.3066600816788,58.3298399155007,12.0665276521619));
#79119=CARTESIAN_POINT('Ctrl Pts',(86.3066808163434,58.3347785551241,12.1335015396935));
#79120=CARTESIAN_POINT('Ctrl Pts',(86.3106535093132,58.3397171947475,12.2003619829515));
#79121=CARTESIAN_POINT('Ctrl Pts',(86.3185129173098,58.3446558343709,12.2666547047214));
#79122=CARTESIAN_POINT('Ctrl Pts',(86.3263921235412,58.3496069146701,12.3331144211136));
#79123=CARTESIAN_POINT('Ctrl Pts',(86.3381775155799,58.3545579949693,12.3990031909576));
#79124=CARTESIAN_POINT('Ctrl Pts',(86.3537529409633,58.3595090752684,12.4638781483247));
#79125=CARTESIAN_POINT('Ctrl Pts',(86.3693917803471,58.3644803134638,12.5290172384823));
#79126=CARTESIAN_POINT('Ctrl Pts',(86.388851417852,58.3694515516592,12.5931338941111));
#79127=CARTESIAN_POINT('Ctrl Pts',(86.4119657193583,58.3744227898545,12.6558001398209));
#79128=CARTESIAN_POINT('Ctrl Pts',(86.4292844558749,58.3781475645116,12.7027537627818));
#79129=CARTESIAN_POINT('Ctrl Pts',(86.4486538909255,58.3818723391686,12.7488935214905));
#79130=CARTESIAN_POINT('Ctrl Pts',(86.4699872979162,58.3855971138257,12.7940485475684));
#79131=CARTESIAN_POINT('Ctrl Pts',(86.4963176000006,58.3901943374178,12.8497801743908));
#79132=CARTESIAN_POINT('Ctrl Pts',(86.5257292004784,58.3947915610099,12.9041959859528));
#79133=CARTESIAN_POINT('Ctrl Pts',(86.5580676803332,58.3993887846019,12.9569335048519));
#79134=CARTESIAN_POINT('Ctrl Pts',(86.590959882971,58.4040647251731,13.0105740335975));
#79135=CARTESIAN_POINT('Ctrl Pts',(86.6268800000254,58.4087406657442,13.0624777348097));
#79136=CARTESIAN_POINT('Ctrl Pts',(86.6656148451287,58.4134166063153,13.1122856305292));
#79137=CARTESIAN_POINT('Ctrl Pts',(86.7035928584113,58.4180011846877,13.1611203404698));
#79138=CARTESIAN_POINT('Ctrl Pts',(86.7442762687742,58.4225857630601,13.2079399862667));
#79139=CARTESIAN_POINT('Ctrl Pts',(86.7874198018873,58.4271703414326,13.2524342941716));
#79140=CARTESIAN_POINT('Ctrl Pts',(86.8305369664244,58.4317521177905,13.2969014079305));
#79141=CARTESIAN_POINT('Ctrl Pts',(86.8761109186961,58.4363338941485,13.3390456371465));
#79142=CARTESIAN_POINT('Ctrl Pts',(86.9238574195489,58.4409156705064,13.3785912712532));
#79143=CARTESIAN_POINT('Ctrl Pts',(86.971592275684,58.4454963294319,13.4181272607213));
#79144=CARTESIAN_POINT('Ctrl Pts',(87.0214982366928,58.4500769883573,13.4550655886343));
#79145=CARTESIAN_POINT('Ctrl Pts',(87.0732572142,58.4546576472828,13.4891701596366));
#79146=CARTESIAN_POINT('Ctrl Pts',(87.1268860678927,58.4594037898683,13.5245068130372));
#79147=CARTESIAN_POINT('Ctrl Pts',(87.1825039376427,58.4641499324538,13.5568006679624));
#79148=CARTESIAN_POINT('Ctrl Pts',(87.2397254403287,58.4688960750393,13.5858389352836));
#79149=CARTESIAN_POINT('Ctrl Pts',(87.2950217578459,58.4734825363357,13.6139002264865));
#79150=CARTESIAN_POINT('Ctrl Pts',(87.3518149960678,58.4780689976321,13.6389213833942));
#79151=CARTESIAN_POINT('Ctrl Pts',(87.4097358913649,58.4826554589285,13.6607590122859));
#79152=CARTESIAN_POINT('Ctrl Pts',(87.4706816295519,58.4874814421586,13.6837370827429));
#79153=CARTESIAN_POINT('Ctrl Pts',(87.5328754240038,58.4923074253887,13.7031897934175));
#79154=CARTESIAN_POINT('Ctrl Pts',(87.5958707470284,58.4971334086187,13.7190101448349));
#79155=CARTESIAN_POINT('Ctrl Pts',(87.658866070053,58.5019593918488,13.7348304962524));
#79156=CARTESIAN_POINT('Ctrl Pts',(87.7226622706541,58.5067853750789,13.7470184428211));
#79157=CARTESIAN_POINT('Ctrl Pts',(87.7868056147989,58.511611358309,13.7555300273284));
#79158=CARTESIAN_POINT('Ctrl Pts',(87.847908457664,58.5162085819011,13.7636381485625));
#79159=CARTESIAN_POINT('Ctrl Pts',(87.9095771487089,58.5208058054932,13.7684439092126));
#79160=CARTESIAN_POINT('Ctrl Pts',(87.9714234063106,58.5254030290852,13.7698804326689));
#79161=CARTESIAN_POINT('Ctrl Pts',(88.0343286401543,58.5300789696564,13.7713415533162));
#79162=CARTESIAN_POINT('Ctrl Pts',(88.0974170654511,58.5347549102275,13.7693168058526));
#79163=CARTESIAN_POINT('Ctrl Pts',(88.1602714651954,58.5394308507986,13.7637905834579));
#79164=CARTESIAN_POINT('Ctrl Pts',(88.2218977663205,58.544015429171,13.7583723367359));
#79165=CARTESIAN_POINT('Ctrl Pts',(88.2832985734276,58.5486000075434,13.7495882603519));
#79166=CARTESIAN_POINT('Ctrl Pts',(88.3440801824787,58.5531845859159,13.7374761223661));
#79167=CARTESIAN_POINT('Ctrl Pts',(88.404824642869,58.5577663622738,13.725371387108));
#79168=CARTESIAN_POINT('Ctrl Pts',(88.4649501574056,58.5623481386318,13.7099427227589));
#79169=CARTESIAN_POINT('Ctrl Pts',(88.5240709248393,58.5669299149897,13.691279379579));
#79170=CARTESIAN_POINT('Ctrl Pts',(88.5831772735275,58.5715105739152,13.6726205881328));
#79171=CARTESIAN_POINT('Ctrl Pts',(88.6412788763462,58.5760912328406,13.6507288371036));
#79172=CARTESIAN_POINT('Ctrl Pts',(88.6980048538477,58.5806718917661,13.6257433014409));
#79173=CARTESIAN_POINT('Ctrl Pts',(88.7567801483862,58.5854180343516,13.5998551231766));
#79174=CARTESIAN_POINT('Ctrl Pts',(88.8140779633559,58.5901641769371,13.570645520284));
#79175=CARTESIAN_POINT('Ctrl Pts',(88.8695104987765,58.5949103195226,13.5383228447221));
#79176=CARTESIAN_POINT('Ctrl Pts',(88.9230780378227,58.599496780819,13.5070876473402));
#79177=CARTESIAN_POINT('Ctrl Pts',(88.9749034236237,58.6040832421154,13.4729458901017));
#79178=CARTESIAN_POINT('Ctrl Pts',(89.024665899943,58.6086697034118,13.436130022623));
#79179=CARTESIAN_POINT('Ctrl Pts',(89.077027156407,58.6134956866419,13.3973914946881));
#79180=CARTESIAN_POINT('Ctrl Pts',(89.1271036276571,58.6183216698719,13.3556922974774));
#79181=CARTESIAN_POINT('Ctrl Pts',(89.1745632251013,58.623147653102,13.3113495319756));
#79182=CARTESIAN_POINT('Ctrl Pts',(89.2220228225455,58.627973636332,13.2670067664738));
#79183=CARTESIAN_POINT('Ctrl Pts',(89.2668651547817,58.6327996195621,13.2200209548678));
#79184=CARTESIAN_POINT('Ctrl Pts',(89.308807187647,58.6376256027922,13.1707494463867));
#79185=CARTESIAN_POINT('Ctrl Pts',(89.3487610983417,58.6422228263842,13.1238134894205));
#79186=CARTESIAN_POINT('Ctrl Pts',(89.3862475413485,58.6468200499763,13.0746109551229));
#79187=CARTESIAN_POINT('Ctrl Pts',(89.4209997287398,58.6514172735684,13.0234317733154));
#79188=CARTESIAN_POINT('Ctrl Pts',(89.4563469681558,58.6560932141395,12.9713762646333));
#79189=CARTESIAN_POINT('Ctrl Pts',(89.4888650187903,58.6607691547106,12.9172761223816));
#79190=CARTESIAN_POINT('Ctrl Pts',(89.5183144710356,58.6654450952818,12.8614733942796));
#79191=CARTESIAN_POINT('Ctrl Pts',(89.5471885167574,58.6700296736542,12.806760983699));
#79192=CARTESIAN_POINT('Ctrl Pts',(89.573112550046,58.6746142520266,12.7504123935714));
#79193=CARTESIAN_POINT('Ctrl Pts',(89.5959047560652,58.679198830399,12.6927788683434));
#79194=CARTESIAN_POINT('Ctrl Pts',(89.618683031885,58.683780606757,12.6351805677223));
#79195=CARTESIAN_POINT('Ctrl Pts',(89.6383330890393,58.6883623831149,12.5762993615891));
#79196=CARTESIAN_POINT('Ctrl Pts',(89.654720650441,58.6929441594729,12.5165077789716));
#79197=CARTESIAN_POINT('Ctrl Pts',(89.6711042151408,58.6975248183983,12.4567307787023));
#79198=CARTESIAN_POINT('Ctrl Pts',(89.6842267291334,58.7021054773238,12.3960443334303));
#79199=CARTESIAN_POINT('Ctrl Pts',(89.6940039516866,58.7066861362492,12.3348355151524));
#79200=CARTESIAN_POINT('Ctrl Pts',(89.7041343921065,58.7114322788347,12.2714154300149));
#79201=CARTESIAN_POINT('Ctrl Pts',(89.710673050288,58.7161784214203,12.2074350701328));
#79202=CARTESIAN_POINT('Ctrl Pts',(89.7135846248931,58.7209245640058,12.1433332443245));
#79203=CARTESIAN_POINT('Ctrl Pts',(89.7163982412135,58.7255110253022,12.0813880882738));
#79204=CARTESIAN_POINT('Ctrl Pts',(89.7158250532987,58.7300974865985,12.0193300375764));
#79205=CARTESIAN_POINT('Ctrl Pts',(89.7118863692065,58.7346839478949,11.9575546467217));
#79206=CARTESIAN_POINT('Ctrl Pts',(89.7077419924965,58.739509931125,11.8925531169954));
#79207=CARTESIAN_POINT('Ctrl Pts',(89.6998710301739,58.7443359143551,11.8278652203452));
#79208=CARTESIAN_POINT('Ctrl Pts',(89.6883597610478,58.7491618975852,11.76394194661));
#79209=CARTESIAN_POINT('Ctrl Pts',(89.6768484919216,58.7539878808152,11.7000186728747));
#79210=CARTESIAN_POINT('Ctrl Pts',(89.6616971423962,58.7588138640453,11.6368606341129));
#79211=CARTESIAN_POINT('Ctrl Pts',(89.6430524117444,58.7636398472754,11.5748994390969));
#79212=CARTESIAN_POINT('Ctrl Pts',(89.6252914723598,58.7682370708675,11.5158753078596));
#79213=CARTESIAN_POINT('Ctrl Pts',(89.6042879819519,58.7728342944595,11.4576947597245));
#79214=CARTESIAN_POINT('Ctrl Pts',(89.5801408112597,58.7774315180516,11.4007391864545));
#79215=CARTESIAN_POINT('Ctrl Pts',(89.5555801752897,58.7821074586227,11.3428083787678));
#79216=CARTESIAN_POINT('Ctrl Pts',(89.5277672508755,58.7867833991939,11.2861454257539));
#79217=CARTESIAN_POINT('Ctrl Pts',(89.4968595440726,58.791459339765,11.2311369867526));
#79218=CARTESIAN_POINT('Ctrl Pts',(89.4665557363157,58.7960439181374,11.1772033458286));
#79219=CARTESIAN_POINT('Ctrl Pts',(89.4332772563873,58.8006284965098,11.1248606110418));
#79220=CARTESIAN_POINT('Ctrl Pts',(89.3972205760408,58.8052130748822,11.0744520434386));
#79221=CARTESIAN_POINT('Ctrl Pts',(89.3611859329093,58.8097948512402,11.0240742846739));
#79222=CARTESIAN_POINT('Ctrl Pts',(89.3223767517619,58.8143766275981,10.9756287622745));
#79223=CARTESIAN_POINT('Ctrl Pts',(89.2810331703959,58.8189584039561,10.9294303445481));
#79224=CARTESIAN_POINT('Ctrl Pts',(89.2396996721633,58.8235390628815,10.8832431939831));
#79225=CARTESIAN_POINT('Ctrl Pts',(89.1958333400602,58.828119721807,10.8393024393121));
#79226=CARTESIAN_POINT('Ctrl Pts',(89.1497136693969,58.8327003807324,10.79788880033));
#79227=CARTESIAN_POINT('Ctrl Pts',(89.1019278515643,58.8374465233179,10.7549790271307));
#79228=CARTESIAN_POINT('Ctrl Pts',(89.0517231568139,58.8421926659035,10.7147828939027));
#79229=CARTESIAN_POINT('Ctrl Pts',(88.999449090322,58.846938808489,10.6775680674078));
#79230=CARTESIAN_POINT('Ctrl Pts',(88.9489337552998,58.8515252697854,10.6416053127506));
#79231=CARTESIAN_POINT('Ctrl Pts',(88.8964865766668,58.8561117310817,10.6084266501165));
#79232=CARTESIAN_POINT('Ctrl Pts',(88.8424514255881,58.8606981923781,10.5782287264208));
#79233=CARTESIAN_POINT('Ctrl Pts',(88.7855943595217,58.8655241756082,10.5464537557145));
#79234=CARTESIAN_POINT('Ctrl Pts',(88.7269794878156,58.8703501588383,10.5179796826691));
#79235=CARTESIAN_POINT('Ctrl Pts',(88.6670324941007,58.8751761420684,10.4929786389613));
#79236=CARTESIAN_POINT('Ctrl Pts',(88.6070855003858,58.8800021252984,10.4679775952535));
#79237=CARTESIAN_POINT('Ctrl Pts',(88.5458070216668,58.8848281085285,10.4464497226561));
#79238=CARTESIAN_POINT('Ctrl Pts',(88.4836392311151,58.8896540917586,10.4285058800683));
#79239=CARTESIAN_POINT('Ctrl Pts',(88.4244182973144,58.8942513153507,10.4114126054869));
#79240=CARTESIAN_POINT('Ctrl Pts',(88.3641473198731,58.8988485389428,10.3975010250991));
#79241=CARTESIAN_POINT('Ctrl Pts',(88.303200341452,58.9034457625348,10.3868949419243));
#79242=CARTESIAN_POINT('Ctrl Pts',(88.2412097848958,58.908121703106,10.3761072537416));
#79243=CARTESIAN_POINT('Ctrl Pts',(88.1785203426625,58.9127976436771,10.368739564741));
#79244=CARTESIAN_POINT('Ctrl Pts',(88.1155422865393,58.9174735842482,10.3648692742987));
#79245=CARTESIAN_POINT('Ctrl Pts',(88.0537947451307,58.9220581626206,10.3610746046301));
#79246=CARTESIAN_POINT('Ctrl Pts',(87.9917702991426,58.9266427409931,10.3606419255504));
#79247=CARTESIAN_POINT('Ctrl Pts',(87.9298638954832,58.9312273193655,10.3635923613471));
#79248=CARTESIAN_POINT('Ctrl Pts',(87.8679953279395,58.9358090957234,10.3665409938887));
#79249=CARTESIAN_POINT('Ctrl Pts',(87.8062451670857,58.9403908720814,10.3728686171715));
#79250=CARTESIAN_POINT('Ctrl Pts',(87.7450081908972,58.9449726484394,10.3825442705286));
#79251=CARTESIAN_POINT('Ctrl Pts',(87.6837861495685,58.9495533073648,10.3922175641263));
#79252=CARTESIAN_POINT('Ctrl Pts',(87.6230775470304,58.9541339662903,10.4052371874353));
#79253=CARTESIAN_POINT('Ctrl Pts',(87.563269819836,58.9587146252157,10.4215205925977));
#79254=CARTESIAN_POINT('Ctrl Pts',(87.5013014424476,58.9634607678013,10.4383922619221));
#79255=CARTESIAN_POINT('Ctrl Pts',(87.4403008556013,58.9682069103868,10.4587679559189));
#79256=CARTESIAN_POINT('Ctrl Pts',(87.3806825029854,58.9729530529723,10.4824992300105));
#79257=CARTESIAN_POINT('Ctrl Pts',(87.3230699762016,58.9775395142687,10.5054320787766));
#79258=CARTESIAN_POINT('Ctrl Pts',(87.2667485944832,58.9821259755651,10.5314979983285));
#79259=CARTESIAN_POINT('Ctrl Pts',(87.2120700803616,58.9867124368615,10.5605147562641));
#79260=CARTESIAN_POINT('Ctrl Pts',(87.1545360524603,58.9915384200915,10.5910468763755));
#79261=CARTESIAN_POINT('Ctrl Pts',(87.0988217469623,58.9963644033216,10.6248461690274));
#79262=CARTESIAN_POINT('Ctrl Pts',(87.0453026656082,59.0011903865517,10.661648372398));
#79263=CARTESIAN_POINT('Ctrl Pts',(86.9917835842541,59.0060163697817,10.6984505757685));
#79264=CARTESIAN_POINT('Ctrl Pts',(86.9404601916607,59.0108423530118,10.7382552315939));
#79265=CARTESIAN_POINT('Ctrl Pts',(86.8916654569177,59.0156683362419,10.7807509905615));
#79266=CARTESIAN_POINT('Ctrl Pts',(86.8458789933511,59.0201967901109,10.8206268199917));
#79267=CARTESIAN_POINT('Ctrl Pts',(86.8021189271895,59.02472524398,10.8630459958341));
#79268=CARTESIAN_POINT('Ctrl Pts',(86.7606873677575,59.029253697849,10.9077715435827));
#79269=CARTESIAN_POINT('Ctrl Pts',(86.7193124721653,59.0337759583817,10.952435922471));
#79270=CARTESIAN_POINT('Ctrl Pts',(86.6802601326207,59.0382982189143,10.9994000478932));
#79271=CARTESIAN_POINT('Ctrl Pts',(86.6437985928296,59.042820479447,11.0483875257097));
#79272=CARTESIAN_POINT('Ctrl Pts',(86.6073725997099,59.0473383311886,11.0973272452091));
#79273=CARTESIAN_POINT('Ctrl Pts',(86.5735327161805,59.0518561829303,11.1482859914009));
#79274=CARTESIAN_POINT('Ctrl Pts',(86.5425080117181,59.0563740346719,11.2009531134372));
#79275=CARTESIAN_POINT('Ctrl Pts',(86.5115013763062,59.0608892551784,11.253589561696));
#79276=CARTESIAN_POINT('Ctrl Pts',(86.4833069364353,59.065404475685,11.3079319621111));
#79277=CARTESIAN_POINT('Ctrl Pts',(86.4581100863428,59.0699196961915,11.3636412941652));
#79278=CARTESIAN_POINT('Ctrl Pts',(86.432903837136,59.0744366009988,11.4193714073244));
#79279=CARTESIAN_POINT('Ctrl Pts',(86.4106976423061,59.0789535058061,11.4764689979253));
#79280=CARTESIAN_POINT('Ctrl Pts',(86.391629846485,59.0834704106135,11.5345725435163));
#79281=CARTESIAN_POINT('Ctrl Pts',(86.3725597501086,59.0879878603914,11.5926830993781));
#79282=CARTESIAN_POINT('Ctrl Pts',(86.3566289553476,59.0925053101694,11.651799347088));
#79283=CARTESIAN_POINT('Ctrl Pts',(86.3439257959816,59.0970227599473,11.7115448774579));
#79284=CARTESIAN_POINT('Ctrl Pts',(86.3312035786438,59.1015469870495,11.7713800413276));
#79285=CARTESIAN_POINT('Ctrl Pts',(86.3217187612233,59.1060712141517,11.8318458547642));
#79286=CARTESIAN_POINT('Ctrl Pts',(86.3155082094182,59.110595441254,11.89255714581));
#79287=CARTESIAN_POINT('Ctrl Pts',(86.309562232134,59.114926932629,11.9506820868425));
#79288=CARTESIAN_POINT('Ctrl Pts',(86.3066171358679,59.1192584240041,12.0090315885683));
#79289=CARTESIAN_POINT('Ctrl Pts',(86.3066604718792,59.1235899153792,12.0672682606086));
#79290=CARTESIAN_POINT('',(86.306660521223,59.9173399154754,12.0646670776546));
#79291=CARTESIAN_POINT('Ctrl Pts',(86.3066604718797,59.1235899154298,12.0672682612888));
#79292=CARTESIAN_POINT('Ctrl Pts',(86.3067208101713,59.1296208038615,12.1483532367145));
#79293=CARTESIAN_POINT('Ctrl Pts',(86.3125682407869,59.1356516922933,12.2292263611692));
#79294=CARTESIAN_POINT('Ctrl Pts',(86.3241094256459,59.1416825807251,12.3092591740417));
#79295=CARTESIAN_POINT('Ctrl Pts',(86.3329070361332,59.1462798043172,12.3702665595444));
#79296=CARTESIAN_POINT('Ctrl Pts',(86.3450365252776,59.1508770279093,12.4309213061331));
#79297=CARTESIAN_POINT('Ctrl Pts',(86.3604567637294,59.1554742515014,12.490831567567));
#79298=CARTESIAN_POINT('Ctrl Pts',(86.376141038629,59.1601501920726,12.5517676557197));
#79299=CARTESIAN_POINT('Ctrl Pts',(86.3952298350125,59.1648261326437,12.6119329851159));
#79300=CARTESIAN_POINT('Ctrl Pts',(86.4176248208747,59.1695020732149,12.6709217917609));
#79301=CARTESIAN_POINT('Ctrl Pts',(86.4395822359172,59.1740866515873,12.7287580287803));
#79302=CARTESIAN_POINT('Ctrl Pts',(86.46471761521,59.1786712299597,12.7854628065256));
#79303=CARTESIAN_POINT('Ctrl Pts',(86.4928876476361,59.1832558083321,12.8406674907341));
#79304=CARTESIAN_POINT('Ctrl Pts',(86.5210404630291,59.1878375846901,12.8958384348011));
#79305=CARTESIAN_POINT('Ctrl Pts',(86.552224023004,59.1924193610481,12.9495106507903));
#79306=CARTESIAN_POINT('Ctrl Pts',(86.5862476177626,59.197001137406,13.0013370969382));
#79307=CARTESIAN_POINT('Ctrl Pts',(86.6202629146324,59.2015817963315,13.0531509033257));
#79308=CARTESIAN_POINT('Ctrl Pts',(86.6571165920408,59.206162455257,13.1031194081535));
#79309=CARTESIAN_POINT('Ctrl Pts',(86.6965739473985,59.2107431141824,13.1509234940043));
#79310=CARTESIAN_POINT('Ctrl Pts',(86.7374567630855,59.2154892567679,13.2004545792279));
#79311=CARTESIAN_POINT('Ctrl Pts',(86.7811346619707,59.2202353993534,13.2476613758826));
#79312=CARTESIAN_POINT('Ctrl Pts',(86.8273017694101,59.2249815419388,13.292227276853));
#79313=CARTESIAN_POINT('Ctrl Pts',(86.8719156105713,59.2295680032352,13.3352937832333));
#79314=CARTESIAN_POINT('Ctrl Pts',(86.9188533668513,59.2341544645316,13.375893995501));
#79315=CARTESIAN_POINT('Ctrl Pts',(86.9678041871651,59.238740925828,13.4137823754908));
#79316=CARTESIAN_POINT('Ctrl Pts',(87.0193113999516,59.243566909058,13.4536494264976));
#79317=CARTESIAN_POINT('Ctrl Pts',(87.0730471767966,59.2483928922881,13.4905132611832));
#79318=CARTESIAN_POINT('Ctrl Pts',(87.1286161204782,59.2532188755181,13.5241404338266));
#79319=CARTESIAN_POINT('Ctrl Pts',(87.1841850641597,59.2580448587481,13.55776760647));
#79320=CARTESIAN_POINT('Ctrl Pts',(87.2415865657944,59.2628708419781,13.5881578822621));
#79321=CARTESIAN_POINT('Ctrl Pts',(87.3003998211841,59.2676968252082,13.6151359596455));
#79322=CARTESIAN_POINT('Ctrl Pts',(87.3564252303735,59.2722940488002,13.6408352312558));
#79323=CARTESIAN_POINT('Ctrl Pts',(87.4139615870079,59.2768912723923,13.6635440501566));
#79324=CARTESIAN_POINT('Ctrl Pts',(87.4726573842561,59.2814884959844,13.683084433069));
#79325=CARTESIAN_POINT('Ctrl Pts',(87.5323582132914,59.2861644365555,13.7029594005151));
#79326=CARTESIAN_POINT('Ctrl Pts',(87.5932581198193,59.2908403771266,13.7195560987896));
#79327=CARTESIAN_POINT('Ctrl Pts',(87.6549628777595,59.2955163176978,13.7327370528031));
#79328=CARTESIAN_POINT('Ctrl Pts',(87.7154619996849,59.3001008960702,13.7456604669866));
#79329=CARTESIAN_POINT('Ctrl Pts',(87.7767342825985,59.3046854744426,13.7553003040122));
#79330=CARTESIAN_POINT('Ctrl Pts',(87.8383922972793,59.309270052815,13.7615770158154));
#79331=CARTESIAN_POINT('Ctrl Pts',(87.9000126276553,59.313851829173,13.7678498914017));
#79332=CARTESIAN_POINT('Ctrl Pts',(87.9620177169563,59.318433605531,13.7707636660454));
#79333=CARTESIAN_POINT('Ctrl Pts',(88.0240125672906,59.3230153818889,13.7702903240623));
#79334=CARTESIAN_POINT('Ctrl Pts',(88.0859922979299,59.3275960408144,13.7698170975209));
#79335=CARTESIAN_POINT('Ctrl Pts',(88.1479612857555,59.3321766997399,13.7659583981145));
#79336=CARTESIAN_POINT('Ctrl Pts',(88.2095241310749,59.3367573586653,13.7587383155647));
#79337=CARTESIAN_POINT('Ctrl Pts',(88.2733110330491,59.3415035012509,13.7512573959377));
#79338=CARTESIAN_POINT('Ctrl Pts',(88.3366613006586,59.3462496438364,13.7401675764964));
#79339=CARTESIAN_POINT('Ctrl Pts',(88.3991430395344,59.3509957864219,13.7255541016975));
#79340=CARTESIAN_POINT('Ctrl Pts',(88.4595226155632,59.3555822477183,13.711432289012));
#79341=CARTESIAN_POINT('Ctrl Pts',(88.5190906943802,59.3601687090147,13.6940203911597));
#79342=CARTESIAN_POINT('Ctrl Pts',(88.5774723889305,59.3647551703111,13.6734463811211));
#79343=CARTESIAN_POINT('Ctrl Pts',(88.6389029910079,59.3695811535412,13.6517979203569));
#79344=CARTESIAN_POINT('Ctrl Pts',(88.6990192978616,59.3744071367713,13.6266482549287));
#79345=CARTESIAN_POINT('Ctrl Pts',(88.7574107238353,59.3792331200013,13.5982029457431));
#79346=CARTESIAN_POINT('Ctrl Pts',(88.8158021498089,59.3840591032314,13.5697576365574));
#79347=CARTESIAN_POINT('Ctrl Pts',(88.8724681673767,59.3888850864615,13.5380170677901));
#79348=CARTESIAN_POINT('Ctrl Pts',(88.9270332583123,59.3937110696915,13.5032396826089));
#79349=CARTESIAN_POINT('Ctrl Pts',(88.9790118731136,59.3983082932836,13.4701108033724));
#79350=CARTESIAN_POINT('Ctrl Pts',(89.0292976813082,59.4029055168757,13.4340905273487));
#79351=CARTESIAN_POINT('Ctrl Pts',(89.077550498505,59.4075027404678,13.3953776249579));
#79352=CARTESIAN_POINT('Ctrl Pts',(89.1266295352504,59.4121786810389,13.3560018523225));
#79353=CARTESIAN_POINT('Ctrl Pts',(89.1736048068095,59.41685462161,13.3138405801563));
#79354=CARTESIAN_POINT('Ctrl Pts',(89.2181469897109,59.4215305621812,13.269150439817));
#79355=CARTESIAN_POINT('Ctrl Pts',(89.2618188724656,59.4261151405536,13.2253334905331));
#79356=CARTESIAN_POINT('Ctrl Pts',(89.3031515140972,59.430699718926,13.1790859841457));
#79357=CARTESIAN_POINT('Ctrl Pts',(89.3418679434624,59.4352842972984,13.1306902613737));
#79358=CARTESIAN_POINT('Ctrl Pts',(89.3805607100203,59.4398660736563,13.0823241172246));
#79359=CARTESIAN_POINT('Ctrl Pts',(89.4166401175261,59.4444478500143,13.0318127567608));
#79360=CARTESIAN_POINT('Ctrl Pts',(89.4498683830425,59.4490296263722,12.9794728304009));
#79361=CARTESIAN_POINT('Ctrl Pts',(89.48308854464,59.4536102852977,12.9271456690323));
#79362=CARTESIAN_POINT('Ctrl Pts',(89.5134586719212,59.4581909442231,12.8729912566345));
#79363=CARTESIAN_POINT('Ctrl Pts',(89.5407845388671,59.4627716031486,12.8173548430955));
#79364=CARTESIAN_POINT('Ctrl Pts',(89.5690975966409,59.4675177457341,12.7597084747671));
#79365=CARTESIAN_POINT('Ctrl Pts',(89.5941419113378,59.4722638883196,12.7004714694172));
#79366=CARTESIAN_POINT('Ctrl Pts',(89.6157548396587,59.4770100309051,12.6400529071366));
#79367=CARTESIAN_POINT('Ctrl Pts',(89.636640613202,59.4815964922015,12.5816670932909));
#79368=CARTESIAN_POINT('Ctrl Pts',(89.6543221614587,59.4861829534979,12.5221784973082));
#79369=CARTESIAN_POINT('Ctrl Pts',(89.668703658964,59.4907694147943,12.4619714821262));
#79370=CARTESIAN_POINT('Ctrl Pts',(89.6838362113392,59.4955953980243,12.3986202344377));
#79371=CARTESIAN_POINT('Ctrl Pts',(89.6953144554487,59.5004213812544,12.3344741049122));
#79372=CARTESIAN_POINT('Ctrl Pts',(89.7030883862101,59.5052473644845,12.269989531234));
#79373=CARTESIAN_POINT('Ctrl Pts',(89.7108623169714,59.5100733477146,12.2055049575557));
#79374=CARTESIAN_POINT('Ctrl Pts',(89.7149319710093,59.5148993309447,12.1406825912867));
#79375=CARTESIAN_POINT('Ctrl Pts',(89.715310791279,59.5197253141747,12.0759780924933));
#79376=CARTESIAN_POINT('Ctrl Pts',(89.7156716548375,59.5243225377668,12.014340694644));
#79377=CARTESIAN_POINT('Ctrl Pts',(89.7126852185318,59.5289197613589,11.9525571694224));
#79378=CARTESIAN_POINT('Ctrl Pts',(89.7063339580072,59.533516984951,11.8910211257674));
#79379=CARTESIAN_POINT('Ctrl Pts',(89.6998739466177,59.5381929255221,11.8284314175772));
#79380=CARTESIAN_POINT('Ctrl Pts',(89.689932698466,59.5428688660932,11.7660982755586));
#79381=CARTESIAN_POINT('Ctrl Pts',(89.6765471903453,59.5475448066643,11.704437567863));
#79382=CARTESIAN_POINT('Ctrl Pts',(89.6634232187934,59.5521293850367,11.6439816354941));
#79383=CARTESIAN_POINT('Ctrl Pts',(89.64698848327,59.5567139634091,11.5841726179499));
#79384=CARTESIAN_POINT('Ctrl Pts',(89.627329955385,59.5612985417816,11.5253963458087));
#79385=CARTESIAN_POINT('Ctrl Pts',(89.6076834424499,59.5658803181395,11.4666559967013));
#79386=CARTESIAN_POINT('Ctrl Pts',(89.5848172051553,59.5704620944975,11.4089476231853));
#79387=CARTESIAN_POINT('Ctrl Pts',(89.5588682950506,59.5750438708554,11.3526427425356));
#79388=CARTESIAN_POINT('Ctrl Pts',(89.5329257135297,59.5796245297809,11.2963515938752));
#79389=CARTESIAN_POINT('Ctrl Pts',(89.5039021646468,59.5842051887063,11.2414637206838));
#79390=CARTESIAN_POINT('Ctrl Pts',(89.4719823521895,59.5887858476318,11.188329559464));
#79391=CARTESIAN_POINT('Ctrl Pts',(89.4389093852451,59.5935319902173,11.1332758413385));
#79392=CARTESIAN_POINT('Ctrl Pts',(89.402727128262,59.5982781328028,11.0801055039213));
#79393=CARTESIAN_POINT('Ctrl Pts',(89.3636910405609,59.6030242753883,11.0291770718265));
#79394=CARTESIAN_POINT('Ctrl Pts',(89.325968300003,59.6076107366847,10.9799620980914));
#79395=CARTESIAN_POINT('Ctrl Pts',(89.285581120993,59.6121971979811,10.9328409141891));
#79396=CARTESIAN_POINT('Ctrl Pts',(89.2428004393584,59.6167836592775,10.8881025031029));
#79397=CARTESIAN_POINT('Ctrl Pts',(89.1977855926613,59.6216096425075,10.841027687098));
#79398=CARTESIAN_POINT('Ctrl Pts',(89.1501208566216,59.6264356257376,10.796591789907));
#79399=CARTESIAN_POINT('Ctrl Pts',(89.1001625715059,59.6312616089677,10.7550843930937));
#79400=CARTESIAN_POINT('Ctrl Pts',(89.0502042863902,59.6360875921977,10.7135769962803));
#79401=CARTESIAN_POINT('Ctrl Pts',(88.9979530194548,59.6409135754278,10.6749984224819));
#79402=CARTESIAN_POINT('Ctrl Pts',(88.9437988718105,59.6457395586579,10.6395845274434));
#79403=CARTESIAN_POINT('Ctrl Pts',(88.8922117209045,59.65033678225,10.6058493099763));
#79404=CARTESIAN_POINT('Ctrl Pts',(88.8386862339935,59.6549340058421,10.5748469706846));
#79405=CARTESIAN_POINT('Ctrl Pts',(88.7835435850918,59.6595312294341,10.5468057251511));
#79406=CARTESIAN_POINT('Ctrl Pts',(88.7274567439725,59.6642071700053,10.5182843371811));
#79407=CARTESIAN_POINT('Ctrl Pts',(88.6696972310118,59.6688831105764,10.4928267710902));
#79408=CARTESIAN_POINT('Ctrl Pts',(88.6106344820152,59.6735590511475,10.4706275282623));
#79409=CARTESIAN_POINT('Ctrl Pts',(88.5527257473881,59.6781436295199,10.448862031673));
#79410=CARTESIAN_POINT('Ctrl Pts',(88.4935647453181,59.6827282078923,10.4302288637889));
#79411=CARTESIAN_POINT('Ctrl Pts',(88.433522793536,59.6873127862648,10.4148642319474));
#79412=CARTESIAN_POINT('Ctrl Pts',(88.3735175383491,59.6918945626227,10.3995089907014));
#79413=CARTESIAN_POINT('Ctrl Pts',(88.3126328931943,59.6964763389807,10.3874184503386));
#79414=CARTESIAN_POINT('Ctrl Pts',(88.2512553141907,59.7010581153387,10.3786789814611));
#79415=CARTESIAN_POINT('Ctrl Pts',(88.1898927043381,59.7056387742641,10.3699416440204));
#79416=CARTESIAN_POINT('Ctrl Pts',(88.1280379030294,59.7102194331896,10.3645538273662));
#79417=CARTESIAN_POINT('Ctrl Pts',(88.0660855024955,59.714800092115,10.3625504342615));
#79418=CARTESIAN_POINT('Ctrl Pts',(88.0018949719991,59.7195462347006,10.3604746653635));
#79419=CARTESIAN_POINT('Ctrl Pts',(87.9376002344375,59.7242923772861,10.3620326202201));
#79420=CARTESIAN_POINT('Ctrl Pts',(87.873641054749,59.7290385198716,10.3672041453549));
#79421=CARTESIAN_POINT('Ctrl Pts',(87.81183374557,59.733624981168,10.3722016774447));
#79422=CARTESIAN_POINT('Ctrl Pts',(87.7503402854361,59.7382114424644,10.3805733297022));
#79423=CARTESIAN_POINT('Ctrl Pts',(87.6895504103278,59.7427979037608,10.3922482272154));
#79424=CARTESIAN_POINT('Ctrl Pts',(87.625585863617,59.7476238869908,10.404532830959));
#79425=CARTESIAN_POINT('Ctrl Pts',(87.5624010317684,59.7524498702209,10.4204750091404));
#79426=CARTESIAN_POINT('Ctrl Pts',(87.5004324769044,59.757275853451,10.4399324614396));
#79427=CARTESIAN_POINT('Ctrl Pts',(87.4384639220403,59.762101836681,10.4593899137387));
#79428=CARTESIAN_POINT('Ctrl Pts',(87.3777122228942,59.7669278199111,10.4823623385896));
#79429=CARTESIAN_POINT('Ctrl Pts',(87.3185871172308,59.7717538031412,10.5086499316547));
#79430=CARTESIAN_POINT('Ctrl Pts',(87.2622646399899,59.7763510267333,10.5336914490525));
#79431=CARTESIAN_POINT('Ctrl Pts',(87.2071867605101,59.7809482503253,10.5618437133064));
#79432=CARTESIAN_POINT('Ctrl Pts',(87.1537194119223,59.7855454739174,10.5929606831774));
#79433=CARTESIAN_POINT('Ctrl Pts',(87.0993365568175,59.7902214144885,10.6246104602561));
#79434=CARTESIAN_POINT('Ctrl Pts',(87.0466204281995,59.7948973550596,10.6593272975581));
#79435=CARTESIAN_POINT('Ctrl Pts',(86.9959348123226,59.7995732956308,10.6969063215523));
#79436=CARTESIAN_POINT('Ctrl Pts',(86.9462395318102,59.8041578740032,10.7337510970663));
#79437=CARTESIAN_POINT('Ctrl Pts',(86.8984965586452,59.8087424523756,10.7733469001858));
#79438=CARTESIAN_POINT('Ctrl Pts',(86.8530217257735,59.813327030748,10.8154556577156));
#79439=CARTESIAN_POINT('Ctrl Pts',(86.8075746863276,59.817908807106,10.8575386791063));
#79440=CARTESIAN_POINT('Ctrl Pts',(86.7643934111796,59.8224905834639,10.9021312643472));
#79441=CARTESIAN_POINT('Ctrl Pts',(86.7237600754219,59.8270723598219,10.9489555907789));
#79442=CARTESIAN_POINT('Ctrl Pts',(86.6831366495782,59.8316530187473,10.9957684973987));
#79443=CARTESIAN_POINT('Ctrl Pts',(86.6450602630228,59.8362336776727,11.0448116804123));
#79444=CARTESIAN_POINT('Ctrl Pts',(86.6097742646436,59.8408143365982,11.0957725657482));
#79445=CARTESIAN_POINT('Ctrl Pts',(86.5732135029048,59.8455604791837,11.1485744949083));
#79446=CARTESIAN_POINT('Ctrl Pts',(86.5396489876384,59.8503066217692,11.2034348978998));
#79447=CARTESIAN_POINT('Ctrl Pts',(86.5093023154406,59.8550527643547,11.2599733876671));
#79448=CARTESIAN_POINT('Ctrl Pts',(86.4799766399047,59.8596392256511,11.3146096718499));
#79449=CARTESIAN_POINT('Ctrl Pts',(86.4536558654889,59.8642256869475,11.3708124034107));
#79450=CARTESIAN_POINT('Ctrl Pts',(86.4304918409927,59.8688121482439,11.4282157144369));
#79451=CARTESIAN_POINT('Ctrl Pts',(86.4061181056582,59.873638131474,11.4886168381923));
#79452=CARTESIAN_POINT('Ctrl Pts',(86.3852400924201,59.8784641147041,11.5503467708357));
#79453=CARTESIAN_POINT('Ctrl Pts',(86.3679750425218,59.8832900979342,11.6129615637679));
#79454=CARTESIAN_POINT('Ctrl Pts',(86.3507099926235,59.8881160811642,11.6755763567001));
#79455=CARTESIAN_POINT('Ctrl Pts',(86.3370579666174,59.8929420643943,11.739075360146));
#79456=CARTESIAN_POINT('Ctrl Pts',(86.3270733459061,59.8977680476244,11.8030059711094));
#79457=CARTESIAN_POINT('Ctrl Pts',(86.3135757387981,59.9042920035595,11.8894299118791));
#79458=CARTESIAN_POINT('Ctrl Pts',(86.3067291470103,59.9108159594947,11.9769188414441));
#79459=CARTESIAN_POINT('Ctrl Pts',(86.3066605212234,59.9173399154298,12.0646670770413));
#79460=CARTESIAN_POINT('',(86.3066600524911,60.7110899153719,12.0655770041428));
#79461=CARTESIAN_POINT('Ctrl Pts',(86.306660521223,59.9173399154754,12.0646670776546));
#79462=CARTESIAN_POINT('Ctrl Pts',(86.3066129479909,59.9218624984084,12.1254965309288));
#79463=CARTESIAN_POINT('Ctrl Pts',(86.3098261904978,59.9263850813415,12.1864461177575));
#79464=CARTESIAN_POINT('Ctrl Pts',(86.3163123336439,59.9309076642745,12.24713130348));
#79465=CARTESIAN_POINT('Ctrl Pts',(86.3227916386046,59.9354254791567,12.3077525102656));
#79466=CARTESIAN_POINT('Ctrl Pts',(86.3325369576799,59.939943294039,12.3681093485899));
#79467=CARTESIAN_POINT('Ctrl Pts',(86.3455083588812,59.9444611089212,12.4278182264114));
#79468=CARTESIAN_POINT('Ctrl Pts',(86.3584711803611,59.9489759355686,12.4874876107709));
#79469=CARTESIAN_POINT('Ctrl Pts',(86.3746557460688,59.9534907622159,12.5465093713017));
#79470=CARTESIAN_POINT('Ctrl Pts',(86.3939707165961,59.9580055888633,12.6045082471181));
#79471=CARTESIAN_POINT('Ctrl Pts',(86.4132804969975,59.9625192023316,12.6624915380562));
#79472=CARTESIAN_POINT('Ctrl Pts',(86.4357188476173,59.9670328157999,12.7194519911633));
#79473=CARTESIAN_POINT('Ctrl Pts',(86.4611447048284,59.9715464292682,12.775029900377));
#79474=CARTESIAN_POINT('Ctrl Pts',(86.4865916952581,59.9760637943181,12.8306540043007));
#79475=CARTESIAN_POINT('Ctrl Pts',(86.5150309359955,59.980581159368,12.8848927886205));
#79476=CARTESIAN_POINT('Ctrl Pts',(86.5462739446734,59.985098524418,12.9374082960631));
#79477=CARTESIAN_POINT('Ctrl Pts',(86.5775291932197,59.9896176592064,12.989944377161));
#79478=CARTESIAN_POINT('Ctrl Pts',(86.6115901042272,59.9941367939947,13.0407553994953));
#79479=CARTESIAN_POINT('Ctrl Pts',(86.6482248598373,59.9986559287831,13.0895324874935));
#79480=CARTESIAN_POINT('Ctrl Pts',(86.684927495256,60.0031834369862,13.1383999535858));
#79481=CARTESIAN_POINT('Ctrl Pts',(86.7242131612465,60.0077109451894,13.1852255552867));
#79482=CARTESIAN_POINT('Ctrl Pts',(86.76581046214,60.0122384533925,13.2297344415304));
#79483=CARTESIAN_POINT('Ctrl Pts',(86.8011641645117,60.0160863996309,13.2675627112343));
#79484=CARTESIAN_POINT('Ctrl Pts',(86.8381868570541,60.0199343458693,13.303718035511));
#79485=CARTESIAN_POINT('Ctrl Pts',(86.876693414237,60.0237822921076,13.3380547964198));
#79486=CARTESIAN_POINT('Ctrl Pts',(86.9226980208934,60.0283795156997,13.3790776583694));
#79487=CARTESIAN_POINT('Ctrl Pts',(86.9710253567054,60.0329767392918,13.4176858363108));
#79488=CARTESIAN_POINT('Ctrl Pts',(87.0213917046313,60.0375739628839,13.4536059445453));
#79489=CARTESIAN_POINT('Ctrl Pts',(87.0726204615035,60.042249903455,13.4901411027878));
#79490=CARTESIAN_POINT('Ctrl Pts',(87.1259583820144,60.0469258440261,13.5238948469401));
#79491=CARTESIAN_POINT('Ctrl Pts',(87.1810690153139,60.0516017845973,13.5546199636771));
#79492=CARTESIAN_POINT('Ctrl Pts',(87.2351028537838,60.0561863629697,13.584744748956));
#79493=CARTESIAN_POINT('Ctrl Pts',(87.2908402888454,60.0607709413421,13.6119579340704));
#79494=CARTESIAN_POINT('Ctrl Pts',(87.3479343506829,60.0653555197145,13.6360696737074));
#79495=CARTESIAN_POINT('Ctrl Pts',(87.4049935176242,60.0699372960725,13.6601666766691));
#79496=CARTESIAN_POINT('Ctrl Pts',(87.4634071992927,60.0745190724304,13.6811657951226));
#79497=CARTESIAN_POINT('Ctrl Pts',(87.5228060535599,60.0791008487884,13.6989242193866));
#79498=CARTESIAN_POINT('Ctrl Pts',(87.5821904212602,60.0836815077139,13.7166783126141));
#79499=CARTESIAN_POINT('Ctrl Pts',(87.6425589970882,60.0882621666393,13.7311931348913));
#79500=CARTESIAN_POINT('Ctrl Pts',(87.7035267489651,60.0928428255648,13.7423755651697));
#79501=CARTESIAN_POINT('Ctrl Pts',(87.7666970587904,60.0975889681503,13.7539619787004));
#79502=CARTESIAN_POINT('Ctrl Pts',(87.8305101056303,60.1023351107358,13.7619704463725));
#79503=CARTESIAN_POINT('Ctrl Pts',(87.8945280086709,60.1070812533213,13.7663555836459));
#79504=CARTESIAN_POINT('Ctrl Pts',(87.9563920654883,60.1116677146177,13.7705931854502));
#79505=CARTESIAN_POINT('Ctrl Pts',(88.0184468831037,60.1162541759141,13.7714474754972));
#79506=CARTESIAN_POINT('Ctrl Pts',(88.080296521582,60.1208406372105,13.768930658511));
#79507=CARTESIAN_POINT('Ctrl Pts',(88.1453761764165,60.1256666204406,13.7662824040543));
#79508=CARTESIAN_POINT('Ctrl Pts',(88.2102279920796,60.1304926036707,13.759901336269));
#79509=CARTESIAN_POINT('Ctrl Pts',(88.2743991136333,60.1353185869007,13.7498633384385));
#79510=CARTESIAN_POINT('Ctrl Pts',(88.3385702351869,60.1401445701308,13.739825340608));
#79511=CARTESIAN_POINT('Ctrl Pts',(88.4020600455273,60.1449705533608,13.7261306249994));
#79512=CARTESIAN_POINT('Ctrl Pts',(88.4644336759938,60.1497965365909,13.7089159251388));
#79513=CARTESIAN_POINT('Ctrl Pts',(88.5238506925549,60.154393760183,13.6925172307056));
#79514=CARTESIAN_POINT('Ctrl Pts',(88.5824989273805,60.158990983775,13.6728574407152));
#79515=CARTESIAN_POINT('Ctrl Pts',(88.6399948155849,60.1635882073671,13.6500266277962));
#79516=CARTESIAN_POINT('Ctrl Pts',(88.698475189868,60.1682641479382,13.6268048892268));
#79517=CARTESIAN_POINT('Ctrl Pts',(88.7557628470377,60.1729400885094,13.6003025620697));
#79518=CARTESIAN_POINT('Ctrl Pts',(88.8114676074206,60.1776160290805,13.5706682176049));
#79519=CARTESIAN_POINT('Ctrl Pts',(88.8660839644523,60.1822006074529,13.5416128922331));
#79520=CARTESIAN_POINT('Ctrl Pts',(88.9191782532287,60.1867851858253,13.50954709097));
#79521=CARTESIAN_POINT('Ctrl Pts',(88.9704027846842,60.1913697641977,13.4746593386409));
#79522=CARTESIAN_POINT('Ctrl Pts',(89.0215960085983,60.1959515405557,13.4397929090983));
#79523=CARTESIAN_POINT('Ctrl Pts',(89.0709213212645,60.2005333169136,13.4021082343319));
#79524=CARTESIAN_POINT('Ctrl Pts',(89.1180584145327,60.2051150932716,13.3618381466882));
#79525=CARTESIAN_POINT('Ctrl Pts',(89.1651840117092,60.209695752197,13.3215778803675));
#79526=CARTESIAN_POINT('Ctrl Pts',(89.2101220620533,60.2142764111225,13.2787337834054));
#79527=CARTESIAN_POINT('Ctrl Pts',(89.2525854916771,60.2188570700479,13.2335788206614));
#79528=CARTESIAN_POINT('Ctrl Pts',(89.2965829808909,60.2236032126334,13.1867925623708));
#79529=CARTESIAN_POINT('Ctrl Pts',(89.3379231818021,60.2283493552189,13.1375256536989));
#79530=CARTESIAN_POINT('Ctrl Pts',(89.376330459886,60.2330954978045,13.0861213510693));
#79531=CARTESIAN_POINT('Ctrl Pts',(89.4134455467713,60.2376819591008,13.0364465171951));
#79532=CARTESIAN_POINT('Ctrl Pts',(89.4478217102424,60.2422684203972,12.9847763170237));
#79533=CARTESIAN_POINT('Ctrl Pts',(89.4792544464154,60.2468548816936,12.9314500079042));
#79534=CARTESIAN_POINT('Ctrl Pts',(89.5123287160632,60.2516808649237,12.8753388021398));
#79535=CARTESIAN_POINT('Ctrl Pts',(89.5421433905218,60.2565068481538,12.8173943355545));
#79536=CARTESIAN_POINT('Ctrl Pts',(89.5685165929858,60.2613328313839,12.7580382201685));
#79537=CARTESIAN_POINT('Ctrl Pts',(89.5948897954498,60.2661588146139,12.6986821047824));
#79538=CARTESIAN_POINT('Ctrl Pts',(89.617821369533,60.270984797844,12.6379149741709));
#79539=CARTESIAN_POINT('Ctrl Pts',(89.6371903157418,60.2758107810741,12.5761763347977));
#79540=CARTESIAN_POINT('Ctrl Pts',(89.6556411416605,60.2804080046662,12.5173642096953));
#79541=CARTESIAN_POINT('Ctrl Pts',(89.6709352658989,60.2850052282582,12.4574291402083));
#79542=CARTESIAN_POINT('Ctrl Pts',(89.6829403152594,60.2896024518503,12.3967422225998));
#79543=CARTESIAN_POINT('Ctrl Pts',(89.6951509237362,60.2942783924214,12.3350161798051));
#79544=CARTESIAN_POINT('Ctrl Pts',(89.7039585120003,60.2989543329926,12.2725127767161));
#79545=CARTESIAN_POINT('Ctrl Pts',(89.7092762649574,60.3036302735637,12.2096403964156));
#79546=CARTESIAN_POINT('Ctrl Pts',(89.7144901154814,60.3082148519361,12.1479964660525));
#79547=CARTESIAN_POINT('Ctrl Pts',(89.7163492335356,60.3127994303085,12.0859983790548));
#79548=CARTESIAN_POINT('Ctrl Pts',(89.714823416698,60.3173840086809,12.0240404919991));
#79549=CARTESIAN_POINT('Ctrl Pts',(89.7132985324129,60.3219657850389,11.9621204725249));
#79550=CARTESIAN_POINT('Ctrl Pts',(89.7083928279001,60.3265475613969,11.900241112112));
#79551=CARTESIAN_POINT('Ctrl Pts',(89.7001281757988,60.3311293377548,11.8387977963955));
#79552=CARTESIAN_POINT('Ctrl Pts',(89.6918655393329,60.3357099966803,11.7773694658623));
#79553=CARTESIAN_POINT('Ctrl Pts',(89.680245649347,60.3402906556057,11.7163774731916));
#79554=CARTESIAN_POINT('Ctrl Pts',(89.6653421208768,60.3448713145311,11.6562110510363));
#79555=CARTESIAN_POINT('Ctrl Pts',(89.6499001785061,60.3496174571167,11.5938710202554));
#79556=CARTESIAN_POINT('Ctrl Pts',(89.630932879344,60.3543635997022,11.5324179319364));
#79557=CARTESIAN_POINT('Ctrl Pts',(89.6085790965537,60.3591097422877,11.4722695343384));
#79558=CARTESIAN_POINT('Ctrl Pts',(89.5869773941715,60.3636962035841,11.4141447956368));
#79559=CARTESIAN_POINT('Ctrl Pts',(89.5622137536472,60.3682826648805,11.3572388002696));
#79560=CARTESIAN_POINT('Ctrl Pts',(89.5344622696087,60.3728691261769,11.3019073690456));
#79561=CARTESIAN_POINT('Ctrl Pts',(89.5052615006662,60.3776951094069,11.2436863263013));
#79562=CARTESIAN_POINT('Ctrl Pts',(89.4727525700976,60.382521092637,11.1872093800826));
#79563=CARTESIAN_POINT('Ctrl Pts',(89.4371910333326,60.3873470758671,11.1328580107821));
#79564=CARTESIAN_POINT('Ctrl Pts',(89.4016294965676,60.3921730590971,11.0785066414816));
#79565=CARTESIAN_POINT('Ctrl Pts',(89.3630158010626,60.3969990423272,11.0262813241333));
#79566=CARTESIAN_POINT('Ctrl Pts',(89.3216535555268,60.4018250255573,10.9765221007359));
#79567=CARTESIAN_POINT('Ctrl Pts',(89.2822519492771,60.4064222491494,10.929121547352));
#79568=CARTESIAN_POINT('Ctrl Pts',(89.2401947425895,60.4110194727414,10.883763922235));
#79569=CARTESIAN_POINT('Ctrl Pts',(89.1957219022323,60.4156166963335,10.8407617170644));
#79570=CARTESIAN_POINT('Ctrl Pts',(89.1504875658173,60.4202926369046,10.7970231971127));
#79571=CARTESIAN_POINT('Ctrl Pts',(89.1027543586077,60.4249685774758,10.7557219872247));
#79572=CARTESIAN_POINT('Ctrl Pts',(89.0528182834772,60.4296445180469,10.717152529078));
#79573=CARTESIAN_POINT('Ctrl Pts',(89.0038578985954,60.4342290964193,10.6793366712916));
#79574=CARTESIAN_POINT('Ctrl Pts',(88.9527803764849,60.4388136747917,10.6441471011552));
#79575=CARTESIAN_POINT('Ctrl Pts',(88.8999006426985,60.4433982531641,10.6118230908826));
#79576=CARTESIAN_POINT('Ctrl Pts',(88.8470532280844,60.4479800295221,10.5795188364821));
#79577=CARTESIAN_POINT('Ctrl Pts',(88.7924062192987,60.45256180588,10.5500769341547));
#79578=CARTESIAN_POINT('Ctrl Pts',(88.7363036518768,60.457143582238,10.5236934649123));
#79579=CARTESIAN_POINT('Ctrl Pts',(88.6802147671027,60.4617242411635,10.4973164302368));
#79580=CARTESIAN_POINT('Ctrl Pts',(88.6226714888481,60.4663049000889,10.4739965644364));
#79581=CARTESIAN_POINT('Ctrl Pts',(88.5640407484093,60.4708855590144,10.4538831412708));
#79582=CARTESIAN_POINT('Ctrl Pts',(88.5032918783133,60.4756317015999,10.4330430883919));
#79583=CARTESIAN_POINT('Ctrl Pts',(88.4413759981938,60.4803778441854,10.4156458388827));
#79584=CARTESIAN_POINT('Ctrl Pts',(88.3787193918396,60.4851239867709,10.4018013085977));
#79585=CARTESIAN_POINT('Ctrl Pts',(88.3181708316499,60.4897104480673,10.3884225697219));
#79586=CARTESIAN_POINT('Ctrl Pts',(88.2569311322003,60.4942969093637,10.3783612868975));
#79587=CARTESIAN_POINT('Ctrl Pts',(88.195393654796,60.4988833706601,10.3716641963085));
#79588=CARTESIAN_POINT('Ctrl Pts',(88.1306424632386,60.5037093538902,10.3646173589356));
#79589=CARTESIAN_POINT('Ctrl Pts',(88.0655621813225,60.5085353371202,10.3612957739798));
#79590=CARTESIAN_POINT('Ctrl Pts',(88.0006119117509,60.5133613203503,10.3616916584073));
#79591=CARTESIAN_POINT('Ctrl Pts',(87.9356616421792,60.5181873035804,10.3620875428348));
#79592=CARTESIAN_POINT('Ctrl Pts',(87.8708420267378,60.5230132868104,10.3662007783859));
#79593=CARTESIAN_POINT('Ctrl Pts',(87.8066034188971,60.5278392700405,10.3739607353157));
#79594=CARTESIAN_POINT('Ctrl Pts',(87.7454098279936,60.5324364936326,10.3813528573705));
#79595=CARTESIAN_POINT('Ctrl Pts',(87.6844921499851,60.5370337172246,10.3920840873396));
#79596=CARTESIAN_POINT('Ctrl Pts',(87.6242430734256,60.5416309408167,10.4061223191612));
#79597=CARTESIAN_POINT('Ctrl Pts',(87.5629623687099,60.5463068813878,10.4204009237161));
#79598=CARTESIAN_POINT('Ctrl Pts',(87.5023739153509,60.550982821959,10.4381008764927));
#79599=CARTESIAN_POINT('Ctrl Pts',(87.442885631628,60.5556587625301,10.4591332040118));
#79600=CARTESIAN_POINT('Ctrl Pts',(87.3845596767063,60.5602433409025,10.4797545854));
#79601=CARTESIAN_POINT('Ctrl Pts',(87.3272917890264,60.5648279192749,10.5035791137684));
#79602=CARTESIAN_POINT('Ctrl Pts',(87.2714538014706,60.5694124976473,10.530471994446));
#79603=CARTESIAN_POINT('Ctrl Pts',(87.2156499411203,60.5739942740053,10.5573484386633));
#79604=CARTESIAN_POINT('Ctrl Pts',(87.1612747056924,60.5785760503632,10.587289296267));
#79605=CARTESIAN_POINT('Ctrl Pts',(87.1086794314454,60.5831578267212,10.6201118898188));
#79606=CARTESIAN_POINT('Ctrl Pts',(87.0560969844655,60.5877384856466,10.6529264783895));
#79607=CARTESIAN_POINT('Ctrl Pts',(87.0052940685559,60.5923191445721,10.6886211383305));
#79608=CARTESIAN_POINT('Ctrl Pts',(86.9565951148436,60.5968998034975,10.7269685687938));
#79609=CARTESIAN_POINT('Ctrl Pts',(86.9061368332193,60.601645946083,10.7667013617673));
#79610=CARTESIAN_POINT('Ctrl Pts',(86.8579379388001,60.6063920886686,10.8092819568575));
#79611=CARTESIAN_POINT('Ctrl Pts',(86.812321990022,60.6111382312541,10.8544118422521));
#79612=CARTESIAN_POINT('Ctrl Pts',(86.7682407641002,60.6157246925505,10.8980233581185));
#79613=CARTESIAN_POINT('Ctrl Pts',(86.7265717301612,60.6203111538469,10.9440148987681));
#79614=CARTESIAN_POINT('Ctrl Pts',(86.6875675109478,60.6248976151433,10.9920813426888));
#79615=CARTESIAN_POINT('Ctrl Pts',(86.6465263474752,60.6297235983733,11.0426579936841));
#79616=CARTESIAN_POINT('Ctrl Pts',(86.6084363492216,60.6345495816034,11.09553169276));
#79617=CARTESIAN_POINT('Ctrl Pts',(86.5735399942341,60.6393755648335,11.1503125165082));
#79618=CARTESIAN_POINT('Ctrl Pts',(86.5386436392466,60.6442015480636,11.2050933402564));
#79619=CARTESIAN_POINT('Ctrl Pts',(86.5069411762764,60.6490275312937,11.261780685355));
#79620=CARTESIAN_POINT('Ctrl Pts',(86.4786175389448,60.6538535145238,11.3199578908329));
#79621=CARTESIAN_POINT('Ctrl Pts',(86.4496369214494,60.6587914387174,11.3794845441073));
#79622=CARTESIAN_POINT('Ctrl Pts',(86.4240874916357,60.663729362911,11.4407864007869));
#79623=CARTESIAN_POINT('Ctrl Pts',(86.4021724737663,60.6686672871046,11.503462155555));
#79624=CARTESIAN_POINT('Ctrl Pts',(86.3803110941619,60.6735931254451,11.5659845078132));
#79625=CARTESIAN_POINT('Ctrl Pts',(86.3620665597285,60.6785189637856,11.6298737052834));
#79626=CARTESIAN_POINT('Ctrl Pts',(86.3475949281985,60.6834448021261,11.6947071200453));
#79627=CARTESIAN_POINT('Ctrl Pts',(86.3331772318557,60.6883522820657,11.7592989032843));
#79628=CARTESIAN_POINT('Ctrl Pts',(86.3225045213705,60.6932597620053,11.8248275188846));
#79629=CARTESIAN_POINT('Ctrl Pts',(86.3156830782276,60.6981672419449,11.8908561438356));
#79630=CARTESIAN_POINT('Ctrl Pts',(86.3096955324728,60.7024747997539,11.9488130020448));
#79631=CARTESIAN_POINT('Ctrl Pts',(86.3066745521873,60.7067823575629,12.007154655696));
#79632=CARTESIAN_POINT('Ctrl Pts',(86.3066600524911,60.7110899153719,12.0655770041428));
#79633=CARTESIAN_POINT('',(86.3066607115161,61.5048399155016,12.0675573471538));
#79634=CARTESIAN_POINT('Ctrl Pts',(86.3066600524909,60.7110899154298,12.0655770049287));
#79635=CARTESIAN_POINT('Ctrl Pts',(86.3066441759981,60.7158064996465,12.1295468780701));
#79636=CARTESIAN_POINT('Ctrl Pts',(86.3102341532229,60.7205230838632,12.1934773303318));
#79637=CARTESIAN_POINT('Ctrl Pts',(86.3173906533801,60.7252396680799,12.256950822574));
#79638=CARTESIAN_POINT('Ctrl Pts',(86.3245616248092,60.729965789776,12.3205526655672));
#79639=CARTESIAN_POINT('Ctrl Pts',(86.3353134694598,60.7346919114722,12.383695239678));
#79640=CARTESIAN_POINT('Ctrl Pts',(86.3495552008937,60.7394180331683,12.4459684396404));
#79641=CARTESIAN_POINT('Ctrl Pts',(86.3638114807984,60.7441489827776,12.5083052540469));
#79642=CARTESIAN_POINT('Ctrl Pts',(86.3815646199732,60.7488799323869,12.5697704781106));
#79643=CARTESIAN_POINT('Ctrl Pts',(86.4026737719427,60.7536108819962,12.6299694847622));
#79644=CARTESIAN_POINT('Ctrl Pts',(86.4238362968947,60.7583537934736,12.6903207003012));
#79645=CARTESIAN_POINT('Ctrl Pts',(86.4483716155272,60.763096704951,12.7493988686388));
#79646=CARTESIAN_POINT('Ctrl Pts',(86.4760907903572,60.7678396164284,12.8068296388197));
#79647=CARTESIAN_POINT('Ctrl Pts',(86.4995229647787,60.7718489972879,12.8553782638165));
#79648=CARTESIAN_POINT('Ctrl Pts',(86.5252294344248,60.7758583781474,12.9027499362615));
#79649=CARTESIAN_POINT('Ctrl Pts',(86.5530718782772,60.7798677590069,12.9487346302768));
#79650=CARTESIAN_POINT('Ctrl Pts',(86.5849964931304,60.784464982599,13.0014614545943));
#79651=CARTESIAN_POINT('Ctrl Pts',(86.6198506742157,60.7890622061911,13.0525624218208));
#79652=CARTESIAN_POINT('Ctrl Pts',(86.6574435278868,60.7936594297831,13.1016928658635));
#79653=CARTESIAN_POINT('Ctrl Pts',(86.6956800735201,60.7983353703543,13.1516645568146));
#79654=CARTESIAN_POINT('Ctrl Pts',(86.7367497681312,60.8030113109254,13.1995971051849));
#79655=CARTESIAN_POINT('Ctrl Pts',(86.7804036226425,60.8076872514965,13.2451553721349));
#79656=CARTESIAN_POINT('Ctrl Pts',(86.8232045338646,60.8122718298689,13.28982348589));
#79657=CARTESIAN_POINT('Ctrl Pts',(86.8684891614438,60.8168564082413,13.3322088797932));
#79658=CARTESIAN_POINT('Ctrl Pts',(86.9159816096461,60.8214409866138,13.3720281621721));
#79659=CARTESIAN_POINT('Ctrl Pts',(86.9634450312912,60.8260227629717,13.4118231076992));
#79660=CARTESIAN_POINT('Ctrl Pts',(87.0131132086595,60.8306045393297,13.4490547251605));
#79661=CARTESIAN_POINT('Ctrl Pts',(87.0646750440703,60.8351863156876,13.4834780116054));
#79662=CARTESIAN_POINT('Ctrl Pts',(87.1162243042556,60.8397669746131,13.5178929026821));
#79663=CARTESIAN_POINT('Ctrl Pts',(87.1696658824878,60.8443476335385,13.5495005398805));
#79664=CARTESIAN_POINT('Ctrl Pts',(87.2246590873795,60.848928292464,13.5780988078625));
#79665=CARTESIAN_POINT('Ctrl Pts',(87.2816390101152,60.8536744350495,13.6077302342032));
#79666=CARTESIAN_POINT('Ctrl Pts',(87.3402843297241,60.858420577635,13.6341303665783));
#79667=CARTESIAN_POINT('Ctrl Pts',(87.4001898151027,60.8631667202205,13.6571271959293));
#79668=CARTESIAN_POINT('Ctrl Pts',(87.4580798142295,60.8677531815169,13.6793503099335));
#79669=CARTESIAN_POINT('Ctrl Pts',(87.5171460004979,60.8723396428133,13.6983954101024));
#79670=CARTESIAN_POINT('Ctrl Pts',(87.5770063166188,60.8769261041097,13.7141578560275));
#79671=CARTESIAN_POINT('Ctrl Pts',(87.6399927593417,60.8817520873398,13.7307434750448));
#79672=CARTESIAN_POINT('Ctrl Pts',(87.7038579222001,60.8865780705699,13.743694034646));
#79673=CARTESIAN_POINT('Ctrl Pts',(87.7681466383619,60.8914040538,13.7529490449747));
#79674=CARTESIAN_POINT('Ctrl Pts',(87.8324353545238,60.8962300370301,13.7622040553035));
#79675=CARTESIAN_POINT('Ctrl Pts',(87.8971469717572,60.9010560202601,13.767763537989));
#79676=CARTESIAN_POINT('Ctrl Pts',(87.9618256413461,60.9058820034902,13.7696304523138));
#79677=CARTESIAN_POINT('Ctrl Pts',(88.0234384343382,60.9104792270823,13.7714088717921));
#79678=CARTESIAN_POINT('Ctrl Pts',(88.0852743034678,60.9150764506744,13.7698442377821));
#79679=CARTESIAN_POINT('Ctrl Pts',(88.1469401469759,60.9196736742664,13.7649099776151));
#79680=CARTESIAN_POINT('Ctrl Pts',(88.2096618775458,60.9243496148376,13.7598912294857));
#79681=CARTESIAN_POINT('Ctrl Pts',(88.2722071777644,60.9290255554087,13.751386264506));
#79682=CARTESIAN_POINT('Ctrl Pts',(88.3341594390292,60.9337014959798,13.7394224847797));
#79683=CARTESIAN_POINT('Ctrl Pts',(88.3949012283648,60.9382860743522,13.7276924627764));
#79684=CARTESIAN_POINT('Ctrl Pts',(88.4550724211052,60.9428706527246,13.7126376736548));
#79685=CARTESIAN_POINT('Ctrl Pts',(88.5142852884022,60.947455231097,13.6943361919695));
#79686=CARTESIAN_POINT('Ctrl Pts',(88.5734619658261,60.952037007455,13.6760458958312));
#79687=CARTESIAN_POINT('Ctrl Pts',(88.6316809938509,60.9566187838129,13.6545129917608));
#79688=CARTESIAN_POINT('Ctrl Pts',(88.6885678013138,60.9612005601709,13.6298659502089));
#79689=CARTESIAN_POINT('Ctrl Pts',(88.7454407348635,60.9657812190963,13.6052249197328));
#79690=CARTESIAN_POINT('Ctrl Pts',(88.800981625966,60.9703618780218,13.5774714617722));
#79691=CARTESIAN_POINT('Ctrl Pts',(88.8548358826594,60.9749425369472,13.546782171265));
#79692=CARTESIAN_POINT('Ctrl Pts',(88.9106357108641,60.9796886795328,13.5149841808523));
#79693=CARTESIAN_POINT('Ctrl Pts',(88.9646241698028,60.9844348221183,13.4800344054183));
#79694=CARTESIAN_POINT('Ctrl Pts',(89.0164369541746,60.9891809647038,13.4421799906916));
#79695=CARTESIAN_POINT('Ctrl Pts',(89.0665065266532,60.9937674260002,13.405599166388));
#79696=CARTESIAN_POINT('Ctrl Pts',(89.1145441448782,60.9983538872966,13.3663064515924));
#79697=CARTESIAN_POINT('Ctrl Pts',(89.1602546708257,61.002940348593,13.3245660638939));
#79698=CARTESIAN_POINT('Ctrl Pts',(89.2083523691176,61.007766331823,13.2806458391209));
#79699=CARTESIAN_POINT('Ctrl Pts',(89.253872793751,61.0125923150531,13.2340157312277));
#79700=CARTESIAN_POINT('Ctrl Pts',(89.2965182439904,61.0174182982832,13.1850253258831));
#79701=CARTESIAN_POINT('Ctrl Pts',(89.3391636942298,61.0222442815133,13.1360349205385));
#79702=CARTESIAN_POINT('Ctrl Pts',(89.3789338344764,61.0270702647434,13.084684777428));
#79703=CARTESIAN_POINT('Ctrl Pts',(89.4155838991065,61.0318962479734,13.0313594698198));
#79704=CARTESIAN_POINT('Ctrl Pts',(89.4504966896689,61.0364934715655,12.9805618705524));
#79705=CARTESIAN_POINT('Ctrl Pts',(89.4827219064413,61.0410906951576,12.9277635922223));
#79706=CARTESIAN_POINT('Ctrl Pts',(89.5120240072541,61.0456879187497,12.8732804749569));
#79707=CARTESIAN_POINT('Ctrl Pts',(89.5418278397772,61.0503638593209,12.8178644584508));
#79708=CARTESIAN_POINT('Ctrl Pts',(89.5686071321136,61.055039799892,12.7607057451108));
#79709=CARTESIAN_POINT('Ctrl Pts',(89.5921589373602,61.0597157404631,12.7021691995107));
#79710=CARTESIAN_POINT('Ctrl Pts',(89.6152505689416,61.0643003188355,12.6447763869047));
#79711=CARTESIAN_POINT('Ctrl Pts',(89.6352395023911,61.068884897208,12.5860595950058));
#79712=CARTESIAN_POINT('Ctrl Pts',(89.6519810261474,61.0734694755804,12.52638691057));
#79713=CARTESIAN_POINT('Ctrl Pts',(89.6687123177759,61.0780512519384,12.4667506970397));
#79714=CARTESIAN_POINT('Ctrl Pts',(89.6821999979823,61.0826330282963,12.4061602385123));
#79715=CARTESIAN_POINT('Ctrl Pts',(89.6923488305763,61.0872148046543,12.3449999023654));
#79716=CARTESIAN_POINT('Ctrl Pts',(89.702495188009,61.0917954635798,12.2838544823869));
#79717=CARTESIAN_POINT('Ctrl Pts',(89.7093042310432,61.0963761225052,12.2221399626512));
#79718=CARTESIAN_POINT('Ctrl Pts',(89.7127319905835,61.1009567814307,12.1602500282483));
#79719=CARTESIAN_POINT('Ctrl Pts',(89.716283583442,61.1057029240162,12.0961242205725));
#79720=CARTESIAN_POINT('Ctrl Pts',(89.7162048105288,61.1104490666017,12.0318106582684));
#79721=CARTESIAN_POINT('Ctrl Pts',(89.7125057054581,61.1151952091872,11.9677494534695));
#79722=CARTESIAN_POINT('Ctrl Pts',(89.7089310546901,61.1197816704836,11.9058435517568));
#79723=CARTESIAN_POINT('Ctrl Pts',(89.7019759578328,61.12436813178,11.8441738117826));
#79724=CARTESIAN_POINT('Ctrl Pts',(89.6917023071775,61.1289545930764,11.7831314965425));
#79725=CARTESIAN_POINT('Ctrl Pts',(89.6808921285736,61.1337805763064,11.7189013263454));
#79726=CARTESIAN_POINT('Ctrl Pts',(89.6664074097455,61.1386065595365,11.6553665410596));
#79727=CARTESIAN_POINT('Ctrl Pts',(89.6483803725037,61.1434325427665,11.5929668602099));
#79728=CARTESIAN_POINT('Ctrl Pts',(89.6303533352618,61.1482585259965,11.5305671793602));
#79729=CARTESIAN_POINT('Ctrl Pts',(89.6087842677816,61.1530845092265,11.469303188463));
#79730=CARTESIAN_POINT('Ctrl Pts',(89.5838634976358,61.1579104924566,11.4095891123657));
#79731=CARTESIAN_POINT('Ctrl Pts',(89.5601240134756,61.1625077160486,11.3527055828697));
#79732=CARTESIAN_POINT('Ctrl Pts',(89.5332459797793,61.1671049396407,11.2969947751641));
#79733=CARTESIAN_POINT('Ctrl Pts',(89.5033669827431,61.1717021632328,11.2428258845067));
#79734=CARTESIAN_POINT('Ctrl Pts',(89.4729763759632,61.1763781038039,11.1877294750227));
#79735=CARTESIAN_POINT('Ctrl Pts',(89.4394811858226,61.181054044375,11.1342288091747));
#79736=CARTESIAN_POINT('Ctrl Pts',(89.4030778646249,61.1857299849461,11.0826922890461));
#79737=CARTESIAN_POINT('Ctrl Pts',(89.3673858201031,61.1903145633186,11.0321627299177));
#79738=CARTESIAN_POINT('Ctrl Pts',(89.3288985729185,61.1948991416909,10.9835216884461));
#79739=CARTESIAN_POINT('Ctrl Pts',(89.2878468691759,61.1994837200633,10.9370903896787));
#79740=CARTESIAN_POINT('Ctrl Pts',(89.2468202555196,61.2040654964213,10.8906874689125));
#79741=CARTESIAN_POINT('Ctrl Pts',(89.2032326296158,61.2086472727792,10.8464919934662));
#79742=CARTESIAN_POINT('Ctrl Pts',(89.157355250644,61.2132290491372,10.8047924536696));
#79743=CARTESIAN_POINT('Ctrl Pts',(89.1114890605367,61.2178097080626,10.7631030838196));
#79744=CARTESIAN_POINT('Ctrl Pts',(89.0633346024734,61.2223903669881,10.7239087834454));
#79745=CARTESIAN_POINT('Ctrl Pts',(89.0131987708498,61.2269710259135,10.6874600262208));
#79746=CARTESIAN_POINT('Ctrl Pts',(88.9612517017919,61.231717168499,10.6496944991057));
#79747=CARTESIAN_POINT('Ctrl Pts',(88.9071777901919,61.2364633110846,10.6148770812555));
#79748=CARTESIAN_POINT('Ctrl Pts',(88.8513522257904,61.2412094536701,10.5832380594954));
#79749=CARTESIAN_POINT('Ctrl Pts',(88.7974048810022,61.2457959149665,10.5526635147692));
#79750=CARTESIAN_POINT('Ctrl Pts',(88.7418223909129,61.2503823762629,10.5250570482046));
#79751=CARTESIAN_POINT('Ctrl Pts',(88.6849670341506,61.2549688375592,10.5005788833422));
#79752=CARTESIAN_POINT('Ctrl Pts',(88.6251424808521,61.2597948207893,10.474822378382));
#79753=CARTESIAN_POINT('Ctrl Pts',(88.563909069067,61.2646208040195,10.4525301083734));
#79754=CARTESIAN_POINT('Ctrl Pts',(88.5017079334239,61.2694467872496,10.4338294943007));
#79755=CARTESIAN_POINT('Ctrl Pts',(88.4395067977809,61.2742727704797,10.4151288802279));
#79756=CARTESIAN_POINT('Ctrl Pts',(88.3763385864904,61.2790987537098,10.400019997572));
#79757=CARTESIAN_POINT('Ctrl Pts',(88.3126545320565,61.2839247369399,10.3885676231544));
#79758=CARTESIAN_POINT('Ctrl Pts',(88.2519892078063,61.2885219605319,10.377658110347));
#79759=CARTESIAN_POINT('Ctrl Pts',(88.1906067665736,61.293119184124,10.3700214422995));
#79760=CARTESIAN_POINT('Ctrl Pts',(88.1288920036934,61.297716407716,10.3657422809865));
#79761=CARTESIAN_POINT('Ctrl Pts',(88.0661205161181,61.3023923482871,10.3613898487861));
#79762=CARTESIAN_POINT('Ctrl Pts',(88.00300572438,61.3070682888583,10.3605111721684));
#79763=CARTESIAN_POINT('Ctrl Pts',(87.9399636863555,61.3117442294294,10.3631410282282));
#79764=CARTESIAN_POINT('Ctrl Pts',(87.8781534131749,61.3163288078018,10.3657195000951));
#79765=CARTESIAN_POINT('Ctrl Pts',(87.8164136091926,61.3209133861742,10.371670610537));
#79766=CARTESIAN_POINT('Ctrl Pts',(87.7551392987735,61.3254979645465,10.3809747369348));
#79767=CARTESIAN_POINT('Ctrl Pts',(87.6939024381457,61.3300797409045,10.3902731768126));
#79768=CARTESIAN_POINT('Ctrl Pts',(87.6331310091896,61.3346615172624,10.4029204929095));
#79769=CARTESIAN_POINT('Ctrl Pts',(87.5732145093823,61.3392432936203,10.4188452714439));
#79770=CARTESIAN_POINT('Ctrl Pts',(87.5133126223886,61.3438239525457,10.434766166143));
#79771=CARTESIAN_POINT('Ctrl Pts',(87.4542657423754,61.3484046114711,10.4539628057942));
#79772=CARTESIAN_POINT('Ctrl Pts',(87.3964507567196,61.3529852703965,10.476313218529));
#79773=CARTESIAN_POINT('Ctrl Pts',(87.3365471118574,61.3577314129821,10.4994710758182));
#79774=CARTESIAN_POINT('Ctrl Pts',(87.2779666392387,61.3624775555676,10.5260147893731));
#79775=CARTESIAN_POINT('Ctrl Pts',(87.221106310152,61.3672236981532,10.5557540616382));
#79776=CARTESIAN_POINT('Ctrl Pts',(87.1661590147529,61.3718101594495,10.5844927728689));
#79777=CARTESIAN_POINT('Ctrl Pts',(87.1128183638655,61.3763966207459,10.6162150862082));
#79778=CARTESIAN_POINT('Ctrl Pts',(87.0614154641582,61.3809830820422,10.6507035487609));
#79779=CARTESIAN_POINT('Ctrl Pts',(87.007328115342,61.3858090652724,10.6869931260968));
#79780=CARTESIAN_POINT('Ctrl Pts',(86.9553869805493,61.3906350485025,10.7263453120269));
#79781=CARTESIAN_POINT('Ctrl Pts',(86.9059383797233,61.3954610317326,10.7684586129947));
#79782=CARTESIAN_POINT('Ctrl Pts',(86.8564897788974,61.4002870149628,10.8105719139625));
#79783=CARTESIAN_POINT('Ctrl Pts',(86.8095341270401,61.4051129981929,10.8554458263333));
#79784=CARTESIAN_POINT('Ctrl Pts',(86.7653705924827,61.4099389814231,10.9027363949955));
#79785=CARTESIAN_POINT('Ctrl Pts',(86.7238082338614,61.4144807203876,10.9472416093955));
#79786=CARTESIAN_POINT('Ctrl Pts',(86.684538764033,61.4190224593521,10.9940794473683));
#79787=CARTESIAN_POINT('Ctrl Pts',(86.6478391663862,61.4235641983167,11.0429812429377));
#79788=CARTESIAN_POINT('Ctrl Pts',(86.6111914874166,61.4280995121132,11.0918138574614));
#79789=CARTESIAN_POINT('Ctrl Pts',(86.5771067908207,61.4326348259098,11.1427042334525));
#79790=CARTESIAN_POINT('Ctrl Pts',(86.5458242256299,61.4371701397064,11.1953480685148));
#79791=CARTESIAN_POINT('Ctrl Pts',(86.5145737630342,61.441700799302,11.2479378797553));
#79792=CARTESIAN_POINT('Ctrl Pts',(86.4861199992106,61.4462314588977,11.302277137944));
#79793=CARTESIAN_POINT('Ctrl Pts',(86.4606595426181,61.4507621184934,11.3580315672256));
#79794=CARTESIAN_POINT('Ctrl Pts',(86.4352075425464,61.4552912732607,11.4137674780457));
#79795=CARTESIAN_POINT('Ctrl Pts',(86.4127471112947,61.459820428028,11.4709171613093));
#79796=CARTESIAN_POINT('Ctrl Pts',(86.3934286111655,61.4643495827954,11.5291223252694));
#79797=CARTESIAN_POINT('Ctrl Pts',(86.3741152572093,61.4688775310604,11.5873119842038));
#79798=CARTESIAN_POINT('Ctrl Pts',(86.3579423331523,61.4734054793255,11.6465560683486));
#79799=CARTESIAN_POINT('Ctrl Pts',(86.3450108760953,61.4779334275906,11.7064793821891));
#79800=CARTESIAN_POINT('Ctrl Pts',(86.3320682999305,61.4824652692101,11.7664542210651));
#79801=CARTESIAN_POINT('Ctrl Pts',(86.3223728674377,61.4869971108295,11.8271089440921));
#79802=CARTESIAN_POINT('Ctrl Pts',(86.3159745177665,61.491528952449,11.8880577335792));
#79803=CARTESIAN_POINT('Ctrl Pts',(86.3097100891034,61.4959659401092,11.9477308310904));
#79804=CARTESIAN_POINT('Ctrl Pts',(86.3066060032365,61.5004029277695,12.0076853217731));
#79805=CARTESIAN_POINT('Ctrl Pts',(86.3066607115152,61.5048399154298,12.0675573461848));
#79806=CARTESIAN_POINT('',(86.3066600835977,62.2985899154715,12.0654661855251));
#79807=CARTESIAN_POINT('Ctrl Pts',(86.3066607115161,61.5048399155016,12.0675573471538));
#79808=CARTESIAN_POINT('Ctrl Pts',(86.3067344748707,61.5108223170385,12.1482829471039));
#79809=CARTESIAN_POINT('Ctrl Pts',(86.312547324273,61.5168047185754,12.2287530864269));
#79810=CARTESIAN_POINT('Ctrl Pts',(86.3239687341642,61.5227871201123,12.3082815380758));
#79811=CARTESIAN_POINT('Ctrl Pts',(86.3323475036833,61.5271758220436,12.3666237719092));
#79812=CARTESIAN_POINT('Ctrl Pts',(86.343743627015,61.531564523975,12.4244598713876));
#79813=CARTESIAN_POINT('Ctrl Pts',(86.3580897682031,61.5359532259064,12.481526895906));
#79814=CARTESIAN_POINT('Ctrl Pts',(86.3731175417349,61.5405504494983,12.541305362418));
#79815=CARTESIAN_POINT('Ctrl Pts',(86.3914232300308,61.5451476730902,12.6003902552955));
#79816=CARTESIAN_POINT('Ctrl Pts',(86.4129256062274,61.5497448966821,12.6583960394604));
#79817=CARTESIAN_POINT('Ctrl Pts',(86.4347961616233,61.5544208372532,12.7173950405132));
#79818=CARTESIAN_POINT('Ctrl Pts',(86.4599738701113,61.5590967778244,12.7752770930347));
#79819=CARTESIAN_POINT('Ctrl Pts',(86.4883191737899,61.5637727183955,12.8316487034484));
#79820=CARTESIAN_POINT('Ctrl Pts',(86.5161106446655,61.5683572967677,12.8869188810688));
#79821=CARTESIAN_POINT('Ctrl Pts',(86.546946802419,61.57294187514,12.9407366335863));
#79822=CARTESIAN_POINT('Ctrl Pts',(86.5806471688951,61.5775264535122,12.9927500278663));
#79823=CARTESIAN_POINT('Ctrl Pts',(86.6143269382942,61.58210822987,13.0447316324656));
#79824=CARTESIAN_POINT('Ctrl Pts',(86.6508671690947,61.5866900062277,13.0949106391781));
#79825=CARTESIAN_POINT('Ctrl Pts',(86.6900424575833,61.5912717825855,13.1429614694744));
#79826=CARTESIAN_POINT('Ctrl Pts',(86.7292081917555,61.5958524415108,13.1910005808312));
#79827=CARTESIAN_POINT('Ctrl Pts',(86.7710073863296,61.600433100436,13.2369121517682));
#79828=CARTESIAN_POINT('Ctrl Pts',(86.8151737513127,61.6050137593613,13.280402906185));
#79829=CARTESIAN_POINT('Ctrl Pts',(86.8609356971641,61.609759901947,13.3254648339533));
#79830=CARTESIAN_POINT('Ctrl Pts',(86.9092387544391,61.6145060445327,13.3679272309615));
#79831=CARTESIAN_POINT('Ctrl Pts',(86.9597460970713,61.6192521871183,13.4075066407503));
#79832=CARTESIAN_POINT('Ctrl Pts',(87.0085541486572,61.6238386484145,13.4457544236278));
#79833=CARTESIAN_POINT('Ctrl Pts',(87.0594200335514,61.6284251097108,13.4813099007641));
#79834=CARTESIAN_POINT('Ctrl Pts',(87.1120092877091,61.633011571007,13.5139608195026));
#79835=CARTESIAN_POINT('Ctrl Pts',(87.1673449467881,61.6378375542374,13.5483168897087));
#79836=CARTESIAN_POINT('Ctrl Pts',(87.224588351958,61.6426635374678,13.5794563917294));
#79837=CARTESIAN_POINT('Ctrl Pts',(87.2833221858692,61.6474895206983,13.607187799855));
#79838=CARTESIAN_POINT('Ctrl Pts',(87.3420560197804,61.6523155039287,13.6349192079806));
#79839=CARTESIAN_POINT('Ctrl Pts',(87.402279652622,61.6571414871591,13.6592423512942));
#79840=CARTESIAN_POINT('Ctrl Pts',(87.4635564771644,61.6619674703895,13.6800261537241));
#79841=CARTESIAN_POINT('Ctrl Pts',(87.5219286782211,61.6665646939814,13.6998247693217));
#79842=CARTESIAN_POINT('Ctrl Pts',(87.5814961302972,61.6711619175733,13.7164933458481));
#79843=CARTESIAN_POINT('Ctrl Pts',(87.6418908798614,61.6757591411652,13.7298910099615));
#79844=CARTESIAN_POINT('Ctrl Pts',(87.7033197519028,61.6804350817363,13.7435180785462));
#79845=CARTESIAN_POINT('Ctrl Pts',(87.7656040475827,61.6851110223075,13.7537609063011));
#79846=CARTESIAN_POINT('Ctrl Pts',(87.8283374885835,61.6897869628786,13.7605233083446));
#79847=CARTESIAN_POINT('Ctrl Pts',(87.889845194349,61.6943715412509,13.7671535812663));
#79848=CARTESIAN_POINT('Ctrl Pts',(87.9517841214331,61.6989561196231,13.770438154704));
#79849=CARTESIAN_POINT('Ctrl Pts',(88.0137607122301,61.7035406979953,13.7703377640796));
#79850=CARTESIAN_POINT('Ctrl Pts',(88.0756994240142,61.708122474353,13.7702374348123));
#79851=CARTESIAN_POINT('Ctrl Pts',(88.137675245877,61.7127042507108,13.766756244499));
#79852=CARTESIAN_POINT('Ctrl Pts',(88.1992923937076,61.7172860270686,13.7599069661796));
#79853=CARTESIAN_POINT('Ctrl Pts',(88.2608945139597,61.7218666859938,13.7530593583054));
#79854=CARTESIAN_POINT('Ctrl Pts',(88.3221376281278,61.7264473449191,13.7428453493028));
#79855=CARTESIAN_POINT('Ctrl Pts',(88.3826309133882,61.7310280038443,13.7293295824383));
#79856=CARTESIAN_POINT('Ctrl Pts',(88.4453096157339,61.73577414643,13.7153255367887));
#79857=CARTESIAN_POINT('Ctrl Pts',(88.5071826929468,61.7405202890157,13.6977766673657));
#79858=CARTESIAN_POINT('Ctrl Pts',(88.5678293132122,61.7452664316014,13.6768122024456));
#79859=CARTESIAN_POINT('Ctrl Pts',(88.6264355121557,61.7498528928976,13.6565530751195));
#79860=CARTESIAN_POINT('Ctrl Pts',(88.6838960142886,61.7544393541938,13.6331048151613));
#79861=CARTESIAN_POINT('Ctrl Pts',(88.7398510887762,61.75902581549,13.6066332873172));
#79862=CARTESIAN_POINT('Ctrl Pts',(88.798728343744,61.7638517987205,13.5787793186014));
#79863=CARTESIAN_POINT('Ctrl Pts',(88.8559380508016,61.7686777819509,13.5475779494007));
#79864=CARTESIAN_POINT('Ctrl Pts',(88.9110929527311,61.7735037651814,13.5132758935475));
#79865=CARTESIAN_POINT('Ctrl Pts',(88.9662478546607,61.7783297484119,13.4789738376944));
#79866=CARTESIAN_POINT('Ctrl Pts',(89.0193474662625,61.7831557316423,13.4415715316011));
#79867=CARTESIAN_POINT('Ctrl Pts',(89.0700448525328,61.7879817148728,13.4013646827454));
#79868=CARTESIAN_POINT('Ctrl Pts',(89.1183390983164,61.7925789384661,13.3630637054432));
#79869=CARTESIAN_POINT('Ctrl Pts',(89.1646520346834,61.7971761620594,13.3220608431329));
#79870=CARTESIAN_POINT('Ctrl Pts',(89.2086657334164,61.8017733856526,13.2785888118403));
#79871=CARTESIAN_POINT('Ctrl Pts',(89.25343306644,61.8064493262236,13.2343724210776));
#79872=CARTESIAN_POINT('Ctrl Pts',(89.2958212078182,61.8111252667946,13.1876017627667));
#79873=CARTESIAN_POINT('Ctrl Pts',(89.3355289857389,61.8158012073656,13.1385659893626));
#79874=CARTESIAN_POINT('Ctrl Pts',(89.3744609219252,61.8203857857392,13.0904883153909));
#79875=CARTESIAN_POINT('Ctrl Pts',(89.4108159590514,61.8249703641128,13.0402336599975));
#79876=CARTESIAN_POINT('Ctrl Pts',(89.444347644956,61.8295549424864,12.9881113622004));
#79877=CARTESIAN_POINT('Ctrl Pts',(89.4778588368781,61.8341367188456,12.936020920644));
#79878=CARTESIAN_POINT('Ctrl Pts',(89.5085498243185,61.8387184952047,12.8820655272747));
#79879=CARTESIAN_POINT('Ctrl Pts',(89.5362166653663,61.8433002715639,12.8265846167842));
#79880=CARTESIAN_POINT('Ctrl Pts',(89.5638767588505,61.8478809304905,12.7711172373281));
#79881=CARTESIAN_POINT('Ctrl Pts',(89.5885139430192,61.8524615894172,12.7141255346751));
#79882=CARTESIAN_POINT('Ctrl Pts',(89.6099705442328,61.8570422483438,12.6559729097814));
#79883=CARTESIAN_POINT('Ctrl Pts',(89.6322022996125,61.8617883909282,12.5957194279529));
#79884=CARTESIAN_POINT('Ctrl Pts',(89.6510190034195,61.8665345335125,12.5342200608254));
#79885=CARTESIAN_POINT('Ctrl Pts',(89.666300964409,61.8712806760969,12.4718984513726));
#79886=CARTESIAN_POINT('Ctrl Pts',(89.6810687724518,61.8758671373944,12.4116736172724));
#79887=CARTESIAN_POINT('Ctrl Pts',(89.6925358981186,61.880453598692,12.3506815257231));
#79888=CARTESIAN_POINT('Ctrl Pts',(89.7006465703345,61.8850400599896,12.2893143590479));
#79889=CARTESIAN_POINT('Ctrl Pts',(89.7091808117768,61.8898660432173,12.224742372522));
#79890=CARTESIAN_POINT('Ctrl Pts',(89.7139983552846,61.894692026445,12.1597557024171));
#79891=CARTESIAN_POINT('Ctrl Pts',(89.7150964225358,61.8995180096728,12.0948135089969));
#79892=CARTESIAN_POINT('Ctrl Pts',(89.7161944897869,61.9043439929005,12.0298713155767));
#79893=CARTESIAN_POINT('Ctrl Pts',(89.7135731842489,61.9091699761282,11.9649742431773));
#79894=CARTESIAN_POINT('Ctrl Pts',(89.7072927589168,61.913995959356,11.9005741506097));
#79895=CARTESIAN_POINT('Ctrl Pts',(89.7013100361987,61.9185931829462,11.8392267296193));
#79896=CARTESIAN_POINT('Ctrl Pts',(89.6919827429114,61.9231904065364,11.7780783495286));
#79897=CARTESIAN_POINT('Ctrl Pts',(89.6793339448426,61.9277876301266,11.7175223334476));
#79898=CARTESIAN_POINT('Ctrl Pts',(89.6664685649219,61.932463570698,11.6559294335428));
#79899=CARTESIAN_POINT('Ctrl Pts',(89.6501668201511,61.9371395112694,11.5949499113494));
#79900=CARTESIAN_POINT('Ctrl Pts',(89.6305082784108,61.9418154518407,11.5349936236174));
#79901=CARTESIAN_POINT('Ctrl Pts',(89.6112338407047,61.9464000302113,11.4762088089429));
#79902=CARTESIAN_POINT('Ctrl Pts',(89.5887327679586,61.9509846085819,11.4184081096921));
#79903=CARTESIAN_POINT('Ctrl Pts',(89.5631312670824,61.9555691869525,11.3619663606439));
#79904=CARTESIAN_POINT('Ctrl Pts',(89.5375454133977,61.9601509633086,11.3055591078095));
#79905=CARTESIAN_POINT('Ctrl Pts',(89.5088630987932,61.9647327396647,11.250509620908));
#79906=CARTESIAN_POINT('Ctrl Pts',(89.4772588716991,61.9693145160209,11.1971733448129));
#79907=CARTESIAN_POINT('Ctrl Pts',(89.4456623524432,61.9738951749445,11.143850076705));
#79908=CARTESIAN_POINT('Ctrl Pts',(89.4111455947277,61.9784758338682,11.0922396276918));
#79909=CARTESIAN_POINT('Ctrl Pts',(89.3739283774024,61.9830564927918,11.042671570965));
#79910=CARTESIAN_POINT('Ctrl Pts',(89.3353666283021,61.9878026353791,10.9913127885449));
#79911=CARTESIAN_POINT('Ctrl Pts',(89.2939058648324,61.9925487779664,10.9421472966084));
#79912=CARTESIAN_POINT('Ctrl Pts',(89.2498370780422,61.9972949205537,10.8955054337299));
#79913=CARTESIAN_POINT('Ctrl Pts',(89.2072509607485,62.0018813818483,10.8504328100428));
#79914=CARTESIAN_POINT('Ctrl Pts',(89.1622299681931,62.006467843143,10.807717000004));
#79915=CARTESIAN_POINT('Ctrl Pts',(89.1150733308866,62.0110543044376,10.7676175772813));
#79916=CARTESIAN_POINT('Ctrl Pts',(89.0654539999091,62.0158802876712,10.7254240146836));
#79917=CARTESIAN_POINT('Ctrl Pts',(89.0134703521095,62.0207062709048,10.6861280048536));
#79918=CARTESIAN_POINT('Ctrl Pts',(88.9595066307898,62.0255322541384,10.6499809298785));
#79919=CARTESIAN_POINT('Ctrl Pts',(88.9055429094701,62.030358237372,10.6138338549034));
#79920=CARTESIAN_POINT('Ctrl Pts',(88.8495997120712,62.0351842206056,10.5808359773451));
#79921=CARTESIAN_POINT('Ctrl Pts',(88.7920893358986,62.0400102038393,10.5511817650472));
#79922=CARTESIAN_POINT('Ctrl Pts',(88.7373050473324,62.0446074274305,10.5229332117974));
#79923=CARTESIAN_POINT('Ctrl Pts',(88.6808738862995,62.0492046510219,10.497602462629));
#79924=CARTESIAN_POINT('Ctrl Pts',(88.6231388027267,62.0538018746131,10.475383477454));
#79925=CARTESIAN_POINT('Ctrl Pts',(88.5644151373884,62.0584778151844,10.4527840427805));
#79926=CARTESIAN_POINT('Ctrl Pts',(88.5043429036074,62.0631537557556,10.4334042662798));
#79927=CARTESIAN_POINT('Ctrl Pts',(88.4433095882361,62.0678296963268,10.4173996070851));
#79928=CARTESIAN_POINT('Ctrl Pts',(88.3834687897197,62.0724142746984,10.4017076594928));
#79929=CARTESIAN_POINT('Ctrl Pts',(88.3227046445502,62.07699885307,10.3892602592979));
#79930=CARTESIAN_POINT('Ctrl Pts',(88.2614005138331,62.0815834314415,10.3801546873239));
#79931=CARTESIAN_POINT('Ctrl Pts',(88.2001338511333,62.0861652077986,10.3710546805169));
#79932=CARTESIAN_POINT('Ctrl Pts',(88.1383283597657,62.0907469841557,10.3652925266471));
#79933=CARTESIAN_POINT('Ctrl Pts',(88.0763773313464,62.0953287605128,10.3629143767426));
#79934=CARTESIAN_POINT('Ctrl Pts',(88.0144414119348,62.0999094194374,10.3605368068364));
#79935=CARTESIAN_POINT('Ctrl Pts',(87.9523605343781,62.104490078362,10.3615416220435));
#79936=CARTESIAN_POINT('Ctrl Pts',(87.8905307878683,62.1090707372866,10.3659229415911));
#79937=CARTESIAN_POINT('Ctrl Pts',(87.8264673424463,62.1138168798729,10.3704625433452));
#79938=CARTESIAN_POINT('Ctrl Pts',(87.7626741049852,62.1185630224592,10.3786273064894));
#79939=CARTESIAN_POINT('Ctrl Pts',(87.6995864330993,62.1233091650455,10.3903519385175));
#79940=CARTESIAN_POINT('Ctrl Pts',(87.6386213103571,62.127895626341,10.4016821019128));
#79941=CARTESIAN_POINT('Ctrl Pts',(87.5783155233266,62.1324820876365,10.4163361883729));
#79942=CARTESIAN_POINT('Ctrl Pts',(87.5190494476001,62.137068548932,10.4342036004472));
#79943=CARTESIAN_POINT('Ctrl Pts',(87.456688278664,62.1418945321637,10.4530041147239));
#79944=CARTESIAN_POINT('Ctrl Pts',(87.3954790026308,62.1467205153954,10.4753625706521));
#79945=CARTESIAN_POINT('Ctrl Pts',(87.3358412240052,62.1515464986272,10.5010925066327));
#79946=CARTESIAN_POINT('Ctrl Pts',(87.2762034453795,62.1563724818589,10.5268224426133));
#79947=CARTESIAN_POINT('Ctrl Pts',(87.2181377087964,62.1611984650906,10.5559234991368));
#79948=CARTESIAN_POINT('Ctrl Pts',(87.1620310203565,62.1660244483224,10.5881547756266));
#79949=CARTESIAN_POINT('Ctrl Pts',(87.1085838822509,62.1706216719236,10.6188582360121));
#79950=CARTESIAN_POINT('Ctrl Pts',(87.0566947915483,62.1752188955248,10.6525278821585));
#79951=CARTESIAN_POINT('Ctrl Pts',(87.0067127136938,62.179816119126,10.6889807981863));
#79952=CARTESIAN_POINT('Ctrl Pts',(86.9558748067559,62.184492059696,10.7260578872587));
#79953=CARTESIAN_POINT('Ctrl Pts',(86.907010340959,62.189168000266,10.7660142758366));
#79954=CARTESIAN_POINT('Ctrl Pts',(86.8604600931996,62.193843940836,10.8086087488535));
#79955=CARTESIAN_POINT('Ctrl Pts',(86.8148193806325,62.1984285192176,10.8503709777027));
#79956=CARTESIAN_POINT('Ctrl Pts',(86.7714036589527,62.2030130975992,10.8946687681268));
#79957=CARTESIAN_POINT('Ctrl Pts',(86.7305025904295,62.2075976759808,10.9412328153421));
#79958=CARTESIAN_POINT('Ctrl Pts',(86.6896265199272,62.2121794523479,10.9877684034226));
#79959=CARTESIAN_POINT('Ctrl Pts',(86.6512623903516,62.2167612287151,11.0365671201859));
#79960=CARTESIAN_POINT('Ctrl Pts',(86.6156622950455,62.2213430050822,11.0873235852784));
#79961=CARTESIAN_POINT('Ctrl Pts',(86.5800708821153,62.2259236640168,11.1380676715639));
#79962=CARTESIAN_POINT('Ctrl Pts',(86.5472424574208,62.2305043229514,11.1907681417634));
#79963=CARTESIAN_POINT('Ctrl Pts',(86.5173869186885,62.235084981886,11.245089043236));
#79964=CARTESIAN_POINT('Ctrl Pts',(86.4864528007921,62.2398311244626,11.3013723742943));
#79965=CARTESIAN_POINT('Ctrl Pts',(86.4587108181782,62.2445772670393,11.3593949809681));
#79966=CARTESIAN_POINT('Ctrl Pts',(86.4343422546599,62.2493234096159,11.4187556955376));
#79967=CARTESIAN_POINT('Ctrl Pts',(86.4107935576202,62.2539098709213,11.4761192525813));
#79968=CARTESIAN_POINT('Ctrl Pts',(86.390394981605,62.2584963322267,11.5347317794983));
#79969=CARTESIAN_POINT('Ctrl Pts',(86.3732599266061,62.263082793532,11.5942137267791));
#79970=CARTESIAN_POINT('Ctrl Pts',(86.3552300159058,62.2679087767443,11.6568020404916));
#79971=CARTESIAN_POINT('Ctrl Pts',(86.3408139925677,62.2727347599566,11.7203524477324));
#79972=CARTESIAN_POINT('Ctrl Pts',(86.3300827992189,62.2775607431689,11.7844112933401));
#79973=CARTESIAN_POINT('Ctrl Pts',(86.3193516058702,62.2823867263812,11.8484701389477));
#79974=CARTESIAN_POINT('Ctrl Pts',(86.3123052358886,62.2872127095934,11.9130367703652));
#79975=CARTESIAN_POINT('Ctrl Pts',(86.3089512152314,62.2920386928057,11.977655391406));
#79976=CARTESIAN_POINT('Ctrl Pts',(86.3074335323714,62.2942224336805,12.0068950961104));
#79977=CARTESIAN_POINT('Ctrl Pts',(86.3066692581048,62.2964061745552,12.0361742440832));
#79978=CARTESIAN_POINT('Ctrl Pts',(86.3066600835979,62.2985899154299,12.0654661849667));
#79979=CARTESIAN_POINT('',(86.3066604360558,63.0923399153734,12.0647808303758));
#79980=CARTESIAN_POINT('Ctrl Pts',(86.3066600835977,62.2985899154715,12.0654661855251));
#79981=CARTESIAN_POINT('Ctrl Pts',(86.3066409247245,62.3031501668908,12.126635812625));
#79982=CARTESIAN_POINT('Ctrl Pts',(86.3099191485247,62.3077104183102,12.1879386415856));
#79983=CARTESIAN_POINT('Ctrl Pts',(86.3165116107995,62.3122706697295,12.2489861592162));
#79984=CARTESIAN_POINT('Ctrl Pts',(86.3230929799242,62.3168232476042,12.3099309520609));
#79985=CARTESIAN_POINT('Ctrl Pts',(86.3329774650661,62.3213758254789,12.3706207754731));
#79986=CARTESIAN_POINT('Ctrl Pts',(86.3461299231414,62.3259284033536,12.4306676058837));
#79987=CARTESIAN_POINT('Ctrl Pts',(86.3592701199207,62.3304767371162,12.4906584580154));
#79988=CARTESIAN_POINT('Ctrl Pts',(86.3756721442038,62.3350250708789,12.5500070010703));
#79989=CARTESIAN_POINT('Ctrl Pts',(86.395249330378,62.3395734046416,12.6083325633003));
#79990=CARTESIAN_POINT('Ctrl Pts',(86.4148157428858,62.3441192353771,12.6666260279584));
#79991=CARTESIAN_POINT('Ctrl Pts',(86.4375536893511,62.3486650661125,12.7238971374533));
#79992=CARTESIAN_POINT('Ctrl Pts',(86.4633264760513,62.353210896848,12.7797797271346));
#79993=CARTESIAN_POINT('Ctrl Pts',(86.4890949221422,62.3577559619823,12.8356529051643));
#79994=CARTESIAN_POINT('Ctrl Pts',(86.5178969762771,62.3623010271166,12.8901375576983));
#79995=CARTESIAN_POINT('Ctrl Pts',(86.5495484264447,62.3668460922509,12.9428888947596));
#79996=CARTESIAN_POINT('Ctrl Pts',(86.581228963405,62.3713953341723,12.9956887088164));
#79997=CARTESIAN_POINT('Ctrl Pts',(86.6157638595154,62.3759445760937,13.0467515806393));
#79998=CARTESIAN_POINT('Ctrl Pts',(86.6529243586932,62.3804938180151,13.0957598691389));
#79999=CARTESIAN_POINT('Ctrl Pts',(86.6901020368947,62.3850451630174,13.1447908138076));
#80000=CARTESIAN_POINT('Ctrl Pts',(86.7299073996572,62.3895965080196,13.1917648882435));
#80001=CARTESIAN_POINT('Ctrl Pts',(86.7720720065963,62.3941478530219,13.2363983350811));
#80002=CARTESIAN_POINT('Ctrl Pts',(86.8143143084384,62.3987075845913,13.2811140260466));
#80003=CARTESIAN_POINT('Ctrl Pts',(86.8589241592856,62.4032673161608,13.3234801196338));
#80004=CARTESIAN_POINT('Ctrl Pts',(86.9055977174153,62.4078270477302,13.3632511820217));
#80005=CARTESIAN_POINT('Ctrl Pts',(86.9404885615714,62.4112356775831,13.3929820616739));
#80006=CARTESIAN_POINT('Ctrl Pts',(86.9765319281591,62.414644307436,13.4212635625407));
#80007=CARTESIAN_POINT('Ctrl Pts',(87.0135906687455,62.418052937289,13.4480092118096));
#80008=CARTESIAN_POINT('Ctrl Pts',(87.0635718411982,62.4226501608808,13.4840811043595));
#80009=CARTESIAN_POINT('Ctrl Pts',(87.1156149772854,62.4272473844726,13.5175121494062));
#80010=CARTESIAN_POINT('Ctrl Pts',(87.1694097378665,62.4318446080644,13.5480596028102));
#80011=CARTESIAN_POINT('Ctrl Pts',(87.2241256111526,62.4365205486355,13.5791301117522));
#80012=CARTESIAN_POINT('Ctrl Pts',(87.280653284269,62.4411964892067,13.6072169623774));
#80013=CARTESIAN_POINT('Ctrl Pts',(87.3386326569108,62.4458724297779,13.6321088696343));
#80014=CARTESIAN_POINT('Ctrl Pts',(87.3954791830314,62.4504570081495,13.6565144192564));
#80015=CARTESIAN_POINT('Ctrl Pts',(87.4537206998271,62.4550415865212,13.677848542848));
#80016=CARTESIAN_POINT('Ctrl Pts',(87.5129925462586,62.4596261648929,13.6959581011848));
#80017=CARTESIAN_POINT('Ctrl Pts',(87.5722281667676,62.4642079412499,13.7140565912742));
#80018=CARTESIAN_POINT('Ctrl Pts',(87.6324923824485,62.468789717607,13.7289342754822));
#80019=CARTESIAN_POINT('Ctrl Pts',(87.6934031180205,62.473371493964,13.7404871024158));
#80020=CARTESIAN_POINT('Ctrl Pts',(87.7542989982961,62.4779521528884,13.7520371117727));
#80021=CARTESIAN_POINT('Ctrl Pts',(87.8158405855425,62.4825328118127,13.760263778773));
#80022=CARTESIAN_POINT('Ctrl Pts',(87.8776353100951,62.4871134707371,13.7651140912507));
#80023=CARTESIAN_POINT('Ctrl Pts',(87.9416624683375,62.4918596133234,13.770139629058));
#80024=CARTESIAN_POINT('Ctrl Pts',(88.0059608294402,62.4966057559096,13.7715400797695));
#80025=CARTESIAN_POINT('Ctrl Pts',(88.0700901669213,62.5013518984959,13.7693153518281));
#80026=CARTESIAN_POINT('Ctrl Pts',(88.1320619090005,62.5059383597908,13.7671654736039));
#80027=CARTESIAN_POINT('Ctrl Pts',(88.1938753015951,62.5105248210857,13.7616306118411));
#80028=CARTESIAN_POINT('Ctrl Pts',(88.2551377616971,62.5151112823806,13.7527636434645));
#80029=CARTESIAN_POINT('Ctrl Pts',(88.3195995735795,62.5199372656126,13.7434336092721));
#80030=CARTESIAN_POINT('Ctrl Pts',(88.3834506984063,62.5247632488445,13.7304140131299));
#80031=CARTESIAN_POINT('Ctrl Pts',(88.4462484918887,62.5295892320764,13.7138269283844));
#80032=CARTESIAN_POINT('Ctrl Pts',(88.5090462853711,62.5344152153083,13.6972398436388));
#80033=CARTESIAN_POINT('Ctrl Pts',(88.5707901555195,62.5392411985402,13.6770855449223));
#80034=CARTESIAN_POINT('Ctrl Pts',(88.6310616095541,62.5440671817722,13.653544782347));
#80035=CARTESIAN_POINT('Ctrl Pts',(88.6884760971671,62.5486644054318,13.6311198907805));
#80036=CARTESIAN_POINT('Ctrl Pts',(88.744790359347,62.5532616290915,13.6055303074046));
#80037=CARTESIAN_POINT('Ctrl Pts',(88.7996321340302,62.5578588527511,13.5769050905914));
#80038=CARTESIAN_POINT('Ctrl Pts',(88.8554129482248,62.5625347933138,13.5477897326446));
#80039=CARTESIAN_POINT('Ctrl Pts',(88.9096698458675,62.5672107338765,13.5155339107476));
#80040=CARTESIAN_POINT('Ctrl Pts',(88.9620300039657,62.5718866744392,13.4803255520413));
#80041=CARTESIAN_POINT('Ctrl Pts',(89.0133671090328,62.5764712528796,13.4458051213207));
#80042=CARTESIAN_POINT('Ctrl Pts',(89.0628804852146,62.58105583132,13.408446791651));
#80043=CARTESIAN_POINT('Ctrl Pts',(89.1102436853043,62.5856404097604,13.3684738599751));
#80044=CARTESIAN_POINT('Ctrl Pts',(89.1575779378311,62.5902221861863,13.3285253590588));
#80045=CARTESIAN_POINT('Ctrl Pts',(89.202764231824,62.5948039626123,13.2859657523754));
#80046=CARTESIAN_POINT('Ctrl Pts',(89.24550791434,62.5993857390382,13.2410595921195));
#80047=CARTESIAN_POINT('Ctrl Pts',(89.288241172256,62.6039663980315,13.1961643838622));
#80048=CARTESIAN_POINT('Ctrl Pts',(89.3285326504828,62.6085470570248,13.1489241266734));
#80049=CARTESIAN_POINT('Ctrl Pts',(89.3661248830719,62.613127716018,13.0996398729148));
#80050=CARTESIAN_POINT('Ctrl Pts',(89.4050751943188,62.6178738585378,13.0485751478039));
#80051=CARTESIAN_POINT('Ctrl Pts',(89.4411270933243,62.6226200010576,12.9953163367531));
#80052=CARTESIAN_POINT('Ctrl Pts',(89.4740417248846,62.6273661435774,12.9402332336664));
#80053=CARTESIAN_POINT('Ctrl Pts',(89.5058489631424,62.6319526049405,12.887003368989));
#80054=CARTESIAN_POINT('Ctrl Pts',(89.534726516419,62.6365390663036,12.8320705261377));
#80055=CARTESIAN_POINT('Ctrl Pts',(89.5605058711942,62.6411255276667,12.7757932027955));
#80056=CARTESIAN_POINT('Ctrl Pts',(89.5876315178696,62.6459515107648,12.7165768724364));
#80057=CARTESIAN_POINT('Ctrl Pts',(89.6113262497302,62.6507774938629,12.6558723794506));
#80058=CARTESIAN_POINT('Ctrl Pts',(89.6314525334729,62.655603476961,12.5941178110623));
#80059=CARTESIAN_POINT('Ctrl Pts',(89.6515788172157,62.6604294600591,12.532363242674));
#80060=CARTESIAN_POINT('Ctrl Pts',(89.6681365624707,62.6652554431573,12.4695592451861));
#80061=CARTESIAN_POINT('Ctrl Pts',(89.6810506312657,62.6700814262554,12.4061554418334));
#80062=CARTESIAN_POINT('Ctrl Pts',(89.6933525516511,62.6746786497019,12.3457570845572));
#80063=CARTESIAN_POINT('Ctrl Pts',(89.7023989868417,62.6792758731483,12.2845665250379));
#80064=CARTESIAN_POINT('Ctrl Pts',(89.7080964470144,62.6838730965948,12.2229665095841));
#80065=CARTESIAN_POINT('Ctrl Pts',(89.7138914634168,62.6885490371841,12.1603117319957));
#80066=CARTESIAN_POINT('Ctrl Pts',(89.716221539061,62.6932249777735,12.0972338451252));
#80067=CARTESIAN_POINT('Ctrl Pts',(89.715042336769,62.6979009183628,12.0341479969423));
#80068=CARTESIAN_POINT('Ctrl Pts',(89.7138861746983,62.7024854965906,11.9722947717923));
#80069=CARTESIAN_POINT('Ctrl Pts',(89.7093566456306,62.7070700748183,11.9104344269658));
#80070=CARTESIAN_POINT('Ctrl Pts',(89.7014642814849,62.7116546530461,11.848962333629));
#80071=CARTESIAN_POINT('Ctrl Pts',(89.6935767410136,62.7162364292602,11.7875278109562));
#80072=CARTESIAN_POINT('Ctrl Pts',(89.6823305055283,62.7208182054742,11.7264815731116));
#80073=CARTESIAN_POINT('Ctrl Pts',(89.6677880115279,62.7253999816883,11.6662146570254));
#80074=CARTESIAN_POINT('Ctrl Pts',(89.6532490642397,62.7299806404708,11.6059624392023));
#80075=CARTESIAN_POINT('Ctrl Pts',(89.6354155736761,62.7345612992533,11.5464896604513));
#80076=CARTESIAN_POINT('Ctrl Pts',(89.614400811079,62.7391419580359,11.4881759137668));
#80077=CARTESIAN_POINT('Ctrl Pts',(89.5926268551138,62.7438881007611,11.4277554856698));
#80078=CARTESIAN_POINT('Ctrl Pts',(89.5674375055463,62.7486342434863,11.3685800056446));
#80079=CARTESIAN_POINT('Ctrl Pts',(89.5390138793376,62.7533803862115,11.3110507168348));
#80080=CARTESIAN_POINT('Ctrl Pts',(89.5115465516341,62.7579668473691,11.2554569718042));
#80081=CARTESIAN_POINT('Ctrl Pts',(89.4810594586578,62.7625533085266,11.2014008237734));
#80082=CARTESIAN_POINT('Ctrl Pts',(89.4477623803717,62.7671397696841,11.1492182931861));
#80083=CARTESIAN_POINT('Ctrl Pts',(89.4127264026994,62.7719657531932,11.0943105934524));
#80084=CARTESIAN_POINT('Ctrl Pts',(89.3745792636135,62.7767917367022,11.0414781006924));
#80085=CARTESIAN_POINT('Ctrl Pts',(89.3336144116812,62.7816177202113,10.991073977609));
#80086=CARTESIAN_POINT('Ctrl Pts',(89.2926495597488,62.7864437037204,10.9406698545257));
#80087=CARTESIAN_POINT('Ctrl Pts',(89.2488674889268,62.7912696872295,10.8926945275948));
#80088=CARTESIAN_POINT('Ctrl Pts',(89.2026051825974,62.7960956707386,10.847454996971));
#80089=CARTESIAN_POINT('Ctrl Pts',(89.1585357887037,62.8006928943761,10.8043598974653));
#80090=CARTESIAN_POINT('Ctrl Pts',(89.112035077645,62.8052901180137,10.7635701106697));
#80091=CARTESIAN_POINT('Ctrl Pts',(89.0633738939566,62.8098873416513,10.7253717805004));
#80092=CARTESIAN_POINT('Ctrl Pts',(89.013879498924,62.8145632822167,10.6865193913952));
#80093=CARTESIAN_POINT('Ctrl Pts',(88.9621502613259,62.8192392227821,10.6503484783872));
#80094=CARTESIAN_POINT('Ctrl Pts',(88.9085109073074,62.8239151633476,10.6171214658005));
#80095=CARTESIAN_POINT('Ctrl Pts',(88.8559196005661,62.8284997417617,10.5845436683414));
#80096=CARTESIAN_POINT('Ctrl Pts',(88.8014926022352,62.8330843201758,10.5547960464102));
#80097=CARTESIAN_POINT('Ctrl Pts',(88.7455677845218,62.83766889859,10.528084200763));
#80098=CARTESIAN_POINT('Ctrl Pts',(88.689677147101,62.8422506749882,10.5013886809393));
#80099=CARTESIAN_POINT('Ctrl Pts',(88.6322909638731,62.8468324513864,10.477725477324));
#80100=CARTESIAN_POINT('Ctrl Pts',(88.5737716187422,62.8514142277845,10.4572542336533));
#80101=CARTESIAN_POINT('Ctrl Pts',(88.5152665456981,62.8559948867486,10.4367879826456));
#80102=CARTESIAN_POINT('Ctrl Pts',(88.4556293396536,62.8605755457127,10.4195123142004));
#80103=CARTESIAN_POINT('Ctrl Pts',(88.3952403429229,62.8651562046769,10.405537957534));
#80104=CARTESIAN_POINT('Ctrl Pts',(88.3326696977595,62.8699023472223,10.3910587550351));
#80105=CARTESIAN_POINT('Ctrl Pts',(88.269292454637,62.8746484897677,10.3801241550034));
#80106=CARTESIAN_POINT('Ctrl Pts',(88.2055439439558,62.8793946323131,10.372799631033));
#80107=CARTESIAN_POINT('Ctrl Pts',(88.1439402149616,62.8839810936439,10.3657215364255));
#80108=CARTESIAN_POINT('Ctrl Pts',(88.0819903367574,62.8885675549747,10.3620144014998));
#80109=CARTESIAN_POINT('Ctrl Pts',(88.0200903916493,62.8931540163055,10.3616842427591));
#80110=CARTESIAN_POINT('Ctrl Pts',(87.9549578045197,62.8979799994582,10.3613368419188));
#80111=CARTESIAN_POINT('Ctrl Pts',(87.8898811525563,62.9028059826109,10.3647287827876));
#80112=CARTESIAN_POINT('Ctrl Pts',(87.8253163012447,62.9076319657636,10.3718050880679));
#80113=CARTESIAN_POINT('Ctrl Pts',(87.7607514499332,62.9124579489163,10.3788813933482));
#80114=CARTESIAN_POINT('Ctrl Pts',(87.696699025486,62.917283932069,10.3896418793765));
#80115=CARTESIAN_POINT('Ctrl Pts',(87.6335997244982,62.9221099152218,10.4039699558518));
#80116=CARTESIAN_POINT('Ctrl Pts',(87.5734914281143,62.9267071392979,10.4176188593088));
#80117=CARTESIAN_POINT('Ctrl Pts',(87.5140011306449,62.931304363374,10.4345607631823));
#80118=CARTESIAN_POINT('Ctrl Pts',(87.4555161334491,62.9359015874501,10.4547233292815));
#80119=CARTESIAN_POINT('Ctrl Pts',(87.3960297209697,62.9405775279607,10.4752311309594));
#80120=CARTESIAN_POINT('Ctrl Pts',(87.3375838976558,62.9452534684713,10.4990709003749));
#80121=CARTESIAN_POINT('Ctrl Pts',(87.2805752627201,62.949929408982,10.526112166822));
#80122=CARTESIAN_POINT('Ctrl Pts',(87.2246805005826,62.9545139878428,10.5526250829383));
#80123=CARTESIAN_POINT('Ctrl Pts',(87.1701677523669,62.9590985667036,10.5822152866476));
#80124=CARTESIAN_POINT('Ctrl Pts',(87.1173930091322,62.9636831455644,10.6147104418924));
#80125=CARTESIAN_POINT('Ctrl Pts',(87.0646505208948,62.968264922411,10.6471857366682));
#80126=CARTESIAN_POINT('Ctrl Pts',(87.013644363941,62.9728466992577,10.682562196162));
#80127=CARTESIAN_POINT('Ctrl Pts',(86.9647052149742,62.9774284761043,10.7206219644918));
#80128=CARTESIAN_POINT('Ctrl Pts',(86.9157780016,62.9820091355179,10.758672450562));
#80129=CARTESIAN_POINT('Ctrl Pts',(86.8689171971213,62.9865897949315,10.7994046339764));
#80130=CARTESIAN_POINT('Ctrl Pts',(86.8244221247348,62.9911704543451,10.8425590404392));
#80131=CARTESIAN_POINT('Ctrl Pts',(86.7783196059005,62.9959165964584,10.8872724599265));
#80132=CARTESIAN_POINT('Ctrl Pts',(86.7347574844944,63.0006627385718,10.934586106822));
#80133=CARTESIAN_POINT('Ctrl Pts',(86.6940268888191,63.0054088806851,10.9841697637677));
#80134=CARTESIAN_POINT('Ctrl Pts',(86.6546666430059,63.0099953424627,11.0320852163492));
#80135=CARTESIAN_POINT('Ctrl Pts',(86.6179506613849,63.0145818042403,11.0821198809277));
#80136=CARTESIAN_POINT('Ctrl Pts',(86.5840988331452,63.0191682660179,11.1339442636684));
#80137=CARTESIAN_POINT('Ctrl Pts',(86.5484791482572,63.0239942482991,11.1884750904727));
#80138=CARTESIAN_POINT('Ctrl Pts',(86.5160313015061,63.0288202305803,11.2449871385155));
#80139=CARTESIAN_POINT('Ctrl Pts',(86.4869563660697,63.0336462128615,11.3030676062215));
#80140=CARTESIAN_POINT('Ctrl Pts',(86.4578814306333,63.0384721951426,11.3611480739276));
#80141=CARTESIAN_POINT('Ctrl Pts',(86.4321795918688,63.0432981774238,11.4207963355849));
#80142=CARTESIAN_POINT('Ctrl Pts',(86.409991933047,63.048124159705,11.4815789145219));
#80143=CARTESIAN_POINT('Ctrl Pts',(86.3855797573436,63.0534339910998,11.5484555060827));
#80144=CARTESIAN_POINT('Ctrl Pts',(86.3653371628071,63.0587438224946,11.6169309864996));
#80145=CARTESIAN_POINT('Ctrl Pts',(86.3494450064644,63.0640536538894,11.6865137169054));
#80146=CARTESIAN_POINT('Ctrl Pts',(86.333693968622,63.0693163352671,11.7554785695136));
#80147=CARTESIAN_POINT('Ctrl Pts',(86.3222165491053,63.0745790166449,11.8255309165857));
#80148=CARTESIAN_POINT('Ctrl Pts',(86.3151423989973,63.0798416980226,11.8961711664021));
#80149=CARTESIAN_POINT('Ctrl Pts',(86.3095423218201,63.0840077704729,11.9520917850975));
#80150=CARTESIAN_POINT('Ctrl Pts',(86.3067007811299,63.0881738429231,12.0083803880777));
#80151=CARTESIAN_POINT('Ctrl Pts',(86.3066604360558,63.0923399153734,12.0647808303758));
#80152=CARTESIAN_POINT('',(86.3066604397214,63.8860899154862,12.067224283217));
#80153=CARTESIAN_POINT('Ctrl Pts',(86.3066604360553,63.0923399154299,12.0647808311405));
#80154=CARTESIAN_POINT('Ctrl Pts',(86.3066159630468,63.0969322453676,12.1269519630066));
#80155=CARTESIAN_POINT('Ctrl Pts',(86.3099776468474,63.1015245753052,12.1891522354369));
#80156=CARTESIAN_POINT('Ctrl Pts',(86.3167284964179,63.1061169052429,12.2509835337255));
#80157=CARTESIAN_POINT('Ctrl Pts',(86.3234790823301,63.1107090558246,12.312812417158));
#80158=CARTESIAN_POINT('Ctrl Pts',(86.3336185148868,63.1153012064062,12.3742718532793));
#80159=CARTESIAN_POINT('Ctrl Pts',(86.3470779954168,63.1198933569879,12.4349693730703));
#80160=CARTESIAN_POINT('Ctrl Pts',(86.3605524404198,63.1244906131985,12.495734377367));
#80161=CARTESIAN_POINT('Ctrl Pts',(86.3773541968501,63.1290878694091,12.5557352789889));
#80162=CARTESIAN_POINT('Ctrl Pts',(86.3973636303177,63.1336851256196,12.6145913798436));
#80163=CARTESIAN_POINT('Ctrl Pts',(86.417383747727,63.1382848365133,12.6734789066327));
#80164=CARTESIAN_POINT('Ctrl Pts',(86.440614764977,63.1428845474069,12.7312199457579));
#80165=CARTESIAN_POINT('Ctrl Pts',(86.466888688362,63.1474842583005,12.7874534585623));
#80166=CARTESIAN_POINT('Ctrl Pts',(86.4932165744992,63.1520934163199,12.8438024666842));
#80167=CARTESIAN_POINT('Ctrl Pts',(86.5225996154727,63.1567025743394,12.8986373151098));
#80168=CARTESIAN_POINT('Ctrl Pts',(86.5548239238879,63.1613117323588,12.9516218555111));
#80169=CARTESIAN_POINT('Ctrl Pts',(86.5847159075744,63.1655872896353,13.0007714911495));
#80170=CARTESIAN_POINT('Ctrl Pts',(86.6170520880028,63.1698628469118,13.048329009007));
#80171=CARTESIAN_POINT('Ctrl Pts',(86.6516306929192,63.1741384041883,13.0940515174672));
#80172=CARTESIAN_POINT('Ctrl Pts',(86.6888107827956,63.1787356285181,13.143213910746));
#80173=CARTESIAN_POINT('Ctrl Pts',(86.7287376134219,63.1833328528479,13.1904576611463));
#80174=CARTESIAN_POINT('Ctrl Pts',(86.7711858425798,63.1879300771777,13.2354595720504));
#80175=CARTESIAN_POINT('Ctrl Pts',(86.814360893162,63.1926060176566,13.2812320298921));
#80176=CARTESIAN_POINT('Ctrl Pts',(86.8601442563419,63.1972819581355,13.3246846734459));
#80177=CARTESIAN_POINT('Ctrl Pts',(86.9082537831574,63.2019578986144,13.365509760194));
#80178=CARTESIAN_POINT('Ctrl Pts',(86.955423316475,63.2065424776949,13.4055371813104));
#80179=CARTESIAN_POINT('Ctrl Pts',(87.0048285241927,63.2111270567754,13.4430384546965));
#80180=CARTESIAN_POINT('Ctrl Pts',(87.0561658174368,63.2157116358559,13.4777600785576));
#80181=CARTESIAN_POINT('Ctrl Pts',(87.1074717340822,63.2202934129091,13.5124604810727));
#80182=CARTESIAN_POINT('Ctrl Pts',(87.1607069739893,63.2248751899622,13.5443843181029));
#80183=CARTESIAN_POINT('Ctrl Pts',(87.215536882838,63.2294569670154,13.573319894659));
#80184=CARTESIAN_POINT('Ctrl Pts',(87.2703534192588,63.2340376266222,13.6022484141378));
#80185=CARTESIAN_POINT('Ctrl Pts',(87.3267634025508,63.238618286229,13.6281898824503));
#80186=CARTESIAN_POINT('Ctrl Pts',(87.3844071542986,63.2431989458357,13.6509783094149));
#80187=CARTESIAN_POINT('Ctrl Pts',(87.4441333616792,63.2479450877387,13.6745899979934));
#80188=CARTESIAN_POINT('Ctrl Pts',(87.5051836700963,63.2526912296417,13.6948161946898));
#80189=CARTESIAN_POINT('Ctrl Pts',(87.5671373018131,63.2574373715447,13.7115274962024));
#80190=CARTESIAN_POINT('Ctrl Pts',(87.6270065555069,63.2620238334805,13.7276765599794));
#80191=CARTESIAN_POINT('Ctrl Pts',(87.687718779297,63.2666102954163,13.7405434605201));
#80192=CARTESIAN_POINT('Ctrl Pts',(87.748883177254,63.2711967573522,13.7500634212623));
#80193=CARTESIAN_POINT('Ctrl Pts',(87.8132417788889,63.2760227392387,13.7600805452992));
#80194=CARTESIAN_POINT('Ctrl Pts',(87.8781004378546,63.2808487211253,13.7663914943369));
#80195=CARTESIAN_POINT('Ctrl Pts',(87.9430001797093,63.2856747030118,13.7689829300496));
#80196=CARTESIAN_POINT('Ctrl Pts',(88.0078999215639,63.2905006848984,13.7715743657623));
#80197=CARTESIAN_POINT('Ctrl Pts',(88.0728400997638,63.2953266667849,13.7704463767699));
#80198=CARTESIAN_POINT('Ctrl Pts',(88.1373675896353,63.3001526486715,13.7656488072216));
#80199=CARTESIAN_POINT('Ctrl Pts',(88.1988364307533,63.3047498755962,13.7610786458702));
#80200=CARTESIAN_POINT('Ctrl Pts',(88.2601832066688,63.3093471025209,13.753160215809));
#80201=CARTESIAN_POINT('Ctrl Pts',(88.321014167319,63.3139443294457,13.741907530761));
#80202=CARTESIAN_POINT('Ctrl Pts',(88.3828866691991,63.3186202696002,13.730462178438));
#80203=CARTESIAN_POINT('Ctrl Pts',(88.4442249902356,63.3232962097547,13.7155672636015));
#80204=CARTESIAN_POINT('Ctrl Pts',(88.5046175526032,63.3279721499093,13.6972929066731));
#80205=CARTESIAN_POINT('Ctrl Pts',(88.5638301665237,63.3325567316563,13.6793755936957));
#80206=CARTESIAN_POINT('Ctrl Pts',(88.6221331352863,63.3371413134033,13.6582098604404));
#80207=CARTESIAN_POINT('Ctrl Pts',(88.6791488201293,63.3417258951503,13.6339132596416));
#80208=CARTESIAN_POINT('Ctrl Pts',(88.7361296580817,63.3463076748891,13.6096315084581));
#80209=CARTESIAN_POINT('Ctrl Pts',(88.791824304825,63.3508894546279,13.5822228831234));
#80210=CARTESIAN_POINT('Ctrl Pts',(88.8458733945532,63.3554712343667,13.5518537110588));
#80211=CARTESIAN_POINT('Ctrl Pts',(88.8999093024665,63.3600518966737,13.5214919456093));
#80212=CARTESIAN_POINT('Ctrl Pts',(88.9523000064715,63.3646325589806,13.4881713160261));
#80213=CARTESIAN_POINT('Ctrl Pts',(89.0027109653233,63.3692132212876,13.4521039632212));
#80214=CARTESIAN_POINT('Ctrl Pts',(89.0549430265505,63.3739593606099,13.4147336726551));
#80215=CARTESIAN_POINT('Ctrl Pts',(89.1050490569066,63.3787054999321,13.3744146941797));
#80216=CARTESIAN_POINT('Ctrl Pts',(89.1526921134748,63.3834516392544,13.3314303432546));
#80217=CARTESIAN_POINT('Ctrl Pts',(89.1987323115123,63.3880381038948,13.2898921177154));
#80218=CARTESIAN_POINT('Ctrl Pts',(89.2424723179012,63.3926245685351,13.2458654513764));
#80219=CARTESIAN_POINT('Ctrl Pts',(89.2836457449736,63.3972110331755,13.1996435257173));
#80220=CARTESIAN_POINT('Ctrl Pts',(89.326969309805,63.4020370098387,13.1510078221746));
#80221=CARTESIAN_POINT('Ctrl Pts',(89.367450475186,63.4068629865019,13.0999417908209));
#80222=CARTESIAN_POINT('Ctrl Pts',(89.4048290890655,63.4116889631651,13.0468237895131));
#80223=CARTESIAN_POINT('Ctrl Pts',(89.442207702945,63.4165149398283,12.9937057882052));
#80224=CARTESIAN_POINT('Ctrl Pts',(89.476483489092,63.4213409164915,12.9385364081796));
#80225=CARTESIAN_POINT('Ctrl Pts',(89.5074525489028,63.4261668931547,12.881723362717));
#80226=CARTESIAN_POINT('Ctrl Pts',(89.5369535985093,63.4307641065609,12.8276033964433));
#80227=CARTESIAN_POINT('Ctrl Pts',(89.563575507742,63.4353613199671,12.7717698886372));
#80228=CARTESIAN_POINT('Ctrl Pts',(89.5871164801729,63.4399585333734,12.7145612357576));
#80229=CARTESIAN_POINT('Ctrl Pts',(89.6110605976892,63.4446344752177,12.6563728702804));
#80230=CARTESIAN_POINT('Ctrl Pts',(89.6318169242142,63.4493104170621,12.5967622370934));
#80231=CARTESIAN_POINT('Ctrl Pts',(89.6492211283399,63.4539863589064,12.5361131462324));
#80232=CARTESIAN_POINT('Ctrl Pts',(89.6662852330027,63.4585709271207,12.4766492128819));
#80233=CARTESIAN_POINT('Ctrl Pts',(89.6801268988914,63.4631554953349,12.4161875550014));
#80234=CARTESIAN_POINT('Ctrl Pts',(89.6906400536717,63.4677400635492,12.3551091933886));
#80235=CARTESIAN_POINT('Ctrl Pts',(89.7011467830677,63.4723218297869,12.2940681613835));
#80236=CARTESIAN_POINT('Ctrl Pts',(89.7083289489158,63.4769035960247,12.2324116736439));
#80237=CARTESIAN_POINT('Ctrl Pts',(89.7121313667431,63.4814853622625,12.1705318548713));
#80238=CARTESIAN_POINT('Ctrl Pts',(89.7159328572555,63.4860660111217,12.1086671270431));
#80239=CARTESIAN_POINT('Ctrl Pts',(89.7163562047732,63.490646659981,12.0465796841666));
#80240=CARTESIAN_POINT('Ctrl Pts',(89.7133981785168,63.4952273088402,11.9846656445125));
#80241=CARTESIAN_POINT('Ctrl Pts',(89.7103332757384,63.49997346124,11.9205145871154));
#80242=CARTESIAN_POINT('Ctrl Pts',(89.7036379391208,63.5047196136398,11.8565502871672));
#80243=CARTESIAN_POINT('Ctrl Pts',(89.693367431562,63.5094657660396,11.793209492798));
#80244=CARTESIAN_POINT('Ctrl Pts',(89.6834425112015,63.514052217519,11.7320000213007));
#80245=CARTESIAN_POINT('Ctrl Pts',(89.670179395771,63.5186386689983,11.6713732593582));
#80246=CARTESIAN_POINT('Ctrl Pts',(89.6536799050908,63.5232251204777,11.61171202414));
#80247=CARTESIAN_POINT('Ctrl Pts',(89.6363186423432,63.5280511233377,11.548934669339));
#80248=CARTESIAN_POINT('Ctrl Pts',(89.6153738562178,63.5328771261977,11.4872270800027));
#80249=CARTESIAN_POINT('Ctrl Pts',(89.5910223117948,63.5377031290578,11.4270130440841));
#80250=CARTESIAN_POINT('Ctrl Pts',(89.5666707673718,63.5425291319178,11.3667990081655));
#80251=CARTESIAN_POINT('Ctrl Pts',(89.5389128115545,63.5473551347778,11.3080790784421));
#80252=CARTESIAN_POINT('Ctrl Pts',(89.5079803849733,63.5521811376379,11.2512457041505));
#80253=CARTESIAN_POINT('Ctrl Pts',(89.4785142705607,63.5567783699971,11.1971064433675));
#80254=CARTESIAN_POINT('Ctrl Pts',(89.4460469112061,63.5613756023564,11.1444566023782));
#80255=CARTESIAN_POINT('Ctrl Pts',(89.4107531490587,63.5659728347156,11.0936492622));
#80256=CARTESIAN_POINT('Ctrl Pts',(89.3748551385258,63.5706487741909,11.0419720727507));
#80257=CARTESIAN_POINT('Ctrl Pts',(89.3360332053818,63.5753247136661,10.9922015782452));
#80258=CARTESIAN_POINT('Ctrl Pts',(89.2945206623623,63.5800006531413,10.9446840120247));
#80259=CARTESIAN_POINT('Ctrl Pts',(89.2538191386571,63.5845852400529,10.8980947836311));
#80260=CARTESIAN_POINT('Ctrl Pts',(89.2105315420466,63.5891698269645,10.8536716471459));
#80261=CARTESIAN_POINT('Ctrl Pts',(89.1649204445675,63.5937544138761,10.8117103830418));
#80262=CARTESIAN_POINT('Ctrl Pts',(89.1193372248128,63.598336198666,10.7697747658661));
#80263=CARTESIAN_POINT('Ctrl Pts',(89.0714336939611,63.6029179834558,10.7302983813848));
#80264=CARTESIAN_POINT('Ctrl Pts',(89.0215093541727,63.6074997682456,10.6935402808354));
#80265=CARTESIAN_POINT('Ctrl Pts',(88.9715971915321,63.6120804354829,10.6567911460294));
#80266=CARTESIAN_POINT('Ctrl Pts',(88.9196656081722,63.6166611027203,10.6227592806352));
#80267=CARTESIAN_POINT('Ctrl Pts',(88.8660456409869,63.6212417699576,10.5916622546278));
#80268=CARTESIAN_POINT('Ctrl Pts',(88.8104887636248,63.6259879043046,10.5594419130104));
#80269=CARTESIAN_POINT('Ctrl Pts',(88.7531196593087,63.6307340386515,10.5303728470156));
#80270=CARTESIAN_POINT('Ctrl Pts',(88.6943352168073,63.6354801729985,10.5046455184453));
#80271=CARTESIAN_POINT('Ctrl Pts',(88.6375283469838,63.6400666422162,10.4797836852322));
#80272=CARTESIAN_POINT('Ctrl Pts',(88.5794003798237,63.6446531114339,10.4580424230845));
#80273=CARTESIAN_POINT('Ctrl Pts',(88.5203281570851,63.6492395806516,10.4395438327455));
#80274=CARTESIAN_POINT('Ctrl Pts',(88.4581712824178,63.6540655475632,10.420079277191));
#80275=CARTESIAN_POINT('Ctrl Pts',(88.3949694553103,63.6588915144748,10.4042055000808));
#80276=CARTESIAN_POINT('Ctrl Pts',(88.3311745735203,63.6637174813864,10.3920038596009));
#80277=CARTESIAN_POINT('Ctrl Pts',(88.2673796917304,63.668543448298,10.379802219121));
#80278=CARTESIAN_POINT('Ctrl Pts',(88.2029924077756,63.6733694152096,10.3712727236636));
#80279=CARTESIAN_POINT('Ctrl Pts',(88.1384682187076,63.6781953821212,10.366433382059));
#80280=CARTESIAN_POINT('Ctrl Pts',(88.0770020850411,63.6827926274573,10.3618233959092));
#80281=CARTESIAN_POINT('Ctrl Pts',(88.0151593784975,63.6873898727934,10.3605427020705));
#80282=CARTESIAN_POINT('Ctrl Pts',(87.9533315665747,63.6919871181294,10.3626359204837));
#80283=CARTESIAN_POINT('Ctrl Pts',(87.8904454282439,63.6966630559826,10.3647649691853));
#80284=CARTESIAN_POINT('Ctrl Pts',(87.8275752209313,63.7013389938357,10.3703846559915));
#80285=CARTESIAN_POINT('Ctrl Pts',(87.7651383693305,63.7060149316888,10.3794867643079));
#80286=CARTESIAN_POINT('Ctrl Pts',(87.7039211269101,63.7105995321893,10.3884110767462));
#80287=CARTESIAN_POINT('Ctrl Pts',(87.6431209903504,63.7151841326898,10.4006829093132));
#80288=CARTESIAN_POINT('Ctrl Pts',(87.5831288716814,63.7197687331902,10.4162420986244));
#80289=CARTESIAN_POINT('Ctrl Pts',(87.5231734179149,63.7243505317572,10.4317917787505));
#80290=CARTESIAN_POINT('Ctrl Pts',(87.4640254945627,63.7289323303241,10.4506247043206));
#80291=CARTESIAN_POINT('Ctrl Pts',(87.4060651872506,63.733514128891,10.4726297643285));
#80292=CARTESIAN_POINT('Ctrl Pts',(87.3481190150353,63.7380948100697,10.4946294578422));
#80293=CARTESIAN_POINT('Ctrl Pts',(87.2913603595842,63.7426754912483,10.5197995694711));
#80294=CARTESIAN_POINT('Ctrl Pts',(87.2361515614434,63.747256172427,10.5479799958938));
#80295=CARTESIAN_POINT('Ctrl Pts',(87.1789487926766,63.7520022936085,10.5771782119517));
#80296=CARTESIAN_POINT('Ctrl Pts',(87.1234105231449,63.7567484147899,10.6096081442033));
#80297=CARTESIAN_POINT('Ctrl Pts',(87.0699120307322,63.7614945359714,10.6450396663878));
#80298=CARTESIAN_POINT('Ctrl Pts',(87.0182129826056,63.7660810193713,10.6792794344261));
#80299=CARTESIAN_POINT('Ctrl Pts',(86.9684190441821,63.7706675027713,10.7163216925554));
#80300=CARTESIAN_POINT('Ctrl Pts',(86.9208371947618,63.7752539861712,10.7559160738047));
#80301=CARTESIAN_POINT('Ctrl Pts',(86.8707711346017,63.7800799262434,10.7975776463956));
#80302=CARTESIAN_POINT('Ctrl Pts',(86.8231549564592,63.7849058663156,10.8420647046982));
#80303=CARTESIAN_POINT('Ctrl Pts',(86.7783021135038,63.7897318063878,10.8890417355625));
#80304=CARTESIAN_POINT('Ctrl Pts',(86.7334492705484,63.79455774646,10.9360187664268));
#80305=CARTESIAN_POINT('Ctrl Pts',(86.6913601237379,63.7993836865322,10.9854852262386));
#80306=CARTESIAN_POINT('Ctrl Pts',(86.6522968591971,63.8042096266043,11.0370682186013));
#80307=CARTESIAN_POINT('Ctrl Pts',(86.6149869464817,63.8088189547027,11.0863359120538));
#80308=CARTESIAN_POINT('Ctrl Pts',(86.580282212688,63.8134282828011,11.1377385149235));
#80309=CARTESIAN_POINT('Ctrl Pts',(86.5484343454252,63.8180376108995,11.1909705481196));
#80310=CARTESIAN_POINT('Ctrl Pts',(86.5166358475953,63.8226397937812,11.244120062908));
#80311=CARTESIAN_POINT('Ctrl Pts',(86.4876856912155,63.8272419766628,11.2990929549601));
#80312=CARTESIAN_POINT('Ctrl Pts',(86.4617940000144,63.8318441595444,11.3555525317038));
#80313=CARTESIAN_POINT('Ctrl Pts',(86.4359346122434,63.8364406005728,11.4119416673944));
#80314=CARTESIAN_POINT('Ctrl Pts',(86.4131263256213,63.8410370416011,11.4698133498059));
#80315=CARTESIAN_POINT('Ctrl Pts',(86.3935337383234,63.8456334826294,11.5288056888443));
#80316=CARTESIAN_POINT('Ctrl Pts',(86.3739560463781,63.8502264291927,11.5877531786919));
#80317=CARTESIAN_POINT('Ctrl Pts',(86.3575893621039,63.8548193757561,11.6478191568059));
#80318=CARTESIAN_POINT('Ctrl Pts',(86.3445497596784,63.8594123223195,11.7086228432984));
#80319=CARTESIAN_POINT('Ctrl Pts',(86.3315110747425,63.864004945715,11.7694222515353));
#80320=CARTESIAN_POINT('Ctrl Pts',(86.3217991299969,63.8685975691104,11.8309587750666));
#80321=CARTESIAN_POINT('Ctrl Pts',(86.3154793842121,63.8731901925059,11.892839158473));
#80322=CARTESIAN_POINT('Ctrl Pts',(86.3095624341705,63.8774901001472,11.9507755295932));
#80323=CARTESIAN_POINT('Ctrl Pts',(86.3066186245782,63.8817900077885,12.0090128773501));
#80324=CARTESIAN_POINT('Ctrl Pts',(86.3066604397209,63.8860899154298,12.0672242824529));
#80325=CARTESIAN_POINT('Ctrl Pts',(86.3066604397214,63.8860899154862,12.067224283217));
#80326=CARTESIAN_POINT('Ctrl Pts',(86.3067115579032,63.8913464639361,12.1383865259391));
#80327=CARTESIAN_POINT('Ctrl Pts',(86.3112236097562,63.896603012386,12.2093698792769));
#80328=CARTESIAN_POINT('Ctrl Pts',(86.3201057341301,63.9018595608358,12.2796619227856));
#80329=CARTESIAN_POINT('Ctrl Pts',(86.3290710981618,63.9071653715202,12.350612714742));
#80330=CARTESIAN_POINT('Ctrl Pts',(86.3424887120832,63.9124711822046,12.4208589876627));
#80331=CARTESIAN_POINT('Ctrl Pts',(86.3602155595618,63.917776992889,12.4898933436694));
#80332=CARTESIAN_POINT('Ctrl Pts',(86.374077337685,63.9219259522885,12.5438758087973));
#80333=CARTESIAN_POINT('Ctrl Pts',(86.3905730726722,63.926074911688,12.5971175918686));
#80334=CARTESIAN_POINT('Ctrl Pts',(86.409614244658,63.9302238710876,12.6493853770775));
#80335=CARTESIAN_POINT('Ctrl Pts',(86.4307130937734,63.934821186233,12.7073014609478));
#80336=CARTESIAN_POINT('Ctrl Pts',(86.4550012082824,63.9394185013784,12.7641903405576));
#80337=CARTESIAN_POINT('Ctrl Pts',(86.4823581174278,63.9440158165238,12.819676874029));
#80338=CARTESIAN_POINT('Ctrl Pts',(86.5101828290803,63.9486917456508,12.8761122259262));
#80339=CARTESIAN_POINT('Ctrl Pts',(86.5411821822989,63.9533676747777,12.9310962899627));
#80340=CARTESIAN_POINT('Ctrl Pts',(86.5751768783403,63.9580436039047,12.984252034524));
#80341=CARTESIAN_POINT('Ctrl Pts',(86.6085080940721,63.9626282721214,13.0363703293074));
#80342=CARTESIAN_POINT('Ctrl Pts',(86.6447184943683,63.9672129403381,13.0867305814165));
#80343=CARTESIAN_POINT('Ctrl Pts',(86.6835923425951,63.9717976085548,13.1350012846871));
#80344=CARTESIAN_POINT('Ctrl Pts',(86.7224424248471,63.9763794738818,13.1832424771074));
#80345=CARTESIAN_POINT('Ctrl Pts',(86.7639524076726,63.9809613392088,13.2293962581041));
#80346=CARTESIAN_POINT('Ctrl Pts',(86.8078645788163,63.9855432045358,13.2731619584352));
#80347=CARTESIAN_POINT('Ctrl Pts',(86.851766030899,63.990123951419,13.3169169754592));
#80348=CARTESIAN_POINT('Ctrl Pts',(86.8980681468718,63.9947046983023,13.3582847098619));
#80349=CARTESIAN_POINT('Ctrl Pts',(86.9464758684385,63.9992854451855,13.3970008297981));
#80350=CARTESIAN_POINT('Ctrl Pts',(86.9966305171738,64.0040315010509,13.437114128523));
#80351=CARTESIAN_POINT('Ctrl Pts',(87.0490452375039,64.0087775569164,13.4743803574942));
#80352=CARTESIAN_POINT('Ctrl Pts',(87.103355859577,64.0135236127818,13.5085522347408));
#80353=CARTESIAN_POINT('Ctrl Pts',(87.1558411568784,64.0181101585366,13.5415756299474));
#80354=CARTESIAN_POINT('Ctrl Pts',(87.2100964340709,64.0226967042913,13.571709190194));
#80355=CARTESIAN_POINT('Ctrl Pts',(87.2657671565741,64.027283250046,13.598776188711));
#80356=CARTESIAN_POINT('Ctrl Pts',(87.3243420395011,64.0321090609668,13.6272551844564));
#80357=CARTESIAN_POINT('Ctrl Pts',(87.3844835014319,64.0369348718876,13.6523386513244));
#80358=CARTESIAN_POINT('Ctrl Pts',(87.4457567944024,64.0417606828084,13.6738790234734));
#80359=CARTESIAN_POINT('Ctrl Pts',(87.5070300873729,64.0465864937292,13.6954193956224));
#80360=CARTESIAN_POINT('Ctrl Pts',(87.5694345675354,64.05141230465,13.7134165678344));
#80361=CARTESIAN_POINT('Ctrl Pts',(87.6325225185108,64.0562381155708,13.7277850738304));
#80362=CARTESIAN_POINT('Ctrl Pts',(87.6926238497539,64.0608354698386,13.7414733665232));
#80363=CARTESIAN_POINT('Ctrl Pts',(87.7535920397938,64.0654328241065,13.7519250364605));
#80364=CARTESIAN_POINT('Ctrl Pts',(87.8150465687771,64.0700301783744,13.7590378283996));
#80365=CARTESIAN_POINT('Ctrl Pts',(87.8775513714924,64.074706102611,13.7662721797853));
#80366=CARTESIAN_POINT('Ctrl Pts',(87.9405587967322,64.0793820268477,13.7700522461079));
#80367=CARTESIAN_POINT('Ctrl Pts',(88.0036548428794,64.0840579510843,13.7703241722944));
#80368=CARTESIAN_POINT('Ctrl Pts',(88.0655200941409,64.0886426635258,13.7705907941015));
#80369=CARTESIAN_POINT('Ctrl Pts',(88.1274700066235,64.0932273759673,13.767484909079));
#80370=CARTESIAN_POINT('Ctrl Pts',(88.1891090515675,64.0978120884088,13.7610079649812));
#80371=CARTESIAN_POINT('Ctrl Pts',(88.2507104367725,64.1023939997188,13.7545349781158));
#80372=CARTESIAN_POINT('Ctrl Pts',(88.3120008258701,64.1069759110287,13.7446950692036));
#80373=CARTESIAN_POINT('Ctrl Pts',(88.372587831095,64.1115578223386,13.7315416764536));
#80374=CARTESIAN_POINT('Ctrl Pts',(88.4331600690939,64.1161386168725,13.7183914896572));
#80375=CARTESIAN_POINT('Ctrl Pts',(88.4930287663523,64.1207194114063,13.7019295302079));
#80376=CARTESIAN_POINT('Ctrl Pts',(88.5518118080388,64.1253002059401,13.6822603205814));
#80377=CARTESIAN_POINT('Ctrl Pts',(88.6127150135252,64.130046218783,13.6618816895805));
#80378=CARTESIAN_POINT('Ctrl Pts',(88.6724521808621,64.1347922316258,13.6380601538275));
#80379=CARTESIAN_POINT('Ctrl Pts',(88.7306180579729,64.1395382444686,13.6109675356587));
#80380=CARTESIAN_POINT('Ctrl Pts',(88.7868301759858,64.1441248414094,13.5847849432965));
#80381=CARTESIAN_POINT('Ctrl Pts',(88.8415744630186,64.1487114383501,13.5555478589231));
#80382=CARTESIAN_POINT('Ctrl Pts',(88.8945101450594,64.1532980352908,13.5234582872855));
#80383=CARTESIAN_POINT('Ctrl Pts',(88.9502056475994,64.1581237560847,13.4896957144849));
#80384=CARTESIAN_POINT('Ctrl Pts',(89.0038982612178,64.1629494768786,13.4527754365747));
#80385=CARTESIAN_POINT('Ctrl Pts',(89.0552282352508,64.1677751976725,13.4129826384571));
#80386=CARTESIAN_POINT('Ctrl Pts',(89.1065582092839,64.1726009184663,13.3731898403395));
#80387=CARTESIAN_POINT('Ctrl Pts',(89.1555251062022,64.1774266392602,13.3305250057805));
#80388=CARTESIAN_POINT('Ctrl Pts',(89.2018143077068,64.1822523600541,13.2853178913477));
#80389=CARTESIAN_POINT('Ctrl Pts',(89.2459054887831,64.1868489338214,13.2422574149602));
#80390=CARTESIAN_POINT('Ctrl Pts',(89.2877486809983,64.1914455075887,13.1967137742867));
#80391=CARTESIAN_POINT('Ctrl Pts',(89.3270516149251,64.196042081356,13.148951052658));
#80392=CARTESIAN_POINT('Ctrl Pts',(89.3670338680375,64.2007181031553,13.1003627913069));
#80393=CARTESIAN_POINT('Ctrl Pts',(89.4043867701727,64.2053941249545,13.0494783130407));
#80394=CARTESIAN_POINT('Ctrl Pts',(89.4388403952444,64.2100701467537,12.9966162696345));
#80395=CARTESIAN_POINT('Ctrl Pts',(89.4726154597161,64.2146540747848,12.9447953387328));
#80396=CARTESIAN_POINT('Ctrl Pts',(89.5036041219738,64.2192380028159,12.8910744794241));
#80397=CARTESIAN_POINT('Ctrl Pts',(89.5315930892139,64.2238219308471,12.835786653973));
#80398=CARTESIAN_POINT('Ctrl Pts',(89.5595649573351,64.2284030584487,12.7805326051557));
#80399=CARTESIAN_POINT('Ctrl Pts',(89.5845405346355,64.2329841860503,12.7237139417204));
#80400=CARTESIAN_POINT('Ctrl Pts',(89.6063519077611,64.2375653136519,12.6656891911675));
#80401=CARTESIAN_POINT('Ctrl Pts',(89.6281579731013,64.2421453264387,12.6076785609048));
#80402=CARTESIAN_POINT('Ctrl Pts',(89.6468011837455,64.2467253392255,12.548462902594));
#80403=CARTESIAN_POINT('Ctrl Pts',(89.6621621144506,64.2513053520123,12.4884198236389));
#80404=CARTESIAN_POINT('Ctrl Pts',(89.6780823366137,64.256052123056,12.4261905762921));
#80405=CARTESIAN_POINT('Ctrl Pts',(89.6904764459661,64.2607988940998,12.3630730413557));
#80406=CARTESIAN_POINT('Ctrl Pts',(89.6992689453396,64.2655456651435,12.2995011858686));
#80407=CARTESIAN_POINT('Ctrl Pts',(89.7077633300022,64.2701314942051,12.2380847704347));
#80408=CARTESIAN_POINT('Ctrl Pts',(89.7128964682595,64.2747173232667,12.176244883587));
#80409=CARTESIAN_POINT('Ctrl Pts',(89.7146532730937,64.2793031523283,12.1143772743872));
#80410=CARTESIAN_POINT('Ctrl Pts',(89.7165025618545,64.2841303943632,12.0492527527987));
#80411=CARTESIAN_POINT('Ctrl Pts',(89.7146102193961,64.288957636398,11.9840981549112));
#80412=CARTESIAN_POINT('Ctrl Pts',(89.7090208327119,64.2937848784328,11.9193709194039));
#80413=CARTESIAN_POINT('Ctrl Pts',(89.7034314460276,64.2986121204676,11.8546436838966));
#80414=CARTESIAN_POINT('Ctrl Pts',(89.6941451849246,64.3034393625024,11.7903444424305));
#80415=CARTESIAN_POINT('Ctrl Pts',(89.6812686762512,64.3082666045373,11.7269168468735));
#80416=CARTESIAN_POINT('Ctrl Pts',(89.669003364973,64.3128647163138,11.6664999106631));
#80417=CARTESIAN_POINT('Ctrl Pts',(89.653430589109,64.3174628280904,11.6066254977153));
#80418=CARTESIAN_POINT('Ctrl Pts',(89.6346138356892,64.322060939867,11.5476825797268));
#80419=CARTESIAN_POINT('Ctrl Pts',(89.6154790395132,64.326736769415,11.4877434023053));
#80420=CARTESIAN_POINT('Ctrl Pts',(89.5929895988853,64.3314125989631,11.428768039135));
#80421=CARTESIAN_POINT('Ctrl Pts',(89.5672668221473,64.3360884285111,11.3711558348209));
#80422=CARTESIAN_POINT('Ctrl Pts',(89.5420412208347,64.3406738826084,11.3146571717266));
#80423=CARTESIAN_POINT('Ctrl Pts',(89.5137063783026,64.3452593367056,11.259469927865));
#80424=CARTESIAN_POINT('Ctrl Pts',(89.482426458777,64.3498447908028,11.2059540640111));
#80425=CARTESIAN_POINT('Ctrl Pts',(89.4511657010337,64.3544274358943,11.1524709834684));
#80426=CARTESIAN_POINT('Ctrl Pts',(89.4169636999067,64.3590100809858,11.1006576911016));
#80427=CARTESIAN_POINT('Ctrl Pts',(89.3800307091691,64.3635927260773,11.0508498864937));
#80428=CARTESIAN_POINT('Ctrl Pts',(89.343106791367,64.368174245399,11.0010543176401));
#80429=CARTESIAN_POINT('Ctrl Pts',(89.3034535187289,64.3727557647208,10.9532636670647));
#80430=CARTESIAN_POINT('Ctrl Pts',(89.2613234747187,64.3773372840426,10.9077832481926));
#80431=CARTESIAN_POINT('Ctrl Pts',(89.2176873879003,64.3820825811241,10.8606770190616));
#80432=CARTESIAN_POINT('Ctrl Pts',(89.1713944443903,64.3868278782055,10.816049791169));
#80433=CARTESIAN_POINT('Ctrl Pts',(89.1227677915072,64.391573175287,10.7742000103084));
#80434=CARTESIAN_POINT('Ctrl Pts',(89.0757602773068,64.3961604665505,10.7337437162506));
#80435=CARTESIAN_POINT('Ctrl Pts',(89.0265724969234,64.400747757814,10.6958830645894));
#80436=CARTESIAN_POINT('Ctrl Pts',(88.975528858915,64.4053350490775,10.660845590008));
#80437=CARTESIAN_POINT('Ctrl Pts',(88.9218479809821,64.410159349068,10.6239978560009));
#80438=CARTESIAN_POINT('Ctrl Pts',(88.8661148135088,64.4149836490585,10.5902732849022));
#80439=CARTESIAN_POINT('Ctrl Pts',(88.8087368562257,64.419807949049,10.5598822277727));
#80440=CARTESIAN_POINT('Ctrl Pts',(88.7513588989427,64.4246322490395,10.5294911706431));
#80441=CARTESIAN_POINT('Ctrl Pts',(88.6923367711396,64.42945654903,10.5024338269264));
#80442=CARTESIAN_POINT('Ctrl Pts',(88.6321000033795,64.4342808490205,10.4788611839534));
#80443=CARTESIAN_POINT('Ctrl Pts',(88.5746901027678,64.4388787481654,10.4563947877545));
#80444=CARTESIAN_POINT('Ctrl Pts',(88.5159421840625,64.4434766473103,10.4370013802393));
#80445=CARTESIAN_POINT('Ctrl Pts',(88.4562174867713,64.4480745464552,10.4208385413361));
#80446=CARTESIAN_POINT('Ctrl Pts',(88.3954801624058,64.4527504025822,10.404401662898));
#80447=CARTESIAN_POINT('Ctrl Pts',(88.3337330873303,64.4574262587092,10.3913062036751));
#80448=CARTESIAN_POINT('Ctrl Pts',(88.2713776271557,64.4621021148362,10.3816668005182));
#80449=CARTESIAN_POINT('Ctrl Pts',(88.2102300152025,64.4666873979085,10.3722141161493));
#80450=CARTESIAN_POINT('Ctrl Pts',(88.148497904085,64.4712726809809,10.3660848723485));
#80451=CARTESIAN_POINT('Ctrl Pts',(88.0865727498605,64.4758579640532,10.363336323557));
#80452=CARTESIAN_POINT('Ctrl Pts',(88.0246853185018,64.4804404539145,10.3605894490953));
#80453=CARTESIAN_POINT('Ctrl Pts',(87.9626055845292,64.4850229437759,10.361219208585));
#80454=CARTESIAN_POINT('Ctrl Pts',(87.9007296089269,64.4896054336373,10.3652309749844));
#80455=CARTESIAN_POINT('Ctrl Pts',(87.8388686195203,64.4941868136319,10.3692417697447));
#80456=CARTESIAN_POINT('Ctrl Pts',(87.7772117980863,64.4987681936265,10.3766329124122));
#80457=CARTESIAN_POINT('Ctrl Pts',(87.7161526250997,64.5033495736211,10.3873577328345));
#80458=CARTESIAN_POINT('Ctrl Pts',(87.6529066462057,64.5080950336113,10.3984666577167));
#80459=CARTESIAN_POINT('Ctrl Pts',(87.5903025204143,64.5128404936015,10.4131525448178));
#80460=CARTESIAN_POINT('Ctrl Pts',(87.5287662939644,64.5175859535917,10.4313056896278));
#80461=CARTESIAN_POINT('Ctrl Pts',(87.4692823831931,64.5221731461271,10.4488534027132));
#80462=CARTESIAN_POINT('Ctrl Pts',(87.4107967292947,64.5267603386625,10.4696404779147));
#80463=CARTESIAN_POINT('Ctrl Pts',(87.3536764029595,64.5313475311979,10.4935177188999));
#80464=CARTESIAN_POINT('Ctrl Pts',(87.2935999257984,64.5361721249155,10.5186306798151));
#80465=CARTESIAN_POINT('Ctrl Pts',(87.2350345197086,64.5409967186332,10.5471620804812));
#80466=CARTESIAN_POINT('Ctrl Pts',(87.1783779586482,64.5458213123508,10.5788835378979));
#80467=CARTESIAN_POINT('Ctrl Pts',(87.1217213975878,64.5506459060684,10.6106049953145));
#80468=CARTESIAN_POINT('Ctrl Pts',(87.0669741850425,64.5554704997861,10.6455160969614));
#80469=CARTESIAN_POINT('Ctrl Pts',(87.0144961418063,64.5602950935037,10.6833377504954));
#80470=CARTESIAN_POINT('Ctrl Pts',(86.9649314865339,64.5648518435214,10.7190596849206));
#80471=CARTESIAN_POINT('Ctrl Pts',(86.9171792470767,64.569408593539,10.7575301788349));
#80472=CARTESIAN_POINT('Ctrl Pts',(86.8715645979647,64.5739653435567,10.7985372588559));
#80473=CARTESIAN_POINT('Ctrl Pts',(86.8260299695178,64.5785140997791,10.8394724011576));
#80474=CARTESIAN_POINT('Ctrl Pts',(86.7826258723447,64.5830628560014,10.8829349551343));
#80475=CARTESIAN_POINT('Ctrl Pts',(86.7416468352425,64.5876116122238,10.9286709452756));
#80476=CARTESIAN_POINT('Ctrl Pts',(86.7007077913486,64.592155929119,10.9743622996933));
#80477=CARTESIAN_POINT('Ctrl Pts',(86.6621894639922,64.5967002460141,11.0223223109148));
#80478=CARTESIAN_POINT('Ctrl Pts',(86.626350443695,64.6012445629093,11.0722593689375));
#80479=CARTESIAN_POINT('Ctrl Pts',(86.5905326579707,64.6057861873026,11.1221668393184));
#80480=CARTESIAN_POINT('Ctrl Pts',(86.5573913350624,64.6103278116959,11.1740486141513));
#80481=CARTESIAN_POINT('Ctrl Pts',(86.5271441651915,64.6148694360892,11.2275808344839));
#80482=CARTESIAN_POINT('Ctrl Pts',(86.4969033197675,64.6194101108643,11.2811018616473));
#80483=CARTESIAN_POINT('Ctrl Pts',(86.4695556810674,64.6239507856394,11.3362721974733));
#80484=CARTESIAN_POINT('Ctrl Pts',(86.4452739044528,64.6284914604146,11.3927417810954));
#80485=CARTESIAN_POINT('Ctrl Pts',(86.4209711114364,64.6330360652417,11.4492602403611));
#80486=CARTESIAN_POINT('Ctrl Pts',(86.3997396873906,64.6375806700689,11.5070797162322));
#80487=CARTESIAN_POINT('Ctrl Pts',(86.3817042747851,64.642125274896,11.5658297535875));
#80488=CARTESIAN_POINT('Ctrl Pts',(86.3636611137683,64.6466718321857,11.6246050312552));
#80489=CARTESIAN_POINT('Ctrl Pts',(86.3488168244642,64.6512183894753,11.6843111623066));
#80490=CARTESIAN_POINT('Ctrl Pts',(86.3372453945193,64.655764946765,11.7445651602077));
#80491=CARTESIAN_POINT('Ctrl Pts',(86.3256530493151,64.6603197219176,11.8049280666883));
#80492=CARTESIAN_POINT('Ctrl Pts',(86.3173454475435,64.6648744970702,11.8658403024834));
#80493=CARTESIAN_POINT('Ctrl Pts',(86.3123448009796,64.6694292722228,11.9269124360668));
#80494=CARTESIAN_POINT('Ctrl Pts',(86.3085348838982,64.6728994866108,11.9734423721382));
#80495=CARTESIAN_POINT('Ctrl Pts',(86.3066434735053,64.6763697009989,12.0200649769014));
#80496=CARTESIAN_POINT('Ctrl Pts',(86.3066601088578,64.6798399153869,12.0666091481311));
#80497=CARTESIAN_POINT('Origin',(88.011,66.41344859951,12.066));
#80498=CARTESIAN_POINT('',(88.2080236424798,49.5646,13.3206241207246));
#80499=CARTESIAN_POINT('Ctrl Pts',(88.2080236424798,49.5646,13.3206241207246));
#80500=CARTESIAN_POINT('Ctrl Pts',(88.2097267967144,49.5647720436039,13.3203566608173));
#80501=CARTESIAN_POINT('Ctrl Pts',(88.2114293848816,49.5649442914476,13.3200857362535));
#80502=CARTESIAN_POINT('Ctrl Pts',(88.2180820755138,49.5656183417018,13.3190132321809));
#80503=CARTESIAN_POINT('Ctrl Pts',(88.2230278040899,49.5661216278726,13.3181858300697));
#80504=CARTESIAN_POINT('Ctrl Pts',(88.23517546855,49.5673629764069,13.3160795429129));
#80505=CARTESIAN_POINT('Ctrl Pts',(88.24237135194,49.5681027991327,13.314767709552));
#80506=CARTESIAN_POINT('Ctrl Pts',(88.2684291775434,49.5707972735995,13.3097843361335));
#80507=CARTESIAN_POINT('Ctrl Pts',(88.2872170891576,49.572769374158,13.3057472475379));
#80508=CARTESIAN_POINT('Ctrl Pts',(88.3236804028145,49.5766462220168,13.2970422258303));
#80509=CARTESIAN_POINT('Ctrl Pts',(88.3413616954967,49.5785491700862,13.2924155353734));
#80510=CARTESIAN_POINT('Ctrl Pts',(88.3592479869665,49.5804945016824,13.2873203694679));
#80511=CARTESIAN_POINT('Ctrl Pts',(88.3595600417179,49.5805284474264,13.2872313468875));
#80512=CARTESIAN_POINT('Ctrl Pts',(88.3602208395918,49.5806003433312,13.2870425614078));
#80513=CARTESIAN_POINT('Ctrl Pts',(88.3605695741056,49.5806382941348,13.2869427686971));
#80514=CARTESIAN_POINT('Ctrl Pts',(88.3613076933374,49.5807186361706,13.2867312087848));
#80515=CARTESIAN_POINT('Ctrl Pts',(88.3616970673495,49.5807610281884,13.2866194046731));
#80516=CARTESIAN_POINT('Ctrl Pts',(88.4253992750408,49.5876980346645,13.2682950768527));
#80517=CARTESIAN_POINT('Ctrl Pts',(88.4871985938793,49.5946799449541,13.2451841330288));
#80518=CARTESIAN_POINT('Ctrl Pts',(88.6039655922378,49.6081902466906,13.1908333883167));
#80519=CARTESIAN_POINT('Ctrl Pts',(88.6589629424759,49.6147072468449,13.1600773964497));
#80520=CARTESIAN_POINT('Ctrl Pts',(88.7272693192359,49.6230072425402,13.1149124474686));
#80521=CARTESIAN_POINT('Ctrl Pts',(88.742840582761,49.6249149311283,13.1041081447339));
#80522=CARTESIAN_POINT('Ctrl Pts',(88.7665779572615,49.6278498719295,13.0868379820414));
#80523=CARTESIAN_POINT('Ctrl Pts',(88.7749153990046,49.6288860402733,13.0806139731869));
#80524=CARTESIAN_POINT('Ctrl Pts',(88.7902467120687,49.6308019513485,13.0688728156558));
#80525=CARTESIAN_POINT('Ctrl Pts',(88.7972607507153,49.6316826818768,13.0633832586405));
#80526=CARTESIAN_POINT('Ctrl Pts',(88.8127417394313,49.6336365544447,13.0510022054533));
#80527=CARTESIAN_POINT('Ctrl Pts',(88.8211788486992,49.6347081970147,13.0440743389822));
#80528=CARTESIAN_POINT('Ctrl Pts',(88.8424392148344,49.6374273553418,13.0261531501222));
#80529=CARTESIAN_POINT('Ctrl Pts',(88.8551347783218,49.6390688961246,13.0150109469476));
#80530=CARTESIAN_POINT('Ctrl Pts',(88.9327304991544,49.6492285974841,12.9441197426848));
#80531=CARTESIAN_POINT('Ctrl Pts',(88.9914838492493,49.6574651478001,12.8779949834701));
#80532=CARTESIAN_POINT('Ctrl Pts',(89.0820913064662,49.6720721464964,12.751696996699));
#80533=CARTESIAN_POINT('Ctrl Pts',(89.1168643005801,49.6784030292887,12.6940745755641));
#80534=CARTESIAN_POINT('Ctrl Pts',(89.1518942754838,49.6860669652867,12.6240183029856));
#80535=CARTESIAN_POINT('Ctrl Pts',(89.1567462445896,49.6871636958455,12.6139869404145));
#80536=CARTESIAN_POINT('Ctrl Pts',(89.1639489257088,49.6888490569957,12.5985816003658));
#80537=CARTESIAN_POINT('Ctrl Pts',(89.1663956380392,49.6894322529589,12.5932525969323));
#80538=CARTESIAN_POINT('Ctrl Pts',(89.1706709432374,49.6904709118824,12.5837682049443));
#80539=CARTESIAN_POINT('Ctrl Pts',(89.1725142958538,49.6909254860735,12.5796196537934));
#80540=CARTESIAN_POINT('Ctrl Pts',(89.1768425177269,49.6920090955987,12.5697363248419));
#80541=CARTESIAN_POINT('Ctrl Pts',(89.1793072743075,49.6926392609403,12.5639931404312));
#80542=CARTESIAN_POINT('Ctrl Pts',(89.1866225910927,49.694549323352,12.5465943265912));
#80543=CARTESIAN_POINT('Ctrl Pts',(89.1913416025946,49.6958361342485,12.5348848916557));
#80544=CARTESIAN_POINT('Ctrl Pts',(89.2166700803913,49.7030520011094,12.4692300765583));
#80545=CARTESIAN_POINT('Ctrl Pts',(89.233753468218,49.7091209351502,12.4140043593033));
#80546=CARTESIAN_POINT('Ctrl Pts',(89.2582780324403,49.7203661131374,12.3101279387641));
#80547=CARTESIAN_POINT('Ctrl Pts',(89.2667683271879,49.7255303507395,12.2618249914497));
#80548=CARTESIAN_POINT('Ctrl Pts',(89.2768023995989,49.7345651663758,12.1758075580762));
#80549=CARTESIAN_POINT('Ctrl Pts',(89.2794986063008,49.7384533214004,12.1382864548802));
#80550=CARTESIAN_POINT('Ctrl Pts',(89.2808679774468,49.743574598978,12.0881821904661));
#80551=CARTESIAN_POINT('Ctrl Pts',(89.281024955551,49.7448484466321,12.0756627844987));
#80552=CARTESIAN_POINT('Ctrl Pts',(89.2809554966367,49.7479758956335,12.0447917202294));
#80553=CARTESIAN_POINT('Ctrl Pts',(89.2805164709481,49.7498228270648,12.0264427717425));
#80554=CARTESIAN_POINT('Ctrl Pts',(89.2792131731109,49.7526810803647,11.9978812628543));
#80555=CARTESIAN_POINT('Ctrl Pts',(89.2786228217866,49.7537006807676,11.9876596390929));
#80556=CARTESIAN_POINT('Ctrl Pts',(89.2772917453297,49.7555946032449,11.9686164517072));
#80557=CARTESIAN_POINT('Ctrl Pts',(89.2765822832286,49.7564698333374,11.9597934365416));
#80558=CARTESIAN_POINT('Ctrl Pts',(89.2747884997344,49.7584219338046,11.9400689662973));
#80559=CARTESIAN_POINT('Ctrl Pts',(89.2736552430741,49.7594972250645,11.9291725436642));
#80560=CARTESIAN_POINT('Ctrl Pts',(89.2703876841445,49.7622441576368,11.9012686428281));
#80561=CARTESIAN_POINT('Ctrl Pts',(89.268049767619,49.7639094681629,11.8842867470458));
#80562=CARTESIAN_POINT('Ctrl Pts',(89.251236965595,49.7742944310938,11.7781194541695));
#80563=CARTESIAN_POINT('Ctrl Pts',(89.2276228109176,49.7827121408086,11.6906398508275));
#80564=CARTESIAN_POINT('Ctrl Pts',(89.1771211686856,49.7957967287859,11.5605494805665));
#80565=CARTESIAN_POINT('Ctrl Pts',(89.1566764850031,49.800418142471,11.5157789811439));
#80566=CARTESIAN_POINT('Ctrl Pts',(89.1255005810498,49.8068177676603,11.4568240057862));
#80567=CARTESIAN_POINT('Ctrl Pts',(89.1169916844225,49.808510645063,11.4415088170721));
#80568=CARTESIAN_POINT('Ctrl Pts',(89.1017129321302,49.8114699739381,11.4153006511157));
#80569=CARTESIAN_POINT('Ctrl Pts',(89.0950895700466,49.8127288578755,11.4043247768336));
#80570=CARTESIAN_POINT('Ctrl Pts',(89.0850052107525,49.8146139431511,11.3881714403324));
#80571=CARTESIAN_POINT('Ctrl Pts',(89.0816700833126,49.8152324856734,11.3829155866702));
#80572=CARTESIAN_POINT('Ctrl Pts',(89.0756099051925,49.8163481584418,11.3735187200292));
#80573=CARTESIAN_POINT('Ctrl Pts',(89.0728990389651,49.816844362743,11.3693688195465));
#80574=CARTESIAN_POINT('Ctrl Pts',(89.0667387015753,49.8179656635505,11.3600578440382));
#80575=CARTESIAN_POINT('Ctrl Pts',(89.063275703445,49.8185916024393,11.3549062146613));
#80576=CARTESIAN_POINT('Ctrl Pts',(89.0525149978231,49.8205227854085,11.3391490906937));
#80577=CARTESIAN_POINT('Ctrl Pts',(89.0450940469585,49.8218354573217,11.3286295430065));
#80578=CARTESIAN_POINT('Ctrl Pts',(89.0009668713741,49.8295244803619,11.2680535275324));
#80579=CARTESIAN_POINT('Ctrl Pts',(88.9607943955332,49.8360640746927,11.2206352447754));
#80580=CARTESIAN_POINT('Ctrl Pts',(88.8664774014941,49.8502636790895,11.1245506705821));
#80581=CARTESIAN_POINT('Ctrl Pts',(88.8112764688783,49.8578970151876,11.0771980894698));
#80582=CARTESIAN_POINT('Ctrl Pts',(88.7248876936699,49.8688410286114,11.0150927181668));
#80583=CARTESIAN_POINT('Ctrl Pts',(88.696672564676,49.8722787828295,10.9964695262743));
#80584=CARTESIAN_POINT('Ctrl Pts',(88.6568307076361,49.8769567664032,10.9723980215661));
#80585=CARTESIAN_POINT('Ctrl Pts',(88.6458177159904,49.8782321354836,10.965968596664));
#80586=CARTESIAN_POINT('Ctrl Pts',(88.6268559678826,49.8803989406136,10.9552782961078));
#80587=CARTESIAN_POINT('Ctrl Pts',(88.6189555334498,49.8812933050731,10.9509343710858));
#80588=CARTESIAN_POINT('Ctrl Pts',(88.6038076589692,49.8829925504876,10.9428144210141));
#80589=CARTESIAN_POINT('Ctrl Pts',(88.5965687760746,49.8837979219343,10.9390235221062));
#80590=CARTESIAN_POINT('Ctrl Pts',(88.5795068212498,49.8856810675994,10.9302972090153));
#80591=CARTESIAN_POINT('Ctrl Pts',(88.5696551095875,49.8867568115958,10.9254188664166));
#80592=CARTESIAN_POINT('Ctrl Pts',(88.534802397185,49.8905238598128,10.9087205433447));
#80593=CARTESIAN_POINT('Ctrl Pts',(88.5094783147442,49.893191688466,10.8975889756812));
#80594=CARTESIAN_POINT('Ctrl Pts',(88.3979685283161,49.9046879380422,10.8528596554389));
#80595=CARTESIAN_POINT('Ctrl Pts',(88.3086236644899,49.9132397237372,10.8279064161989));
#80596=CARTESIAN_POINT('Ctrl Pts',(88.167010391284,49.9267384098283,10.8045864166829));
#80597=CARTESIAN_POINT('Ctrl Pts',(88.1162186372644,49.9315750897967,10.7993387370236));
#80598=CARTESIAN_POINT('Ctrl Pts',(88.0527885201105,49.9377692844856,10.7966263369692));
#80599=CARTESIAN_POINT('Ctrl Pts',(88.0403125399372,49.9389950426173,10.7962769953361));
#80600=CARTESIAN_POINT('Ctrl Pts',(88.0217112071195,49.9408365785735,10.7960304062589));
#80601=CARTESIAN_POINT('Ctrl Pts',(88.0155878327021,49.9414450493578,10.7959935256065));
#80602=CARTESIAN_POINT('Ctrl Pts',(88.0050119260407,49.9425002522374,10.7960063110774));
#80603=CARTESIAN_POINT('Ctrl Pts',(88.0005595153956,49.942945820831,10.7960351104507));
#80604=CARTESIAN_POINT('Ctrl Pts',(87.9900840314062,49.9439972945511,10.7961579595303));
#80605=CARTESIAN_POINT('Ctrl Pts',(87.9840615062244,49.944604227458,10.796271447286));
#80606=CARTESIAN_POINT('Ctrl Pts',(87.9665604181,49.9463745822525,10.7967257984163));
#80607=CARTESIAN_POINT('Ctrl Pts',(87.9550858795067,49.9475436195289,10.7971795032423));
#80608=CARTESIAN_POINT('Ctrl Pts',(87.8584984547107,49.9574463036794,10.8023112025123));
#80609=CARTESIAN_POINT('Ctrl Pts',(87.7740585656811,49.9664934828993,10.8153913956363));
#80610=CARTESIAN_POINT('Ctrl Pts',(87.6405645101739,49.9810035402672,10.8500825418811));
#80611=CARTESIAN_POINT('Ctrl Pts',(87.5904230273555,49.9865078328281,10.8665025304761));
#80612=CARTESIAN_POINT('Ctrl Pts',(87.5206497744989,49.9942259419302,10.8942673622174));
#80613=CARTESIAN_POINT('Ctrl Pts',(87.5000794495506,49.9965094760542,10.9030893997864));
#80614=CARTESIAN_POINT('Ctrl Pts',(87.463455266699,50.0005920438064,10.9199560862405));
#80615=CARTESIAN_POINT('Ctrl Pts',(87.4473189863176,50.0023969038322,10.9278059539436));
#80616=CARTESIAN_POINT('Ctrl Pts',(87.4223397919524,50.0052024371873,10.9406192723622));
#80617=CARTESIAN_POINT('Ctrl Pts',(87.4133815135729,50.006210979588,10.945350731677));
#80618=CARTESIAN_POINT('Ctrl Pts',(87.3967276717559,50.008090970631,10.9544032331983));
#80619=CARTESIAN_POINT('Ctrl Pts',(87.3890187607374,50.0089632692538,10.9586982285163));
#80620=CARTESIAN_POINT('Ctrl Pts',(87.3717963706809,50.010917253196,10.9685302441104));
#80621=CARTESIAN_POINT('Ctrl Pts',(87.3623087317852,50.0119972957776,10.9741113600636));
#80622=CARTESIAN_POINT('Ctrl Pts',(87.3380155570588,50.0147734747744,10.988830286705));
#80623=CARTESIAN_POINT('Ctrl Pts',(87.3233226328539,50.0164629915661,10.9981504980386));
#80624=CARTESIAN_POINT('Ctrl Pts',(87.2516525011199,50.0247683884528,11.0457063077488));
#80625=CARTESIAN_POINT('Ctrl Pts',(87.197643026823,50.0312240934094,11.0882165308644));
#80626=CARTESIAN_POINT('Ctrl Pts',(87.1001233262038,50.0436948393222,11.1786731864601));
#80627=CARTESIAN_POINT('Ctrl Pts',(87.0563226578107,50.0496958081879,11.2259792957401));
#80628=CARTESIAN_POINT('Ctrl Pts',(87.0069289657661,50.0572897765511,11.2882027357601));
#80629=CARTESIAN_POINT('Ctrl Pts',(86.997768409111,50.0587385520758,11.3001743568044));
#80630=CARTESIAN_POINT('Ctrl Pts',(86.978230636241,50.0619261235956,11.3266718945819));
#80631=CARTESIAN_POINT('Ctrl Pts',(86.9679426576656,50.0636687822992,11.3412587561351));
#80632=CARTESIAN_POINT('Ctrl Pts',(86.9540079240187,50.0661293241174,11.361927635367));
#80633=CARTESIAN_POINT('Ctrl Pts',(86.950098804876,50.0668312249718,11.367831833372));
#80634=CARTESIAN_POINT('Ctrl Pts',(86.9434870877152,50.0680391902686,11.3780016858574));
#80635=CARTESIAN_POINT('Ctrl Pts',(86.9407601780801,50.068543660943,11.3822513474958));
#80636=CARTESIAN_POINT('Ctrl Pts',(86.9350333616865,50.0696167182829,11.3912943116648));
#80637=CARTESIAN_POINT('Ctrl Pts',(86.9320401380705,50.0701856639433,11.3960913611524));
#80638=CARTESIAN_POINT('Ctrl Pts',(86.9238215641207,50.0717702159644,11.4094607105698));
#80639=CARTESIAN_POINT('Ctrl Pts',(86.9186658693362,50.0727899407057,11.4180749163416));
#80640=CARTESIAN_POINT('Ctrl Pts',(86.881935893481,50.0802405721036,11.4811283693055));
#80641=CARTESIAN_POINT('Ctrl Pts',(86.8543493269671,50.0868575860968,11.5377790442601));
#80642=CARTESIAN_POINT('Ctrl Pts',(86.812454297466,50.0987970659119,11.6430070212977));
#80643=CARTESIAN_POINT('Ctrl Pts',(86.7966277352883,50.1041052975822,11.690852657582));
#80644=CARTESIAN_POINT('Ctrl Pts',(86.7742169967274,50.1131970337355,11.7750985650213));
#80645=CARTESIAN_POINT('Ctrl Pts',(86.7663020745541,50.1170034884842,11.8110813444863));
#80646=CARTESIAN_POINT('Ctrl Pts',(86.7578398617064,50.1220240544275,11.8595016823623));
#80647=CARTESIAN_POINT('Ctrl Pts',(86.7558949005567,50.1232776581811,11.8716726906734));
#80648=CARTESIAN_POINT('Ctrl Pts',(86.7515286101213,50.1263611558463,11.9018044087611));
#80649=CARTESIAN_POINT('Ctrl Pts',(86.7493138483551,50.1281844627442,11.9197929007142));
#80650=CARTESIAN_POINT('Ctrl Pts',(86.7464594032621,50.1310111940452,11.9479310154748));
#80651=CARTESIAN_POINT('Ctrl Pts',(86.7455553657337,50.1320227075707,11.9580504798649));
#80652=CARTESIAN_POINT('Ctrl Pts',(86.7440943866172,50.1339041400774,11.9769620836901));
#80653=CARTESIAN_POINT('Ctrl Pts',(86.7435073097484,50.1347749421174,11.985751175705));
#80654=CARTESIAN_POINT('Ctrl Pts',(86.742396603616,50.1367202429151,12.0054612178035));
#80655=CARTESIAN_POINT('Ctrl Pts',(86.7419224490456,50.137793145599,12.0163843829065));
#80656=CARTESIAN_POINT('Ctrl Pts',(86.7409178801289,50.1410166907371,12.0493464034488));
#80657=CARTESIAN_POINT('Ctrl Pts',(86.7408201065641,50.1431539473633,12.0713952958311));
#80658=CARTESIAN_POINT('Ctrl Pts',(86.7434309180857,50.1547883986694,12.192215236219));
#80659=CARTESIAN_POINT('Ctrl Pts',(86.7570841460695,50.1639311885861,12.2904085065647));
#80660=CARTESIAN_POINT('Ctrl Pts',(86.7919085474611,50.1769266341357,12.4241437042271));
#80661=CARTESIAN_POINT('Ctrl Pts',(86.803598653043,50.1806504833118,12.4617678724369));
#80662=CARTESIAN_POINT('Ctrl Pts',(86.8247021576846,50.1866123166092,12.519989167242));
#80663=CARTESIAN_POINT('Ctrl Pts',(86.8329510883193,50.1888045104766,12.5409834460733));
#80664=CARTESIAN_POINT('Ctrl Pts',(86.8447618621988,50.1917859489306,12.5688399332129));
#80665=CARTESIAN_POINT('Ctrl Pts',(86.8478345370942,50.1925487627717,12.5759073321859));
#80666=CARTESIAN_POINT('Ctrl Pts',(86.8530678356417,50.1938277713648,12.5876508741064));
#80667=CARTESIAN_POINT('Ctrl Pts',(86.855193026749,50.194341867765,12.5923428253558));
#80668=CARTESIAN_POINT('Ctrl Pts',(86.859325052362,50.1953316563716,12.60131972009));
#80669=CARTESIAN_POINT('Ctrl Pts',(86.8613273941846,50.1958070430285,12.6056066015568));
#80670=CARTESIAN_POINT('Ctrl Pts',(86.8668669989379,50.1971105524673,12.6172957304816));
#80671=CARTESIAN_POINT('Ctrl Pts',(86.8704520023896,50.1979414377093,12.6246748237477));
#80672=CARTESIAN_POINT('Ctrl Pts',(86.8851175486864,50.2012891743505,12.6541317178038));
#80673=CARTESIAN_POINT('Ctrl Pts',(86.8967686881854,50.2038351105929,12.6759168182268));
#80674=CARTESIAN_POINT('Ctrl Pts',(86.945528234777,50.2140291023914,12.7610219413424));
#80675=CARTESIAN_POINT('Ctrl Pts',(86.9874592028914,50.2218137436217,12.8214132528099));
#80676=CARTESIAN_POINT('Ctrl Pts',(87.0652277460183,50.2345903651937,12.9149671626036));
#80677=CARTESIAN_POINT('Ctrl Pts',(87.0981821164097,50.2396193089436,12.9503048677441));
#80678=CARTESIAN_POINT('Ctrl Pts',(87.1484102351758,50.2467530109683,12.998356906835));
#80679=CARTESIAN_POINT('Ctrl Pts',(87.1641136814851,50.2489163345288,13.0126436505277));
#80680=CARTESIAN_POINT('Ctrl Pts',(87.1803269728098,50.2510849025526,13.0266676665082));
#80681=CARTESIAN_POINT('Ctrl Pts',(87.1804848873278,50.2511060179337,13.026804189832));
#80682=CARTESIAN_POINT('Ctrl Pts',(87.1806428354213,50.2511271317289,13.0269406741484));
#80683=CARTESIAN_POINT('',(89.2765936958547,49.5646,12.1717005062084));
#80684=CARTESIAN_POINT('Origin',(88.011,49.5646,12.066));
#80685=CARTESIAN_POINT('Ctrl Pts',(89.2765936958547,49.5645999999999,12.1717005062084));
#80686=CARTESIAN_POINT('Ctrl Pts',(89.2769323000493,49.5650046868909,12.1676462651325));
#80687=CARTESIAN_POINT('Ctrl Pts',(89.2772514280172,49.565408516634,12.1635903372669));
#80688=CARTESIAN_POINT('Ctrl Pts',(89.2779126985219,49.5662979343296,12.1546359137711));
#80689=CARTESIAN_POINT('Ctrl Pts',(89.2782459359607,49.5667831431295,12.1497367954486));
#80690=CARTESIAN_POINT('Ctrl Pts',(89.2792425199579,49.5683658484442,12.133713345017));
#80691=CARTESIAN_POINT('Ctrl Pts',(89.2797878903809,49.5694586556053,12.1225817908385));
#80692=CARTESIAN_POINT('Ctrl Pts',(89.2822519137991,49.5761806799657,12.0537650718098));
#80693=CARTESIAN_POINT('Ctrl Pts',(89.2803831184224,49.5816768845998,11.996004944591));
#80694=CARTESIAN_POINT('Ctrl Pts',(89.2687771479741,49.5926656596804,11.8809244195437));
#80695=CARTESIAN_POINT('Ctrl Pts',(89.2590269501668,49.5981458364218,11.8237510638077));
#80696=CARTESIAN_POINT('Ctrl Pts',(89.2374492555629,49.6069527026906,11.7345356591435));
#80697=CARTESIAN_POINT('Ctrl Pts',(89.2281776015839,49.6102236370538,11.7019605849923));
#80698=CARTESIAN_POINT('Ctrl Pts',(89.2142958350412,49.614570312701,11.6596843173648));
#80699=CARTESIAN_POINT('Ctrl Pts',(89.2108482338348,49.6156134279439,11.6496137588617));
#80700=CARTESIAN_POINT('Ctrl Pts',(89.20377286592,49.6176858602253,11.6297642152997));
#80701=CARTESIAN_POINT('Ctrl Pts',(89.2001504054557,49.6187149499584,11.6199842287395));
#80702=CARTESIAN_POINT('Ctrl Pts',(89.1928303632922,49.6207349684929,11.6009447504895));
#80703=CARTESIAN_POINT('Ctrl Pts',(89.1891433682059,49.6217255104158,11.5916819806983));
#80704=CARTESIAN_POINT('Ctrl Pts',(89.1808121183426,49.6239072545291,11.5714481557508));
#80705=CARTESIAN_POINT('Ctrl Pts',(89.1761218268057,49.6250998091589,11.5604972557697));
#80706=CARTESIAN_POINT('Ctrl Pts',(89.159600459255,49.6291845559768,11.5233750253254));
#80707=CARTESIAN_POINT('Ctrl Pts',(89.1470370362848,49.6320995648524,11.4975420805315));
#80708=CARTESIAN_POINT('Ctrl Pts',(89.0875690162719,49.6451333895115,11.3851223167385));
#80709=CARTESIAN_POINT('Ctrl Pts',(89.0315711283794,49.6555434747946,11.3037523224961));
#80710=CARTESIAN_POINT('Ctrl Pts',(88.9381047214701,49.6705770056107,11.1969371953824));
#80711=CARTESIAN_POINT('Ctrl Pts',(88.9077845422685,49.6751734267477,11.1656825692961));
#80712=CARTESIAN_POINT('Ctrl Pts',(88.8638279400527,49.6814238595994,11.124800196136));
#80713=CARTESIAN_POINT('Ctrl Pts',(88.851519825673,49.6831328581012,11.1137925287434));
#80714=CARTESIAN_POINT('Ctrl Pts',(88.8299400521271,49.6860554884921,11.0952374395651));
#80715=CARTESIAN_POINT('Ctrl Pts',(88.820770343694,49.6872753468725,11.0875753549224));
#80716=CARTESIAN_POINT('Ctrl Pts',(88.8075623427943,49.6890000720258,11.0768518453986));
#80717=CARTESIAN_POINT('Ctrl Pts',(88.8036122516282,49.6895118489977,11.0736837905623));
#80718=CARTESIAN_POINT('Ctrl Pts',(88.7956901350752,49.6905300833802,11.0674075773513));
#80719=CARTESIAN_POINT('Ctrl Pts',(88.7917183237476,49.6910365460048,11.064299277719));
#80720=CARTESIAN_POINT('Ctrl Pts',(88.7833942769881,49.692089442313,11.0578645504107));
#80721=CARTESIAN_POINT('Ctrl Pts',(88.7790388626329,49.6926355248832,11.0545424812232));
#80722=CARTESIAN_POINT('Ctrl Pts',(88.7668631370902,49.6941492085432,11.0453795092804));
#80723=CARTESIAN_POINT('Ctrl Pts',(88.758996442199,49.6951125394715,11.0396001690265));
#80724=CARTESIAN_POINT('Ctrl Pts',(88.7027752587467,49.7019010551538,10.9992865207747));
#80725=CARTESIAN_POINT('Ctrl Pts',(88.6521062282323,49.7075222453052,10.9680854424479));
#80726=CARTESIAN_POINT('Ctrl Pts',(88.5353566848549,49.7198880030529,10.907044717012));
#80727=CARTESIAN_POINT('Ctrl Pts',(88.4685450207078,49.7265937271633,10.8790799166231));
#80728=CARTESIAN_POINT('Ctrl Pts',(88.3625541117604,49.7371500013212,10.8450029978505));
#80729=CARTESIAN_POINT('Ctrl Pts',(88.3248630363222,49.7408871104389,10.8347756959694));
#80730=CARTESIAN_POINT('Ctrl Pts',(88.2740052622932,49.7459517859196,10.8234626382528));
#80731=CARTESIAN_POINT('Ctrl Pts',(88.2612032162937,49.7472284190329,10.8208216263615));
#80732=CARTESIAN_POINT('Ctrl Pts',(88.2397019262584,49.7493770455482,10.8167309484277));
#80733=CARTESIAN_POINT('Ctrl Pts',(88.2310239460632,49.7502454521437,10.8151733984029));
#80734=CARTESIAN_POINT('Ctrl Pts',(88.2138481733429,49.7519671286929,10.8122749019376));
#80735=CARTESIAN_POINT('Ctrl Pts',(88.2053515711777,49.752820209205,10.8109296991635));
#80736=CARTESIAN_POINT('Ctrl Pts',(88.1845611057612,49.7549115226841,10.807854273543));
#80737=CARTESIAN_POINT('Ctrl Pts',(88.1722546044664,49.7561527576014,10.8062178563233));
#80738=CARTESIAN_POINT('Ctrl Pts',(88.1291301060743,49.760515681839,10.8011257255669));
#80739=CARTESIAN_POINT('Ctrl Pts',(88.0982145124258,49.7636676128701,10.798618907008));
#80740=CARTESIAN_POINT('Ctrl Pts',(87.9655774587639,49.7773124396985,10.7927393429728));
#80741=CARTESIAN_POINT('Ctrl Pts',(87.8637565256329,49.7881363221284,10.8004697136525));
#80742=CARTESIAN_POINT('Ctrl Pts',(87.7319622453892,49.8023197095386,10.8266037199878));
#80743=CARTESIAN_POINT('Ctrl Pts',(87.7002014977306,49.8057471915974,10.8341843042755));
#80744=CARTESIAN_POINT('Ctrl Pts',(87.6496795407766,49.8111852152096,10.8483217522422));
#80745=CARTESIAN_POINT('Ctrl Pts',(87.6307193950464,49.8132226659892,10.854109075081));
#80746=CARTESIAN_POINT('Ctrl Pts',(87.6051532890732,49.8159588637391,10.8625719954764));
#80747=CARTESIAN_POINT('Ctrl Pts',(87.5984245293166,49.8166779403467,10.8648622039702));
#80748=CARTESIAN_POINT('Ctrl Pts',(87.5870617769268,49.8178900281601,10.868836400174));
#80749=CARTESIAN_POINT('Ctrl Pts',(87.5824181004758,49.8183847211985,10.8704909621451));
#80750=CARTESIAN_POINT('Ctrl Pts',(87.5726900960301,49.8194197803,10.8740210609205));
#80751=CARTESIAN_POINT('Ctrl Pts',(87.5676080355378,49.8199598005803,10.8759021329875));
#80752=CARTESIAN_POINT('Ctrl Pts',(87.5541286333398,49.8213906505748,10.8809897275288));
#80753=CARTESIAN_POINT('Ctrl Pts',(87.545752762003,49.8222782288989,10.8842530659663));
#80754=CARTESIAN_POINT('Ctrl Pts',(87.5070460980611,49.8263761616861,10.8998089896386));
#80755=CARTESIAN_POINT('Ctrl Pts',(87.4771591065237,49.8295296518795,10.913183660978));
#80756=CARTESIAN_POINT('Ctrl Pts',(87.38702977778,49.8391125782347,10.9577757674378));
#80757=CARTESIAN_POINT('Ctrl Pts',(87.3287432147873,49.8454182479325,10.9926748033746));
#80758=CARTESIAN_POINT('Ctrl Pts',(87.2215263468942,49.8577704798631,11.0691500172164));
#80759=CARTESIAN_POINT('Ctrl Pts',(87.17241272399,49.8637929224047,11.1100983730446));
#80760=CARTESIAN_POINT('Ctrl Pts',(87.1130599642401,49.8717831167394,11.1676909324373));
#80761=CARTESIAN_POINT('Ctrl Pts',(87.099823689606,49.873615909198,11.1811197073028));
#80762=CARTESIAN_POINT('Ctrl Pts',(87.0797676074864,49.8764782507339,11.2023947067934));
#80763=CARTESIAN_POINT('Ctrl Pts',(87.0727364437849,49.8774987776753,11.210038929206));
#80764=CARTESIAN_POINT('Ctrl Pts',(87.0598490037513,49.8794021763518,11.2243996359065));
#80765=CARTESIAN_POINT('Ctrl Pts',(87.0539680795527,49.8802839542825,11.2310932485596));
#80766=CARTESIAN_POINT('Ctrl Pts',(87.0410212097189,49.8822554486975,11.2461457827901));
#80767=CARTESIAN_POINT('Ctrl Pts',(87.0339920173032,49.8833465675926,11.2545351678547));
#80768=CARTESIAN_POINT('Ctrl Pts',(87.0163349803454,49.8861420245164,11.2761709702983));
#80769=CARTESIAN_POINT('Ctrl Pts',(87.0058632180014,49.8878522817962,11.2895411300496));
#80770=CARTESIAN_POINT('Ctrl Pts',(86.9436470725428,49.8983465691198,11.3723458184373));
#80771=CARTESIAN_POINT('Ctrl Pts',(86.8988594413864,49.9073829336367,11.4466978875224));
#80772=CARTESIAN_POINT('Ctrl Pts',(86.8412933146105,49.921594676046,11.5689621292214));
#80773=CARTESIAN_POINT('Ctrl Pts',(86.8231357400698,49.9267083943839,11.6140714077037));
#80774=CARTESIAN_POINT('Ctrl Pts',(86.8020477176019,49.9335591036386,11.6765941462585));
#80775=CARTESIAN_POINT('Ctrl Pts',(86.7968275469791,49.9353553051812,11.6931892194839));
#80776=CARTESIAN_POINT('Ctrl Pts',(86.7883669080754,49.9384469312673,11.7221518154864));
#80777=CARTESIAN_POINT('Ctrl Pts',(86.7849692360516,49.939748526432,11.7344704220278));
#80778=CARTESIAN_POINT('Ctrl Pts',(86.7801776564371,49.9416767465736,11.7529250953683));
#80779=CARTESIAN_POINT('Ctrl Pts',(86.7786426253116,49.9423103754458,11.7590230556088));
#80780=CARTESIAN_POINT('Ctrl Pts',(86.7759570545057,49.9434481646863,11.7700364838419));
#80781=CARTESIAN_POINT('Ctrl Pts',(86.7747904528073,49.943953163568,11.7749477033214));
#80782=CARTESIAN_POINT('Ctrl Pts',(86.772212475991,49.9450940953002,11.7860958104379));
#80783=CARTESIAN_POINT('Ctrl Pts',(86.7708188743494,49.9457290402113,11.7923365808807));
#80784=CARTESIAN_POINT('Ctrl Pts',(86.7666112371446,49.9477056514021,11.8118715861533));
#80785=CARTESIAN_POINT('Ctrl Pts',(86.7639632290181,49.9490386622054,11.8252013507172));
#80786=CARTESIAN_POINT('Ctrl Pts',(86.7444921589084,49.9596305486429,11.9321737957046));
#80787=CARTESIAN_POINT('Ctrl Pts',(86.7380234189308,49.9684302105805,12.0274116063342));
#80788=CARTESIAN_POINT('Ctrl Pts',(86.7449602574838,49.9830791329554,12.1832013170017));
#80789=CARTESIAN_POINT('Ctrl Pts',(86.7520166093667,49.9888219618752,12.2436282975283));
#80790=CARTESIAN_POINT('Ctrl Pts',(86.7667991746953,49.9964713448086,12.321345425353));
#80791=CARTESIAN_POINT('Ctrl Pts',(86.7706197367687,49.9982569606994,12.3393014844075));
#80792=CARTESIAN_POINT('Ctrl Pts',(86.777175719583,50.001057743096,12.3671353822076));
#80793=CARTESIAN_POINT('Ctrl Pts',(86.7796439706478,50.0020644326792,12.3770742471473));
#80794=CARTESIAN_POINT('Ctrl Pts',(86.7844696811376,50.0039486620166,12.395547811436));
#80795=CARTESIAN_POINT('Ctrl Pts',(86.7867967480551,50.0048251770037,12.4040898859954));
#80796=CARTESIAN_POINT('Ctrl Pts',(86.7922034086236,50.0067930955415,12.4231483434946));
#80797=CARTESIAN_POINT('Ctrl Pts',(86.7953301427021,50.0078859600801,12.4336504443208));
#80798=CARTESIAN_POINT('Ctrl Pts',(86.8036969718199,50.010700414025,12.4604786129577));
#80799=CARTESIAN_POINT('Ctrl Pts',(86.8091323121346,50.0124281786764,12.4767407521832));
#80800=CARTESIAN_POINT('Ctrl Pts',(86.8452534301501,50.0233246196986,12.5779494240839));
#80801=CARTESIAN_POINT('Ctrl Pts',(86.8845919924673,50.0327740382255,12.6595103748224));
#80802=CARTESIAN_POINT('Ctrl Pts',(86.9581998254973,50.0474828835358,12.7779925928973));
#80803=CARTESIAN_POINT('Ctrl Pts',(86.986577962565,50.0526752123085,12.8182511529358));
#80804=CARTESIAN_POINT('Ctrl Pts',(87.0281349537844,50.0596163826883,12.8704771215578));
#80805=CARTESIAN_POINT('Ctrl Pts',(87.0393305894005,50.0614287681075,12.8839644145795));
#80806=CARTESIAN_POINT('Ctrl Pts',(87.0591952191831,50.0645420993583,12.9069114614065));
#80807=CARTESIAN_POINT('Ctrl Pts',(87.0677347606364,50.0658495787102,12.9164793709917));
#80808=CARTESIAN_POINT('Ctrl Pts',(87.0806340466589,50.0677775640108,12.9304986739871));
#80809=CARTESIAN_POINT('Ctrl Pts',(87.0848835456706,50.0684053772195,12.9350495287782));
#80810=CARTESIAN_POINT('Ctrl Pts',(87.0925767687912,50.0695286145152,12.9431677996641));
#80811=CARTESIAN_POINT('Ctrl Pts',(87.0960080982478,50.0700249054027,12.9467465036873));
#80812=CARTESIAN_POINT('Ctrl Pts',(87.1037832604899,50.0711389669835,12.9547611198974));
#80813=CARTESIAN_POINT('Ctrl Pts',(87.1081387736843,50.0717558231018,12.9591853966009));
#80814=CARTESIAN_POINT('Ctrl Pts',(87.1216251817373,50.0736445564625,12.9726852605607));
#80815=CARTESIAN_POINT('Ctrl Pts',(87.1308622393573,50.0749086055255,12.9816545737792));
#80816=CARTESIAN_POINT('Ctrl Pts',(87.1534450821938,50.0779338965543,13.0029252358484));
#80817=CARTESIAN_POINT('Ctrl Pts',(87.1669176652258,50.0796858746954,13.0150806361318));
#80818=CARTESIAN_POINT('Ctrl Pts',(87.1806428554372,50.081424866233,13.0269406914443));
#80819=CARTESIAN_POINT('Origin',(88.011,49.5646,12.066));
#80820=CARTESIAN_POINT('',(87.4793792431904,49.5646,10.446693294484));
#80821=CARTESIAN_POINT('',(86.30666,49.5646,12.066));
#80822=CARTESIAN_POINT('Origin',(88.011,49.5646,12.066));
#80823=CARTESIAN_POINT('Ctrl Pts',(87.4793792431904,49.5646000000001,10.446693294484));
#80824=CARTESIAN_POINT('Ctrl Pts',(87.5432134943017,49.5646000000001,10.4346997308512));
#80825=CARTESIAN_POINT('Ctrl Pts',(87.607765068069,49.5646000000001,10.4266992315549));
#80826=CARTESIAN_POINT('Ctrl Pts',(87.6726821165043,49.5646000000001,10.422592732542));
#80827=CARTESIAN_POINT('Ctrl Pts',(87.7301000591824,49.5646,10.4189606092306));
#80828=CARTESIAN_POINT('Ctrl Pts',(87.7878044036963,49.5646000000001,10.4183758163793));
#80829=CARTESIAN_POINT('Ctrl Pts',(87.8455396127937,49.5646000000001,10.4208015589989));
#80830=CARTESIAN_POINT('Ctrl Pts',(87.8597334500476,49.5646000000001,10.4213979125326));
#80831=CARTESIAN_POINT('Ctrl Pts',(87.8739193815678,49.5646,10.4221759525792));
#80832=CARTESIAN_POINT('Ctrl Pts',(87.888092217474,49.5646,10.4231345189642));
#80833=CARTESIAN_POINT('Ctrl Pts',(87.9516421369536,49.5646,10.4274326578117));
#80834=CARTESIAN_POINT('Ctrl Pts',(88.0149405906727,49.5646,10.4353571812218));
#80835=CARTESIAN_POINT('Ctrl Pts',(88.0776421524961,49.5646,10.446837972588));
#80836=CARTESIAN_POINT('Ctrl Pts',(88.1194110731014,49.5646,10.4544859521457));
#80837=CARTESIAN_POINT('Ctrl Pts',(88.1609147379759,49.5646,10.4637130627391));
#80838=CARTESIAN_POINT('Ctrl Pts',(88.2020432503533,49.5646,10.4745089165249));
#80839=CARTESIAN_POINT('Ctrl Pts',(88.217204017084,49.5646,10.4784884774535));
#80840=CARTESIAN_POINT('Ctrl Pts',(88.2323177970543,49.5646,10.482682610884));
#80841=CARTESIAN_POINT('Ctrl Pts',(88.2473520841595,49.5646,10.487082783089));
#80842=CARTESIAN_POINT('Ctrl Pts',(88.3060841492863,49.5646,10.5042722380133));
#80843=CARTESIAN_POINT('Ctrl Pts',(88.3636811048161,49.5646,10.5246207416929));
#80844=CARTESIAN_POINT('Ctrl Pts',(88.4198383627968,49.5646,10.5480572671525));
#80845=CARTESIAN_POINT('Ctrl Pts',(88.4751444718139,49.5646,10.5711385762949));
#80846=CARTESIAN_POINT('Ctrl Pts',(88.5290549999893,49.5646,10.5972155885462));
#80847=CARTESIAN_POINT('Ctrl Pts',(88.5812452068814,49.5646,10.6262565481873));
#80848=CARTESIAN_POINT('Ctrl Pts',(88.6126791782889,49.5646,10.6437478123414));
#80849=CARTESIAN_POINT('Ctrl Pts',(88.6434883754159,49.5646,10.662314937626));
#80850=CARTESIAN_POINT('Ctrl Pts',(88.6735939944165,49.5646,10.6819561549177));
#80851=CARTESIAN_POINT('Ctrl Pts',(88.6985873415264,49.5646,10.6982620731393));
#80852=CARTESIAN_POINT('Ctrl Pts',(88.7230956814319,49.5646,10.7153083477659));
#80853=CARTESIAN_POINT('Ctrl Pts',(88.7470702501294,49.5646,10.7330956630536));
#80854=CARTESIAN_POINT('Ctrl Pts',(88.7576802894461,49.5646,10.7409675091303));
#80855=CARTESIAN_POINT('Ctrl Pts',(88.7681881486854,49.5646,10.7489865796549));
#80856=CARTESIAN_POINT('Ctrl Pts',(88.7785699894182,49.5646,10.7571372605137));
#80857=CARTESIAN_POINT('Ctrl Pts',(88.8233248591948,49.5646,10.7922738677701));
#80858=CARTESIAN_POINT('Ctrl Pts',(88.8658175386404,49.5646,10.8299084505779));
#80859=CARTESIAN_POINT('Ctrl Pts',(88.9057642508585,49.5646,10.8700060633041));
#80860=CARTESIAN_POINT('Ctrl Pts',(88.9108943848685,49.5646,10.8751555766269));
#80861=CARTESIAN_POINT('Ctrl Pts',(88.9159824695673,49.5646,10.8803457510599));
#80862=CARTESIAN_POINT('Ctrl Pts',(88.9210278497657,49.5646,10.885576545595));
#80863=CARTESIAN_POINT('Ctrl Pts',(88.961402604043,49.5646,10.9274350450001));
#80864=CARTESIAN_POINT('Ctrl Pts',(88.9990468409029,49.5646,10.9718936611491));
#80865=CARTESIAN_POINT('Ctrl Pts',(89.0338429995909,49.5646,11.0186424351575));
#80866=CARTESIAN_POINT('Ctrl Pts',(89.0640183489715,49.5646,11.059183133959));
#80867=CARTESIAN_POINT('Ctrl Pts',(89.0920511066818,49.5646,11.1014469418056));
#80868=CARTESIAN_POINT('Ctrl Pts',(89.1178329221646,49.5646,11.1452333647597));
#80869=CARTESIAN_POINT('Ctrl Pts',(89.1229657557734,49.5646,11.1539506881576));
#80870=CARTESIAN_POINT('Ctrl Pts',(89.1280104794418,49.5646,11.1627305054241));
#80871=CARTESIAN_POINT('Ctrl Pts',(89.1329621268224,49.5646,11.1715640955915));
#80872=CARTESIAN_POINT('Ctrl Pts',(89.1604471489843,49.5646,11.2205965494101));
#80873=CARTESIAN_POINT('Ctrl Pts',(89.1849976183063,49.5646,11.2711543804104));
#80874=CARTESIAN_POINT('Ctrl Pts',(89.206531164753,49.5646,11.3229450829069));
#80875=CARTESIAN_POINT('Ctrl Pts',(89.2278894852167,49.5646,11.3743143463813));
#80876=CARTESIAN_POINT('Ctrl Pts',(89.2462797865637,49.5646,11.4268976855764));
#80877=CARTESIAN_POINT('Ctrl Pts',(89.2615710260204,49.5646,11.4804105356582));
#80878=CARTESIAN_POINT('Ctrl Pts',(89.2765031578003,49.5646,11.5326666612395));
#80879=CARTESIAN_POINT('Ctrl Pts',(89.2884799242348,49.5646,11.5858101238446));
#80880=CARTESIAN_POINT('Ctrl Pts',(89.2973320937201,49.5646,11.6395609907597));
#80881=CARTESIAN_POINT('Ctrl Pts',(89.2991414178106,49.5646,11.6505473075663));
#80882=CARTESIAN_POINT('Ctrl Pts',(89.3008200504352,49.5646,11.6615589214129));
#80883=CARTESIAN_POINT('Ctrl Pts',(89.3023663054708,49.5646,11.672593307726));
#80884=CARTESIAN_POINT('Ctrl Pts',(89.3036790583404,49.5646,11.6819613757116));
#80885=CARTESIAN_POINT('Ctrl Pts',(89.3048950581329,49.5646,11.6913363184933));
#80886=CARTESIAN_POINT('Ctrl Pts',(89.3060138301966,49.5646,11.700716616931));
#80887=CARTESIAN_POINT('Ctrl Pts',(89.3122581336349,49.5646,11.7530717227543));
#80888=CARTESIAN_POINT('Ctrl Pts',(89.3154777290993,49.5646,11.8055958073229));
#80889=CARTESIAN_POINT('Ctrl Pts',(89.3155636653537,49.5646,11.8580373686408));
#80890=CARTESIAN_POINT('Ctrl Pts',(89.3156502223929,49.5646,11.9108577563898));
#80891=CARTESIAN_POINT('Ctrl Pts',(89.3125576884502,49.5646,11.9635954633224));
#80892=CARTESIAN_POINT('Ctrl Pts',(89.3061247018758,49.5646,12.0159713836245));
#80893=CARTESIAN_POINT('Ctrl Pts',(89.3000447623628,49.5646,12.0654728746809));
#80894=CARTESIAN_POINT('Ctrl Pts',(89.2909804830363,49.5646,12.1146517005517));
#80895=CARTESIAN_POINT('Ctrl Pts',(89.2787553837174,49.5646,12.1632419914215));
#80896=CARTESIAN_POINT('Ctrl Pts',(89.2780455024135,49.5646,12.1660635095243));
#80897=CARTESIAN_POINT('Ctrl Pts',(89.2773249526241,49.5645999999999,12.1688830330924));
#80898=CARTESIAN_POINT('Ctrl Pts',(89.2765936958546,49.5646,12.1717005062084));
#80899=CARTESIAN_POINT('',(88.1950623699338,49.5639392675618,13.3237488200268));
#80900=CARTESIAN_POINT('Ctrl Pts',(88.2080236424798,49.5646,13.3206241207246));
#80901=CARTESIAN_POINT('Ctrl Pts',(88.2036514348987,49.5643797558539,13.3213107233884));
#80902=CARTESIAN_POINT('Ctrl Pts',(88.1992756381996,49.5641595117079,13.3219744709519));
#80903=CARTESIAN_POINT('Ctrl Pts',(88.1948964915141,49.5639392675618,13.3226153271422));
#80904=CARTESIAN_POINT('Ctrl Pts',(88.1951651089274,49.5646,13.3249038896975));
#80905=CARTESIAN_POINT('Ctrl Pts',(88.147583815449,49.5646,13.3404287431933));
#80906=CARTESIAN_POINT('Ctrl Pts',(88.0990977222012,49.5646,13.3528110980375));
#80907=CARTESIAN_POINT('Ctrl Pts',(88.0499901030814,49.5646,13.3622015070427));
#80908=CARTESIAN_POINT('Ctrl Pts',(88.0131050869839,49.5646,13.3692546974341));
#80909=CARTESIAN_POINT('Ctrl Pts',(87.9758684960568,49.5646,13.3746192028678));
#80910=CARTESIAN_POINT('Ctrl Pts',(87.9383887371113,49.5646,13.3783443583316));
#80911=CARTESIAN_POINT('Ctrl Pts',(87.9251861406984,49.5646,13.3796565792623));
#80912=CARTESIAN_POINT('Ctrl Pts',(87.9119513363239,49.5646,13.3807653943206));
#80913=CARTESIAN_POINT('Ctrl Pts',(87.8986950683556,49.5646,13.3816721668229));
#80914=CARTESIAN_POINT('Ctrl Pts',(87.8455772117481,49.5646,13.3853056036145));
#80915=CARTESIAN_POINT('Ctrl Pts',(87.7922338268483,49.5646,13.3856915703243));
#80916=CARTESIAN_POINT('Ctrl Pts',(87.7389685900434,49.5646,13.3829815726137));
#80917=CARTESIAN_POINT('Ctrl Pts',(87.7008670109547,49.5646,13.3810430626531));
#80918=CARTESIAN_POINT('Ctrl Pts',(87.662804589928,49.5646,13.3775194839648));
#80919=CARTESIAN_POINT('Ctrl Pts',(87.6248847851905,49.5646,13.3724519617938));
#80920=CARTESIAN_POINT('Ctrl Pts',(87.612841961819,49.5646,13.370842584455));
#80921=CARTESIAN_POINT('Ctrl Pts',(87.6008115951672,49.5646,13.3690770863748));
#80922=CARTESIAN_POINT('Ctrl Pts',(87.5888029110002,49.5646,13.3671574954402));
#80923=CARTESIAN_POINT('Ctrl Pts',(87.5342255989436,49.5646,13.3584332995169));
#80924=CARTESIAN_POINT('Ctrl Pts',(87.480254606079,49.5646,13.3465559506408));
#80925=CARTESIAN_POINT('Ctrl Pts',(87.4271969284901,49.5646,13.3316854838884));
#80926=CARTESIAN_POINT('Ctrl Pts',(87.3725247345629,49.5646,13.3163625169019));
#80927=CARTESIAN_POINT('Ctrl Pts',(87.318821216024,49.5646,13.2978617600648));
#80928=CARTESIAN_POINT('Ctrl Pts',(87.2664029391945,49.5646,13.2763069116344));
#80929=CARTESIAN_POINT('Ctrl Pts',(87.2141247648759,49.5646,13.2548096745673));
#80930=CARTESIAN_POINT('Ctrl Pts',(87.1631237126695,49.5646,13.2302745990502));
#80931=CARTESIAN_POINT('Ctrl Pts',(87.1137126784811,49.5646,13.2027729015126));
#80932=CARTESIAN_POINT('Ctrl Pts',(87.1044241328058,49.5646,13.1976029879918));
#80933=CARTESIAN_POINT('Ctrl Pts',(87.095191804154,49.5646,13.1923280933648));
#80934=CARTESIAN_POINT('Ctrl Pts',(87.0860178237703,49.5646,13.1869484894039));
#80935=CARTESIAN_POINT('Ctrl Pts',(87.0776898390854,49.5646,13.1820649756483));
#80936=CARTESIAN_POINT('Ctrl Pts',(87.0694132039564,49.5646,13.1770970225026));
#80937=CARTESIAN_POINT('Ctrl Pts',(87.0611963948787,49.5646,13.1720494758806));
#80938=CARTESIAN_POINT('Ctrl Pts',(87.0109104049247,49.5646,13.1411590321176));
#80939=CARTESIAN_POINT('Ctrl Pts',(86.9627871139725,49.5646,13.107246058951));
#80940=CARTESIAN_POINT('Ctrl Pts',(86.9171559545492,49.5646,13.0704523153941));
#80941=CARTESIAN_POINT('Ctrl Pts',(86.9114896833008,49.5646,13.0658834345269));
#80942=CARTESIAN_POINT('Ctrl Pts',(86.9058618367084,49.5646,13.0612700676731));
#80943=CARTESIAN_POINT('Ctrl Pts',(86.9002730461311,49.5646,13.0566124305091));
#80944=CARTESIAN_POINT('Ctrl Pts',(86.8568625806386,49.5646,13.0204346216277));
#80945=CARTESIAN_POINT('Ctrl Pts',(86.8158067936454,49.5646,12.9815899007508));
#80946=CARTESIAN_POINT('Ctrl Pts',(86.7771379528804,49.5646,12.9403791635712));
#80947=CARTESIAN_POINT('Ctrl Pts',(86.7561113369255,49.5646,12.9179703629257));
#80948=CARTESIAN_POINT('Ctrl Pts',(86.7357908280484,49.5646,12.8948611228301));
#80949=CARTESIAN_POINT('Ctrl Pts',(86.7161845486795,49.5646,12.871094260736));
#80950=CARTESIAN_POINT('Ctrl Pts',(86.7018051845722,49.5646,12.8536635000441));
#80951=CARTESIAN_POINT('Ctrl Pts',(86.6878100364862,49.5646,12.8358789337154));
#80952=CARTESIAN_POINT('Ctrl Pts',(86.6742031561875,49.5646,12.8177563007364));
#80953=CARTESIAN_POINT('Ctrl Pts',(86.6653701582013,49.5646,12.8059918714849));
#80954=CARTESIAN_POINT('Ctrl Pts',(86.6566978401993,49.5646,12.7940805137582));
#80955=CARTESIAN_POINT('Ctrl Pts',(86.6482054177523,49.5646,12.7820525218999));
#80956=CARTESIAN_POINT('Ctrl Pts',(86.6133892636089,49.5646,12.7327416896628));
#80957=CARTESIAN_POINT('Ctrl Pts',(86.5815409247293,49.5646,12.6814071691517));
#80958=CARTESIAN_POINT('Ctrl Pts',(86.5526856719227,49.5646,12.6284074774605));
#80959=CARTESIAN_POINT('Ctrl Pts',(86.523830419116,49.5646,12.5754077857694));
#80960=CARTESIAN_POINT('Ctrl Pts',(86.4979677303733,49.5646,12.5207421219677));
#80961=CARTESIAN_POINT('Ctrl Pts',(86.475150702407,49.5646,12.4647232688012));
#80962=CARTESIAN_POINT('Ctrl Pts',(86.451851227582,49.5646,12.4075199441172));
#80963=CARTESIAN_POINT('Ctrl Pts',(86.431726870377,49.5646,12.3489048167329));
#80964=CARTESIAN_POINT('Ctrl Pts',(86.4148726192312,49.5646,12.2891750718329));
#80965=CARTESIAN_POINT('Ctrl Pts',(86.4116417237766,49.5646,12.2777251082816));
#80966=CARTESIAN_POINT('Ctrl Pts',(86.4085311259145,49.5646,12.2662341026577));
#80967=CARTESIAN_POINT('Ctrl Pts',(86.4055416858706,49.5646,12.2547040415001));
#80968=CARTESIAN_POINT('Ctrl Pts',(86.4025231478382,49.5646,12.2430617514366));
#80969=CARTESIAN_POINT('Ctrl Pts',(86.3996302010096,49.5646,12.2313873791669));
#80970=CARTESIAN_POINT('Ctrl Pts',(86.3968649172368,49.5646,12.2196906431064));
#80971=CARTESIAN_POINT('Ctrl Pts',(86.3820925664019,49.5646,12.1572058122891));
#80972=CARTESIAN_POINT('Ctrl Pts',(86.3709436194787,49.5646,12.0940211401315));
#80973=CARTESIAN_POINT('Ctrl Pts',(86.3634668315128,49.5646,12.0304891040359));
#80974=CARTESIAN_POINT('Ctrl Pts',(86.3559769727694,49.5646,11.9668460024514));
#80975=CARTESIAN_POINT('Ctrl Pts',(86.3521715596108,49.5646,11.9028533267291));
#80976=CARTESIAN_POINT('Ctrl Pts',(86.3521409187914,49.5646,11.8388343782705));
#80977=CARTESIAN_POINT('Ctrl Pts',(86.3521105495977,49.5646,11.7753829468404));
#80978=CARTESIAN_POINT('Ctrl Pts',(86.3557878467311,49.5646,11.7119046684883));
#80979=CARTESIAN_POINT('Ctrl Pts',(86.3633089374713,49.5646,11.6486990891005));
#80980=CARTESIAN_POINT('Ctrl Pts',(86.364728299535,49.5646,11.6367710849457));
#80981=CARTESIAN_POINT('Ctrl Pts',(86.3662847067316,49.5646,11.6248527747873));
#80982=CARTESIAN_POINT('Ctrl Pts',(86.3679792906019,49.5646,11.6129461576272));
#80983=CARTESIAN_POINT('Origin',(88.011,49.5646,12.066));
#80984=CARTESIAN_POINT('Ctrl Pts',(87.4195227899263,65.1917000946238,13.1872458288696));
#80985=CARTESIAN_POINT('Ctrl Pts',(87.046706091828,65.1496953464628,12.9905783588265));
#80986=CARTESIAN_POINT('Ctrl Pts',(86.5192450187475,65.0656858501406,12.1991954050947));
#80987=CARTESIAN_POINT('Ctrl Pts',(87.0905702611622,64.9396716056574,10.8825794754981));
#80988=CARTESIAN_POINT('Ctrl Pts',(88.5057114362722,64.8136573611742,10.652019091688));
#80989=CARTESIAN_POINT('Ctrl Pts',(89.4673758848142,64.6876431166909,11.7140895996939));
#80990=CARTESIAN_POINT('Ctrl Pts',(89.0965192186417,64.5616288722077,13.0989494595771));
#80991=CARTESIAN_POINT('Ctrl Pts',(87.7320138686435,64.4356146277245,13.5380917202516));
#80992=CARTESIAN_POINT('Ctrl Pts',(86.6229267036533,64.3096003832413,12.63015179099));
#80993=CARTESIAN_POINT('Ctrl Pts',(86.7841629682104,64.1835861387581,11.2058088685007));
#80994=CARTESIAN_POINT('Ctrl Pts',(88.0682258576584,64.0575718942748,10.5687599281523));
#80995=CARTESIAN_POINT('Ctrl Pts',(89.2999043335523,63.9315576497916,11.3019663445296));
#80996=CARTESIAN_POINT('Ctrl Pts',(89.351979957255,63.8055434053084,12.7344294808954));
#80997=CARTESIAN_POINT('Ctrl Pts',(88.1767846159536,63.6795291608251,13.5551386896109));
#80998=CARTESIAN_POINT('Ctrl Pts',(86.8498641790876,63.553514916342,13.0129872916757));
#80999=CARTESIAN_POINT('Ctrl Pts',(86.5856174206176,63.4275006718586,11.6041493789204));
#81000=CARTESIAN_POINT('Ctrl Pts',(87.6258846736599,63.3014864273755,10.6179989983799));
#81001=CARTESIAN_POINT('Ctrl Pts',(89.0186102518103,63.1754721828922,10.9570623661457));
#81002=CARTESIAN_POINT('Ctrl Pts',(89.4891685219261,63.0494579384091,12.3110283750348));
#81003=CARTESIAN_POINT('Ctrl Pts',(88.6069032604118,62.9234436939258,13.4407437213165));
#81004=CARTESIAN_POINT('Ctrl Pts',(87.1792658825502,62.7974294494426,13.3122902566958));
#81005=CARTESIAN_POINT('Ctrl Pts',(86.5128336157025,62.6714152049593,12.0432288440844));
#81006=CARTESIAN_POINT('Ctrl Pts',(87.2175269354857,62.5454009604761,10.7950076606443));
#81007=CARTESIAN_POINT('Ctrl Pts',(88.6484087641475,62.4193867159929,10.7100018049911));
#81008=CARTESIAN_POINT('Ctrl Pts',(89.4959325163499,62.2933724715096,11.8660088547187));
#81009=CARTESIAN_POINT('Ctrl Pts',(88.9844423553679,62.1673582270265,13.2050482939942));
#81010=CARTESIAN_POINT('Ctrl Pts',(87.5820553429153,62.0413439825432,13.5016279174233));
#81011=CARTESIAN_POINT('Ctrl Pts',(86.5722395416138,61.91532973806,12.4843173189171));
#81012=CARTESIAN_POINT('Ctrl Pts',(86.8791808712292,61.7893154935768,11.0841616754428));
#81013=CARTESIAN_POINT('Ctrl Pts',(88.2219658674358,61.6633012490936,10.5825868954658));
#81014=CARTESIAN_POINT('Ctrl Pts',(89.3716743798821,61.5372870046104,11.4386354585839));
#81015=CARTESIAN_POINT('Ctrl Pts',(89.2760903337081,61.411272760127,12.8688496020078));
#81016=CARTESIAN_POINT('Ctrl Pts',(88.0226924844505,61.2852585156439,13.5642938035331));
#81017=CARTESIAN_POINT('Ctrl Pts',(86.7585936444956,61.1592442711607,12.8884958094639));
#81018=CARTESIAN_POINT('Ctrl Pts',(86.6407001993997,61.0332300266774,11.4599476158219));
#81019=CARTESIAN_POINT('Ctrl Pts',(87.7769085217668,60.9072157821942,10.5860600634779));
#81020=CARTESIAN_POINT('Ctrl Pts',(89.1273579441268,60.7812015377109,11.06661720223));
#81021=CARTESIAN_POINT('Ctrl Pts',(89.4561138142887,60.6551872932278,12.4618119498517));
#81022=CARTESIAN_POINT('Ctrl Pts',(88.4622979465789,60.5291730487445,13.4947586217789));
#81023=CARTESIAN_POINT('Ctrl Pts',(87.0554530817039,60.4031588042614,13.2201018684798));
#81024=CARTESIAN_POINT('Ctrl Pts',(86.5231271203599,60.277144559778,11.8892082300412));
#81025=CARTESIAN_POINT('Ctrl Pts',(87.3525060992781,60.151130315295,10.7201148568299));
#81026=CARTESIAN_POINT('Ctrl Pts',(88.7845403251703,60.0251160708116,10.7827788962033));
#81027=CARTESIAN_POINT('Ctrl Pts',(89.5086285318225,59.8991018263285,12.0198500643034));
#81028=CARTESIAN_POINT('Ctrl Pts',(88.862083401201,59.7730875818452,13.2991577677224));
#81029=CARTESIAN_POINT('Ctrl Pts',(87.4366246363239,59.647073337362,13.4498764314403));
#81030=CARTESIAN_POINT('Ctrl Pts',(86.5368356252177,59.5210590928787,12.3340679615629));
#81031=CARTESIAN_POINT('Ctrl Pts',(86.9862054968145,59.3950448483955,10.9729230300959));
#81032=CARTESIAN_POINT('Ctrl Pts',(88.3734698329432,59.2690306039123,10.6121648456238));
#81033=CARTESIAN_POINT('Ctrl Pts',(89.4290008812559,59.1430163594291,11.5819601910473));
#81034=CARTESIAN_POINT('Ctrl Pts',(89.1867740150826,59.0170021149458,12.9947499670796));
#81035=CARTESIAN_POINT('Ctrl Pts',(87.8684758615844,58.8909878704626,13.5575454756268));
#81036=CARTESIAN_POINT('Ctrl Pts',(86.6806161521516,58.7649736259794,12.7552748749792));
#81037=CARTESIAN_POINT('Ctrl Pts',(86.7103270314763,58.6389593814962,11.322178203569));
#81038=CARTESIAN_POINT('Ctrl Pts',(87.9304170293001,58.5129451370129,10.5698290803765));
#81039=CARTESIAN_POINT('Ctrl Pts',(89.2242567612607,58.3869308925298,11.1867792841674));
#81040=CARTESIAN_POINT('Ctrl Pts',(89.4077209038666,58.2609166480465,12.6083944621729));
#81041=CARTESIAN_POINT('Ctrl Pts',(88.3129026199372,58.1349024035633,13.5336088865802));
#81042=CARTESIAN_POINT('Ctrl Pts',(86.941782311371,58.0088881590801,13.1156640273043));
#81043=CARTESIAN_POINT('Ctrl Pts',(86.549212676552,57.8828739145968,11.7370640534991));
#81044=CARTESIAN_POINT('Ctrl Pts',(87.4944744164356,57.7568596701136,10.6595070716789));
#81045=CARTESIAN_POINT('Ctrl Pts',(88.9124616482187,57.6308454256303,10.8691758973496));
#81046=CARTESIAN_POINT('Ctrl Pts',(89.5054289494459,57.5048311811472,12.1741811025625));
#81047=CARTESIAN_POINT('Ctrl Pts',(88.730691179106,57.3788169366639,13.3801786950834));
#81048=CARTESIAN_POINT('Ctrl Pts',(87.2972902612201,57.2528026921807,13.3834366947466));
#81049=CARTESIAN_POINT('Ctrl Pts',(86.5170782618964,57.1267884476975,12.1809733722003));
#81050=CARTESIAN_POINT('Ctrl Pts',(87.1041071330646,57.0007742032142,10.8732861349864));
#81051=CARTESIAN_POINT('Ctrl Pts',(88.5211265995945,56.874759958731,10.6571735776611));
#81052=CARTESIAN_POINT('Ctrl Pts',(89.4712769401843,56.7487457142478,11.7304224473247));
#81053=CARTESIAN_POINT('Ctrl Pts',(89.0849782125712,56.6227314697646,13.1107927233745));
#81054=CARTESIAN_POINT('Ctrl Pts',(87.7157719679219,56.4967172252814,13.5349661143026));
#81055=CARTESIAN_POINT('Ctrl Pts',(86.6167591485887,56.3707029807981,12.6147380833783));
#81056=CARTESIAN_POINT('Ctrl Pts',(86.7937590056485,56.2446887363149,11.1923036010353));
#81057=CARTESIAN_POINT('Ctrl Pts',(88.0847808320441,56.1186744918317,10.5694782244428));
#81058=CARTESIAN_POINT('Ctrl Pts',(89.3082782584284,55.9926602473484,11.3162732790522));
#81059=CARTESIAN_POINT('Ctrl Pts',(89.3445034133909,55.8666460028653,12.7492200834052));
#81060=CARTESIAN_POINT('Ctrl Pts',(88.1603029454942,55.740631758382,13.5568821772229));
#81061=CARTESIAN_POINT('Ctrl Pts',(86.8394600525235,55.6146175138988,13.0000852141859));
#81062=CARTESIAN_POINT('Ctrl Pts',(86.5908134177302,55.4886032694155,11.5884111523135));
#81063=CARTESIAN_POINT('Ctrl Pts',(87.6419250563981,55.3625890249324,10.6138275853401));
#81064=CARTESIAN_POINT('Ctrl Pts',(89.0308149964968,55.2365747804491,10.9682758047605));
#81065=CARTESIAN_POINT('Ctrl Pts',(89.4863677289041,55.1105605359659,12.3273639232995));
#81066=CARTESIAN_POINT('Ctrl Pts',(88.5916602659388,54.9845462914826,13.4472511326524));
#81067=CARTESIAN_POINT('Ctrl Pts',(87.165531091104,54.8585320469995,13.3030138883554));
#81068=CARTESIAN_POINT('Ctrl Pts',(86.5131771532775,54.7325178025162,12.0266584732144));
#81069=CARTESIAN_POINT('Ctrl Pts',(87.2316343902018,54.606503558033,10.7863085207138));
#81070=CARTESIAN_POINT('Ctrl Pts',(88.6633689612688,54.4804893135498,10.7171353758561));
#81071=CARTESIAN_POINT('Ctrl Pts',(89.4980538451014,54.3544750690665,11.8824464719411));
#81072=CARTESIAN_POINT('Ctrl Pts',(88.9717833711079,54.2284608245833,13.2157462109946));
#81073=CARTESIAN_POINT('Ctrl Pts',(87.5662015790156,54.1024465801001,13.4967953734143));
#81074=CARTESIAN_POINT('Ctrl Pts',(86.5677004021856,53.9764323356168,12.4683770704725));
#81075=CARTESIAN_POINT('Ctrl Pts',(86.8901105878214,53.8504180911337,11.0717022772023));
#81076=CARTESIAN_POINT('Ctrl Pts',(88.2383615364273,53.7244038466504,10.5850112196082));
#81077=CARTESIAN_POINT('Ctrl Pts',(89.3785306444292,53.5983896021672,11.4537247576126));
#81078=CARTESIAN_POINT('Ctrl Pts',(89.2671323235476,53.4723753576839,12.8827941121466));
#81079=CARTESIAN_POINT('Ctrl Pts',(88.0061185926342,53.3463611132008,13.5643314745901));
#81080=CARTESIAN_POINT('Ctrl Pts',(86.7495723378244,53.2203468687175,12.8745921648102));
#81081=CARTESIAN_POINT('Ctrl Pts',(86.6474878000429,53.0943326242343,11.4448273054174));
#81082=CARTESIAN_POINT('Ctrl Pts',(87.7932930008493,52.9683183797511,10.5835612328527));
#81083=CARTESIAN_POINT('Ctrl Pts',(89.1383441858098,52.8423041352678,11.0790267872718));
#81084=CARTESIAN_POINT('Ctrl Pts',(89.4516471831037,52.7162898907846,12.4777726677943));
#81085=CARTESIAN_POINT('Ctrl Pts',(88.4464663142398,52.5902756463014,13.499663183749));
#81086=CARTESIAN_POINT('Ctrl Pts',(87.042745597686,52.4642614018182,13.2094616078837));
#81087=CARTESIAN_POINT('Ctrl Pts',(86.5251737046872,52.338247157335,11.8727611383899));
#81088=CARTESIAN_POINT('Ctrl Pts',(87.3674337144834,52.2122329128517,10.7129133557097));
#81089=CARTESIAN_POINT('Ctrl Pts',(88.7986871777436,52.0862186683684,10.7914138120163));
#81090=CARTESIAN_POINT('Ctrl Pts',(89.5090473935824,51.9602044238853,12.0364187112151));
#81091=CARTESIAN_POINT('Ctrl Pts',(88.8483909162438,51.834190179402,13.3084964581282));
#81092=CARTESIAN_POINT('Ctrl Pts',(87.42135222593,51.7081759349188,13.4434384147102));
#81093=CARTESIAN_POINT('Ctrl Pts',(86.5339605868047,51.5821616904356,12.3177452426549));
#81094=CARTESIAN_POINT('Ctrl Pts',(86.9983591733833,51.4561474459524,10.9616543695276));
#81095=CARTESIAN_POINT('Ctrl Pts',(88.389528948128,51.3301332014691,10.6162630137755));
#81096=CARTESIAN_POINT('Ctrl Pts',(89.434268496194,51.204118956986,11.597675205714));
#81097=CARTESIAN_POINT('Ctrl Pts',(89.1764283892337,51.0781047125027,13.0076980648546));
#81098=CARTESIAN_POINT('Ctrl Pts',(87.8519869502598,50.9520904680195,13.5558792121182));
#81099=CARTESIAN_POINT('Ctrl Pts',(86.6730714212938,50.8260762235362,12.740513844204));
#81100=CARTESIAN_POINT('Ctrl Pts',(86.7186378916432,50.7000619790531,11.3078424883874));
#81101=CARTESIAN_POINT('Ctrl Pts',(87.9469644498306,50.5740477345697,10.5690172567477));
#81102=CARTESIAN_POINT('Ctrl Pts',(89.2339223286193,50.4480334900867,11.2002773553426));
#81103=CARTESIAN_POINT('Ctrl Pts',(89.4016070035495,50.3220192456032,12.6237629030343));
#81104=CARTESIAN_POINT('Ctrl Pts',(88.2967080575638,50.1960050011202,13.536954610423));
#81105=CARTESIAN_POINT('Ctrl Pts',(86.9301216186333,50.0699907566368,13.1035806341709));
#81106=CARTESIAN_POINT('Ctrl Pts',(86.5531718275547,49.9439765121537,11.7212995011988));
#81107=CARTESIAN_POINT('Ctrl Pts',(87.5095953909142,49.8179622676705,10.6531063522201));
#81108=CARTESIAN_POINT('Ctrl Pts',(88.9267744927432,49.6919367901709,10.8808357729695));
#81109=CARTESIAN_POINT('Ctrl Pts',(89.3094755969595,49.6079160608325,11.7516938683196));
#81110=CARTESIAN_POINT('Ctrl Pts',(89.2742633450769,49.565900079655,12.1718452204411));
#81111=CARTESIAN_POINT('Ctrl Pts',(87.3512658244469,65.1072380988749,13.316638536706));
#81112=CARTESIAN_POINT('Ctrl Pts',(86.9354257671071,65.0652333507139,13.0972754758862));
#81113=CARTESIAN_POINT('Ctrl Pts',(86.3470952443779,64.9812238543917,12.2145662664107));
#81114=CARTESIAN_POINT('Ctrl Pts',(86.9843518983242,64.8552096099085,10.7460117557066));
#81115=CARTESIAN_POINT('Ctrl Pts',(88.5628015504014,64.7291953654253,10.4888445104814));
#81116=CARTESIAN_POINT('Ctrl Pts',(89.6354428818203,64.603181120942,11.6734788447291));
#81117=CARTESIAN_POINT('Ctrl Pts',(89.2217890457325,64.4771668764588,13.2181526924379));
#81118=CARTESIAN_POINT('Ctrl Pts',(87.6998186353989,64.3511526319757,13.7079723378312));
#81119=CARTESIAN_POINT('Ctrl Pts',(86.4627418825683,64.2251383874924,12.6952553802185));
#81120=CARTESIAN_POINT('Ctrl Pts',(86.6425849471111,64.0991241430091,11.1065420914071));
#81121=CARTESIAN_POINT('Ctrl Pts',(88.074829769566,63.9731098985258,10.3959771697335));
#81122=CARTESIAN_POINT('Ctrl Pts',(89.4486449732643,63.8470956540426,11.2137962207137));
#81123=CARTESIAN_POINT('Ctrl Pts',(89.5067301675622,63.7210814095594,12.8115668028847));
#81124=CARTESIAN_POINT('Ctrl Pts',(88.1959162995001,63.5950671650762,13.7269865417335));
#81125=CARTESIAN_POINT('Ctrl Pts',(86.7158681327567,63.469052920593,13.1222704183564));
#81126=CARTESIAN_POINT('Ctrl Pts',(86.421127077019,63.3430386761097,11.5508514303896));
#81127=CARTESIAN_POINT('Ctrl Pts',(87.5814420424177,63.2170244316266,10.4508984699093));
#81128=CARTESIAN_POINT('Ctrl Pts',(89.1348893188699,63.0910101871434,10.8290900343238));
#81129=CARTESIAN_POINT('Ctrl Pts',(89.6597504075091,62.9649959426601,12.339304854756));
#81130=CARTESIAN_POINT('Ctrl Pts',(88.6756709958075,62.8389816981769,13.5993902982778));
#81131=CARTESIAN_POINT('Ctrl Pts',(87.0832830687143,62.7129674536937,13.4561131962439));
#81132=CARTESIAN_POINT('Ctrl Pts',(86.3399439600512,62.5869532092103,12.040601033618));
#81133=CARTESIAN_POINT('Ctrl Pts',(87.1259594792068,62.4609389647273,10.6483340800663));
#81134=CARTESIAN_POINT('Ctrl Pts',(88.7219662694403,62.3349247202439,10.5535184774675));
#81135=CARTESIAN_POINT('Ctrl Pts',(89.6672949725552,62.2089104757607,11.8429297090355));
#81136=CARTESIAN_POINT('Ctrl Pts',(89.0967784185581,62.0828962312775,13.3364954212178));
#81137=CARTESIAN_POINT('Ctrl Pts',(87.5325547701926,61.9568819867942,13.6673005816136));
#81138=CARTESIAN_POINT('Ctrl Pts',(86.4062053795725,61.830867742311,12.5325914879137));
#81139=CARTESIAN_POINT('Ctrl Pts',(86.7485679957279,61.7048534978279,10.9708567103754));
#81140=CARTESIAN_POINT('Ctrl Pts',(88.2463115052484,61.5788392533447,10.4113997806569));
#81141=CARTESIAN_POINT('Ctrl Pts',(89.5286973430571,61.4528250088614,11.3662370650074));
#81142=CARTESIAN_POINT('Ctrl Pts',(89.4220828178908,61.3268107643783,12.9614991185673));
#81143=CARTESIAN_POINT('Ctrl Pts',(88.0240418069501,61.2007965198949,13.737198163471));
#81144=CARTESIAN_POINT('Ctrl Pts',(86.6140649020221,61.0747822754117,12.9834125148202));
#81145=CARTESIAN_POINT('Ctrl Pts',(86.4825664546115,60.9487680309286,11.3900086630425));
#81146=CARTESIAN_POINT('Ctrl Pts',(87.7498941690976,60.8227537864452,10.4152737551668));
#81147=CARTESIAN_POINT('Ctrl Pts',(89.2561865859698,60.696739541962,10.9512875902581));
#81148=CARTESIAN_POINT('Ctrl Pts',(89.622881158923,60.5707252974788,12.507488980407));
#81149=CARTESIAN_POINT('Ctrl Pts',(88.5143781076331,60.4447110529956,13.6596385634979));
#81150=CARTESIAN_POINT('Ctrl Pts',(86.9451821669415,60.3186968085123,13.3532861908084));
#81151=CARTESIAN_POINT('Ctrl Pts',(86.351425343768,60.1926825640292,11.8688063117025));
#81152=CARTESIAN_POINT('Ctrl Pts',(87.276515351563,60.066668319546,10.5647985839596));
#81153=CARTESIAN_POINT('Ctrl Pts',(88.8738075266325,59.9406540750628,10.6346941059655));
#81154=CARTESIAN_POINT('Ctrl Pts',(89.681456118848,59.8146398305795,12.0145243230676));
#81155=CARTESIAN_POINT('Ctrl Pts',(88.9602991385892,59.6886255860963,13.4414652070427));
#81156=CARTESIAN_POINT('Ctrl Pts',(87.3703412382439,59.562611341613,13.6095769307997));
#81157=CARTESIAN_POINT('Ctrl Pts',(86.3667158215692,59.4365970971297,12.3650032288681));
#81158=CARTESIAN_POINT('Ctrl Pts',(86.8679433527522,59.3105828526465,10.846781032179));
#81159=CARTESIAN_POINT('Ctrl Pts',(88.415299155279,59.1845686081633,10.4443910510384));
#81160=CARTESIAN_POINT('Ctrl Pts',(89.5926393707076,59.05855436368,11.5261015916497));
#81161=CARTESIAN_POINT('Ctrl Pts',(89.3224593212823,58.9325401191969,13.1019284912259));
#81162=CARTESIAN_POINT('Ctrl Pts',(87.8520284566294,58.8065258747136,13.7296710728716));
#81163=CARTESIAN_POINT('Ctrl Pts',(86.5270887417454,58.6805116302305,12.8348177729066));
#81164=CARTESIAN_POINT('Ctrl Pts',(86.5602282814311,58.5544973857473,11.2363405452162));
#81165=CARTESIAN_POINT('Ctrl Pts',(87.9211176869828,58.4284831412641,10.39716970302));
#81166=CARTESIAN_POINT('Ctrl Pts',(89.3642676077659,58.3024688967808,11.085316477102));
#81167=CARTESIAN_POINT('Ctrl Pts',(89.5689036661028,58.1764546522976,12.6709872374314));
#81168=CARTESIAN_POINT('Ctrl Pts',(88.3477424351596,58.0504404078143,13.7029721813991));
#81169=CARTESIAN_POINT('Ctrl Pts',(86.8183936944983,57.9244261633312,13.2367961352814));
#81170=CARTESIAN_POINT('Ctrl Pts',(86.3805211949948,57.7984119188478,11.6991045697475));
#81171=CARTESIAN_POINT('Ctrl Pts',(87.4348669314369,57.6723976743646,10.4971966096353));
#81172=CARTESIAN_POINT('Ctrl Pts',(89.0164910775108,57.5463834298814,10.7310613934125));
#81173=CARTESIAN_POINT('Ctrl Pts',(89.6778873019851,57.4203691853982,12.1866652924135));
#81174=CARTESIAN_POINT('Ctrl Pts',(88.8137441440068,57.2943549409149,13.5318360172864));
#81175=CARTESIAN_POINT('Ctrl Pts',(87.2149275595431,57.1683406964318,13.5354699928398));
#81176=CARTESIAN_POINT('Ctrl Pts',(86.3446784419712,57.0423264519486,12.1942413956571));
#81177=CARTESIAN_POINT('Ctrl Pts',(86.9994509365831,56.9163122074654,10.7356459559154));
#81178=CARTESIAN_POINT('Ctrl Pts',(88.5799956364829,56.7902979629822,10.4945938284533));
#81179=CARTESIAN_POINT('Ctrl Pts',(89.6397941222479,56.6642837184989,11.6916965166575));
#81180=CARTESIAN_POINT('Ctrl Pts',(89.2089161978942,56.5382694740156,13.2313626787977));
#81181=CARTESIAN_POINT('Ctrl Pts',(87.6817024057294,56.4122552295323,13.7044860343376));
#81182=CARTESIAN_POINT('Ctrl Pts',(86.4558625864833,56.2862409850493,12.6780629178376));
#81183=CARTESIAN_POINT('Ctrl Pts',(86.6532883753072,56.1602267405659,11.0914783047638));
#81184=CARTESIAN_POINT('Ctrl Pts',(88.0932952018629,56.0342124960827,10.3967783580177));
#81185=CARTESIAN_POINT('Ctrl Pts',(89.4579852560851,55.9081982515995,11.2297541874641));
#81186=CARTESIAN_POINT('Ctrl Pts',(89.4983908242738,55.7821840071162,12.8280642533132));
#81187=CARTESIAN_POINT('Ctrl Pts',(88.177532630464,55.6561697626331,13.7289312292763));
#81188=CARTESIAN_POINT('Ctrl Pts',(86.7042633612723,55.5301555181499,13.1078794303172));
#81189=CARTESIAN_POINT('Ctrl Pts',(86.4269226965508,55.4041412736666,11.5332969992495));
#81190=CARTESIAN_POINT('Ctrl Pts',(87.5993334987596,55.2781270291835,10.4462456723107));
#81191=CARTESIAN_POINT('Ctrl Pts',(89.1485025013162,55.1521127847002,10.8415975131473));
#81192=CARTESIAN_POINT('Ctrl Pts',(89.6566264006262,55.0260985402169,12.3575255389735));
#81193=CARTESIAN_POINT('Ctrl Pts',(88.6586689470046,54.9000842957338,13.6066486703326));
#81194=CARTESIAN_POINT('Ctrl Pts',(87.0679632708306,54.7740700512506,13.4457663272269));
#81195=CARTESIAN_POINT('Ctrl Pts',(86.3403271421501,54.6480558067672,12.0221184280699));
#81196=CARTESIAN_POINT('Ctrl Pts',(87.1416949460142,54.522041562284,10.6386310521009));
#81197=CARTESIAN_POINT('Ctrl Pts',(88.7386528858405,54.3960273178008,10.5614752683855));
#81198=CARTESIAN_POINT('Ctrl Pts',(89.6696611044214,54.2700130733175,11.8612642410538));
#81199=CARTESIAN_POINT('Ctrl Pts',(89.082658576911,54.1439988288344,13.3484278868009));
#81200=CARTESIAN_POINT('Ctrl Pts',(87.5148714686594,54.0179845843512,13.661910357978));
#81201=CARTESIAN_POINT('Ctrl Pts',(86.401142419652,53.891970339868,12.5148117214466));
#81202=CARTESIAN_POINT('Ctrl Pts',(86.7607590107698,53.7659560953848,10.9569594871417));
#81203=CARTESIAN_POINT('Ctrl Pts',(88.2645992481749,53.6399418509016,10.414103873836));
#81204=CARTESIAN_POINT('Ctrl Pts',(89.5363448262758,53.5139276064182,11.3830676817832));
#81205=CARTESIAN_POINT('Ctrl Pts',(89.4120910458545,53.3879133619351,12.9770528368564));
#81206=CARTESIAN_POINT('Ctrl Pts',(88.0055552741355,53.2618991174519,13.7372401817996));
#81207=CARTESIAN_POINT('Ctrl Pts',(86.6040025290045,53.1358848729685,12.9679043779273));
#81208=CARTESIAN_POINT('Ctrl Pts',(86.4901373500544,53.0098706284853,11.373143456152));
#81209=CARTESIAN_POINT('Ctrl Pts',(87.7681694307903,52.8838563840021,10.4124865573944));
#81210=CARTESIAN_POINT('Ctrl Pts',(89.2684406491452,52.7578421395189,10.9651292518083));
#81211=CARTESIAN_POINT('Ctrl Pts',(89.6178990747577,52.6318278950357,12.5252915785692));
#81212=CARTESIAN_POINT('Ctrl Pts',(88.4967194916609,52.5058136505524,13.6651091160275));
#81213=CARTESIAN_POINT('Ctrl Pts',(86.9310082286238,52.3797994060693,13.3414180352269));
#81214=CARTESIAN_POINT('Ctrl Pts',(86.353708105641,52.253785161586,11.8504612118982));
#81215=CARTESIAN_POINT('Ctrl Pts',(87.2931656260668,52.1277709171029,10.5567660235778));
#81216=CARTESIAN_POINT('Ctrl Pts',(88.8895869378427,52.0017566726195,10.6443254982963));
#81217=CARTESIAN_POINT('Ctrl Pts',(89.6819233176056,51.8757424281364,12.0330050057112));
#81218=CARTESIAN_POINT('Ctrl Pts',(88.9450265293989,51.7497281836532,13.4518815901437));
#81219=CARTESIAN_POINT('Ctrl Pts',(87.3533063788977,51.6237139391698,13.6023959615463));
#81220=CARTESIAN_POINT('Ctrl Pts',(86.3635090013151,51.4976996946866,12.3467968545257));
#81221=CARTESIAN_POINT('Ctrl Pts',(86.8814995737771,51.3716854502034,10.8342119587422));
#81222=CARTESIAN_POINT('Ctrl Pts',(88.4332115058078,51.2456712057202,10.4489621512275));
#81223=CARTESIAN_POINT('Ctrl Pts',(89.5985148728217,51.119656961237,11.5436301321723));
#81224=CARTESIAN_POINT('Ctrl Pts',(89.3109198015447,50.9936427167538,13.1163708103297));
#81225=CARTESIAN_POINT('Ctrl Pts',(87.8336367111264,50.8676284722706,13.7278125211585));
#81226=CARTESIAN_POINT('Ctrl Pts',(86.5186733426272,50.7416142277874,12.8183533068156));
#81227=CARTESIAN_POINT('Ctrl Pts',(86.5694982218224,50.6155999833041,11.2203504764948));
#81228=CARTESIAN_POINT('Ctrl Pts',(87.9395746937033,50.4895857388209,10.3962641942645));
#81229=CARTESIAN_POINT('Ctrl Pts',(89.3750485896936,50.3635714943377,11.1003722369971));
#81230=CARTESIAN_POINT('Ctrl Pts',(89.5620842165681,50.2375572498545,12.6881292092412));
#81231=CARTESIAN_POINT('Ctrl Pts',(88.3296790067231,50.1115430053713,13.7067040045759));
#81232=CARTESIAN_POINT('Ctrl Pts',(86.8053873480519,49.9855287608879,13.223318308459));
#81233=CARTESIAN_POINT('Ctrl Pts',(86.3849372353393,49.8595145164047,11.6815207749069));
#81234=CARTESIAN_POINT('Ctrl Pts',(87.4517328790361,49.7335002719215,10.4900572417896));
#81235=CARTESIAN_POINT('Ctrl Pts',(89.0324556362825,49.6074747944219,10.7440668284456));
#81236=CARTESIAN_POINT('Ctrl Pts',(89.4593207684858,49.5234540650835,11.7154226774526));
#81237=CARTESIAN_POINT('Ctrl Pts',(89.4200449932413,49.4814380839061,12.1840598475387));
#81238=CARTESIAN_POINT('Ctrl Pts',(87.2830088589676,65.022776103126,13.4460312445424));
#81239=CARTESIAN_POINT('Ctrl Pts',(86.8241454423862,64.9807713549649,13.2039725929459));
#81240=CARTESIAN_POINT('Ctrl Pts',(86.1749454700084,64.8967618586428,12.2299371277265));
#81241=CARTESIAN_POINT('Ctrl Pts',(86.8781335354862,64.7707476141595,10.609444035915));
#81242=CARTESIAN_POINT('Ctrl Pts',(88.6198916645305,64.6447333696763,10.3256699292747));
#81243=CARTESIAN_POINT('Ctrl Pts',(89.8035098788265,64.5187191251931,11.6328680897644));
#81244=CARTESIAN_POINT('Ctrl Pts',(89.347058872823,64.3927048807099,13.3373559252986));
#81245=CARTESIAN_POINT('Ctrl Pts',(87.6676234021542,64.2666906362266,13.8778529554108));
#81246=CARTESIAN_POINT('Ctrl Pts',(86.3025570614835,64.1406763917435,12.7603589694471));
#81247=CARTESIAN_POINT('Ctrl Pts',(86.5010069260116,64.0146621472602,11.0072753143134));
#81248=CARTESIAN_POINT('Ctrl Pts',(88.0814336814738,63.888647902777,10.2231944113149));
#81249=CARTESIAN_POINT('Ctrl Pts',(89.5973856129763,63.7626336582937,11.1256260968977));
#81250=CARTESIAN_POINT('Ctrl Pts',(89.6614803778694,63.6366194138105,12.8887041248741));
#81251=CARTESIAN_POINT('Ctrl Pts',(88.2150479830468,63.5106051693273,13.8988343938561));
#81252=CARTESIAN_POINT('Ctrl Pts',(86.5818720864256,63.3845909248441,13.2315535450371));
#81253=CARTESIAN_POINT('Ctrl Pts',(86.2566367334206,63.2585766803608,11.4975534818589));
#81254=CARTESIAN_POINT('Ctrl Pts',(87.5369994111753,63.1325624358777,10.2837979414388));
#81255=CARTESIAN_POINT('Ctrl Pts',(89.2511683859297,63.0065481913943,10.7011177025018));
#81256=CARTESIAN_POINT('Ctrl Pts',(89.830332293092,62.8805339469112,12.3675813344771));
#81257=CARTESIAN_POINT('Ctrl Pts',(88.7444387312032,62.7545197024279,13.7580368752391));
#81258=CARTESIAN_POINT('Ctrl Pts',(86.9873002548784,62.6285054579448,13.5999361357919));
#81259=CARTESIAN_POINT('Ctrl Pts',(86.1670543043998,62.5024912134615,12.0379732231516));
#81260=CARTESIAN_POINT('Ctrl Pts',(87.0343920229282,62.3764769689783,10.5016604994881));
#81261=CARTESIAN_POINT('Ctrl Pts',(88.7955237747332,62.2504627244951,10.3970351499439));
#81262=CARTESIAN_POINT('Ctrl Pts',(89.8386574287603,62.1244484800117,11.8198505633521));
#81263=CARTESIAN_POINT('Ctrl Pts',(89.2091144817484,61.9984342355287,13.4679425484414));
#81264=CARTESIAN_POINT('Ctrl Pts',(87.4830541974697,61.8724199910453,13.8329732458038));
#81265=CARTESIAN_POINT('Ctrl Pts',(86.2401712175313,61.7464057465622,12.5808656569103));
#81266=CARTESIAN_POINT('Ctrl Pts',(86.6179551202264,61.6203915020788,10.857551745308));
#81267=CARTESIAN_POINT('Ctrl Pts',(88.270657143061,61.4943772575958,10.240212665848));
#81268=CARTESIAN_POINT('Ctrl Pts',(89.6857203062321,61.3683630131124,11.293838671431));
#81269=CARTESIAN_POINT('Ctrl Pts',(89.5680753020734,61.2423487686293,13.0541486351269));
#81270=CARTESIAN_POINT('Ctrl Pts',(88.0253911294497,61.116334524146,13.9101025234088));
#81271=CARTESIAN_POINT('Ctrl Pts',(86.4695361595484,60.9903202796628,13.0783292201763));
#81272=CARTESIAN_POINT('Ctrl Pts',(86.3244327098233,60.8643060351796,11.320069710263));
#81273=CARTESIAN_POINT('Ctrl Pts',(87.7228798164282,60.7382917906963,10.2444874468557));
#81274=CARTESIAN_POINT('Ctrl Pts',(89.3850152278127,60.6122775462132,10.8359579782862));
#81275=CARTESIAN_POINT('Ctrl Pts',(89.789648503557,60.4862633017299,12.5531660109623));
#81276=CARTESIAN_POINT('Ctrl Pts',(88.5664582686874,60.3602490572467,13.8245185052168));
#81277=CARTESIAN_POINT('Ctrl Pts',(86.834911252179,60.2342348127635,13.486470513137));
#81278=CARTESIAN_POINT('Ctrl Pts',(86.1797235671763,60.1082205682802,11.8484043933639));
#81279=CARTESIAN_POINT('Ctrl Pts',(87.2005246038479,59.982206323797,10.4094823110891));
#81280=CARTESIAN_POINT('Ctrl Pts',(88.9630747280948,59.8561920793138,10.4866093157278));
#81281=CARTESIAN_POINT('Ctrl Pts',(89.8542837058732,59.7301778348306,12.0091985818318));
#81282=CARTESIAN_POINT('Ctrl Pts',(89.0585148759775,59.6041635903473,13.5837726463632));
#81283=CARTESIAN_POINT('Ctrl Pts',(87.304057840164,59.4781493458641,13.769277430159));
#81284=CARTESIAN_POINT('Ctrl Pts',(86.1965960179204,59.3521351013809,12.3959384961732));
#81285=CARTESIAN_POINT('Ctrl Pts',(86.74968120869,59.2261208568977,10.7206390342622));
#81286=CARTESIAN_POINT('Ctrl Pts',(88.4571284776149,59.1001066124145,10.2766172564529));
#81287=CARTESIAN_POINT('Ctrl Pts',(89.7562778601591,58.9740923679312,11.4702429922521));
#81288=CARTESIAN_POINT('Ctrl Pts',(89.4581446274822,58.848078123448,13.2091070153721));
#81289=CARTESIAN_POINT('Ctrl Pts',(87.8355810516741,58.7220638789647,13.9017966701166));
#81290=CARTESIAN_POINT('Ctrl Pts',(86.3735613313395,58.5960496344816,12.9143606708339));
#81291=CARTESIAN_POINT('Ctrl Pts',(86.4101295313855,58.4700353899983,11.1505028868634));
#81292=CARTESIAN_POINT('Ctrl Pts',(87.9118183446658,58.3440211455151,10.2245103256635));
#81293=CARTESIAN_POINT('Ctrl Pts',(89.5042784542709,58.2180069010319,10.9838536700367));
#81294=CARTESIAN_POINT('Ctrl Pts',(89.7300864283392,58.0919926565487,12.7335800126899));
#81295=CARTESIAN_POINT('Ctrl Pts',(88.3825822503817,57.9659784120654,13.8723354762181));
#81296=CARTESIAN_POINT('Ctrl Pts',(86.6950050776261,57.8399641675822,13.3579282432583));
#81297=CARTESIAN_POINT('Ctrl Pts',(86.2118297134374,57.713949923099,11.661145085996));
#81298=CARTESIAN_POINT('Ctrl Pts',(87.3752594464383,57.5879356786158,10.3348861475917));
#81299=CARTESIAN_POINT('Ctrl Pts',(89.1205205068032,57.4619214341325,10.5929468894755));
#81300=CARTESIAN_POINT('Ctrl Pts',(89.8503456545239,57.3359071896493,12.1991494822645));
#81301=CARTESIAN_POINT('Ctrl Pts',(88.8967971089079,57.209892945166,13.6834933394896));
#81302=CARTESIAN_POINT('Ctrl Pts',(87.132564857866,57.0838787006829,13.687503290933));
#81303=CARTESIAN_POINT('Ctrl Pts',(86.172278622046,56.9578644561996,12.2075094191137));
#81304=CARTESIAN_POINT('Ctrl Pts',(86.8947947401016,56.8318502117164,10.5980057768445));
#81305=CARTESIAN_POINT('Ctrl Pts',(88.6388646733714,56.7058359672331,10.3320140792455));
#81306=CARTESIAN_POINT('Ctrl Pts',(89.8083113043114,56.57982172275,11.6529705859901));
#81307=CARTESIAN_POINT('Ctrl Pts',(89.3328541832171,56.4538074782667,13.3519326342209));
#81308=CARTESIAN_POINT('Ctrl Pts',(87.6476328435369,56.3277932337835,13.8740059543726));
#81309=CARTESIAN_POINT('Ctrl Pts',(86.2949660243777,56.2017789893003,12.7413877522968));
#81310=CARTESIAN_POINT('Ctrl Pts',(86.5128177449663,56.0757647448171,10.9906530084923));
#81311=CARTESIAN_POINT('Ctrl Pts',(88.1018095716815,55.9497505003338,10.2240784915925));
#81312=CARTESIAN_POINT('Ctrl Pts',(89.6076922537419,55.8237362558506,11.143235095876));
#81313=CARTESIAN_POINT('Ctrl Pts',(89.6522782351566,55.6977220113674,12.9069084232212));
#81314=CARTESIAN_POINT('Ctrl Pts',(88.194762315434,55.5717077668842,13.9009802813298));
#81315=CARTESIAN_POINT('Ctrl Pts',(86.5690666700211,55.4456935224009,13.2156736464485));
#81316=CARTESIAN_POINT('Ctrl Pts',(86.2630319753712,55.3196792779177,11.4781828461855));
#81317=CARTESIAN_POINT('Ctrl Pts',(87.5567419411211,55.1936650334345,10.2786637592813));
#81318=CARTESIAN_POINT('Ctrl Pts',(89.2661900061356,55.0676507889513,10.7149192215342));
#81319=CARTESIAN_POINT('Ctrl Pts',(89.8268850723484,54.941636544468,12.3876871546476));
#81320=CARTESIAN_POINT('Ctrl Pts',(88.7256776280701,54.8156222999848,13.7660462080128));
#81321=CARTESIAN_POINT('Ctrl Pts',(86.9703954505572,54.6896080555015,13.5885187660983));
#81322=CARTESIAN_POINT('Ctrl Pts',(86.1674771310224,54.5635938110184,12.0175783829253));
#81323=CARTESIAN_POINT('Ctrl Pts',(87.0517555018266,54.4375795665351,10.4909535834882));
#81324=CARTESIAN_POINT('Ctrl Pts',(88.8139368104121,54.3115653220519,10.405815160915));
#81325=CARTESIAN_POINT('Ctrl Pts',(89.8412683637416,54.1855510775687,11.8400820101666));
#81326=CARTESIAN_POINT('Ctrl Pts',(89.193533782714,54.0595368330855,13.4811095626073));
#81327=CARTESIAN_POINT('Ctrl Pts',(87.4635413583032,53.9335225886023,13.8270253425417));
#81328=CARTESIAN_POINT('Ctrl Pts',(86.2345844371186,53.807508344119,12.5612463724207));
#81329=CARTESIAN_POINT('Ctrl Pts',(86.6314074337182,53.6814940996358,10.8422166970809));
#81330=CARTESIAN_POINT('Ctrl Pts',(88.2908369599225,53.5554798551525,10.2431965280638));
#81331=CARTESIAN_POINT('Ctrl Pts',(89.6941590081224,53.4294656106693,11.3124106059539));
#81332=CARTESIAN_POINT('Ctrl Pts',(89.5570497681611,53.3034513661862,13.0713115615662));
#81333=CARTESIAN_POINT('Ctrl Pts',(88.0049919556368,53.1774371217029,13.9101488890089));
#81334=CARTESIAN_POINT('Ctrl Pts',(86.4584327201847,53.0514228772197,13.0612165910444));
#81335=CARTESIAN_POINT('Ctrl Pts',(86.3327869000657,52.9254086327364,11.3014596068867));
#81336=CARTESIAN_POINT('Ctrl Pts',(87.7430458607311,52.7993943882532,10.2414118819361));
#81337=CARTESIAN_POINT('Ctrl Pts',(89.3985371124807,52.67338014377,10.8512317163449));
#81338=CARTESIAN_POINT('Ctrl Pts',(89.7841509664117,52.5473658992868,12.5728104893443));
#81339=CARTESIAN_POINT('Ctrl Pts',(88.5469726690822,52.4213516548036,13.830555048306));
#81340=CARTESIAN_POINT('Ctrl Pts',(86.8192708595616,52.2953374103203,13.4733744625701));
#81341=CARTESIAN_POINT('Ctrl Pts',(86.1822425065949,52.1693231658371,11.8281612854064));
#81342=CARTESIAN_POINT('Ctrl Pts',(87.2188975376501,52.0433089213539,10.4006186914459));
#81343=CARTESIAN_POINT('Ctrl Pts',(88.9804866979417,51.9172946768706,10.4972371845761));
#81344=CARTESIAN_POINT('Ctrl Pts',(89.8547992416286,51.7912804323874,12.0295913002075));
#81345=CARTESIAN_POINT('Ctrl Pts',(89.0416621425541,51.6652661879042,13.5952667221593));
#81346=CARTESIAN_POINT('Ctrl Pts',(87.2852605318656,51.539251943421,13.7613535083824));
#81347=CARTESIAN_POINT('Ctrl Pts',(86.1930574158255,51.4132376989378,12.3758484663964));
#81348=CARTESIAN_POINT('Ctrl Pts',(86.7646399741709,51.2872234544545,10.7067695479568));
#81349=CARTESIAN_POINT('Ctrl Pts',(88.4768940634877,51.1612092099713,10.2816612886795));
#81350=CARTESIAN_POINT('Ctrl Pts',(89.7627612494493,51.0351949654881,11.4895850586306));
#81351=CARTESIAN_POINT('Ctrl Pts',(89.4454112138556,50.9091807210049,13.2250435558049));
#81352=CARTESIAN_POINT('Ctrl Pts',(87.8152864719929,50.7831664765216,13.8997458301988));
#81353=CARTESIAN_POINT('Ctrl Pts',(86.3642752639605,50.6571522320384,12.8961927694272));
#81354=CARTESIAN_POINT('Ctrl Pts',(86.4203585520016,50.5311379875552,11.1328584646021));
#81355=CARTESIAN_POINT('Ctrl Pts',(87.9321849375758,50.4051237430719,10.2235111317813));
#81356=CARTESIAN_POINT('Ctrl Pts',(89.5161748507681,50.2791094985888,11.0004671186517));
#81357=CARTESIAN_POINT('Ctrl Pts',(89.7225614295866,50.1530952541055,12.7524955154482));
#81358=CARTESIAN_POINT('Ctrl Pts',(88.3626499558826,50.0270810096223,13.8764533987288));
#81359=CARTESIAN_POINT('Ctrl Pts',(86.6806530774701,49.901066765139,13.343055982747));
#81360=CARTESIAN_POINT('Ctrl Pts',(86.2167026431241,49.7750525206558,11.6417420486151));
#81361=CARTESIAN_POINT('Ctrl Pts',(87.3938703671579,49.6490382761727,10.3270081313591));
#81362=CARTESIAN_POINT('Ctrl Pts',(89.1381367798218,49.523012798673,10.6072978839217));
#81363=CARTESIAN_POINT('Ctrl Pts',(89.6091659400121,49.4389920693345,11.6791514865856));
#81364=CARTESIAN_POINT('Ctrl Pts',(89.5658266414056,49.3969760881572,12.1962744746363));
#81365=CARTESIAN_POINT('Ctrl Pts',(87.2147518934884,64.938314107377,13.5754239523789));
#81366=CARTESIAN_POINT('Ctrl Pts',(86.7128651176654,64.8963093592159,13.3106697100055));
#81367=CARTESIAN_POINT('Ctrl Pts',(86.0027956956387,64.8122998628938,12.2453079890425));
#81368=CARTESIAN_POINT('Ctrl Pts',(86.7719151726484,64.6862856184105,10.4728763161236));
#81369=CARTESIAN_POINT('Ctrl Pts',(88.6769817786594,64.5602713739274,10.1624953480681));
#81370=CARTESIAN_POINT('Ctrl Pts',(89.9715768758327,64.4342571294441,11.5922573347997));
#81371=CARTESIAN_POINT('Ctrl Pts',(89.4723286999136,64.3082428849609,13.4565591581593));
#81372=CARTESIAN_POINT('Ctrl Pts',(87.6354281689097,64.1822286404776,14.0477335729905));
#81373=CARTESIAN_POINT('Ctrl Pts',(86.1423722403985,64.0562143959944,12.8254625586757));
#81374=CARTESIAN_POINT('Ctrl Pts',(86.3594289049123,63.9302001515112,10.9080085372198));
#81375=CARTESIAN_POINT('Ctrl Pts',(88.0880375933813,63.804185907028,10.0504116528962));
#81376=CARTESIAN_POINT('Ctrl Pts',(89.7461262526883,63.6781716625447,11.0374559730818));
#81377=CARTESIAN_POINT('Ctrl Pts',(89.8162305881765,63.5521574180616,12.9658414468634));
#81378=CARTESIAN_POINT('Ctrl Pts',(88.2341796665934,63.4261431735783,14.0706822459788));
#81379=CARTESIAN_POINT('Ctrl Pts',(86.4478760400945,63.3001289290951,13.3408366717179));
#81380=CARTESIAN_POINT('Ctrl Pts',(86.092146389822,63.1741146846118,11.4442555333281));
#81381=CARTESIAN_POINT('Ctrl Pts',(87.4925567799329,63.0481004401286,10.1166974129684));
#81382=CARTESIAN_POINT('Ctrl Pts',(89.3674474529893,62.9220861956454,10.5731453706797));
#81383=CARTESIAN_POINT('Ctrl Pts',(90.0009141786748,62.7960719511622,12.3958578141983));
#81384=CARTESIAN_POINT('Ctrl Pts',(88.8132064665991,62.670057706679,13.9166834522003));
#81385=CARTESIAN_POINT('Ctrl Pts',(86.8913174410423,62.5440434621957,13.74375907534));
#81386=CARTESIAN_POINT('Ctrl Pts',(85.9941646487486,62.4180292177125,12.0353454126853));
#81387=CARTESIAN_POINT('Ctrl Pts',(86.9428245666493,62.2920149732293,10.3549869189101));
#81388=CARTESIAN_POINT('Ctrl Pts',(88.8690812800261,62.1660007287461,10.2405518224203));
#81389=CARTESIAN_POINT('Ctrl Pts',(90.0100198849654,62.0399864842628,11.7967714176689));
#81390=CARTESIAN_POINT('Ctrl Pts',(89.3214505449387,61.9139722397797,13.5993896756649));
#81391=CARTESIAN_POINT('Ctrl Pts',(87.4335536247469,61.7879579952963,13.998645909994));
#81392=CARTESIAN_POINT('Ctrl Pts',(86.0741370554901,61.6619437508132,12.6291398259069));
#81393=CARTESIAN_POINT('Ctrl Pts',(86.4873422447249,61.5359295063299,10.7442467802406));
#81394=CARTESIAN_POINT('Ctrl Pts',(88.2950027808736,61.4099152618468,10.0690255510391));
#81395=CARTESIAN_POINT('Ctrl Pts',(89.842743269407,61.2839010173635,11.2214402778546));
#81396=CARTESIAN_POINT('Ctrl Pts',(89.7140677862562,61.1578867728803,13.1467981516864));
#81397=CARTESIAN_POINT('Ctrl Pts',(88.0267404519492,61.031872528397,14.0830068833467));
#81398=CARTESIAN_POINT('Ctrl Pts',(86.325007417075,60.9058582839138,13.1732459255325));
#81399=CARTESIAN_POINT('Ctrl Pts',(86.1662989650349,60.7798440394306,11.2501307574836));
#81400=CARTESIAN_POINT('Ctrl Pts',(87.695865463759,60.6538297949474,10.0737011385446));
#81401=CARTESIAN_POINT('Ctrl Pts',(89.5138438696553,60.5278155504641,10.7206283663143));
#81402=CARTESIAN_POINT('Ctrl Pts',(89.9564158481913,60.401801305981,12.5988430415177));
#81403=CARTESIAN_POINT('Ctrl Pts',(88.6185384297414,60.2757870614977,13.9893984469357));
#81404=CARTESIAN_POINT('Ctrl Pts',(86.7246403374166,60.1497728170145,13.6196548354655));
#81405=CARTESIAN_POINT('Ctrl Pts',(86.0080217905846,60.0237585725313,11.8280024750253));
#81406=CARTESIAN_POINT('Ctrl Pts',(87.1245338561328,59.8977443280481,10.2541660382186));
#81407=CARTESIAN_POINT('Ctrl Pts',(89.0523419295571,59.7717300835648,10.33852452549));
#81408=CARTESIAN_POINT('Ctrl Pts',(90.0271112928982,59.6457158390816,12.0038728405961));
#81409=CARTESIAN_POINT('Ctrl Pts',(89.1567306133662,59.5197015945983,13.7260800856836));
#81410=CARTESIAN_POINT('Ctrl Pts',(87.2377744420838,59.3936873501152,13.9289779295184));
#81411=CARTESIAN_POINT('Ctrl Pts',(86.026476214272,59.2676731056318,12.4268737634783));
#81412=CARTESIAN_POINT('Ctrl Pts',(86.6314190646277,59.1416588611488,10.5944970363454));
#81413=CARTESIAN_POINT('Ctrl Pts',(88.4989577999506,59.0156446166654,10.1088434618676));
#81414=CARTESIAN_POINT('Ctrl Pts',(89.9199163496109,58.8896303721822,11.4143843928545));
#81415=CARTESIAN_POINT('Ctrl Pts',(89.5938299336816,58.763616127699,13.3162855395183));
#81416=CARTESIAN_POINT('Ctrl Pts',(87.8191336467193,58.6376018832158,14.0739222673615));
#81417=CARTESIAN_POINT('Ctrl Pts',(86.2200339209332,58.5115876387326,12.9939035687612));
#81418=CARTESIAN_POINT('Ctrl Pts',(86.2600307813403,58.3855733942493,11.0646652285107));
#81419=CARTESIAN_POINT('Ctrl Pts',(87.9025190023484,58.2595591497662,10.0518509483069));
#81420=CARTESIAN_POINT('Ctrl Pts',(89.644289300776,58.1335449052829,10.8823908629712));
#81421=CARTESIAN_POINT('Ctrl Pts',(89.8912691905753,58.0075306607997,12.7961727879484));
#81422=CARTESIAN_POINT('Ctrl Pts',(88.4174220656041,57.8815164163164,14.0416987710371));
#81423=CARTESIAN_POINT('Ctrl Pts',(86.5716164607535,57.7555021718333,13.4790603512354));
#81424=CARTESIAN_POINT('Ctrl Pts',(86.0431382318802,57.6294879273499,11.6231856022445));
#81425=CARTESIAN_POINT('Ctrl Pts',(87.3156519614396,57.5034736828668,10.1725756855481));
#81426=CARTESIAN_POINT('Ctrl Pts',(89.2245499360954,57.3774594383835,10.4548323855383));
#81427=CARTESIAN_POINT('Ctrl Pts',(90.0228040070628,57.2514451939003,12.2116336721156));
#81428=CARTESIAN_POINT('Ctrl Pts',(88.9798500738089,57.1254309494171,13.8351506616927));
#81429=CARTESIAN_POINT('Ctrl Pts',(87.0502021561888,56.9994167049339,13.8395365890262));
#81430=CARTESIAN_POINT('Ctrl Pts',(85.999878802121,56.8734024604507,12.2207774425703));
#81431=CARTESIAN_POINT('Ctrl Pts',(86.79013854362,56.7473882159674,10.4603655977736));
#81432=CARTESIAN_POINT('Ctrl Pts',(88.69773371026,56.6213739714842,10.1694343300376));
#81433=CARTESIAN_POINT('Ctrl Pts',(89.9768284863748,56.495359727001,11.6142446553228));
#81434=CARTESIAN_POINT('Ctrl Pts',(89.4567921685402,56.3693454825178,13.472502589644));
#81435=CARTESIAN_POINT('Ctrl Pts',(87.6135632813443,56.2433312380345,14.0435258744077));
#81436=CARTESIAN_POINT('Ctrl Pts',(86.1340694622722,56.1173169935513,12.8047125867561));
#81437=CARTESIAN_POINT('Ctrl Pts',(86.3723471146252,55.9913027490681,10.8898277122208));
#81438=CARTESIAN_POINT('Ctrl Pts',(88.1103239415,55.8652885045849,10.0513786251675));
#81439=CARTESIAN_POINT('Ctrl Pts',(89.757399251399,55.7392742601016,11.0567160042878));
#81440=CARTESIAN_POINT('Ctrl Pts',(89.8061656460392,55.6132600156184,12.9857525931292));
#81441=CARTESIAN_POINT('Ctrl Pts',(88.2119920004042,55.4872457711352,14.0730293333833));
#81442=CARTESIAN_POINT('Ctrl Pts',(86.4338699787695,55.3612315266519,13.3234678625798));
#81443=CARTESIAN_POINT('Ctrl Pts',(86.0991412541919,55.2352172821688,11.4230686931216));
#81444=CARTESIAN_POINT('Ctrl Pts',(87.5141503834826,55.1092030376855,10.1110818462519));
#81445=CARTESIAN_POINT('Ctrl Pts',(89.383877510955,54.9831887932023,10.588240929921));
#81446=CARTESIAN_POINT('Ctrl Pts',(89.9971437440707,54.8571745487191,12.4178487703216));
#81447=CARTESIAN_POINT('Ctrl Pts',(88.7926863091356,54.7311603042359,13.925443745693));
#81448=CARTESIAN_POINT('Ctrl Pts',(86.8728276302837,54.6051460597526,13.7312712049698));
#81449=CARTESIAN_POINT('Ctrl Pts',(85.9946271198952,54.4791318152694,12.0130383377808));
#81450=CARTESIAN_POINT('Ctrl Pts',(86.9618160576386,54.3531175707862,10.3432761148755));
#81451=CARTESIAN_POINT('Ctrl Pts',(88.889220734984,54.2271033263029,10.2501550534444));
#81452=CARTESIAN_POINT('Ctrl Pts',(90.0128756230614,54.1010890818197,11.8188997792793));
#81453=CARTESIAN_POINT('Ctrl Pts',(89.3044089885173,53.9750748373365,13.6137912384136));
#81454=CARTESIAN_POINT('Ctrl Pts',(87.4122112479467,53.8490605928533,13.9921403271053));
#81455=CARTESIAN_POINT('Ctrl Pts',(86.0680264545852,53.72304634837,12.6076810233948));
#81456=CARTESIAN_POINT('Ctrl Pts',(86.5020558566665,53.5970321038868,10.7274739070203));
#81457=CARTESIAN_POINT('Ctrl Pts',(88.3170746716699,53.4710178594036,10.0722891822916));
#81458=CARTESIAN_POINT('Ctrl Pts',(89.8519731899692,53.3450036149203,11.2417535301247));
#81459=CARTESIAN_POINT('Ctrl Pts',(89.7020084904678,53.2189893704372,13.165570286276));
#81460=CARTESIAN_POINT('Ctrl Pts',(88.0044286371382,53.0929751259539,14.0830575962183));
#81461=CARTESIAN_POINT('Ctrl Pts',(86.3128629113647,52.9669608814707,13.1545288041614));
#81462=CARTESIAN_POINT('Ctrl Pts',(86.1754364500773,52.8409466369875,11.2297757576214));
#81463=CARTESIAN_POINT('Ctrl Pts',(87.717922290672,52.7149323925042,10.0703372064778));
#81464=CARTESIAN_POINT('Ctrl Pts',(89.5286335758161,52.5889181480211,10.7373341808814));
#81465=CARTESIAN_POINT('Ctrl Pts',(89.9504028580656,52.4629039035377,12.6203294001193));
#81466=CARTESIAN_POINT('Ctrl Pts',(88.5972258465035,52.3368896590546,13.9960009805844));
#81467=CARTESIAN_POINT('Ctrl Pts',(86.7075334904992,52.2108754145714,13.6053308899133));
#81468=CARTESIAN_POINT('Ctrl Pts',(86.0107769075489,52.0848611700881,11.8058613589148));
#81469=CARTESIAN_POINT('Ctrl Pts',(87.1446294492335,51.9588469256049,10.244471359314));
#81470=CARTESIAN_POINT('Ctrl Pts',(89.0713864580408,51.8328326811216,10.3501488708561));
#81471=CARTESIAN_POINT('Ctrl Pts',(90.0276751656518,51.7068184366385,12.0261775947036));
#81472=CARTESIAN_POINT('Ctrl Pts',(89.1382977557091,51.5808041921552,13.7386518541748));
#81473=CARTESIAN_POINT('Ctrl Pts',(87.2172146848335,51.4547899476721,13.9203110552184));
#81474=CARTESIAN_POINT('Ctrl Pts',(86.0226058303358,51.3287757031887,12.4049000782672));
#81475=CARTESIAN_POINT('Ctrl Pts',(86.6477803745648,51.2027614587056,10.5793271371715));
#81476=CARTESIAN_POINT('Ctrl Pts',(88.5205766211674,51.0767472142223,10.1143604261315));
#81477=CARTESIAN_POINT('Ctrl Pts',(89.9270076260771,50.9507329697391,11.4355399850889));
#81478=CARTESIAN_POINT('Ctrl Pts',(89.5799026261666,50.8247187252559,13.33371630128));
#81479=CARTESIAN_POINT('Ctrl Pts',(87.7969362328594,50.6987044807726,14.071679139239));
#81480=CARTESIAN_POINT('Ctrl Pts',(86.2098771852938,50.5726902362894,12.9740322320388));
#81481=CARTESIAN_POINT('Ctrl Pts',(86.2712188821809,50.4466759918062,11.0453664527095));
#81482=CARTESIAN_POINT('Ctrl Pts',(87.9247951814485,50.320661747323,10.050758069298));
#81483=CARTESIAN_POINT('Ctrl Pts',(89.6573011118424,50.1946475028397,10.9005620003063));
#81484=CARTESIAN_POINT('Ctrl Pts',(89.8830386426052,50.0686332583566,12.8168618216552));
#81485=CARTESIAN_POINT('Ctrl Pts',(88.3956209050421,49.9426190138733,14.0462027928817));
#81486=CARTESIAN_POINT('Ctrl Pts',(86.5559188068883,49.8166047693901,13.4627936570351));
#81487=CARTESIAN_POINT('Ctrl Pts',(86.0484680509088,49.6905905249069,11.6019633223233));
#81488=CARTESIAN_POINT('Ctrl Pts',(87.3360078552799,49.5645762804237,10.1639590209286));
#81489=CARTESIAN_POINT('Ctrl Pts',(89.243817923361,49.4385508029241,10.4705289393977));
#81490=CARTESIAN_POINT('Ctrl Pts',(89.7590111115383,49.3545300735857,11.6428802957186));
#81491=CARTESIAN_POINT('Ctrl Pts',(89.71160828957,49.3125140924083,12.208489101734));
#81492=CARTESIAN_POINT('Ctrl Pts',(87.4571200021394,49.5646,10.4541712921126));
#81493=CARTESIAN_POINT('Ctrl Pts',(87.4645397491564,49.5646,10.4516786262364));
#81494=CARTESIAN_POINT('Ctrl Pts',(87.4719594961734,49.5646,10.4491859603602));
#81495=CARTESIAN_POINT('Ctrl Pts',(87.4793792431904,49.5646,10.446693294484));
#81496=CARTESIAN_POINT('',(87.2206343719404,64.9402624628529,11.0704469075988));
#81497=CARTESIAN_POINT('Ctrl Pts',(87.2198612186734,64.9396,11.0695788312558));
#81498=CARTESIAN_POINT('Ctrl Pts',(87.1759605752479,64.9396,11.0936148929512));
#81499=CARTESIAN_POINT('Ctrl Pts',(87.1337299408,64.9396,11.1204625428497));
#81500=CARTESIAN_POINT('Ctrl Pts',(87.0932536351023,64.9396,11.1498122632398));
#81501=CARTESIAN_POINT('Ctrl Pts',(87.06285156423,64.9396,11.1718570685649));
#81502=CARTESIAN_POINT('Ctrl Pts',(87.0334391262825,64.9396,11.1953146437608));
#81503=CARTESIAN_POINT('Ctrl Pts',(87.0050546235115,64.9396,11.2200722090875));
#81504=CARTESIAN_POINT('Ctrl Pts',(86.9950559696152,64.9396,11.2287932470784));
#81505=CARTESIAN_POINT('Ctrl Pts',(86.9851834629052,64.9396,11.2376770661783));
#81506=CARTESIAN_POINT('Ctrl Pts',(86.9754434689203,64.9396,11.2467149039896));
#81507=CARTESIAN_POINT('Ctrl Pts',(86.9364152092815,64.9396,11.2829296163624));
#81508=CARTESIAN_POINT('Ctrl Pts',(86.8995986840039,64.9396,11.3215328739256));
#81509=CARTESIAN_POINT('Ctrl Pts',(86.8650914925254,64.9396,11.3621996401194));
#81510=CARTESIAN_POINT('Ctrl Pts',(86.8404078686452,64.9396,11.3912893202161));
#81511=CARTESIAN_POINT('Ctrl Pts',(86.816905992572,64.9396,11.4214360951945));
#81512=CARTESIAN_POINT('Ctrl Pts',(86.7946267588473,64.9396,11.452536414632));
#81513=CARTESIAN_POINT('Ctrl Pts',(86.7875511713339,64.9396,11.462413461329));
#81514=CARTESIAN_POINT('Ctrl Pts',(86.7805978697889,64.9396,11.4723883600038));
#81515=CARTESIAN_POINT('Ctrl Pts',(86.7737716954075,64.9396,11.4824529995981));
#81516=CARTESIAN_POINT('Ctrl Pts',(86.7427479749459,64.9396,11.5281949551758));
#81517=CARTESIAN_POINT('Ctrl Pts',(86.7144370065936,64.9396,11.5756547454386));
#81518=CARTESIAN_POINT('Ctrl Pts',(86.6889324487018,64.9396,11.6244990730909));
#81519=CARTESIAN_POINT('Ctrl Pts',(86.6626517910026,64.9396,11.6748297261853));
#81520=CARTESIAN_POINT('Ctrl Pts',(86.6393500200212,64.9396,11.7266310638056));
#81521=CARTESIAN_POINT('Ctrl Pts',(86.619153825068,64.9396,11.7795877023749));
#81522=CARTESIAN_POINT('Ctrl Pts',(86.606400388163,64.9396,11.8130286129156));
#81523=CARTESIAN_POINT('Ctrl Pts',(86.594885871267,64.9396,11.8469311773599));
#81524=CARTESIAN_POINT('Ctrl Pts',(86.5846495052905,64.9396,11.8812237860087));
#81525=CARTESIAN_POINT('Ctrl Pts',(86.5756798766991,64.9396,11.9112727275679));
#81526=CARTESIAN_POINT('Ctrl Pts',(86.567691684042,64.9396,11.9416212794647));
#81527=CARTESIAN_POINT('Ctrl Pts',(86.5607158280894,64.9396,11.9722240399934));
#81528=CARTESIAN_POINT('Ctrl Pts',(86.5585702068065,64.9396,11.9816367822791));
#81529=CARTESIAN_POINT('Ctrl Pts',(86.5565212796045,64.9396,11.9910699427111));
#81530=CARTESIAN_POINT('Ctrl Pts',(86.5545713212498,64.9396,12.0005140259519));
#81531=CARTESIAN_POINT('Ctrl Pts',(86.5426377398758,64.9396,12.0583110222738));
#81532=CARTESIAN_POINT('Ctrl Pts',(86.5343877160295,64.9396,12.1166023576027));
#81533=CARTESIAN_POINT('Ctrl Pts',(86.529943591577,64.9396,12.175050903628));
#81534=CARTESIAN_POINT('Ctrl Pts',(86.5293917345136,64.9396,12.1823088558545));
#81535=CARTESIAN_POINT('Ctrl Pts',(86.5288986098997,64.9396,12.1895692794264));
#81536=CARTESIAN_POINT('Ctrl Pts',(86.5284644930199,64.9396,12.1968315665752));
#81537=CARTESIAN_POINT('Ctrl Pts',(86.5250925617142,64.9396,12.253240184917));
#81538=CARTESIAN_POINT('Ctrl Pts',(86.5252765631312,64.9396,12.3097596931312));
#81539=CARTESIAN_POINT('Ctrl Pts',(86.5288193552493,64.9396,12.3661604963907));
#81540=CARTESIAN_POINT('Ctrl Pts',(86.5307457881762,64.9396,12.3968290653843));
#81541=CARTESIAN_POINT('Ctrl Pts',(86.5336662011508,64.9396,12.4274628778467));
#81542=CARTESIAN_POINT('Ctrl Pts',(86.5375549590848,64.9396,12.4580266898644));
#81543=CARTESIAN_POINT('Ctrl Pts',(86.5404069972119,64.9396,12.4804423708263));
#81544=CARTESIAN_POINT('Ctrl Pts',(86.5437799813636,64.9396,12.5028204237354));
#81545=CARTESIAN_POINT('Ctrl Pts',(86.5476652186841,64.9396,12.5251471167369));
#81546=CARTESIAN_POINT('Ctrl Pts',(86.550187349591,64.9396,12.539640656725));
#81547=CARTESIAN_POINT('Ctrl Pts',(86.5529265884863,64.9396,12.5541177525244));
#81548=CARTESIAN_POINT('Ctrl Pts',(86.5558740228598,64.9396,12.5685436542528));
#81549=CARTESIAN_POINT('Ctrl Pts',(86.5678233329496,64.9396,12.6270282721379));
#81550=CARTESIAN_POINT('Ctrl Pts',(86.5832024740279,64.9396,12.6847536646261));
#81551=CARTESIAN_POINT('Ctrl Pts',(86.6017752752113,64.9396,12.7414644776671));
#81552=CARTESIAN_POINT('Ctrl Pts',(86.6207652315832,64.9396,12.7994490463292));
#81553=CARTESIAN_POINT('Ctrl Pts',(86.6430939545549,64.9396,12.8563738552118));
#81554=CARTESIAN_POINT('Ctrl Pts',(86.6685631613741,64.9396,12.911977439809));
#81555=CARTESIAN_POINT('Ctrl Pts',(86.6942849057222,64.9396,12.9681323565285));
#81556=CARTESIAN_POINT('Ctrl Pts',(86.7232099116878,64.9396,13.0229407764153));
#81557=CARTESIAN_POINT('Ctrl Pts',(86.7551867041488,64.9396,13.07612995671));
#81558=CARTESIAN_POINT('Ctrl Pts',(86.7613170644924,64.9396,13.0863270032708));
#81559=CARTESIAN_POINT('Ctrl Pts',(86.7675597386682,64.9396,13.0964644988554));
#81560=CARTESIAN_POINT('Ctrl Pts',(86.7739138682006,64.9396,13.1065404556599));
#81561=CARTESIAN_POINT('Ctrl Pts',(86.7803293490461,64.9396,13.1167136993038));
#81562=CARTESIAN_POINT('Ctrl Pts',(86.7868542233655,64.9396,13.126817407223));
#81563=CARTESIAN_POINT('Ctrl Pts',(86.7934828292441,64.9396,13.1368434139113));
#81564=CARTESIAN_POINT('Ctrl Pts',(86.82892240913,64.9396,13.1904470632271));
#81565=CARTESIAN_POINT('Ctrl Pts',(86.8673584956895,64.9396,13.2418863883912));
#81566=CARTESIAN_POINT('Ctrl Pts',(86.9085671282906,64.9396,13.2908837724665));
#81567=CARTESIAN_POINT('Ctrl Pts',(86.9498138259472,64.9396,13.3399264161883));
#81568=CARTESIAN_POINT('Ctrl Pts',(86.993838540083,64.9396,13.3865236975521));
#81569=CARTESIAN_POINT('Ctrl Pts',(87.0404676106388,64.9396,13.4303883642256));
#81570=CARTESIAN_POINT('Ctrl Pts',(87.0866458828893,64.9396,13.473828958166));
#81571=CARTESIAN_POINT('Ctrl Pts',(87.1353788326133,64.9396,13.5145905707275));
#81572=CARTESIAN_POINT('Ctrl Pts',(87.186541758314,64.9396,13.5523695888373));
#81573=CARTESIAN_POINT('Ctrl Pts',(87.1962049576915,64.9396,13.5595049545202));
#81574=CARTESIAN_POINT('Ctrl Pts',(87.2059549562448,64.9396,13.5665338266344));
#81575=CARTESIAN_POINT('Ctrl Pts',(87.2157910724421,64.9396,13.5734540116143));
#81576=CARTESIAN_POINT('Ctrl Pts',(87.2213448804068,64.9402624628529,11.0713418717467));
#81577=CARTESIAN_POINT('Ctrl Pts',(87.2248110539969,64.940041641902,11.0685900903627));
#81578=CARTESIAN_POINT('Ctrl Pts',(87.2282916117831,64.939820820951,11.065856427469));
#81579=CARTESIAN_POINT('Ctrl Pts',(87.2317863635668,64.9396,11.0631410324494));
#81580=CARTESIAN_POINT('Origin',(88.011,64.9396,12.066));
#81581=CARTESIAN_POINT('',(88.8267644998355,64.9396,13.5624301241315));
#81582=CARTESIAN_POINT('',(88.011,64.9396,10.36166));
#81583=CARTESIAN_POINT('Origin',(88.011,64.9396,12.066));
#81584=CARTESIAN_POINT('Ctrl Pts',(88.8267644998355,64.9396,13.5624301241314));
#81585=CARTESIAN_POINT('Ctrl Pts',(88.8792239118267,64.9396,13.5241330768566));
#81586=CARTESIAN_POINT('Ctrl Pts',(88.9292651527422,64.9396,13.4825784936921));
#81587=CARTESIAN_POINT('Ctrl Pts',(88.9767194214882,64.9396,13.4380905893019));
#81588=CARTESIAN_POINT('Ctrl Pts',(89.0186917952495,64.9396,13.39874190687));
#81589=CARTESIAN_POINT('Ctrl Pts',(89.0586399546992,64.9396,13.3570974140756));
#81590=CARTESIAN_POINT('Ctrl Pts',(89.0964156918618,64.9396,13.3133685018894));
#81591=CARTESIAN_POINT('Ctrl Pts',(89.1057026187326,64.9396,13.3026180244634));
#81592=CARTESIAN_POINT('Ctrl Pts',(89.1148517489142,64.9396,13.2917488694527));
#81593=CARTESIAN_POINT('Ctrl Pts',(89.1238603732724,64.9396,13.2807656128255));
#81594=CARTESIAN_POINT('Ctrl Pts',(89.1642153727066,64.9396,13.2315650581841));
#81595=CARTESIAN_POINT('Ctrl Pts',(89.2017612778272,64.9396,13.1800684361628));
#81596=CARTESIAN_POINT('Ctrl Pts',(89.2363131557526,64.9396,13.1265745930018));
#81597=CARTESIAN_POINT('Ctrl Pts',(89.2593857598928,64.9396,13.0908531694122));
#81598=CARTESIAN_POINT('Ctrl Pts',(89.2811223081476,64.9396,13.0542407522625));
#81599=CARTESIAN_POINT('Ctrl Pts',(89.3014548131317,64.9396,13.0168249099951));
#81600=CARTESIAN_POINT('Ctrl Pts',(89.3089388815175,64.9396,13.003052739647));
#81601=CARTESIAN_POINT('Ctrl Pts',(89.316234425451,64.9396,12.9891678435316));
#81602=CARTESIAN_POINT('Ctrl Pts',(89.3233253993205,64.9396,12.9751997511491));
#81603=CARTESIAN_POINT('Ctrl Pts',(89.3510266681094,64.9396,12.9206326509628));
#81604=CARTESIAN_POINT('Ctrl Pts',(89.3756487137203,64.9396,12.8647289665995));
#81605=CARTESIAN_POINT('Ctrl Pts',(89.3970346749571,64.9396,12.8077592753298));
#81606=CARTESIAN_POINT('Ctrl Pts',(89.4180965022183,64.9396,12.7516530389365));
#81607=CARTESIAN_POINT('Ctrl Pts',(89.4360197262363,64.9396,12.694511880481));
#81608=CARTESIAN_POINT('Ctrl Pts',(89.4506050688772,64.9396,12.6365941638578));
#81609=CARTESIAN_POINT('Ctrl Pts',(89.4593897614298,64.9396,12.6017105586925));
#81610=CARTESIAN_POINT('Ctrl Pts',(89.4669626385987,64.9396,12.5665453156468));
#81611=CARTESIAN_POINT('Ctrl Pts',(89.4732710163763,64.9396,12.5311570647892));
#81612=CARTESIAN_POINT('Ctrl Pts',(89.4785081647443,64.9396,12.50177811401));
#81613=CARTESIAN_POINT('Ctrl Pts',(89.4828736823687,64.9396,12.4722454765804));
#81614=CARTESIAN_POINT('Ctrl Pts',(89.486333671955,64.9396,12.4425942145647));
#81615=CARTESIAN_POINT('Ctrl Pts',(89.4878648992325,64.9396,12.4294719724081));
#81616=CARTESIAN_POINT('Ctrl Pts',(89.4892188715992,64.9396,12.4163233464084));
#81617=CARTESIAN_POINT('Ctrl Pts',(89.4903906388985,64.9396,12.4031763999801));
#81618=CARTESIAN_POINT('Ctrl Pts',(89.4954420029305,64.9396,12.3465013141025));
#81619=CARTESIAN_POINT('Ctrl Pts',(89.4971238769072,64.9396,12.2897636382346));
#81620=CARTESIAN_POINT('Ctrl Pts',(89.4952673630745,64.9396,12.2331940740218));
#81621=CARTESIAN_POINT('Ctrl Pts',(89.4950289427188,64.9396,12.2259292018803));
#81622=CARTESIAN_POINT('Ctrl Pts',(89.4947320962779,64.9396,12.2186671188516));
#81623=CARTESIAN_POINT('Ctrl Pts',(89.4943764048968,64.9396,12.2114083304016));
#81624=CARTESIAN_POINT('Ctrl Pts',(89.4915291054699,64.9396,12.1533019345514));
#81625=CARTESIAN_POINT('Ctrl Pts',(89.4849146853584,64.9396,12.0954043606453));
#81626=CARTESIAN_POINT('Ctrl Pts',(89.4746786054393,64.9396,12.0380138587617));
#81627=CARTESIAN_POINT('Ctrl Pts',(89.4658080685349,64.9396,11.988279529903));
#81628=CARTESIAN_POINT('Ctrl Pts',(89.4542166247864,64.9396,11.9389259734772));
#81629=CARTESIAN_POINT('Ctrl Pts',(89.4399760645016,64.9396,11.8901692188597));
#81630=CARTESIAN_POINT('Ctrl Pts',(89.4371398843635,64.9396,11.8804587203765));
#81631=CARTESIAN_POINT('Ctrl Pts',(89.4341978223645,64.9396,11.8707696187348));
#81632=CARTESIAN_POINT('Ctrl Pts',(89.4311528313475,64.9396,11.8611115055916));
#81633=CARTESIAN_POINT('Ctrl Pts',(89.4142502690964,64.9396,11.8074998996061));
#81634=CARTESIAN_POINT('Ctrl Pts',(89.3942260903348,64.9396,11.7549818499913));
#81635=CARTESIAN_POINT('Ctrl Pts',(89.3712370268497,64.9396,11.7038177520467));
#81636=CARTESIAN_POINT('Ctrl Pts',(89.3486106528764,64.9396,11.6534608501727));
#81637=CARTESIAN_POINT('Ctrl Pts',(89.3231113234063,64.9396,11.6044147668208));
#81638=CARTESIAN_POINT('Ctrl Pts',(89.294854050429,64.9396,11.5569631056049));
#81639=CARTESIAN_POINT('Ctrl Pts',(89.266830818113,64.9396,11.5099044624337));
#81640=CARTESIAN_POINT('Ctrl Pts',(89.2360943686532,64.9396,11.4644132591656));
#81641=CARTESIAN_POINT('Ctrl Pts',(89.2027349021024,64.9396,11.4208117620039));
#81642=CARTESIAN_POINT('Ctrl Pts',(89.1959684082983,64.9396,11.4119678178136));
#81643=CARTESIAN_POINT('Ctrl Pts',(89.1890939463749,64.9396,11.4032017907954));
#81644=CARTESIAN_POINT('Ctrl Pts',(89.182112201192,64.9396,11.3945166396301));
#81645=CARTESIAN_POINT('Ctrl Pts',(89.1761860368709,64.9396,11.3871446099138));
#81646=CARTESIAN_POINT('Ctrl Pts',(89.1701886137191,64.9396,11.3798383596809));
#81647=CARTESIAN_POINT('Ctrl Pts',(89.1641207087587,64.9396,11.3725992692063));
#81648=CARTESIAN_POINT('Ctrl Pts',(89.1302500105541,64.9396,11.3321910804916));
#81649=CARTESIAN_POINT('Ctrl Pts',(89.094184545402,64.9396,11.2938710507113));
#81650=CARTESIAN_POINT('Ctrl Pts',(89.0560329421154,64.9396,11.2578908221689));
#81651=CARTESIAN_POINT('Ctrl Pts',(89.0176057889962,64.9396,11.2216507265411));
#81652=CARTESIAN_POINT('Ctrl Pts',(88.9770615013913,64.9396,11.1877836370067));
#81653=CARTESIAN_POINT('Ctrl Pts',(88.934492924419,64.9395999999999,11.156598288569));
#81654=CARTESIAN_POINT('Ctrl Pts',(88.894260499953,64.9395999999999,11.1271243839967));
#81655=CARTESIAN_POINT('Ctrl Pts',(88.8522191812581,64.9395999999999,11.1000459568663));
#81656=CARTESIAN_POINT('Ctrl Pts',(88.8084418149977,64.9396,11.0756736932927));
#81657=CARTESIAN_POINT('Ctrl Pts',(88.8058998204431,64.9396,11.0742584834119));
#81658=CARTESIAN_POINT('Ctrl Pts',(88.8033519724573,64.9395999999999,11.0728524126409));
#81659=CARTESIAN_POINT('Ctrl Pts',(88.8007982854172,64.9396,11.0714555473222));
#81660=CARTESIAN_POINT('Origin',(88.011,64.9396,12.066));
#81661=CARTESIAN_POINT('Ctrl Pts',(89.0718796700043,65.1916319044036,10.7293673777971));
#81662=CARTESIAN_POINT('Ctrl Pts',(89.5164413428676,65.1496159224031,11.0821987329325));
#81663=CARTESIAN_POINT('Ctrl Pts',(90.0177633195797,65.0655951922414,12.2604733260601));
#81664=CARTESIAN_POINT('Ctrl Pts',(88.9345264728421,64.9395697139188,13.8604429432028));
#81665=CARTESIAN_POINT('Ctrl Pts',(87.0050126573686,64.8135554694356,13.81368644293));
#81666=CARTESIAN_POINT('Ctrl Pts',(85.9967684956509,64.6875412249523,12.1695349971148));
#81667=CARTESIAN_POINT('Ctrl Pts',(86.8316594286458,64.5615269804691,10.4295873623058));
#81668=CARTESIAN_POINT('Ctrl Pts',(88.7460330609348,64.4355127359859,10.1878084334815));
#81669=CARTESIAN_POINT('Ctrl Pts',(89.9876289924894,64.3094984915027,11.6646952830303));
#81670=CARTESIAN_POINT('Ctrl Pts',(89.4202459804645,64.1834842470194,13.50898705082));
#81671=CARTESIAN_POINT('Ctrl Pts',(87.5630991669237,64.0574700025362,14.0325885979808));
#81672=CARTESIAN_POINT('Ctrl Pts',(86.1158814976775,63.931455758053,12.7563958350616));
#81673=CARTESIAN_POINT('Ctrl Pts',(86.4030763747105,63.8054415135697,10.8483348815267));
#81674=CARTESIAN_POINT('Ctrl Pts',(88.1618492283001,63.6794272690866,10.054692161214));
#81675=CARTESIAN_POINT('Ctrl Pts',(89.7825633469161,63.5534130246033,11.1017992998498));
#81676=CARTESIAN_POINT('Ctrl Pts',(89.7819388816329,63.4273987801201,13.0313473293058));
#81677=CARTESIAN_POINT('Ctrl Pts',(88.1605464839761,63.3013845356368,14.0774060828112));
#81678=CARTESIAN_POINT('Ctrl Pts',(86.4022889175842,63.1753702911537,13.2826215191919));
#81679=CARTESIAN_POINT('Ctrl Pts',(86.1163276419185,63.0493560466704,11.3743816786031));
#81680=CARTESIAN_POINT('Ctrl Pts',(87.564375231372,62.9233418021872,10.0991127631089));
#81681=CARTESIAN_POINT('Ctrl Pts',(89.4211748960676,62.7973275577039,10.6239438494911));
#81682=CARTESIAN_POINT('Ctrl Pts',(89.9873790162293,62.6713133132208,12.4685483238613));
#81683=CARTESIAN_POINT('Ctrl Pts',(88.7447961669459,62.5452990687375,13.9447395605978));
#81684=CARTESIAN_POINT('Ctrl Pts',(86.8306412525868,62.4192848242543,13.7015037115908));
#81685=CARTESIAN_POINT('Ctrl Pts',(85.9967535828063,62.2932705797711,11.9614508157573));
#81686=CARTESIAN_POINT('Ctrl Pts',(87.0063092175991,62.1672563352878,10.3170815939551));
#81687=CARTESIAN_POINT('Ctrl Pts',(88.9353603416485,62.0412420908047,10.2733268229905));
#81688=CARTESIAN_POINT('Ctrl Pts',(90.0184345944058,61.9152278463213,11.8702309789716));
#81689=CARTESIAN_POINT('Ctrl Pts',(89.2642997401459,61.7892136018382,13.6463034270604));
#81690=CARTESIAN_POINT('Ctrl Pts',(87.3631418632286,61.6631993573549,13.976078269349));
#81691=CARTESIAN_POINT('Ctrl Pts',(86.0549053557891,61.5371851128717,12.5577447541679));
#81692=CARTESIAN_POINT('Ctrl Pts',(86.536891505879,61.4111708683884,10.6893652234866));
#81693=CARTESIAN_POINT('Ctrl Pts',(88.3679853965483,61.2851566239053,10.0808852458812));
#81694=CARTESIAN_POINT('Ctrl Pts',(89.8723653691606,61.159142379422,11.2891872021841));
#81695=CARTESIAN_POINT('Ctrl Pts',(89.6732191511257,61.0331281349388,13.2084301527842));
#81696=CARTESIAN_POINT('Ctrl Pts',(87.9528058538541,60.9071138904556,14.0821182013256));
#81697=CARTESIAN_POINT('Ctrl Pts',(86.2856519831005,60.7810996459724,13.110649884383));
#81698=CARTESIAN_POINT('Ctrl Pts',(86.197540885713,60.6550854014891,11.1831154089174));
#81699=CARTESIAN_POINT('Ctrl Pts',(87.7691120559976,60.529071157006,10.063599095359));
#81700=CARTESIAN_POINT('Ctrl Pts',(89.5620596710339,60.4030569125226,10.776685043423));
#81701=CARTESIAN_POINT('Ctrl Pts',(89.9354736380084,60.2770426680396,12.669755229354));
#81702=CARTESIAN_POINT('Ctrl Pts',(88.5476045705647,60.1510284235562,14.0102671357635));
#81703=CARTESIAN_POINT('Ctrl Pts',(86.6686336726467,60.0250141790731,13.5713809496431));
#81704=CARTESIAN_POINT('Ctrl Pts',(86.0181997583719,59.8989999345897,11.754766394281));
#81705=CARTESIAN_POINT('Ctrl Pts',(87.19158155518,59.7729856901067,10.2229936048267));
#81706=CARTESIAN_POINT('Ctrl Pts',(89.1148971398279,59.6469714456233,10.3779448276076));
#81707=CARTESIAN_POINT('Ctrl Pts',(90.0279233311991,59.5209572011402,12.0778083202041));
#81708=CARTESIAN_POINT('Ctrl Pts',(89.095056300235,59.3949429566568,13.7668648089374));
#81709=CARTESIAN_POINT('Ctrl Pts',(87.1700582614733,59.2689287121738,13.8992856167997));
#81710=CARTESIAN_POINT('Ctrl Pts',(86.0146921821982,59.1429144676904,12.3538788928424));
#81711=CARTESIAN_POINT('Ctrl Pts',(86.6863519563968,59.0169002232073,10.5450046939786));
#81712=CARTESIAN_POINT('Ctrl Pts',(88.5703328971182,58.890885978724,10.128149161942));
#81713=CARTESIAN_POINT('Ctrl Pts',(89.9424109866762,58.7648717342408,11.4848195109021));
#81714=CARTESIAN_POINT('Ctrl Pts',(89.5468569631531,58.6388574897575,13.3733876812541));
#81715=CARTESIAN_POINT('Ctrl Pts',(87.7456828474303,58.5128432452744,14.0654314114051));
#81716=CARTESIAN_POINT('Ctrl Pts',(86.1873276461012,58.3868290007911,12.9275905674894));
#81717=CARTESIAN_POINT('Ctrl Pts',(86.298001894603,58.2608147563079,11.0012199047376));
#81718=CARTESIAN_POINT('Ctrl Pts',(87.9764162469118,58.1348005118247,10.0493386193059));
#81719=CARTESIAN_POINT('Ctrl Pts',(89.686481735603,58.0087862673415,10.943110818459));
#81720=CARTESIAN_POINT('Ctrl Pts',(89.8631421949334,57.8827720228582,12.8645539744491));
#81721=CARTESIAN_POINT('Ctrl Pts',(88.3447175354873,57.756757778375,14.0551585574985));
#81722=CARTESIAN_POINT('Ctrl Pts',(86.520873761987,57.6307435338917,13.4252803077902));
#81723=CARTESIAN_POINT('Ctrl Pts',(86.0607972079062,57.5047292894086,11.5513853576991));
#81724=CARTESIAN_POINT('Ctrl Pts',(87.385551073713,57.3787150449253,10.1484670013355));
#81725=CARTESIAN_POINT('Ctrl Pts',(89.2827173441418,57.2527008004422,10.5004795890918));
#81726=CARTESIAN_POINT('Ctrl Pts',(90.0160047551388,57.1266865559588,12.2852603298174));
#81727=CARTESIAN_POINT('Ctrl Pts',(88.9143068540964,57.0006723114758,13.8693734742708));
#81728=CARTESIAN_POINT('Ctrl Pts',(86.985900285514,56.8746580669923,13.8030347537462));
#81729=CARTESIAN_POINT('Ctrl Pts',(85.9956675116008,56.7486438225092,12.1469575293814));
#81730=CARTESIAN_POINT('Ctrl Pts',(86.8498720167566,56.6226295780259,10.4167877738477));
#81731=CARTESIAN_POINT('Ctrl Pts',(88.7667437246655,56.4966153335428,10.1959811276381));
#81732=CARTESIAN_POINT('Ctrl Pts',(89.9919569061429,56.3706010890595,11.6866203796121));
#81733=CARTESIAN_POINT('Ctrl Pts',(89.4041934264733,56.2445868445763,13.5244687987039));
#81734=CARTESIAN_POINT('Ctrl Pts',(87.5413758763049,56.1185726000931,14.0275229651484));
#81735=CARTESIAN_POINT('Ctrl Pts',(86.1083594859353,55.9925583556099,12.7353864613211));
#81736=CARTESIAN_POINT('Ctrl Pts',(86.4166444009374,55.8665441111266,10.8306258121125));
#81737=CARTESIAN_POINT('Ctrl Pts',(88.1840875044425,55.7405298666434,10.0564826758231));
#81738=CARTESIAN_POINT('Ctrl Pts',(89.7931204956846,55.6145156221602,11.1214547659207));
#81739=CARTESIAN_POINT('Ctrl Pts',(89.771152400528,55.488501377677,13.050876990937));
#81740=CARTESIAN_POINT('Ctrl Pts',(88.1382884740062,55.3624871331937,14.0789373573826));
#81741=CARTESIAN_POINT('Ctrl Pts',(86.3889298211781,55.2364728887105,13.2647524745907));
#81742=CARTESIAN_POINT('Ctrl Pts',(86.1240938088108,55.1104586442273,11.3534663614863));
#81743=CARTESIAN_POINT('Ctrl Pts',(87.5861590105954,54.9844443997441,10.0942927970709));
#81744=CARTESIAN_POINT('Ctrl Pts',(89.4370397368875,54.8584301552608,10.6396305425386));
#81745=CARTESIAN_POINT('Ctrl Pts',(89.9828053681324,54.7324159107776,12.4903851441387));
#81746=CARTESIAN_POINT('Ctrl Pts',(88.723969848457,54.6064016662943,13.9527414119461));
#81747=CARTESIAN_POINT('Ctrl Pts',(86.8126225596736,54.4803874218113,13.6883472719729));
#81748=CARTESIAN_POINT('Ctrl Pts',(85.9980332689162,54.3543731773279,11.9391768952013));
#81749=CARTESIAN_POINT('Ctrl Pts',(87.0257161102803,54.2283589328448,10.3060753376864));
#81750=CARTESIAN_POINT('Ctrl Pts',(88.9551332049876,54.1023446883614,10.2836611849593));
#81751=CARTESIAN_POINT('Ctrl Pts',(90.0204772548203,53.9763304438783,11.8924479250456));
#81752=CARTESIAN_POINT('Ctrl Pts',(89.2467427498404,53.850316199395,13.6600699534772));
#81753=CARTESIAN_POINT('Ctrl Pts',(87.3420534231299,53.7243019549118,13.9687952169514));
#81754=CARTESIAN_POINT('Ctrl Pts',(86.0495856584636,53.5982877104286,12.5360775905908));
#81755=CARTESIAN_POINT('Ctrl Pts',(86.5522091514694,53.4722734659454,10.6731437904033));
#81756=CARTESIAN_POINT('Ctrl Pts',(88.3899216379232,53.3462592214621,10.0849554390021));
#81757=CARTESIAN_POINT('Ctrl Pts',(89.8808441039386,53.2202449769789,11.3098239706732));
#81758=CARTESIAN_POINT('Ctrl Pts',(89.6604806202747,53.0942307324956,13.2267466751012));
#81759=CARTESIAN_POINT('Ctrl Pts',(87.9305083923,52.9682164880125,14.0813511508713));
#81760=CARTESIAN_POINT('Ctrl Pts',(86.274202282863,52.8422022435292,13.0915012677515));
#81761=CARTESIAN_POINT('Ctrl Pts',(86.2074177406864,52.716187999046,11.1631100871809));
#81762=CARTESIAN_POINT('Ctrl Pts',(87.7912761442532,52.5901737545628,10.0610459889415));
#81763=CARTESIAN_POINT('Ctrl Pts',(89.5762263638141,52.4641595100796,10.7939207606738));
#81764=CARTESIAN_POINT('Ctrl Pts',(89.9286775437447,52.3381452655963,12.6910056011268));
#81765=CARTESIAN_POINT('Ctrl Pts',(88.5260654901182,52.2121310211131,14.016083765398));
#81766=CARTESIAN_POINT('Ctrl Pts',(86.6520642285717,52.0861167766299,13.5564404509969));
#81767=CARTESIAN_POINT('Ctrl Pts',(86.0217643411852,51.9601025321467,11.7327423332934));
#81768=CARTESIAN_POINT('Ctrl Pts',(87.2120178612602,51.8340882876634,10.2140424873741));
#81769=CARTESIAN_POINT('Ctrl Pts',(89.1335017885094,51.7080740431803,10.3902586769542));
#81770=CARTESIAN_POINT('Ctrl Pts',(90.0276693475674,51.5820597986969,12.1001175941515));
#81771=CARTESIAN_POINT('Ctrl Pts',(89.0761760395382,51.4560455542138,13.7787517583213));
#81772=CARTESIAN_POINT('Ctrl Pts',(87.1498311674703,51.3300313097305,13.8898717692197));
#81773=CARTESIAN_POINT('Ctrl Pts',(86.0116297763121,51.2040170652473,12.3317788383906));
#81774=CARTESIAN_POINT('Ctrl Pts',(86.7032576904153,51.0780028207641,10.530446430839));
#81775=CARTESIAN_POINT('Ctrl Pts',(88.5917331402567,50.9519885762809,10.1344524998545));
#81776=CARTESIAN_POINT('Ctrl Pts',(89.9487231068468,50.8259743317976,11.5062235195118));
#81777=CARTESIAN_POINT('Ctrl Pts',(89.5322982436163,50.6999600873144,13.3902875533465));
#81778=CARTESIAN_POINT('Ctrl Pts',(87.723589165804,50.5739458428312,14.0623919641885));
#81779=CARTESIAN_POINT('Ctrl Pts',(86.1778957835015,50.447931598348,12.9073302450681));
#81780=CARTESIAN_POINT('Ctrl Pts',(86.3099107531474,50.3219173538647,10.9824075787222));
#81781=CARTESIAN_POINT('Ctrl Pts',(87.998673098572,50.1959031093816,10.048938138889));
#81782=CARTESIAN_POINT('Ctrl Pts',(89.6989045810523,50.0698888648982,10.9619953922184));
#81783=CARTESIAN_POINT('Ctrl Pts',(89.8539859089795,49.9438746204151,12.8844261577189));
#81784=CARTESIAN_POINT('Ctrl Pts',(88.3231209088254,49.8178603759318,14.0598673879485));
#81785=CARTESIAN_POINT('Ctrl Pts',(86.5050006083808,49.6918461314486,13.4063554329357));
#81786=CARTESIAN_POINT('Ctrl Pts',(86.215092379416,49.6078366351265,12.1593708946452));
#81787=CARTESIAN_POINT('Ctrl Pts',(86.3659223664004,49.5658318869654,11.6123789721938));
#81788=CARTESIAN_POINT('Ctrl Pts',(88.9809519941789,65.1071878779614,10.8439297557986));
#81789=CARTESIAN_POINT('Ctrl Pts',(89.3874104204466,65.0651718959608,11.166520042142));
#81790=CARTESIAN_POINT('Ctrl Pts',(89.8457642420782,64.9811511657991,12.2438050760703));
#81791=CARTESIAN_POINT('Ctrl Pts',(88.8553712980253,64.8551256874765,13.7066417809788));
#81792=CARTESIAN_POINT('Ctrl Pts',(87.0912355284081,64.7291114429933,13.6638927662105));
#81793=CARTESIAN_POINT('Ctrl Pts',(86.1694076690113,64.60309719851,12.1606610438093));
#81794=CARTESIAN_POINT('Ctrl Pts',(86.9327403525165,64.4770829540269,10.5698437948154));
#81795=CARTESIAN_POINT('Ctrl Pts',(88.6830335994734,64.3510687095436,10.3487876648937));
#81796=CARTESIAN_POINT('Ctrl Pts',(89.8182127190535,64.2250544650604,11.6990909890124));
#81797=CARTESIAN_POINT('Ctrl Pts',(89.2994599334764,64.0990402205772,13.3853090668914));
#81798=CARTESIAN_POINT('Ctrl Pts',(87.6014886119317,63.9730259760939,13.8640328837232));
#81799=CARTESIAN_POINT('Ctrl Pts',(86.2783115316406,63.8470117316107,12.6972222167366));
#81800=CARTESIAN_POINT('Ctrl Pts',(86.5408910225787,63.7209974871275,10.952700590746));
#81801=CARTESIAN_POINT('Ctrl Pts',(88.1489199865423,63.5949832426443,10.2270807480829));
#81802=CARTESIAN_POINT('Ctrl Pts',(89.6307231879736,63.468968998161,11.1844406503936));
#81803=CARTESIAN_POINT('Ctrl Pts',(89.6301522454211,63.3429547536778,12.9486077015236));
#81804=CARTESIAN_POINT('Ctrl Pts',(88.1477289000405,63.2169405091946,13.9050090754766));
#81805=CARTESIAN_POINT('Ctrl Pts',(86.5401710581646,63.0909262647113,13.1783452565515));
#81806=CARTESIAN_POINT('Ctrl Pts',(86.2787194369936,62.9649120202282,11.4336600758624));
#81807=CARTESIAN_POINT('Ctrl Pts',(87.602655305282,62.8388977757449,10.2676940736172));
#81808=CARTESIAN_POINT('Ctrl Pts',(89.300309232004,62.7128835312617,10.7475420462355));
#81809=CARTESIAN_POINT('Ctrl Pts',(89.8179841681831,62.5868692867784,12.4340460287084));
#81810=CARTESIAN_POINT('Ctrl Pts',(88.6819027192945,62.4608550422953,13.7837133607787));
#81811=CARTESIAN_POINT('Ctrl Pts',(86.9318094440195,62.334840797812,13.5613251828629));
#81812=CARTESIAN_POINT('Ctrl Pts',(86.1693940343423,62.2088265533288,11.9704116947348));
#81813=CARTESIAN_POINT('Ctrl Pts',(87.0924209608531,62.0828123088455,10.4669808618608));
#81814=CARTESIAN_POINT('Ctrl Pts',(88.8561336961885,61.9567980643624,10.4269762990892));
#81815=CARTESIAN_POINT('Ctrl Pts',(89.846377982142,61.8307838198791,11.8870102825854));
#81816=CARTESIAN_POINT('Ctrl Pts',(89.1568797982749,61.7047695753959,13.5108560980332));
#81817=CARTESIAN_POINT('Ctrl Pts',(87.4186695882918,61.5787553309127,13.8123660382761));
#81818=CARTESIAN_POINT('Ctrl Pts',(86.2225616364411,61.4527410864295,12.5155974599365));
#81819=CARTESIAN_POINT('Ctrl Pts',(86.6632368993054,61.3267268419462,10.8073561740419));
#81820=CARTESIAN_POINT('Ctrl Pts',(88.3373882861223,61.2007125974631,10.2510288313811));
#81821=CARTESIAN_POINT('Ctrl Pts',(89.7128283060376,61.0746983529797,11.355767592264));
#81822=CARTESIAN_POINT('Ctrl Pts',(89.5307508501508,60.9486841084966,13.1105128097316));
#81823=CARTESIAN_POINT('Ctrl Pts',(87.957793656529,60.8226698640132,13.9093173197375));
#81824=CARTESIAN_POINT('Ctrl Pts',(86.4335310400774,60.6966556195302,13.0211132585772));
#81825=CARTESIAN_POINT('Ctrl Pts',(86.3529719182124,60.5706413750468,11.258787180334));
#81826=CARTESIAN_POINT('Ctrl Pts',(87.7898441985583,60.4446271305637,10.2352242715947));
#81827=CARTESIAN_POINT('Ctrl Pts',(89.4291188154956,60.3186128860804,10.8871918386073));
#81828=CARTESIAN_POINT('Ctrl Pts',(89.7705275842394,60.1925986415973,12.6180075511538));
#81829=CARTESIAN_POINT('Ctrl Pts',(88.5016123550305,60.0665843971139,13.843624587285));
#81830=CARTESIAN_POINT('Ctrl Pts',(86.7836874847833,59.9405701526308,13.4423552035072));
#81831=CARTESIAN_POINT('Ctrl Pts',(86.189002064683,59.8145559081475,11.781442132545));
#81832=CARTESIAN_POINT('Ctrl Pts',(87.2618136623853,59.6885416636643,10.380957125839));
#81833=CARTESIAN_POINT('Ctrl Pts',(89.0202824496677,59.5625274191811,10.5226275261552));
#81834=CARTESIAN_POINT('Ctrl Pts',(89.8550534421729,59.4365131746979,12.0767962326489));
#81835=CARTESIAN_POINT('Ctrl Pts',(89.0021421624386,59.3104989302146,13.6210842003138));
#81836=CARTESIAN_POINT('Ctrl Pts',(87.2421351236761,59.1844846857314,13.7421552607633));
#81837=CARTESIAN_POINT('Ctrl Pts',(86.1857951218026,59.0584704412482,12.3292048799591));
#81838=CARTESIAN_POINT('Ctrl Pts',(86.7998871397895,58.932456196765,10.6753687418796));
#81839=CARTESIAN_POINT('Ctrl Pts',(88.5223926435856,58.8064419522817,10.2942417714836));
#81840=CARTESIAN_POINT('Ctrl Pts',(89.7768703348499,58.6804277077986,11.534632314939));
#81841=CARTESIAN_POINT('Ctrl Pts',(89.4152191271117,58.5544134633152,13.2613318783009));
#81842=CARTESIAN_POINT('Ctrl Pts',(87.7684231003749,58.4283992188321,13.8940607495369));
#81843=CARTESIAN_POINT('Ctrl Pts',(86.3436340522804,58.3023849743488,12.853743900398));
#81844=CARTESIAN_POINT('Ctrl Pts',(86.4448224443983,58.1763707298656,11.0924818848327));
#81845=CARTESIAN_POINT('Ctrl Pts',(87.9793804099347,58.0503564853824,10.2221860566334));
#81846=CARTESIAN_POINT('Ctrl Pts',(89.5428767025218,57.9243422408992,11.0393533107734));
#81847=CARTESIAN_POINT('Ctrl Pts',(89.7043956472854,57.798327996416,12.796110154692));
#81848=CARTESIAN_POINT('Ctrl Pts',(88.3161147063994,57.6723137519327,13.8846683788333));
#81849=CARTESIAN_POINT('Ctrl Pts',(86.6485920314004,57.5462995074495,13.3087768035031));
#81850=CARTESIAN_POINT('Ctrl Pts',(86.2279484996942,57.4202852629663,11.595492823129));
#81851=CARTESIAN_POINT('Ctrl Pts',(87.4391581121195,57.294271018483,10.3128181750045));
#81852=CARTESIAN_POINT('Ctrl Pts',(89.1737188349997,57.1682567739999,10.6346598702733));
#81853=CARTESIAN_POINT('Ctrl Pts',(89.844156403664,57.0422425295165,12.2664675932285));
#81854=CARTESIAN_POINT('Ctrl Pts',(88.8368846966901,56.9162282850334,13.7148068789286));
#81855=CARTESIAN_POINT('Ctrl Pts',(87.0737612721676,56.7902140405501,13.6541540300867));
#81856=CARTESIAN_POINT('Ctrl Pts',(86.1684010499714,56.664199796067,12.1400186840105));
#81857=CARTESIAN_POINT('Ctrl Pts',(86.9493919452058,56.5381855515836,10.5581412552148));
#81858=CARTESIAN_POINT('Ctrl Pts',(88.7019691584764,56.4121713071005,10.3562598799046));
#81859=CARTESIAN_POINT('Ctrl Pts',(89.8221696885362,56.2861570626172,11.7191368921938));
#81860=CARTESIAN_POINT('Ctrl Pts',(89.2847832390352,56.1601428181341,13.3994638788441));
#81861=CARTESIAN_POINT('Ctrl Pts',(87.5816272179853,56.0341285736508,13.8594014247497));
#81862=CARTESIAN_POINT('Ctrl Pts',(86.271434229251,55.9081143291676,12.6780135500685));
#81863=CARTESIAN_POINT('Ctrl Pts',(86.5532961373791,55.7821000846843,10.936509360318));
#81864=CARTESIAN_POINT('Ctrl Pts',(88.1692522267591,55.6560858402012,10.2287177982261));
#81865=CARTESIAN_POINT('Ctrl Pts',(89.6403754867124,55.5300715957179,11.2024114524093));
#81866=CARTESIAN_POINT('Ctrl Pts',(89.6202902703509,55.4040573512348,12.9664634817599));
#81867=CARTESIAN_POINT('Ctrl Pts',(88.1273786173767,55.2780431067514,13.9064091049674));
#81868=CARTESIAN_POINT('Ctrl Pts',(86.5279569658731,55.1520288622683,13.1620077623615));
#81869=CARTESIAN_POINT('Ctrl Pts',(86.2858199680693,55.026014617785,11.4145374042533));
#81870=CARTESIAN_POINT('Ctrl Pts',(87.6225720033731,54.9000003733019,10.2632872254112));
#81871=CARTESIAN_POINT('Ctrl Pts',(89.3148143021131,54.7739861288185,10.7618842375638));
#81872=CARTESIAN_POINT('Ctrl Pts',(89.813802526082,54.6479718843354,12.4540112217209));
#81873=CARTESIAN_POINT('Ctrl Pts',(88.6628614182677,54.5219576398521,13.7910293758668));
#81874=CARTESIAN_POINT('Ctrl Pts',(86.9153351278294,54.3959433953689,13.5492963777076));
#81875=CARTESIAN_POINT('Ctrl Pts',(86.1705640389423,54.2699291508856,11.9500468651766));
#81876=CARTESIAN_POINT('Ctrl Pts',(87.110164494629,54.1439149064024,10.4569179484899));
#81877=CARTESIAN_POINT('Ctrl Pts',(88.8742118333879,54.0179006619192,10.4364249060175));
#81878=CARTESIAN_POINT('Ctrl Pts',(89.8482455667497,53.891886417436,11.9073230209273));
#81879=CARTESIAN_POINT('Ctrl Pts',(89.1408276123014,53.7658721729527,13.5234426996323));
#81880=CARTESIAN_POINT('Ctrl Pts',(87.3993886320191,53.6398579284696,13.8057072140979));
#81881=CARTESIAN_POINT('Ctrl Pts',(86.2176978887654,53.5138436839863,12.4957873823999));
#81882=CARTESIAN_POINT('Ctrl Pts',(86.6772416741224,53.3878294395032,10.7925250750846));
#81883=CARTESIAN_POINT('Ctrl Pts',(88.3574443788803,53.2618151950198,10.25475016948));
#81884=CARTESIAN_POINT('Ctrl Pts',(89.7205803310206,53.1358009505367,11.3746355895643));
#81885=CARTESIAN_POINT('Ctrl Pts',(89.5191041349285,53.0097867060534,13.1272594284577));
#81886=CARTESIAN_POINT('Ctrl Pts',(87.9374073036642,52.8837724615702,13.9086160129458));
#81887=CARTESIAN_POINT('Ctrl Pts',(86.4230626901862,52.7577582170869,13.0036058640888));
#81888=CARTESIAN_POINT('Ctrl Pts',(86.3620022309317,52.6317439726038,11.2404965086763));
#81889=CARTESIAN_POINT('Ctrl Pts',(87.8101086095093,52.5057297281205,10.2328899911565));
#81890=CARTESIAN_POINT('Ctrl Pts',(89.4420712853203,52.3797154836374,10.9029502877427));
#81891=CARTESIAN_POINT('Ctrl Pts',(89.7643139811604,52.253701239154,12.6374365599856));
#81892=CARTESIAN_POINT('Ctrl Pts',(88.4819193826581,52.1276869946709,13.848942675352));
#81893=CARTESIAN_POINT('Ctrl Pts',(86.7685382027512,52.0016727501876,13.4286952504836));
#81894=CARTESIAN_POINT('Ctrl Pts',(86.1922611281809,51.8756585057044,11.7613057471672));
#81895=CARTESIAN_POINT('Ctrl Pts',(87.2804983788489,51.7496442612212,10.3727732059575));
#81896=CARTESIAN_POINT('Ctrl Pts',(89.0372924995348,51.6236300167379,10.5338859591966));
#81897=CARTESIAN_POINT('Ctrl Pts',(89.8548212274014,51.4976157722547,12.0971933854702));
#81898=CARTESIAN_POINT('Ctrl Pts',(88.9848801231789,51.3716015277715,13.6319523228593));
#81899=CARTESIAN_POINT('Ctrl Pts',(87.2236416877859,51.2455872832883,13.7335482712137));
#81900=CARTESIAN_POINT('Ctrl Pts',(86.1829951937994,51.1195730388051,12.3089990144938));
#81901=CARTESIAN_POINT('Ctrl Pts',(86.8153438884555,50.9935587943218,10.6620582630729));
#81902=CARTESIAN_POINT('Ctrl Pts',(88.5419586783537,50.8675445498387,10.3000048522091));
#81903=CARTESIAN_POINT('Ctrl Pts',(89.7826414451086,50.7415303053553,11.5542017924411));
#81904=CARTESIAN_POINT('Ctrl Pts',(89.4019082310255,50.6155160608722,13.2767832674649));
#81905=CARTESIAN_POINT('Ctrl Pts',(87.7482230615222,50.4895018163889,13.8912818124225));
#81906=CARTESIAN_POINT('Ctrl Pts',(86.3350105917728,50.3634875719057,12.835220084087));
#81907=CARTESIAN_POINT('Ctrl Pts',(86.4557105982768,50.2374733274225,11.0752819575934));
#81908=CARTESIAN_POINT('Ctrl Pts',(87.9997296335672,50.1114590829393,10.221819901272));
#81909=CARTESIAN_POINT('Ctrl Pts',(89.5542347896429,49.985444838456,11.0566192934245));
#81910=CARTESIAN_POINT('Ctrl Pts',(89.6960241438328,49.8594305939729,12.814279099141));
#81911=CARTESIAN_POINT('Ctrl Pts',(88.2963691200802,49.7334163494895,13.8889736168488));
#81912=CARTESIAN_POINT('Ctrl Pts',(86.6340793609915,49.6074021050064,13.2914739739516));
#81913=CARTESIAN_POINT('Ctrl Pts',(86.3690190786956,49.5233926086842,12.15136810349));
#81914=CARTESIAN_POINT('Ctrl Pts',(86.5069214730896,49.4813878605231,11.6512586933631));
#81915=CARTESIAN_POINT('Ctrl Pts',(88.8900243183537,65.022743851519,10.9584921338002));
#81916=CARTESIAN_POINT('Ctrl Pts',(89.2583794980258,64.9807278695185,11.2508413513514));
#81917=CARTESIAN_POINT('Ctrl Pts',(89.6737651645768,64.8967071393568,12.2271368260806));
#81918=CARTESIAN_POINT('Ctrl Pts',(88.7762161232086,64.7706816610343,13.5528406187548));
#81919=CARTESIAN_POINT('Ctrl Pts',(87.1774583994475,64.644667416551,13.5140990894909));
#81920=CARTESIAN_POINT('Ctrl Pts',(86.3420468423718,64.5186531720677,12.151787090504));
#81921=CARTESIAN_POINT('Ctrl Pts',(87.0338212763872,64.3926389275846,10.7101002273247));
#81922=CARTESIAN_POINT('Ctrl Pts',(88.6200341380121,64.2666246831013,10.509766896306));
#81923=CARTESIAN_POINT('Ctrl Pts',(89.6487964456177,64.1406104386181,11.7334866949944));
#81924=CARTESIAN_POINT('Ctrl Pts',(89.1786738864885,64.0145961941349,13.2616310829627));
#81925=CARTESIAN_POINT('Ctrl Pts',(87.6398780569399,63.8885819496517,13.6954771694657));
#81926=CARTESIAN_POINT('Ctrl Pts',(86.4407415656038,63.7625677051684,12.6380485984115));
#81927=CARTESIAN_POINT('Ctrl Pts',(86.6787056704468,63.6365534606853,11.0570662999652));
#81928=CARTESIAN_POINT('Ctrl Pts',(88.1359907447846,63.5105392162019,10.3994693349518));
#81929=CARTESIAN_POINT('Ctrl Pts',(89.478883029031,63.3845249717188,11.2670820009376));
#81930=CARTESIAN_POINT('Ctrl Pts',(89.4783656092092,63.2585107272356,12.8658680737414));
#81931=CARTESIAN_POINT('Ctrl Pts',(88.1349113161049,63.1324964827523,13.732612068142));
#81932=CARTESIAN_POINT('Ctrl Pts',(86.678053198745,63.0064822382691,13.0740689939112));
#81933=CARTESIAN_POINT('Ctrl Pts',(86.4411112320687,62.8804679937859,11.4929384731217));
#81934=CARTESIAN_POINT('Ctrl Pts',(87.640935379192,62.7544537493026,10.4362753841254));
#81935=CARTESIAN_POINT('Ctrl Pts',(89.1794435679404,62.6284395048194,10.8711402429799));
#81936=CARTESIAN_POINT('Ctrl Pts',(89.6485893201372,62.5024252603362,12.3995437335558));
#81937=CARTESIAN_POINT('Ctrl Pts',(88.6190092716429,62.3764110158529,13.6226871609596));
#81938=CARTESIAN_POINT('Ctrl Pts',(87.0329776354527,62.2503967713698,13.4211466541349));
#81939=CARTESIAN_POINT('Ctrl Pts',(86.3420344858781,62.1243825268866,11.9793725737123));
#81940=CARTESIAN_POINT('Ctrl Pts',(87.1785327041071,61.9983682824033,10.6168801297665));
#81941=CARTESIAN_POINT('Ctrl Pts',(88.7769070507285,61.8723540379201,10.5806257751877));
#81942=CARTESIAN_POINT('Ctrl Pts',(89.6743213698781,61.7463397934368,11.9037895861992));
#81943=CARTESIAN_POINT('Ctrl Pts',(89.0494598564039,61.6203255489537,13.3754087690061));
#81944=CARTESIAN_POINT('Ctrl Pts',(87.474197313355,61.4943113044703,13.6486538072033));
#81945=CARTESIAN_POINT('Ctrl Pts',(86.3902179170933,61.3682970599872,12.4734501657051));
#81946=CARTESIAN_POINT('Ctrl Pts',(86.7895822927318,61.242282815504,10.9253471245972));
#81947=CARTESIAN_POINT('Ctrl Pts',(88.3067911756965,61.1162685710207,10.421172416881));
#81948=CARTESIAN_POINT('Ctrl Pts',(89.5532912429143,60.9902543265374,11.4223479823439));
#81949=CARTESIAN_POINT('Ctrl Pts',(89.3882825491763,60.8642400820543,13.012595466679));
#81950=CARTESIAN_POINT('Ctrl Pts',(87.9627814592036,60.738225837571,13.7365164381495));
#81951=CARTESIAN_POINT('Ctrl Pts',(86.5814100970547,60.6122115930879,12.9315766327714));
#81952=CARTESIAN_POINT('Ctrl Pts',(86.5084029507116,60.4861973486045,11.3344589517505));
#81953=CARTESIAN_POINT('Ctrl Pts',(87.810576341119,60.3601831041214,10.4068494478305));
#81954=CARTESIAN_POINT('Ctrl Pts',(89.2961779599576,60.2341688596381,10.9976986337916));
#81955=CARTESIAN_POINT('Ctrl Pts',(89.6055815304699,60.108154615155,12.5662598729536));
#81956=CARTESIAN_POINT('Ctrl Pts',(88.4556201394965,59.9821403706717,13.6769820388066));
#81957=CARTESIAN_POINT('Ctrl Pts',(86.8987412969199,59.8561261261885,13.3133294573713));
#81958=CARTESIAN_POINT('Ctrl Pts',(86.3598043709943,59.7301118817052,11.8081178708092));
#81959=CARTESIAN_POINT('Ctrl Pts',(87.3320457695907,59.6040976372221,10.5389206468513));
#81960=CARTESIAN_POINT('Ctrl Pts',(88.9256677595075,59.4780833927388,10.6673102247027));
#81961=CARTESIAN_POINT('Ctrl Pts',(89.6821835531468,59.3520691482556,12.0757841450938));
#81962=CARTESIAN_POINT('Ctrl Pts',(88.9092280246422,59.2260549037723,13.4753035916902));
#81963=CARTESIAN_POINT('Ctrl Pts',(87.314211985879,59.1000406592892,13.585024904727));
#81964=CARTESIAN_POINT('Ctrl Pts',(86.3568980614073,58.9740264148058,12.3045308670758));
#81965=CARTESIAN_POINT('Ctrl Pts',(86.9134223231819,58.8480121703227,10.8057327897807));
#81966=CARTESIAN_POINT('Ctrl Pts',(88.4744523900531,58.7219979258394,10.4603343810253));
#81967=CARTESIAN_POINT('Ctrl Pts',(89.6113296830234,58.5959836813563,11.584445118976));
#81968=CARTESIAN_POINT('Ctrl Pts',(89.2835812910705,58.469969436873,13.1492760753477));
#81969=CARTESIAN_POINT('Ctrl Pts',(87.7911633533195,58.3439551923898,13.7226900876687));
#81970=CARTESIAN_POINT('Ctrl Pts',(86.4999404584594,58.2179409479065,12.7798972333066));
#81971=CARTESIAN_POINT('Ctrl Pts',(86.5916429941938,58.0919267034233,11.1837438649278));
#81972=CARTESIAN_POINT('Ctrl Pts',(87.9823445729578,57.9659124589401,10.3950334939609));
#81973=CARTESIAN_POINT('Ctrl Pts',(89.3992716694407,57.8398982144569,11.1355958030878));
#81974=CARTESIAN_POINT('Ctrl Pts',(89.5456490996371,57.7138839699737,12.727666334935));
#81975=CARTESIAN_POINT('Ctrl Pts',(88.2875118773115,57.5878697254904,13.7141782001681));
#81976=CARTESIAN_POINT('Ctrl Pts',(86.7763103008137,57.4618554810072,13.192273299216));
#81977=CARTESIAN_POINT('Ctrl Pts',(86.3950997914827,57.335841236524,11.639600288559));
#81978=CARTESIAN_POINT('Ctrl Pts',(87.492765150526,57.2098269920407,10.4771693486735));
#81979=CARTESIAN_POINT('Ctrl Pts',(89.0647203258579,57.0838127475576,10.7688401514549));
#81980=CARTESIAN_POINT('Ctrl Pts',(89.6723080521893,56.9577985030743,12.2476748566395));
#81981=CARTESIAN_POINT('Ctrl Pts',(88.759462539284,56.8317842585912,13.5602402835864));
#81982=CARTESIAN_POINT('Ctrl Pts',(87.1616222588214,56.7057700141078,13.5052733064272));
#81983=CARTESIAN_POINT('Ctrl Pts',(86.3411345883419,56.5797557696247,12.1330798386397));
#81984=CARTESIAN_POINT('Ctrl Pts',(87.0489118736551,56.4537415251414,10.6994947365818));
#81985=CARTESIAN_POINT('Ctrl Pts',(88.6371945922872,56.3277272806582,10.5165386321713));
#81986=CARTESIAN_POINT('Ctrl Pts',(89.6523824709294,56.2017130361749,11.7516534047755));
#81987=CARTESIAN_POINT('Ctrl Pts',(89.1653730515974,56.0756987916918,13.2744589589843));
#81988=CARTESIAN_POINT('Ctrl Pts',(87.6218785596657,55.9496845472086,13.6912798843509));
#81989=CARTESIAN_POINT('Ctrl Pts',(86.4345089725667,55.8236703027253,12.620640638816));
#81990=CARTESIAN_POINT('Ctrl Pts',(86.6899478738208,55.6976560582421,11.0423929085234));
#81991=CARTESIAN_POINT('Ctrl Pts',(88.1544169490754,55.5716418137588,10.4009529206292));
#81992=CARTESIAN_POINT('Ctrl Pts',(89.4876304777402,55.4456275692756,11.2833681388979));
#81993=CARTESIAN_POINT('Ctrl Pts',(89.469428140174,55.3196133247924,12.8820499725828));
#81994=CARTESIAN_POINT('Ctrl Pts',(88.1164687607474,55.1935990803092,13.7338808525521));
#81995=CARTESIAN_POINT('Ctrl Pts',(86.6669841105681,55.067584835826,13.0592630501324));
#81996=CARTESIAN_POINT('Ctrl Pts',(86.4475461273278,54.9415705913427,11.4756084470202));
#81997=CARTESIAN_POINT('Ctrl Pts',(87.6589849961508,54.8155563468595,10.4322816537516));
#81998=CARTESIAN_POINT('Ctrl Pts',(89.1925888673385,54.6895421023763,10.8841379325889));
#81999=CARTESIAN_POINT('Ctrl Pts',(89.6447996840317,54.563527857893,12.4176372993032));
#82000=CARTESIAN_POINT('Ctrl Pts',(88.6017529880784,54.4375136134099,13.6293173397875));
#82001=CARTESIAN_POINT('Ctrl Pts',(87.0180476959851,54.3114993689266,13.4102454834423));
#82002=CARTESIAN_POINT('Ctrl Pts',(86.3430948089686,54.1854851244434,11.9609168351518));
#82003=CARTESIAN_POINT('Ctrl Pts',(87.1946128789778,54.0594708799602,10.6077605592933));
#82004=CARTESIAN_POINT('Ctrl Pts',(88.7932904617882,53.9334566354769,10.5891886270757));
#82005=CARTESIAN_POINT('Ctrl Pts',(89.6760138786792,53.8074423909938,11.922198116809));
#82006=CARTESIAN_POINT('Ctrl Pts',(89.0349124747621,53.6814281465105,13.3868154457874));
#82007=CARTESIAN_POINT('Ctrl Pts',(87.4567238409084,53.5554139020273,13.6426192112445));
#82008=CARTESIAN_POINT('Ctrl Pts',(86.385810119067,53.429399657544,12.4554971742089));
#82009=CARTESIAN_POINT('Ctrl Pts',(86.8022741967758,53.3033854130608,10.911906359766));
#82010=CARTESIAN_POINT('Ctrl Pts',(88.324967119837,53.1773711685776,10.4245448999579));
#82011=CARTESIAN_POINT('Ctrl Pts',(89.5603165581028,53.0513569240944,11.4394472084552));
#82012=CARTESIAN_POINT('Ctrl Pts',(89.3777276495823,52.9253426796111,13.0277721818141));
#82013=CARTESIAN_POINT('Ctrl Pts',(87.9443062150286,52.7993284351279,13.7358808750203));
#82014=CARTESIAN_POINT('Ctrl Pts',(86.5719230975097,52.6733141906447,12.9157104604262));
#82015=CARTESIAN_POINT('Ctrl Pts',(86.5165867211766,52.5472999461614,11.3178829301715));
#82016=CARTESIAN_POINT('Ctrl Pts',(87.8289410747657,52.4212857016782,10.4047339933716));
#82017=CARTESIAN_POINT('Ctrl Pts',(89.3079162068262,52.2952714571951,11.0119798148115));
#82018=CARTESIAN_POINT('Ctrl Pts',(89.5999504185763,52.1692572127118,12.5838675188445));
#82019=CARTESIAN_POINT('Ctrl Pts',(88.4377732751979,52.0432429682286,13.6818015853059));
#82020=CARTESIAN_POINT('Ctrl Pts',(86.885012176931,51.9172287237453,13.3009500499704));
#82021=CARTESIAN_POINT('Ctrl Pts',(86.3627579151766,51.7912144792622,11.7898691610409));
#82022=CARTESIAN_POINT('Ctrl Pts',(87.3489788964379,51.6652002347788,10.5315039245408));
#82023=CARTESIAN_POINT('Ctrl Pts',(88.9410832105601,51.5391859902957,10.677513241439));
#82024=CARTESIAN_POINT('Ctrl Pts',(89.6819731072355,51.4131717458124,12.0942691767888));
#82025=CARTESIAN_POINT('Ctrl Pts',(88.8935842068198,51.2871575013293,13.4851528873972));
#82026=CARTESIAN_POINT('Ctrl Pts',(87.2974522081011,51.1611432568459,13.5772247732078));
#82027=CARTESIAN_POINT('Ctrl Pts',(86.3543606112868,51.0351290123629,12.2862191905969));
#82028=CARTESIAN_POINT('Ctrl Pts',(86.9274300864957,50.9091147678794,10.7936700953069));
#82029=CARTESIAN_POINT('Ctrl Pts',(88.4921842164508,50.7831005233964,10.4655572045636));
#82030=CARTESIAN_POINT('Ctrl Pts',(89.6165597833704,50.6570862789131,11.6021800653702));
#82031=CARTESIAN_POINT('Ctrl Pts',(89.2715182184349,50.5310720344298,13.1632789815833));
#82032=CARTESIAN_POINT('Ctrl Pts',(87.7728569572402,50.4050577899467,13.7201716606564));
#82033=CARTESIAN_POINT('Ctrl Pts',(86.4921254000443,50.2790435454634,12.7631099231059));
#82034=CARTESIAN_POINT('Ctrl Pts',(86.6015104434062,50.1530293009802,11.1681563364645));
#82035=CARTESIAN_POINT('Ctrl Pts',(88.0007861685625,50.027015056497,10.3947016636549));
#82036=CARTESIAN_POINT('Ctrl Pts',(89.4095649982335,49.9010008120137,11.1512431946305));
#82037=CARTESIAN_POINT('Ctrl Pts',(89.538062378686,49.7749865675306,12.7441320405629));
#82038=CARTESIAN_POINT('Ctrl Pts',(88.269617331335,49.6489723230473,13.7180798457492));
#82039=CARTESIAN_POINT('Ctrl Pts',(86.7631581136022,49.5229580785641,13.1765925149675));
#82040=CARTESIAN_POINT('Ctrl Pts',(86.5229457779753,49.4389485822419,12.1433653123349));
#82041=CARTESIAN_POINT('Ctrl Pts',(86.6479205797788,49.3969438340809,11.6901384145323));
#82042=CARTESIAN_POINT('Ctrl Pts',(88.7990966425285,64.9382998250767,11.0730545118016));
#82043=CARTESIAN_POINT('Ctrl Pts',(89.1293485756048,64.8962838430762,11.3351626605608));
#82044=CARTESIAN_POINT('Ctrl Pts',(89.5017660870752,64.8122631129146,12.2104685760909));
#82045=CARTESIAN_POINT('Ctrl Pts',(88.697060948392,64.6862376345919,13.3990394565308));
#82046=CARTESIAN_POINT('Ctrl Pts',(87.2636812704869,64.5602233901086,13.3643054127713));
#82047=CARTESIAN_POINT('Ctrl Pts',(86.5146860157324,64.4342091456255,12.1429131371986));
#82048=CARTESIAN_POINT('Ctrl Pts',(87.134902200258,64.3081949011423,10.8503566598342));
#82049=CARTESIAN_POINT('Ctrl Pts',(88.5570346765508,64.1821806566591,10.6707461277182));
#82050=CARTESIAN_POINT('Ctrl Pts',(89.4793801721819,64.0561664121758,11.7678824009764));
#82051=CARTESIAN_POINT('Ctrl Pts',(89.0578878395004,63.9301521676926,13.1379530990341));
#82052=CARTESIAN_POINT('Ctrl Pts',(87.6782675019479,63.8041379232094,13.5269214552082));
#82053=CARTESIAN_POINT('Ctrl Pts',(86.603171599567,63.6781236787262,12.5788749800865));
#82054=CARTESIAN_POINT('Ctrl Pts',(86.8165203183149,63.5521094342429,11.1614320091845));
#82055=CARTESIAN_POINT('Ctrl Pts',(88.123061503027,63.4260951897596,10.5718579218206));
#82056=CARTESIAN_POINT('Ctrl Pts',(89.3270428700885,63.3000809452764,11.3497233514816));
#82057=CARTESIAN_POINT('Ctrl Pts',(89.3265789729973,63.1740667007934,12.7831284459591));
#82058=CARTESIAN_POINT('Ctrl Pts',(88.1220937321693,63.04805245631,13.5602150608074));
#82059=CARTESIAN_POINT('Ctrl Pts',(86.8159353393254,62.9220382118268,12.9697927312709));
#82060=CARTESIAN_POINT('Ctrl Pts',(86.6035030271439,62.7960239673435,11.5522168703809));
#82061=CARTESIAN_POINT('Ctrl Pts',(87.679215453102,62.6700097228603,10.6048566946338));
#82062=CARTESIAN_POINT('Ctrl Pts',(89.0585779038768,62.5439954783771,10.9947384397243));
#82063=CARTESIAN_POINT('Ctrl Pts',(89.4791944720911,62.4179812338939,12.365041438403));
#82064=CARTESIAN_POINT('Ctrl Pts',(88.5561158239914,62.2919669894107,13.4616609611405));
#82065=CARTESIAN_POINT('Ctrl Pts',(87.1341458268856,62.1659527449274,13.280968125407));
#82066=CARTESIAN_POINT('Ctrl Pts',(86.514674937414,62.0399385004443,11.9883334526898));
#82067=CARTESIAN_POINT('Ctrl Pts',(87.2646444473611,61.9139242559609,10.7667793976723));
#82068=CARTESIAN_POINT('Ctrl Pts',(88.6976804052685,61.7879100114779,10.7342752512863));
#82069=CARTESIAN_POINT('Ctrl Pts',(89.5022647576141,61.6618957669944,11.920568889813));
#82070=CARTESIAN_POINT('Ctrl Pts',(88.942039914533,61.5358815225114,13.2399614399788));
#82071=CARTESIAN_POINT('Ctrl Pts',(87.5297250384181,61.409867278028,13.4849415761304));
#82072=CARTESIAN_POINT('Ctrl Pts',(86.5578741977455,61.2838530335449,12.4313028714737));
#82073=CARTESIAN_POINT('Ctrl Pts',(86.9159276861581,61.1578387890616,11.0433380751525));
#82074=CARTESIAN_POINT('Ctrl Pts',(88.2761940652707,61.0318245445784,10.5913160023808));
#82075=CARTESIAN_POINT('Ctrl Pts',(89.3937541797914,60.9058103000952,11.4889283724238));
#82076=CARTESIAN_POINT('Ctrl Pts',(89.2458142482015,60.779796055612,12.9146781236264));
#82077=CARTESIAN_POINT('Ctrl Pts',(87.9677692618783,60.6537818111288,13.5637155565615));
#82078=CARTESIAN_POINT('Ctrl Pts',(86.7292891540317,60.5277675666455,12.8420400069658));
#82079=CARTESIAN_POINT('Ctrl Pts',(86.663833983211,60.4017533221623,11.4101307231672));
#82080=CARTESIAN_POINT('Ctrl Pts',(87.8313084836797,60.2757390776791,10.5784746240662));
#82081=CARTESIAN_POINT('Ctrl Pts',(89.1632371044194,60.1497248331959,11.1082054289759));
#82082=CARTESIAN_POINT('Ctrl Pts',(89.4406354767009,60.0237105887127,12.5145121947534));
#82083=CARTESIAN_POINT('Ctrl Pts',(88.4096279239622,59.8976963442293,13.5103394903283));
#82084=CARTESIAN_POINT('Ctrl Pts',(87.0137951090567,59.7716820997463,13.1843037112354));
#82085=CARTESIAN_POINT('Ctrl Pts',(86.5306066773052,59.6456678552628,11.8347936090732));
#82086=CARTESIAN_POINT('Ctrl Pts',(87.4022778767963,59.5196536107797,10.6968841678635));
#82087=CARTESIAN_POINT('Ctrl Pts',(88.8310530693473,59.3936393662964,10.8119929232504));
#82088=CARTESIAN_POINT('Ctrl Pts',(89.5093136641206,59.2676251218134,12.0747720575386));
#82089=CARTESIAN_POINT('Ctrl Pts',(88.8163138868459,59.14161087733,13.3295229830665));
#82090=CARTESIAN_POINT('Ctrl Pts',(87.3862888480817,59.0155966328469,13.4278945486906));
#82091=CARTESIAN_POINT('Ctrl Pts',(86.5280010010119,58.8895823883636,12.2798568541925));
#82092=CARTESIAN_POINT('Ctrl Pts',(87.0269575065745,58.7635681438805,10.9360968376817));
#82093=CARTESIAN_POINT('Ctrl Pts',(88.4265121365204,58.6375538993971,10.6264269905669));
#82094=CARTESIAN_POINT('Ctrl Pts',(89.4457890311971,58.511539654914,11.6342579230129));
#82095=CARTESIAN_POINT('Ctrl Pts',(89.1519434550291,58.3855254104306,13.0372202723946));
#82096=CARTESIAN_POINT('Ctrl Pts',(87.8139036062642,58.2595111659476,13.5513194258006));
#82097=CARTESIAN_POINT('Ctrl Pts',(86.6562468646385,58.1334969214642,12.7060505662153));
#82098=CARTESIAN_POINT('Ctrl Pts',(86.7384635439892,58.007482676981,11.2750058450229));
#82099=CARTESIAN_POINT('Ctrl Pts',(87.9853087359807,57.8814684324977,10.5678809312884));
#82100=CARTESIAN_POINT('Ctrl Pts',(89.2556666363595,57.7554541880146,11.2318382954022));
#82101=CARTESIAN_POINT('Ctrl Pts',(89.3869025519891,57.6294399435314,12.659222515178));
#82102=CARTESIAN_POINT('Ctrl Pts',(88.2589090482235,57.5034256990482,13.5436880215029));
#82103=CARTESIAN_POINT('Ctrl Pts',(86.904028570227,57.3774114545649,13.0757697949289));
#82104=CARTESIAN_POINT('Ctrl Pts',(86.5622510832708,57.2513972100816,11.6837077539889));
#82105=CARTESIAN_POINT('Ctrl Pts',(87.5463721889326,57.1253829655985,10.6415205223426));
#82106=CARTESIAN_POINT('Ctrl Pts',(88.9557218167158,56.9993687211153,10.9030204326364));
#82107=CARTESIAN_POINT('Ctrl Pts',(89.5004597007143,56.873354476632,12.2288821200505));
#82108=CARTESIAN_POINT('Ctrl Pts',(88.6820403818779,56.7473402321489,13.405673688244));
#82109=CARTESIAN_POINT('Ctrl Pts',(87.2494832454748,56.6213259876655,13.3563925827677));
#82110=CARTESIAN_POINT('Ctrl Pts',(86.5138681267126,56.4953117431823,12.1261409932689));
#82111=CARTESIAN_POINT('Ctrl Pts',(87.1484318021042,56.3692974986991,10.8408482179489));
#82112=CARTESIAN_POINT('Ctrl Pts',(88.5724200260982,56.243283254216,10.6768173844378));
#82113=CARTESIAN_POINT('Ctrl Pts',(89.4825952533226,56.1172690097327,11.7841699173571));
#82114=CARTESIAN_POINT('Ctrl Pts',(89.0459628641595,55.9912547652494,13.1494540391244));
#82115=CARTESIAN_POINT('Ctrl Pts',(87.662129901346,55.8652405207662,13.5231583439522));
#82116=CARTESIAN_POINT('Ctrl Pts',(86.5975837158827,55.7392262762831,12.5632677275634));
#82117=CARTESIAN_POINT('Ctrl Pts',(86.8265996102624,55.6132120317998,11.1482764567289));
#82118=CARTESIAN_POINT('Ctrl Pts',(88.139581671392,55.4871977873166,10.5731880430321));
#82119=CARTESIAN_POINT('Ctrl Pts',(89.334885468768,55.3611835428333,11.3643248253865));
#82120=CARTESIAN_POINT('Ctrl Pts',(89.3185660099971,55.2351692983502,12.7976364634058));
#82121=CARTESIAN_POINT('Ctrl Pts',(88.1055589041179,55.1091550538668,13.5613526001369));
#82122=CARTESIAN_POINT('Ctrl Pts',(86.8060112552633,54.9831408093836,12.9565183379033));
#82123=CARTESIAN_POINT('Ctrl Pts',(86.6092722865862,54.8571265649004,11.536679489787));
#82124=CARTESIAN_POINT('Ctrl Pts',(87.6953979889286,54.7311123204173,10.601276082092));
#82125=CARTESIAN_POINT('Ctrl Pts',(89.070363432564,54.6050980759339,11.0063916276142));
#82126=CARTESIAN_POINT('Ctrl Pts',(89.4757968419816,54.4790838314508,12.3812633768855));
#82127=CARTESIAN_POINT('Ctrl Pts',(88.540644557889,54.3530695869675,13.4676053037081));
#82128=CARTESIAN_POINT('Ctrl Pts',(87.1207602641408,54.2270553424844,13.271194589177));
#82129=CARTESIAN_POINT('Ctrl Pts',(86.5156255789948,54.101041098001,11.971786805127));
#82130=CARTESIAN_POINT('Ctrl Pts',(87.2790612633266,53.975026853518,10.7586031700967));
#82131=CARTESIAN_POINT('Ctrl Pts',(88.7123690901885,53.8490126090346,10.7419523481339));
#82132=CARTESIAN_POINT('Ctrl Pts',(89.5037821906086,53.7229983645515,11.9370732126907));
#82133=CARTESIAN_POINT('Ctrl Pts',(88.928997337223,53.5969841200682,13.2501881919425));
#82134=CARTESIAN_POINT('Ctrl Pts',(87.5140590497977,53.4709698755849,13.479531208391));
#82135=CARTESIAN_POINT('Ctrl Pts',(86.553922349369,53.3449556311017,12.415206966018));
#82136=CARTESIAN_POINT('Ctrl Pts',(86.9273067194287,53.2189413866186,11.0312876444473));
#82137=CARTESIAN_POINT('Ctrl Pts',(88.2924898607941,53.0929271421353,10.5943396304358));
#82138=CARTESIAN_POINT('Ctrl Pts',(89.400052785185,52.9669128976521,11.5042588273461));
#82139=CARTESIAN_POINT('Ctrl Pts',(89.2363511642362,52.8408986531688,12.9282849351706));
#82140=CARTESIAN_POINT('Ctrl Pts',(87.9512051263928,52.7148844086857,13.5631457370948));
#82141=CARTESIAN_POINT('Ctrl Pts',(86.7207835048331,52.5888701642023,12.8278150567635));
#82142=CARTESIAN_POINT('Ctrl Pts',(86.6711712114218,52.4628559197193,11.3952693516667));
#82143=CARTESIAN_POINT('Ctrl Pts',(87.8477735400219,52.3368416752359,10.5765779955867));
#82144=CARTESIAN_POINT('Ctrl Pts',(89.1737611283324,52.2108274307528,11.1210093418804));
#82145=CARTESIAN_POINT('Ctrl Pts',(89.435586855992,52.0848131862694,12.5302984777034));
#82146=CARTESIAN_POINT('Ctrl Pts',(88.3936271677379,51.9587989417864,13.5146604952599));
#82147=CARTESIAN_POINT('Ctrl Pts',(87.0014861511104,51.832784697303,13.1732048494572));
#82148=CARTESIAN_POINT('Ctrl Pts',(86.5332547021724,51.7067704528199,11.8184325749146));
#82149=CARTESIAN_POINT('Ctrl Pts',(87.4174594140269,51.5807562083366,10.6902346431241));
#82150=CARTESIAN_POINT('Ctrl Pts',(88.8448739215852,51.4547419638534,10.8211405236814));
#82151=CARTESIAN_POINT('Ctrl Pts',(89.5091249870697,51.3287277193701,12.0913449681073));
#82152=CARTESIAN_POINT('Ctrl Pts',(88.8022882904604,51.202713474887,13.3383534519352));
#82153=CARTESIAN_POINT('Ctrl Pts',(87.3712627284166,51.0766992304037,13.4209012752018));
#82154=CARTESIAN_POINT('Ctrl Pts',(86.5257260287742,50.9506849859204,12.2634393667001));
#82155=CARTESIAN_POINT('Ctrl Pts',(87.0395162845361,50.8246707414373,10.9252819275408));
#82156=CARTESIAN_POINT('Ctrl Pts',(88.4424097545478,50.698656496954,10.6311095569182));
#82157=CARTESIAN_POINT('Ctrl Pts',(89.4504781216323,50.5726422524708,11.6501583382993));
#82158=CARTESIAN_POINT('Ctrl Pts',(89.1411282058441,50.4466280079875,13.0497746957017));
#82159=CARTESIAN_POINT('Ctrl Pts',(87.7974908529584,50.3206137635044,13.5490615088904));
#82160=CARTESIAN_POINT('Ctrl Pts',(86.6492402083156,50.1945995190211,12.6909997621248));
#82161=CARTESIAN_POINT('Ctrl Pts',(86.7473102885359,50.0685852745379,11.2610307153356));
#82162=CARTESIAN_POINT('Ctrl Pts',(88.0018427035575,49.9425710300547,10.567583426038));
#82163=CARTESIAN_POINT('Ctrl Pts',(89.2648952068242,49.8165567855714,11.2458670958365));
#82164=CARTESIAN_POINT('Ctrl Pts',(89.3801006135392,49.6905425410883,12.673984981985));
#82165=CARTESIAN_POINT('Ctrl Pts',(88.2428655425899,49.564528296605,13.5471860746496));
#82166=CARTESIAN_POINT('Ctrl Pts',(86.8922368662129,49.4385140521219,13.0617110559835));
#82167=CARTESIAN_POINT('Ctrl Pts',(86.6768724772548,49.3545045557997,12.1353625211796));
#82168=CARTESIAN_POINT('Ctrl Pts',(86.788919686468,49.3124998076386,11.7290181357015));
#82169=CARTESIAN_POINT('Ctrl Pts',(88.8060699928714,64.9396,13.5735272939604));
#82170=CARTESIAN_POINT('Ctrl Pts',(88.8129681618595,64.9396,13.5698282373507));
#82171=CARTESIAN_POINT('Ctrl Pts',(88.8198663308475,64.9396,13.5661291807411));
#82172=CARTESIAN_POINT('Ctrl Pts',(88.8267644998355,64.9396,13.5624301241315));
#82173=CARTESIAN_POINT('Origin',(88.011,64.9396,12.066));
#82174=CARTESIAN_POINT('',(88.011,65.0896,10.21166));
#82175=CARTESIAN_POINT('Origin',(88.011,65.0896,12.066));
#82176=CARTESIAN_POINT('Origin',(88.011,64.9396,10.21166));
#82177=CARTESIAN_POINT('Origin',(88.011,65.0896,12.066));
#82178=CARTESIAN_POINT('',(85.1408,65.0896,12.066));
#82179=CARTESIAN_POINT('Origin',(88.011,65.0896,12.066));
#82180=CARTESIAN_POINT('Origin',(88.011,49.3896,12.066));
#82181=CARTESIAN_POINT('',(86.65666,49.2146,12.066));
#82182=CARTESIAN_POINT('',(86.48166,49.3896,12.066));
#82183=CARTESIAN_POINT('Origin',(88.011,49.2146,12.066));
#82184=CARTESIAN_POINT('Origin',(88.011,49.2146,12.066));
#82185=CARTESIAN_POINT('Origin',(91.160821247026,68.5948,11.6730697876423));
#82186=CARTESIAN_POINT('',(90.8451530928687,65.6896,11.6125418584009));
#82187=CARTESIAN_POINT('',(90.8451530928687,68.2948,11.6125418584009));
#82188=CARTESIAN_POINT('',(90.8451530928687,65.0896,11.6125418584009));
#82189=CARTESIAN_POINT('',(90.7194182823342,65.6896,11.5884327817804));
#82190=CARTESIAN_POINT('',(91.160821247026,65.6896,11.6730697876423));
#82191=CARTESIAN_POINT('',(90.7194182823342,68.4148,11.5884327817804));
#82192=CARTESIAN_POINT('',(90.7194182823342,68.5948,11.5884327817804));
#82193=CARTESIAN_POINT('Ctrl Pts',(90.8451530928688,68.2948,11.6125418584009));
#82194=CARTESIAN_POINT('Ctrl Pts',(90.780943418612,68.3562581248798,11.6002299461321));
#82195=CARTESIAN_POINT('Ctrl Pts',(90.7194182823342,68.4148,11.5884327817804));
#82196=CARTESIAN_POINT('Origin',(90.7194182823342,68.5948,11.5884327817804));
#82197=CARTESIAN_POINT('',(90.8293245661282,68.2948,11.5227738224662));
#82198=CARTESIAN_POINT('',(90.8293245661282,65.6896,11.5227738224662));
#82199=CARTESIAN_POINT('',(90.8293245661282,65.0896,11.5227738224662));
#82200=CARTESIAN_POINT('Ctrl Pts',(90.7194182823342,68.4148,11.5884327817804));
#82201=CARTESIAN_POINT('Ctrl Pts',(90.7731981310438,68.356258124881,11.5563042375657));
#82202=CARTESIAN_POINT('Ctrl Pts',(90.8293245661282,68.2948,11.5227738224661));
#82203=CARTESIAN_POINT('',(90.7194182823342,65.6896,11.5884327817804));
#82204=CARTESIAN_POINT('Origin',(90.9262279104668,65.6896,11.5519666644704));
#82205=CARTESIAN_POINT('Origin',(88.011,65.6896,12.066));
#82206=CARTESIAN_POINT('Origin',(88.011,68.4448,12.066));
#82207=CARTESIAN_POINT('',(85.2608,68.4148,12.066));
#82208=CARTESIAN_POINT('',(85.1411618809824,68.2948,12.1115764262924));
#82209=CARTESIAN_POINT('Ctrl Pts',(85.2608,68.4148,12.066));
#82210=CARTESIAN_POINT('Ctrl Pts',(85.2022581248795,68.3562581248795,12.0883016667126));
#82211=CARTESIAN_POINT('Ctrl Pts',(85.1411618809824,68.2948,12.1115764262924));
#82212=CARTESIAN_POINT('',(85.1768469071313,68.2948,12.5194581415991));
#82213=CARTESIAN_POINT('Origin',(88.011,68.2948,12.066));
#82214=CARTESIAN_POINT('',(85.3025817176658,68.4148,12.5435672182196));
#82215=CARTESIAN_POINT('Ctrl Pts',(85.1768469071312,68.2948,12.5194581415991));
#82216=CARTESIAN_POINT('Ctrl Pts',(85.2410565813881,68.3562581248799,12.5317700538679));
#82217=CARTESIAN_POINT('Ctrl Pts',(85.3025817176658,68.4148,12.5435672182196));
#82218=CARTESIAN_POINT('',(85.1926754338717,68.2948,12.6092261775339));
#82219=CARTESIAN_POINT('Ctrl Pts',(85.3025817176658,68.4148,12.5435672182196));
#82220=CARTESIAN_POINT('Ctrl Pts',(85.2488018689554,68.3562581248801,12.5756957624348));
#82221=CARTESIAN_POINT('Ctrl Pts',(85.1926754338717,68.2948,12.6092261775339));
#82222=CARTESIAN_POINT('',(85.2986462408562,68.2948,13.0047146133191));
#82223=CARTESIAN_POINT('Origin',(88.011,68.2948,12.066));
#82224=CARTESIAN_POINT('',(85.4266573543146,68.4148,13.0066237981742));
#82225=CARTESIAN_POINT('Ctrl Pts',(85.2986462408562,68.2948,13.0047146133191));
#82226=CARTESIAN_POINT('Ctrl Pts',(85.3640183670116,68.3562581248796,13.0056895870525));
#82227=CARTESIAN_POINT('Ctrl Pts',(85.4266573543146,68.4148,13.0066237981742));
#82228=CARTESIAN_POINT('',(85.3298223525619,68.2948,13.0903702762566));
#82229=CARTESIAN_POINT('Ctrl Pts',(85.4266573543146,68.4148,13.0066237981742));
#82230=CARTESIAN_POINT('Ctrl Pts',(85.3792736055028,68.3562581248801,13.0476030103342));
#82231=CARTESIAN_POINT('Ctrl Pts',(85.3298223525618,68.2948,13.0903702762567));
#82232=CARTESIAN_POINT('',(85.5028590710356,68.2948,13.4614487165259));
#82233=CARTESIAN_POINT('Origin',(88.011,68.2948,12.066));
#82234=CARTESIAN_POINT('',(85.629256934512,68.4148,13.4411));
#82235=CARTESIAN_POINT('Ctrl Pts',(85.5028590710356,68.2948,13.4614487165259));
#82236=CARTESIAN_POINT('Ctrl Pts',(85.5674073501147,68.3562581248781,13.4510571276407));
#82237=CARTESIAN_POINT('Ctrl Pts',(85.629256934512,68.4148,13.4411));
#82238=CARTESIAN_POINT('',(85.548435497328,68.2948,13.5403894024917));
#82239=CARTESIAN_POINT('Ctrl Pts',(85.629256934512,68.4148,13.4411));
#82240=CARTESIAN_POINT('Ctrl Pts',(85.5897090168301,68.3562581248814,13.4896847474785));
#82241=CARTESIAN_POINT('Ctrl Pts',(85.548435497328,68.2948,13.5403894024917));
#82242=CARTESIAN_POINT('',(85.783280494161,68.2948,13.8757828166121));
#82243=CARTESIAN_POINT('Origin',(88.011,68.2948,12.066));
#82244=CARTESIAN_POINT('',(85.9042245725342,68.4148,13.8337944841599));
#82245=CARTESIAN_POINT('Ctrl Pts',(85.783280494161,68.2948,13.8757828166121));
#82246=CARTESIAN_POINT('Ctrl Pts',(85.8450436593707,68.35625812488,13.8543404082776));
#82247=CARTESIAN_POINT('Ctrl Pts',(85.9042245725342,68.4148,13.8337944841599));
#82248=CARTESIAN_POINT('',(85.8418724183901,68.2948,13.9456099528092));
#82249=CARTESIAN_POINT('Ctrl Pts',(85.9042245725342,68.4148,13.8337944841599));
#82250=CARTESIAN_POINT('Ctrl Pts',(85.8737141294464,68.3562581248792,13.888508543993));
#82251=CARTESIAN_POINT('Ctrl Pts',(85.8418724183901,68.2948,13.9456099528092));
#82252=CARTESIAN_POINT('',(86.1313900471908,68.2948,14.2351275816099));
#82253=CARTESIAN_POINT('Origin',(88.011,68.2948,12.066));
#82254=CARTESIAN_POINT('',(86.2432055158401,68.4148,14.1727754274658));
#82255=CARTESIAN_POINT('Ctrl Pts',(86.1313900471908,68.2948,14.2351275816099));
#82256=CARTESIAN_POINT('Ctrl Pts',(86.1884914560068,68.3562581248789,14.2032858705537));
#82257=CARTESIAN_POINT('Ctrl Pts',(86.2432055158401,68.4148,14.1727754274658));
#82258=CARTESIAN_POINT('',(86.2012171833879,68.2948,14.293719505839));
#82259=CARTESIAN_POINT('Ctrl Pts',(86.2432055158401,68.4148,14.1727754274658));
#82260=CARTESIAN_POINT('Ctrl Pts',(86.2226595917223,68.3562581248796,14.2319563406297));
#82261=CARTESIAN_POINT('Ctrl Pts',(86.2012171833879,68.2948,14.293719505839));
#82262=CARTESIAN_POINT('',(86.5366105975083,68.2948,14.528564502672));
#82263=CARTESIAN_POINT('Origin',(88.011,68.2948,12.066));
#82264=CARTESIAN_POINT('',(86.6359,68.4148,14.447743065488));
#82265=CARTESIAN_POINT('Ctrl Pts',(86.5366105975083,68.2948,14.528564502672));
#82266=CARTESIAN_POINT('Ctrl Pts',(86.5873152525206,68.3562581248803,14.4872909831707));
#82267=CARTESIAN_POINT('Ctrl Pts',(86.6359,68.4148,14.447743065488));
#82268=CARTESIAN_POINT('',(86.6155512834742,68.2948,14.5741409289644));
#82269=CARTESIAN_POINT('Ctrl Pts',(86.6359,68.4148,14.447743065488));
#82270=CARTESIAN_POINT('Ctrl Pts',(86.6259428723596,68.3562581248798,14.5095926498835));
#82271=CARTESIAN_POINT('Ctrl Pts',(86.6155512834741,68.2948,14.5741409289644));
#82272=CARTESIAN_POINT('',(86.9866297237434,68.2948,14.7471776474381));
#82273=CARTESIAN_POINT('Origin',(88.011,68.2948,12.066));
#82274=CARTESIAN_POINT('',(87.0703762018258,68.4148,14.6503426456854));
#82275=CARTESIAN_POINT('Ctrl Pts',(86.9866297237434,68.2948,14.7471776474382));
#82276=CARTESIAN_POINT('Ctrl Pts',(87.029396989666,68.3562581248803,14.697726394497));
#82277=CARTESIAN_POINT('Ctrl Pts',(87.0703762018258,68.4148,14.6503426456854));
#82278=CARTESIAN_POINT('',(87.0722853866809,68.2948,14.7783537591437));
#82279=CARTESIAN_POINT('Ctrl Pts',(87.0703762018258,68.4148,14.6503426456854));
#82280=CARTESIAN_POINT('Ctrl Pts',(87.0713104129475,68.3562581248798,14.7129816329883));
#82281=CARTESIAN_POINT('Ctrl Pts',(87.0722853866809,68.2948,14.7783537591438));
#82282=CARTESIAN_POINT('',(87.4677738224661,68.2948,14.8843245661282));
#82283=CARTESIAN_POINT('Origin',(88.011,68.2948,12.066));
#82284=CARTESIAN_POINT('',(87.5334327817804,68.4148,14.7744182823342));
#82285=CARTESIAN_POINT('Ctrl Pts',(87.4677738224661,68.2948,14.8843245661283));
#82286=CARTESIAN_POINT('Ctrl Pts',(87.5013042375649,68.3562581248796,14.8281981310451));
#82287=CARTESIAN_POINT('Ctrl Pts',(87.5334327817804,68.4148,14.7744182823342));
#82288=CARTESIAN_POINT('',(87.5575418584009,68.2948,14.9001530928687));
#82289=CARTESIAN_POINT('Ctrl Pts',(87.5334327817804,68.4148,14.7744182823342));
#82290=CARTESIAN_POINT('Ctrl Pts',(87.545229946132,68.35625812488,14.8359434186118));
#82291=CARTESIAN_POINT('Ctrl Pts',(87.5575418584008,68.2948,14.9001530928687));
#82292=CARTESIAN_POINT('',(87.9654235737076,68.2948,14.9358381190176));
#82293=CARTESIAN_POINT('Origin',(88.011,68.2948,12.066));
#82294=CARTESIAN_POINT('',(88.011,68.4148,14.8162));
#82295=CARTESIAN_POINT('Ctrl Pts',(87.9654235737076,68.2948,14.9358381190176));
#82296=CARTESIAN_POINT('Ctrl Pts',(87.9886983332876,68.35625812488,14.87474187512));
#82297=CARTESIAN_POINT('Ctrl Pts',(88.011,68.4148,14.8162));
#82298=CARTESIAN_POINT('',(88.0565764262924,68.2948,14.9358381190176));
#82299=CARTESIAN_POINT('Ctrl Pts',(88.011,68.4148,14.8162));
#82300=CARTESIAN_POINT('Ctrl Pts',(88.0333016667125,68.3562581248797,14.8747418751203));
#82301=CARTESIAN_POINT('Ctrl Pts',(88.0565764262924,68.2948,14.9358381190176));
#82302=CARTESIAN_POINT('',(88.4644581415992,68.2948,14.9001530928687));
#82303=CARTESIAN_POINT('Origin',(88.011,68.2948,12.066));
#82304=CARTESIAN_POINT('',(88.4885672182196,68.4148,14.7744182823342));
#82305=CARTESIAN_POINT('Ctrl Pts',(88.4644581415992,68.2948,14.9001530928688));
#82306=CARTESIAN_POINT('Ctrl Pts',(88.476770053868,68.3562581248804,14.8359434186114));
#82307=CARTESIAN_POINT('Ctrl Pts',(88.4885672182196,68.4148,14.7744182823342));
#82308=CARTESIAN_POINT('',(88.5542261775338,68.2948,14.8843245661282));
#82309=CARTESIAN_POINT('Ctrl Pts',(88.4885672182196,68.4148,14.7744182823342));
#82310=CARTESIAN_POINT('Ctrl Pts',(88.5206957624349,68.3562581248798,14.8281981310449));
#82311=CARTESIAN_POINT('Ctrl Pts',(88.5542261775338,68.2948,14.8843245661283));
#82312=CARTESIAN_POINT('',(88.9497146133191,68.2948,14.7783537591437));
#82313=CARTESIAN_POINT('Origin',(88.011,68.2948,12.066));
#82314=CARTESIAN_POINT('',(88.9516237981743,68.4148,14.6503426456854));
#82315=CARTESIAN_POINT('Ctrl Pts',(88.9497146133191,68.2948,14.7783537591438));
#82316=CARTESIAN_POINT('Ctrl Pts',(88.9506895870525,68.3562581248811,14.7129816329868));
#82317=CARTESIAN_POINT('Ctrl Pts',(88.9516237981743,68.4148,14.6503426456854));
#82318=CARTESIAN_POINT('',(89.0353702762567,68.2948,14.7471776474381));
#82319=CARTESIAN_POINT('Ctrl Pts',(88.9516237981743,68.4148,14.6503426456854));
#82320=CARTESIAN_POINT('Ctrl Pts',(88.9926030103332,68.3562581248815,14.6977263944961));
#82321=CARTESIAN_POINT('Ctrl Pts',(89.0353702762566,68.2948,14.7471776474381));
#82322=CARTESIAN_POINT('',(89.4064487165259,68.2948,14.5741409289644));
#82323=CARTESIAN_POINT('Origin',(88.011,68.2948,12.066));
#82324=CARTESIAN_POINT('',(89.3861,68.4148,14.447743065488));
#82325=CARTESIAN_POINT('Ctrl Pts',(89.4064487165259,68.2948,14.5741409289644));
#82326=CARTESIAN_POINT('Ctrl Pts',(89.3960571276401,68.3562581248814,14.5095926498817));
#82327=CARTESIAN_POINT('Ctrl Pts',(89.3861,68.4148,14.447743065488));
#82328=CARTESIAN_POINT('',(89.4853894024917,68.2948,14.528564502672));
#82329=CARTESIAN_POINT('Ctrl Pts',(89.3861,68.4148,14.447743065488));
#82330=CARTESIAN_POINT('Ctrl Pts',(89.4346847474787,68.3562581248812,14.4872909831701));
#82331=CARTESIAN_POINT('Ctrl Pts',(89.4853894024917,68.2948,14.528564502672));
#82332=CARTESIAN_POINT('',(89.8207828166121,68.2948,14.293719505839));
#82333=CARTESIAN_POINT('Origin',(88.011,68.2948,12.066));
#82334=CARTESIAN_POINT('',(89.7787944841599,68.4148,14.1727754274658));
#82335=CARTESIAN_POINT('Ctrl Pts',(89.8207828166121,68.2948,14.293719505839));
#82336=CARTESIAN_POINT('Ctrl Pts',(89.7993404082776,68.35625812488,14.2319563406293));
#82337=CARTESIAN_POINT('Ctrl Pts',(89.7787944841599,68.4148,14.1727754274658));
#82338=CARTESIAN_POINT('',(89.8906099528091,68.2948,14.2351275816099));
#82339=CARTESIAN_POINT('Ctrl Pts',(89.7787944841599,68.4148,14.1727754274658));
#82340=CARTESIAN_POINT('Ctrl Pts',(89.8335085439913,68.3562581248809,14.2032858705527));
#82341=CARTESIAN_POINT('Ctrl Pts',(89.8906099528091,68.2948,14.2351275816099));
#82342=CARTESIAN_POINT('',(90.1801275816099,68.2948,13.9456099528092));
#82343=CARTESIAN_POINT('Origin',(88.011,68.2948,12.066));
#82344=CARTESIAN_POINT('',(90.1177754274658,68.4148,13.8337944841599));
#82345=CARTESIAN_POINT('Ctrl Pts',(90.1801275816099,68.2948,13.9456099528092));
#82346=CARTESIAN_POINT('Ctrl Pts',(90.1482858705531,68.3562581248803,13.8885085439919));
#82347=CARTESIAN_POINT('Ctrl Pts',(90.1177754274658,68.4148,13.8337944841599));
#82348=CARTESIAN_POINT('',(90.238719505839,68.2948,13.8757828166121));
#82349=CARTESIAN_POINT('Ctrl Pts',(90.1177754274658,68.4148,13.8337944841599));
#82350=CARTESIAN_POINT('Ctrl Pts',(90.176956340628,68.3562581248813,13.8543404082771));
#82351=CARTESIAN_POINT('Ctrl Pts',(90.238719505839,68.2948,13.8757828166121));
#82352=CARTESIAN_POINT('',(90.473564502672,68.2948,13.5403894024917));
#82353=CARTESIAN_POINT('Origin',(88.011,68.2948,12.066));
#82354=CARTESIAN_POINT('',(90.392743065488,68.4148,13.4411));
#82355=CARTESIAN_POINT('Ctrl Pts',(90.473564502672,68.2948,13.5403894024917));
#82356=CARTESIAN_POINT('Ctrl Pts',(90.4322909831698,68.3562581248816,13.4896847474783));
#82357=CARTESIAN_POINT('Ctrl Pts',(90.392743065488,68.4148,13.4411));
#82358=CARTESIAN_POINT('',(90.5191409289644,68.2948,13.4614487165259));
#82359=CARTESIAN_POINT('Ctrl Pts',(90.392743065488,68.4148,13.4411));
#82360=CARTESIAN_POINT('Ctrl Pts',(90.4545926498819,68.3562581248813,13.4510571276401));
#82361=CARTESIAN_POINT('Ctrl Pts',(90.5191409289644,68.2948,13.4614487165259));
#82362=CARTESIAN_POINT('',(90.6921776474381,68.2948,13.0903702762567));
#82363=CARTESIAN_POINT('Origin',(88.011,68.2948,12.066));
#82364=CARTESIAN_POINT('',(90.5953426456854,68.4148,13.0066237981743));
#82365=CARTESIAN_POINT('Ctrl Pts',(90.6921776474381,68.2948,13.0903702762567));
#82366=CARTESIAN_POINT('Ctrl Pts',(90.6427263944977,68.3562581248795,13.0476030103346));
#82367=CARTESIAN_POINT('Ctrl Pts',(90.5953426456854,68.4148,13.0066237981743));
#82368=CARTESIAN_POINT('',(90.7233537591437,68.2948,13.0047146133191));
#82369=CARTESIAN_POINT('Ctrl Pts',(90.5953426456854,68.4148,13.0066237981743));
#82370=CARTESIAN_POINT('Ctrl Pts',(90.6579816329875,68.3562581248805,13.0056895870525));
#82371=CARTESIAN_POINT('Ctrl Pts',(90.7233537591438,68.2948,13.0047146133191));
#82372=CARTESIAN_POINT('',(90.8293245661282,68.2948,12.6092261775338));
#82373=CARTESIAN_POINT('Origin',(88.011,68.2948,12.066));
#82374=CARTESIAN_POINT('',(90.7194182823342,68.4148,12.5435672182196));
#82375=CARTESIAN_POINT('Ctrl Pts',(90.8293245661282,68.2948,12.6092261775338));
#82376=CARTESIAN_POINT('Ctrl Pts',(90.7731981310446,68.3562581248802,12.5756957624347));
#82377=CARTESIAN_POINT('Ctrl Pts',(90.7194182823342,68.4148,12.5435672182196));
#82378=CARTESIAN_POINT('',(90.8451530928687,68.2948,12.5194581415991));
#82379=CARTESIAN_POINT('Ctrl Pts',(90.7194182823342,68.4148,12.5435672182196));
#82380=CARTESIAN_POINT('Ctrl Pts',(90.7809434186119,68.3562581248799,12.5317700538679));
#82381=CARTESIAN_POINT('Ctrl Pts',(90.8451530928687,68.2948,12.5194581415991));
#82382=CARTESIAN_POINT('',(90.8808381190176,68.2948,12.1115764262924));
#82383=CARTESIAN_POINT('Origin',(88.011,68.2948,12.066));
#82384=CARTESIAN_POINT('',(90.7612,68.4148,12.066));
#82385=CARTESIAN_POINT('Ctrl Pts',(90.8808381190176,68.2948,12.1115764262924));
#82386=CARTESIAN_POINT('Ctrl Pts',(90.81974187512,68.35625812488,12.0883016667124));
#82387=CARTESIAN_POINT('Ctrl Pts',(90.7612,68.4148,12.066));
#82388=CARTESIAN_POINT('',(90.8808381190176,68.2948,12.0204235737076));
#82389=CARTESIAN_POINT('Ctrl Pts',(90.7612,68.4148,12.066));
#82390=CARTESIAN_POINT('Ctrl Pts',(90.8197418751187,68.3562581248813,12.0436983332881));
#82391=CARTESIAN_POINT('Ctrl Pts',(90.8808381190176,68.2948,12.0204235737076));
#82392=CARTESIAN_POINT('Origin',(88.011,68.2948,12.066));
#82393=CARTESIAN_POINT('',(90.7233537591437,68.2948,11.1272853866809));
#82394=CARTESIAN_POINT('Origin',(88.011,68.2948,12.066));
#82395=CARTESIAN_POINT('',(90.5953426456854,68.4148,11.1253762018257));
#82396=CARTESIAN_POINT('Ctrl Pts',(90.7233537591438,68.2948,11.1272853866809));
#82397=CARTESIAN_POINT('Ctrl Pts',(90.6579816329897,68.3562581248785,11.1263104129475));
#82398=CARTESIAN_POINT('Ctrl Pts',(90.5953426456854,68.4148,11.1253762018257));
#82399=CARTESIAN_POINT('',(90.6921776474381,68.2948,11.0416297237434));
#82400=CARTESIAN_POINT('Ctrl Pts',(90.5953426456854,68.4148,11.1253762018257));
#82401=CARTESIAN_POINT('Ctrl Pts',(90.6427263944974,68.3562581248798,11.0843969896657));
#82402=CARTESIAN_POINT('Ctrl Pts',(90.6921776474382,68.2948,11.0416297237433));
#82403=CARTESIAN_POINT('',(90.5191409289644,68.2948,10.6705512834741));
#82404=CARTESIAN_POINT('Origin',(88.011,68.2948,12.066));
#82405=CARTESIAN_POINT('',(90.392743065488,68.4148,10.6909));
#82406=CARTESIAN_POINT('Ctrl Pts',(90.5191409289644,68.2948,10.6705512834741));
#82407=CARTESIAN_POINT('Ctrl Pts',(90.4545926498816,68.3562581248815,10.6809428723599));
#82408=CARTESIAN_POINT('Ctrl Pts',(90.392743065488,68.4148,10.6909));
#82409=CARTESIAN_POINT('',(90.473564502672,68.2948,10.5916105975083));
#82410=CARTESIAN_POINT('Ctrl Pts',(90.392743065488,68.4148,10.6909));
#82411=CARTESIAN_POINT('Ctrl Pts',(90.4322909831703,68.3562581248808,10.642315252521));
#82412=CARTESIAN_POINT('Ctrl Pts',(90.473564502672,68.2948,10.5916105975082));
#82413=CARTESIAN_POINT('',(90.238719505839,68.2948,10.2562171833879));
#82414=CARTESIAN_POINT('Origin',(88.011,68.2948,12.066));
#82415=CARTESIAN_POINT('',(90.1177754274658,68.4148,10.2982055158401));
#82416=CARTESIAN_POINT('Ctrl Pts',(90.238719505839,68.2948,10.2562171833879));
#82417=CARTESIAN_POINT('Ctrl Pts',(90.1769563406299,68.3562581248795,10.2776595917222));
#82418=CARTESIAN_POINT('Ctrl Pts',(90.1177754274658,68.4148,10.2982055158401));
#82419=CARTESIAN_POINT('',(90.1801275816099,68.2948,10.1863900471908));
#82420=CARTESIAN_POINT('Ctrl Pts',(90.1177754274658,68.4148,10.2982055158401));
#82421=CARTESIAN_POINT('Ctrl Pts',(90.1482858705526,68.3562581248811,10.2434914560088));
#82422=CARTESIAN_POINT('Ctrl Pts',(90.1801275816099,68.2948,10.1863900471908));
#82423=CARTESIAN_POINT('',(89.8906099528092,68.2948,9.89687241839011));
#82424=CARTESIAN_POINT('Origin',(88.011,68.2948,12.066));
#82425=CARTESIAN_POINT('',(89.7787944841599,68.4148,9.95922457253419));
#82426=CARTESIAN_POINT('Ctrl Pts',(89.8906099528092,68.2948,9.8968724183901));
#82427=CARTESIAN_POINT('Ctrl Pts',(89.8335085439914,68.3562581248809,9.92871412944728));
#82428=CARTESIAN_POINT('Ctrl Pts',(89.7787944841599,68.4148,9.95922457253419));
#82429=CARTESIAN_POINT('',(89.8207828166121,68.2948,9.838280494161));
#82430=CARTESIAN_POINT('Ctrl Pts',(89.7787944841599,68.4148,9.95922457253419));
#82431=CARTESIAN_POINT('Ctrl Pts',(89.7993404082777,68.3562581248795,9.9000436593701));
#82432=CARTESIAN_POINT('Ctrl Pts',(89.8207828166121,68.2948,9.83828049416098));
#82433=CARTESIAN_POINT('',(89.4853894024917,68.2948,9.60343549732802));
#82434=CARTESIAN_POINT('Origin',(88.011,68.2948,12.066));
#82435=CARTESIAN_POINT('',(89.3861,68.4148,9.68425693451204));
#82436=CARTESIAN_POINT('Ctrl Pts',(89.4853894024917,68.2948,9.60343549732801));
#82437=CARTESIAN_POINT('Ctrl Pts',(89.4346847474794,68.3562581248803,9.64470901682936));
#82438=CARTESIAN_POINT('Ctrl Pts',(89.3861,68.4148,9.68425693451204));
#82439=CARTESIAN_POINT('',(89.4064487165258,68.2948,9.55785907103561));
#82440=CARTESIAN_POINT('Ctrl Pts',(89.3861,68.4148,9.68425693451204));
#82441=CARTESIAN_POINT('Ctrl Pts',(89.3960571276404,68.3562581248794,9.62240735011616));
#82442=CARTESIAN_POINT('Ctrl Pts',(89.4064487165259,68.2948,9.5578590710356));
#82443=CARTESIAN_POINT('',(89.0353702762566,68.2948,9.38482235256186));
#82444=CARTESIAN_POINT('Origin',(88.011,68.2948,12.066));
#82445=CARTESIAN_POINT('',(88.9516237981742,68.4148,9.48165735431459));
#82446=CARTESIAN_POINT('Ctrl Pts',(89.0353702762567,68.2948,9.38482235256184));
#82447=CARTESIAN_POINT('Ctrl Pts',(88.9926030103341,68.3562581248802,9.4342736055029));
#82448=CARTESIAN_POINT('Ctrl Pts',(88.9516237981742,68.4148,9.48165735431459));
#82449=CARTESIAN_POINT('',(88.9497146133191,68.2948,9.35364624085626));
#82450=CARTESIAN_POINT('Ctrl Pts',(88.9516237981742,68.4148,9.48165735431459));
#82451=CARTESIAN_POINT('Ctrl Pts',(88.9506895870525,68.3562581248798,9.41901836701178));
#82452=CARTESIAN_POINT('Ctrl Pts',(88.9497146133191,68.2948,9.35364624085623));
#82453=CARTESIAN_POINT('',(88.5542261775338,68.2948,9.24767543387175));
#82454=CARTESIAN_POINT('Origin',(88.011,68.2948,12.066));
#82455=CARTESIAN_POINT('',(88.4885672182196,68.4148,9.35758171766581));
#82456=CARTESIAN_POINT('Ctrl Pts',(88.5542261775338,68.2948,9.24767543387173));
#82457=CARTESIAN_POINT('Ctrl Pts',(88.5206957624345,68.3562581248806,9.30380186895581));
#82458=CARTESIAN_POINT('Ctrl Pts',(88.4885672182196,68.4148,9.35758171766581));
#82459=CARTESIAN_POINT('',(88.4644581415991,68.2948,9.23184690713126));
#82460=CARTESIAN_POINT('Ctrl Pts',(88.4885672182196,68.4148,9.35758171766581));
#82461=CARTESIAN_POINT('Ctrl Pts',(88.4767700538679,68.3562581248799,9.29605658138816));
#82462=CARTESIAN_POINT('Ctrl Pts',(88.4644581415991,68.2948,9.23184690713123));
#82463=CARTESIAN_POINT('',(88.0565764262924,68.2948,9.19616188098241));
#82464=CARTESIAN_POINT('Origin',(88.011,68.2948,12.066));
#82465=CARTESIAN_POINT('',(88.011,68.4148,9.3158));
#82466=CARTESIAN_POINT('Ctrl Pts',(88.0565764262924,68.2948,9.19616188098239));
#82467=CARTESIAN_POINT('Ctrl Pts',(88.0333016667122,68.3562581248804,9.25725812488037));
#82468=CARTESIAN_POINT('Ctrl Pts',(88.011,68.4148,9.3158));
#82469=CARTESIAN_POINT('',(87.9654235737076,68.2948,9.19616188098241));
#82470=CARTESIAN_POINT('Ctrl Pts',(88.011,68.4148,9.3158));
#82471=CARTESIAN_POINT('Ctrl Pts',(87.9886983332877,68.3562581248803,9.2572581248803));
#82472=CARTESIAN_POINT('Ctrl Pts',(87.9654235737076,68.2948,9.19616188098239));
#82473=CARTESIAN_POINT('',(87.5575418584008,68.2948,9.23184690713126));
#82474=CARTESIAN_POINT('Origin',(88.011,68.2948,12.066));
#82475=CARTESIAN_POINT('',(87.5334327817804,68.4148,9.35758171766581));
#82476=CARTESIAN_POINT('Ctrl Pts',(87.5575418584008,68.2948,9.23184690713124));
#82477=CARTESIAN_POINT('Ctrl Pts',(87.545229946132,68.3562581248804,9.29605658138868));
#82478=CARTESIAN_POINT('Ctrl Pts',(87.5334327817804,68.4148,9.35758171766581));
#82479=CARTESIAN_POINT('',(87.4677738224661,68.2948,9.24767543387176));
#82480=CARTESIAN_POINT('Ctrl Pts',(87.5334327817804,68.4148,9.35758171766581));
#82481=CARTESIAN_POINT('Ctrl Pts',(87.5013042375654,68.3562581248805,9.30380186895576));
#82482=CARTESIAN_POINT('Ctrl Pts',(87.4677738224661,68.2948,9.24767543387173));
#82483=CARTESIAN_POINT('',(87.0722853866809,68.2948,9.35364624085626));
#82484=CARTESIAN_POINT('Origin',(88.011,68.2948,12.066));
#82485=CARTESIAN_POINT('',(87.0703762018258,68.4148,9.48165735431459));
#82486=CARTESIAN_POINT('Ctrl Pts',(87.0722853866809,68.2948,9.35364624085623));
#82487=CARTESIAN_POINT('Ctrl Pts',(87.0713104129475,68.3562581248812,9.41901836701324));
#82488=CARTESIAN_POINT('Ctrl Pts',(87.0703762018258,68.4148,9.48165735431459));
#82489=CARTESIAN_POINT('',(86.9866297237434,68.2948,9.38482235256186));
#82490=CARTESIAN_POINT('Ctrl Pts',(87.0703762018257,68.4148,9.48165735431459));
#82491=CARTESIAN_POINT('Ctrl Pts',(87.0293969896666,68.3562581248812,9.43427360550364));
#82492=CARTESIAN_POINT('Ctrl Pts',(86.9866297237434,68.2948,9.38482235256185));
#82493=CARTESIAN_POINT('',(86.6155512834741,68.2948,9.55785907103562));
#82494=CARTESIAN_POINT('Origin',(88.011,68.2948,12.066));
#82495=CARTESIAN_POINT('',(86.6359,68.4148,9.68425693451204));
#82496=CARTESIAN_POINT('Ctrl Pts',(86.6155512834741,68.2948,9.55785907103559));
#82497=CARTESIAN_POINT('Ctrl Pts',(86.6259428723597,68.3562581248802,9.62240735011689));
#82498=CARTESIAN_POINT('Ctrl Pts',(86.6359,68.4148,9.68425693451204));
#82499=CARTESIAN_POINT('',(86.5366105975083,68.2948,9.60343549732803));
#82500=CARTESIAN_POINT('Ctrl Pts',(86.6359,68.4148,9.68425693451204));
#82501=CARTESIAN_POINT('Ctrl Pts',(86.587315252521,68.3562581248808,9.64470901682966));
#82502=CARTESIAN_POINT('Ctrl Pts',(86.5366105975082,68.2948,9.60343549732803));
#82503=CARTESIAN_POINT('',(86.2012171833879,68.2948,9.838280494161));
#82504=CARTESIAN_POINT('Origin',(88.011,68.2948,12.066));
#82505=CARTESIAN_POINT('',(86.2432055158401,68.4148,9.95922457253419));
#82506=CARTESIAN_POINT('Ctrl Pts',(86.2012171833879,68.2948,9.83828049416098));
#82507=CARTESIAN_POINT('Ctrl Pts',(86.2226595917224,68.35625812488,9.90004365937064));
#82508=CARTESIAN_POINT('Ctrl Pts',(86.2432055158401,68.4148,9.95922457253419));
#82509=CARTESIAN_POINT('',(86.1313900471908,68.2948,9.89687241839012));
#82510=CARTESIAN_POINT('Ctrl Pts',(86.2432055158401,68.4148,9.95922457253419));
#82511=CARTESIAN_POINT('Ctrl Pts',(86.1884914560078,68.35625812488,9.92871412944681));
#82512=CARTESIAN_POINT('Ctrl Pts',(86.1313900471908,68.2948,9.89687241839012));
#82513=CARTESIAN_POINT('',(85.8418724183901,68.2948,10.1863900471908));
#82514=CARTESIAN_POINT('Origin',(88.011,68.2948,12.066));
#82515=CARTESIAN_POINT('',(85.9042245725342,68.4148,10.2982055158401));
#82516=CARTESIAN_POINT('Ctrl Pts',(85.8418724183901,68.2948,10.1863900471908));
#82517=CARTESIAN_POINT('Ctrl Pts',(85.8737141294469,68.3562581248803,10.2434914560081));
#82518=CARTESIAN_POINT('Ctrl Pts',(85.9042245725342,68.4148,10.2982055158401));
#82519=CARTESIAN_POINT('',(85.783280494161,68.2948,10.2562171833879));
#82520=CARTESIAN_POINT('Ctrl Pts',(85.9042245725342,68.4148,10.2982055158401));
#82521=CARTESIAN_POINT('Ctrl Pts',(85.8450436593716,68.3562581248809,10.2776595917227));
#82522=CARTESIAN_POINT('Ctrl Pts',(85.783280494161,68.2948,10.2562171833879));
#82523=CARTESIAN_POINT('',(85.548435497328,68.2948,10.5916105975083));
#82524=CARTESIAN_POINT('Origin',(88.011,68.2948,12.066));
#82525=CARTESIAN_POINT('',(85.629256934512,68.4148,10.6909));
#82526=CARTESIAN_POINT('Ctrl Pts',(85.548435497328,68.2948,10.5916105975083));
#82527=CARTESIAN_POINT('Ctrl Pts',(85.5897090168295,68.3562581248805,10.6423152525208));
#82528=CARTESIAN_POINT('Ctrl Pts',(85.629256934512,68.4148,10.6909));
#82529=CARTESIAN_POINT('',(85.5028590710356,68.2948,10.6705512834741));
#82530=CARTESIAN_POINT('Ctrl Pts',(85.629256934512,68.4148,10.6909));
#82531=CARTESIAN_POINT('Ctrl Pts',(85.5674073501174,68.3562581248806,10.6809428723598));
#82532=CARTESIAN_POINT('Ctrl Pts',(85.5028590710356,68.2948,10.6705512834741));
#82533=CARTESIAN_POINT('',(85.3298223525619,68.2948,11.0416297237433));
#82534=CARTESIAN_POINT('Origin',(88.011,68.2948,12.066));
#82535=CARTESIAN_POINT('',(85.4266573543146,68.4148,11.1253762018257));
#82536=CARTESIAN_POINT('Ctrl Pts',(85.3298223525618,68.2948,11.0416297237433));
#82537=CARTESIAN_POINT('Ctrl Pts',(85.3792736055027,68.35625812488,11.0843969896658));
#82538=CARTESIAN_POINT('Ctrl Pts',(85.4266573543146,68.4148,11.1253762018257));
#82539=CARTESIAN_POINT('',(85.2986462408563,68.2948,11.1272853866809));
#82540=CARTESIAN_POINT('Ctrl Pts',(85.4266573543146,68.4148,11.1253762018257));
#82541=CARTESIAN_POINT('Ctrl Pts',(85.3640183670115,68.3562581248796,11.1263104129475));
#82542=CARTESIAN_POINT('Ctrl Pts',(85.2986462408562,68.2948,11.1272853866809));
#82543=CARTESIAN_POINT('',(85.1926754338717,68.2948,11.5227738224661));
#82544=CARTESIAN_POINT('Origin',(88.011,68.2948,12.066));
#82545=CARTESIAN_POINT('',(85.3025817176658,68.4148,11.5884327817804));
#82546=CARTESIAN_POINT('Ctrl Pts',(85.1926754338717,68.2948,11.5227738224661));
#82547=CARTESIAN_POINT('Ctrl Pts',(85.2488018689556,68.3562581248803,11.5563042375653));
#82548=CARTESIAN_POINT('Ctrl Pts',(85.3025817176658,68.4148,11.5884327817804));
#82549=CARTESIAN_POINT('',(85.1768469071313,68.2948,11.6125418584009));
#82550=CARTESIAN_POINT('Ctrl Pts',(85.3025817176658,68.4148,11.5884327817804));
#82551=CARTESIAN_POINT('Ctrl Pts',(85.2410565813872,68.356258124879,11.6002299461323));
#82552=CARTESIAN_POINT('Ctrl Pts',(85.1768469071312,68.2948,11.6125418584009));
#82553=CARTESIAN_POINT('',(85.1411618809824,68.2948,12.0204235737076));
#82554=CARTESIAN_POINT('Origin',(88.011,68.2948,12.066));
#82555=CARTESIAN_POINT('Ctrl Pts',(85.1411618809824,68.2948,12.0204235737076));
#82556=CARTESIAN_POINT('Ctrl Pts',(85.2022581248785,68.3562581248785,12.0436983332871));
#82557=CARTESIAN_POINT('Ctrl Pts',(85.2608,68.4148,12.066));
#82558=CARTESIAN_POINT('',(85.4408,68.5948,12.066));
#82559=CARTESIAN_POINT('',(85.2908,68.4448,12.066));
#82560=CARTESIAN_POINT('Origin',(88.011,68.5948,12.066));
#82561=CARTESIAN_POINT('Origin',(91.0447367693476,68.5948,11.1320785609547));
#82562=CARTESIAN_POINT('',(90.7233537591437,65.6896,11.1272853866809));
#82563=CARTESIAN_POINT('',(90.7233537591437,65.0896,11.1272853866809));
#82564=CARTESIAN_POINT('',(90.5953426456854,65.6896,11.1253762018257));
#82565=CARTESIAN_POINT('',(91.0447367693476,65.6896,11.1320785609547));
#82566=CARTESIAN_POINT('',(90.5953426456854,68.5948,11.1253762018257));
#82567=CARTESIAN_POINT('Origin',(90.5953426456854,68.5948,11.1253762018257));
#82568=CARTESIAN_POINT('',(90.6921776474381,65.6896,11.0416297237434));
#82569=CARTESIAN_POINT('',(90.6921776474381,65.0896,11.0416297237434));
#82570=CARTESIAN_POINT('',(90.5953426456854,65.6896,11.1253762018257));
#82571=CARTESIAN_POINT('Origin',(90.7926780960505,65.6896,11.0535519717273));
#82572=CARTESIAN_POINT('Origin',(88.011,65.6896,12.066));
#82573=CARTESIAN_POINT('Origin',(90.8364737350774,68.5948,10.6194640646055));
#82574=CARTESIAN_POINT('',(90.5191409289644,65.6896,10.6705512834741));
#82575=CARTESIAN_POINT('',(90.5191409289644,65.0896,10.6705512834741));
#82576=CARTESIAN_POINT('',(90.392743065488,65.6896,10.6909));
#82577=CARTESIAN_POINT('',(90.8364737350774,65.6896,10.6194640646055));
#82578=CARTESIAN_POINT('',(90.392743065488,68.5948,10.6909));
#82579=CARTESIAN_POINT('Origin',(90.392743065488,68.5948,10.6909));
#82580=CARTESIAN_POINT('',(90.473564502672,65.6896,10.5916105975083));
#82581=CARTESIAN_POINT('',(90.473564502672,65.0896,10.5916105975083));
#82582=CARTESIAN_POINT('',(90.392743065488,65.6896,10.6909));
#82583=CARTESIAN_POINT('Origin',(90.5746084002827,65.6896,10.5859));
#82584=CARTESIAN_POINT('Origin',(88.011,65.6896,12.066));
#82585=CARTESIAN_POINT('Origin',(90.5423601111256,68.5948,10.1508018306708));
#82586=CARTESIAN_POINT('',(90.238719505839,65.6896,10.2562171833879));
#82587=CARTESIAN_POINT('',(90.238719505839,65.0896,10.2562171833879));
#82588=CARTESIAN_POINT('',(90.1177754274658,65.6896,10.2982055158401));
#82589=CARTESIAN_POINT('',(90.5423601111256,65.6896,10.1508018306708));
#82590=CARTESIAN_POINT('',(90.1177754274658,68.5948,10.2982055158401));
#82591=CARTESIAN_POINT('Origin',(90.1177754274658,68.5948,10.2982055158401));
#82592=CARTESIAN_POINT('',(90.1801275816099,65.6896,10.1863900471908));
#82593=CARTESIAN_POINT('',(90.1801275816099,65.0896,10.1863900471908));
#82594=CARTESIAN_POINT('',(90.1177754274658,65.6896,10.2982055158401));
#82595=CARTESIAN_POINT('Origin',(90.2786447605208,65.6896,10.1632201178059));
#82596=CARTESIAN_POINT('Origin',(88.011,65.6896,12.066));
#82597=CARTESIAN_POINT('Origin',(90.1713323911273,68.5948,9.74033192397407));
#82598=CARTESIAN_POINT('',(89.8906099528092,65.6896,9.89687241839011));
#82599=CARTESIAN_POINT('',(89.8906099528092,65.0896,9.89687241839011));
#82600=CARTESIAN_POINT('',(89.7787944841599,65.6896,9.95922457253418));
#82601=CARTESIAN_POINT('',(90.1713323911273,65.6896,9.74033192397407));
#82602=CARTESIAN_POINT('',(89.7787944841599,68.5948,9.95922457253418));
#82603=CARTESIAN_POINT('Origin',(89.7787944841599,68.5948,9.95922457253418));
#82604=CARTESIAN_POINT('',(89.8207828166121,65.6896,9.838280494161));
#82605=CARTESIAN_POINT('',(89.8207828166121,65.0896,9.838280494161));
#82606=CARTESIAN_POINT('',(89.7787944841599,65.6896,9.95922457253418));
#82607=CARTESIAN_POINT('Origin',(89.9137798821941,65.6896,9.79835523947919));
#82608=CARTESIAN_POINT('Origin',(88.011,65.6896,12.066));
#82609=CARTESIAN_POINT('Origin',(89.7346640646055,68.5948,9.40052626492258));
#82610=CARTESIAN_POINT('',(89.4853894024917,65.6896,9.60343549732802));
#82611=CARTESIAN_POINT('',(89.4853894024917,65.0896,9.60343549732802));
#82612=CARTESIAN_POINT('',(89.3861,65.6896,9.68425693451204));
#82613=CARTESIAN_POINT('',(89.7346640646055,65.6896,9.40052626492258));
#82614=CARTESIAN_POINT('',(89.3861,68.5948,9.68425693451204));
#82615=CARTESIAN_POINT('Origin',(89.3861,68.5948,9.68425693451204));
#82616=CARTESIAN_POINT('',(89.4064487165258,65.6896,9.55785907103561));
#82617=CARTESIAN_POINT('',(89.4064487165258,65.0896,9.55785907103561));
#82618=CARTESIAN_POINT('',(89.3861,65.6896,9.68425693451204));
#82619=CARTESIAN_POINT('Origin',(89.4911,65.6896,9.5023915997173));
#82620=CARTESIAN_POINT('Origin',(88.011,65.6896,12.066));
#82621=CARTESIAN_POINT('Origin',(89.2456230776968,68.5948,9.14170967651661));
#82622=CARTESIAN_POINT('',(89.0353702762566,65.6896,9.38482235256186));
#82623=CARTESIAN_POINT('',(89.0353702762566,65.0896,9.38482235256186));
#82624=CARTESIAN_POINT('',(88.9516237981742,65.6896,9.48165735431459));
#82625=CARTESIAN_POINT('',(89.2456230776968,65.6896,9.14170967651661));
#82626=CARTESIAN_POINT('',(88.9516237981742,68.5948,9.48165735431459));
#82627=CARTESIAN_POINT('Origin',(88.9516237981742,68.5948,9.48165735431459));
#82628=CARTESIAN_POINT('',(88.9497146133191,65.6896,9.35364624085626));
#82629=CARTESIAN_POINT('',(88.9497146133191,65.0896,9.35364624085626));
#82630=CARTESIAN_POINT('',(88.9516237981742,65.6896,9.48165735431459));
#82631=CARTESIAN_POINT('Origin',(89.0234480282727,65.6896,9.28432190394954));
#82632=CARTESIAN_POINT('Origin',(88.011,65.6896,12.066));
#82633=CARTESIAN_POINT('Origin',(88.7190686933216,68.5948,8.9717461698274));
#82634=CARTESIAN_POINT('',(88.5542261775338,65.6896,9.24767543387175));
#82635=CARTESIAN_POINT('',(88.5542261775338,65.0896,9.24767543387175));
#82636=CARTESIAN_POINT('',(88.4885672182196,65.6896,9.35758171766581));
#82637=CARTESIAN_POINT('',(88.7190686933216,65.6896,8.9717461698274));
#82638=CARTESIAN_POINT('',(88.4885672182196,68.5948,9.35758171766581));
#82639=CARTESIAN_POINT('Origin',(88.4885672182196,68.5948,9.35758171766581));
#82640=CARTESIAN_POINT('',(88.4644581415991,65.6896,9.23184690713126));
#82641=CARTESIAN_POINT('',(88.4644581415991,65.0896,9.23184690713126));
#82642=CARTESIAN_POINT('',(88.4885672182196,65.6896,9.35758171766581));
#82643=CARTESIAN_POINT('Origin',(88.5250333355296,65.6896,9.15077208953324));
#82644=CARTESIAN_POINT('Origin',(88.011,65.6896,12.066));
#82645=CARTESIAN_POINT('Origin',(88.171,68.5948,8.8958));
#82646=CARTESIAN_POINT('',(88.0565764262924,65.6896,9.19616188098241));
#82647=CARTESIAN_POINT('',(88.0565764262924,65.0896,9.19616188098241));
#82648=CARTESIAN_POINT('',(88.011,65.6896,9.3158));
#82649=CARTESIAN_POINT('',(88.171,65.6896,8.8958));
#82650=CARTESIAN_POINT('',(88.011,68.5948,9.3158));
#82651=CARTESIAN_POINT('Origin',(88.011,68.5948,9.3158));
#82652=CARTESIAN_POINT('',(87.9654235737076,65.6896,9.19616188098241));
#82653=CARTESIAN_POINT('',(87.9654235737076,65.0896,9.19616188098241));
#82654=CARTESIAN_POINT('',(88.011,65.6896,9.3158));
#82655=CARTESIAN_POINT('Origin',(88.011,65.6896,9.1058));
#82656=CARTESIAN_POINT('Origin',(88.011,65.6896,12.066));
#82657=CARTESIAN_POINT('Origin',(87.6180697876423,68.5948,8.91617875297397));
#82658=CARTESIAN_POINT('',(87.5575418584008,65.6896,9.23184690713126));
#82659=CARTESIAN_POINT('',(87.5575418584008,65.0896,9.23184690713126));
#82660=CARTESIAN_POINT('',(87.5334327817804,65.6896,9.35758171766581));
#82661=CARTESIAN_POINT('',(87.6180697876423,65.6896,8.91617875297397));
#82662=CARTESIAN_POINT('',(87.5334327817804,68.5948,9.35758171766581));
#82663=CARTESIAN_POINT('Origin',(87.5334327817804,68.5948,9.35758171766581));
#82664=CARTESIAN_POINT('',(87.4677738224661,65.6896,9.24767543387176));
#82665=CARTESIAN_POINT('',(87.4677738224661,65.0896,9.24767543387176));
#82666=CARTESIAN_POINT('',(87.5334327817804,65.6896,9.35758171766581));
#82667=CARTESIAN_POINT('Origin',(87.4969666644703,65.6896,9.15077208953324));
#82668=CARTESIAN_POINT('Origin',(88.011,65.6896,12.066));
#82669=CARTESIAN_POINT('Origin',(87.0770785609547,68.5948,9.03226323065242));
#82670=CARTESIAN_POINT('',(87.0722853866809,65.6896,9.35364624085626));
#82671=CARTESIAN_POINT('',(87.0722853866809,65.0896,9.35364624085626));
#82672=CARTESIAN_POINT('',(87.0703762018258,65.6896,9.48165735431459));
#82673=CARTESIAN_POINT('',(87.0770785609547,65.6896,9.03226323065242));
#82674=CARTESIAN_POINT('',(87.0703762018258,68.5948,9.48165735431459));
#82675=CARTESIAN_POINT('Origin',(87.0703762018258,68.5948,9.48165735431459));
#82676=CARTESIAN_POINT('',(86.9866297237434,65.6896,9.38482235256186));
#82677=CARTESIAN_POINT('',(86.9866297237434,65.0896,9.38482235256186));
#82678=CARTESIAN_POINT('',(87.0703762018258,65.6896,9.48165735431459));
#82679=CARTESIAN_POINT('Origin',(86.9985519717274,65.6896,9.28432190394956));
#82680=CARTESIAN_POINT('Origin',(88.011,65.6896,12.066));
#82681=CARTESIAN_POINT('Origin',(86.5644640646055,68.5948,9.24052626492257));
#82682=CARTESIAN_POINT('',(86.6155512834741,65.6896,9.55785907103562));
#82683=CARTESIAN_POINT('',(86.6155512834741,65.0896,9.55785907103562));
#82684=CARTESIAN_POINT('',(86.6359,65.6896,9.68425693451204));
#82685=CARTESIAN_POINT('',(86.5644640646055,65.6896,9.24052626492257));
#82686=CARTESIAN_POINT('',(86.6359,68.5948,9.68425693451204));
#82687=CARTESIAN_POINT('Origin',(86.6359,68.5948,9.68425693451204));
#82688=CARTESIAN_POINT('',(86.5366105975083,65.6896,9.60343549732803));
#82689=CARTESIAN_POINT('',(86.5366105975083,65.0896,9.60343549732803));
#82690=CARTESIAN_POINT('',(86.6359,65.6896,9.68425693451204));
#82691=CARTESIAN_POINT('Origin',(86.5309,65.6896,9.5023915997173));
#82692=CARTESIAN_POINT('Origin',(88.011,65.6896,12.066));
#82693=CARTESIAN_POINT('Origin',(86.0958018306708,68.5948,9.53463988887438));
#82694=CARTESIAN_POINT('',(86.2012171833879,65.6896,9.838280494161));
#82695=CARTESIAN_POINT('',(86.2012171833879,65.0896,9.838280494161));
#82696=CARTESIAN_POINT('',(86.2432055158401,65.6896,9.95922457253419));
#82697=CARTESIAN_POINT('',(86.0958018306708,65.6896,9.53463988887438));
#82698=CARTESIAN_POINT('',(86.2432055158401,68.5948,9.95922457253419));
#82699=CARTESIAN_POINT('Origin',(86.2432055158401,68.5948,9.95922457253419));
#82700=CARTESIAN_POINT('',(86.1313900471908,65.6896,9.89687241839012));
#82701=CARTESIAN_POINT('',(86.1313900471908,65.0896,9.89687241839012));
#82702=CARTESIAN_POINT('',(86.2432055158401,65.6896,9.95922457253419));
#82703=CARTESIAN_POINT('Origin',(86.1082201178059,65.6896,9.7983552394792));
#82704=CARTESIAN_POINT('Origin',(88.011,65.6896,12.066));
#82705=CARTESIAN_POINT('Origin',(85.6853319239741,68.5948,9.90566760887269));
#82706=CARTESIAN_POINT('',(85.8418724183901,65.6896,10.1863900471908));
#82707=CARTESIAN_POINT('',(85.8418724183901,65.0896,10.1863900471908));
#82708=CARTESIAN_POINT('',(85.9042245725342,65.6896,10.2982055158401));
#82709=CARTESIAN_POINT('',(85.6853319239741,65.6896,9.90566760887269));
#82710=CARTESIAN_POINT('',(85.9042245725342,68.5948,10.2982055158401));
#82711=CARTESIAN_POINT('Origin',(85.9042245725342,68.5948,10.2982055158401));
#82712=CARTESIAN_POINT('',(85.783280494161,65.6896,10.2562171833879));
#82713=CARTESIAN_POINT('',(85.783280494161,65.0896,10.2562171833879));
#82714=CARTESIAN_POINT('',(85.9042245725342,65.6896,10.2982055158401));
#82715=CARTESIAN_POINT('Origin',(85.7433552394792,65.6896,10.1632201178059));
#82716=CARTESIAN_POINT('Origin',(88.011,65.6896,12.066));
#82717=CARTESIAN_POINT('Origin',(85.3455262649226,68.5948,10.3423359353945));
#82718=CARTESIAN_POINT('',(85.548435497328,65.6896,10.5916105975083));
#82719=CARTESIAN_POINT('',(85.548435497328,65.0896,10.5916105975083));
#82720=CARTESIAN_POINT('',(85.629256934512,65.6896,10.6909));
#82721=CARTESIAN_POINT('',(85.3455262649226,65.6896,10.3423359353945));
#82722=CARTESIAN_POINT('',(85.629256934512,68.5948,10.6909));
#82723=CARTESIAN_POINT('Origin',(85.629256934512,68.5948,10.6909));
#82724=CARTESIAN_POINT('',(85.5028590710356,65.6896,10.6705512834741));
#82725=CARTESIAN_POINT('',(85.5028590710356,65.0896,10.6705512834741));
#82726=CARTESIAN_POINT('',(85.629256934512,65.6896,10.6909));
#82727=CARTESIAN_POINT('Origin',(85.4473915997173,65.6896,10.5859));
#82728=CARTESIAN_POINT('Origin',(88.011,65.6896,12.066));
#82729=CARTESIAN_POINT('Origin',(85.0867096765166,68.5948,10.8313769223032));
#82730=CARTESIAN_POINT('',(85.3298223525619,65.6896,11.0416297237433));
#82731=CARTESIAN_POINT('',(85.3298223525619,65.0896,11.0416297237433));
#82732=CARTESIAN_POINT('',(85.4266573543146,65.6896,11.1253762018257));
#82733=CARTESIAN_POINT('',(85.0867096765166,65.6896,10.8313769223032));
#82734=CARTESIAN_POINT('',(85.4266573543146,68.5948,11.1253762018257));
#82735=CARTESIAN_POINT('Origin',(85.4266573543146,68.5948,11.1253762018257));
#82736=CARTESIAN_POINT('',(85.2986462408563,65.6896,11.1272853866809));
#82737=CARTESIAN_POINT('',(85.2986462408563,65.0896,11.1272853866809));
#82738=CARTESIAN_POINT('',(85.4266573543146,65.6896,11.1253762018257));
#82739=CARTESIAN_POINT('Origin',(85.2293219039495,65.6896,11.0535519717273));
#82740=CARTESIAN_POINT('Origin',(88.011,65.6896,12.066));
#82741=CARTESIAN_POINT('Origin',(84.9167461698274,68.5948,11.3579313066783));
#82742=CARTESIAN_POINT('',(85.1926754338717,65.6896,11.5227738224661));
#82743=CARTESIAN_POINT('',(85.1926754338717,65.0896,11.5227738224661));
#82744=CARTESIAN_POINT('',(85.3025817176658,65.6896,11.5884327817804));
#82745=CARTESIAN_POINT('',(84.9167461698274,65.6896,11.3579313066783));
#82746=CARTESIAN_POINT('',(85.3025817176658,68.5948,11.5884327817804));
#82747=CARTESIAN_POINT('Origin',(85.3025817176658,68.5948,11.5884327817804));
#82748=CARTESIAN_POINT('',(85.1768469071313,65.6896,11.6125418584009));
#82749=CARTESIAN_POINT('',(85.1768469071313,65.0896,11.6125418584009));
#82750=CARTESIAN_POINT('',(85.3025817176658,65.6896,11.5884327817804));
#82751=CARTESIAN_POINT('Origin',(85.0957720895332,65.6896,11.5519666644703));
#82752=CARTESIAN_POINT('Origin',(88.011,65.6896,12.066));
#82753=CARTESIAN_POINT('Origin',(84.8408,68.5948,11.906));
#82754=CARTESIAN_POINT('',(85.1411618809824,65.6896,12.0204235737076));
#82755=CARTESIAN_POINT('',(85.1411618809824,65.0896,12.0204235737076));
#82756=CARTESIAN_POINT('',(85.2608,65.6896,12.066));
#82757=CARTESIAN_POINT('',(84.8408,65.6896,11.906));
#82758=CARTESIAN_POINT('',(85.2608,68.5948,12.066));
#82759=CARTESIAN_POINT('Origin',(85.2608,68.5948,12.066));
#82760=CARTESIAN_POINT('',(85.1411618809824,65.6896,12.1115764262924));
#82761=CARTESIAN_POINT('',(85.1411618809824,65.0896,12.1115764262924));
#82762=CARTESIAN_POINT('',(85.2608,65.6896,12.066));
#82763=CARTESIAN_POINT('Origin',(85.0508,65.6896,12.066));
#82764=CARTESIAN_POINT('',(85.1408,65.6896,12.066));
#82765=CARTESIAN_POINT('Origin',(88.011,65.6896,12.066));
#82766=CARTESIAN_POINT('Origin',(88.011,65.6896,12.066));
#82767=CARTESIAN_POINT('Origin',(84.861178752974,68.5948,12.4589302123577));
#82768=CARTESIAN_POINT('',(85.1768469071313,65.6896,12.5194581415991));
#82769=CARTESIAN_POINT('',(85.1768469071313,65.0896,12.5194581415991));
#82770=CARTESIAN_POINT('',(85.3025817176658,65.6896,12.5435672182196));
#82771=CARTESIAN_POINT('',(84.861178752974,65.6896,12.4589302123577));
#82772=CARTESIAN_POINT('',(85.3025817176658,68.5948,12.5435672182196));
#82773=CARTESIAN_POINT('Origin',(85.3025817176658,68.5948,12.5435672182196));
#82774=CARTESIAN_POINT('',(85.1926754338717,65.6896,12.6092261775339));
#82775=CARTESIAN_POINT('',(85.1926754338717,65.0896,12.6092261775339));
#82776=CARTESIAN_POINT('',(85.3025817176658,65.6896,12.5435672182196));
#82777=CARTESIAN_POINT('Origin',(85.0957720895333,65.6896,12.5800333355296));
#82778=CARTESIAN_POINT('Origin',(88.011,65.6896,12.066));
#82779=CARTESIAN_POINT('Origin',(84.9772632306524,68.5948,12.9999214390453));
#82780=CARTESIAN_POINT('',(85.2986462408562,65.6896,13.0047146133191));
#82781=CARTESIAN_POINT('',(85.2986462408562,65.0896,13.0047146133191));
#82782=CARTESIAN_POINT('',(85.4266573543146,65.6896,13.0066237981742));
#82783=CARTESIAN_POINT('',(84.9772632306524,65.6896,12.9999214390453));
#82784=CARTESIAN_POINT('',(85.4266573543146,68.5948,13.0066237981742));
#82785=CARTESIAN_POINT('Origin',(85.4266573543146,68.5948,13.0066237981742));
#82786=CARTESIAN_POINT('',(85.3298223525619,65.6896,13.0903702762566));
#82787=CARTESIAN_POINT('',(85.3298223525619,65.0896,13.0903702762566));
#82788=CARTESIAN_POINT('',(85.4266573543146,65.6896,13.0066237981742));
#82789=CARTESIAN_POINT('Origin',(85.2293219039496,65.6896,13.0784480282726));
#82790=CARTESIAN_POINT('Origin',(88.011,65.6896,12.066));
#82791=CARTESIAN_POINT('Origin',(85.1855262649226,68.5948,13.5125359353945));
#82792=CARTESIAN_POINT('',(85.5028590710356,65.6896,13.4614487165259));
#82793=CARTESIAN_POINT('',(85.5028590710356,65.0896,13.4614487165259));
#82794=CARTESIAN_POINT('',(85.629256934512,65.6896,13.4411));
#82795=CARTESIAN_POINT('',(85.1855262649226,65.6896,13.5125359353945));
#82796=CARTESIAN_POINT('',(85.629256934512,68.5948,13.4411));
#82797=CARTESIAN_POINT('Origin',(85.629256934512,68.5948,13.4411));
#82798=CARTESIAN_POINT('',(85.548435497328,65.6896,13.5403894024917));
#82799=CARTESIAN_POINT('',(85.548435497328,65.0896,13.5403894024917));
#82800=CARTESIAN_POINT('',(85.629256934512,65.6896,13.4411));
#82801=CARTESIAN_POINT('Origin',(85.4473915997173,65.6896,13.5461));
#82802=CARTESIAN_POINT('Origin',(88.011,65.6896,12.066));
#82803=CARTESIAN_POINT('Origin',(85.4796398888744,68.5948,13.9811981693292));
#82804=CARTESIAN_POINT('',(85.783280494161,65.6896,13.8757828166121));
#82805=CARTESIAN_POINT('',(85.783280494161,65.0896,13.8757828166121));
#82806=CARTESIAN_POINT('',(85.9042245725342,65.6896,13.8337944841599));
#82807=CARTESIAN_POINT('',(85.4796398888744,65.6896,13.9811981693292));
#82808=CARTESIAN_POINT('',(85.9042245725342,68.5948,13.8337944841599));
#82809=CARTESIAN_POINT('Origin',(85.9042245725342,68.5948,13.8337944841599));
#82810=CARTESIAN_POINT('',(85.8418724183901,65.6896,13.9456099528092));
#82811=CARTESIAN_POINT('',(85.8418724183901,65.0896,13.9456099528092));
#82812=CARTESIAN_POINT('',(85.9042245725342,65.6896,13.8337944841599));
#82813=CARTESIAN_POINT('Origin',(85.7433552394792,65.6896,13.9687798821941));
#82814=CARTESIAN_POINT('Origin',(88.011,65.6896,12.066));
#82815=CARTESIAN_POINT('Origin',(85.8506676088727,68.5948,14.3916680760259));
#82816=CARTESIAN_POINT('',(86.1313900471908,65.6896,14.2351275816099));
#82817=CARTESIAN_POINT('',(86.1313900471908,65.0896,14.2351275816099));
#82818=CARTESIAN_POINT('',(86.2432055158401,65.6896,14.1727754274658));
#82819=CARTESIAN_POINT('',(85.8506676088727,65.6896,14.3916680760259));
#82820=CARTESIAN_POINT('',(86.2432055158401,68.5948,14.1727754274658));
#82821=CARTESIAN_POINT('Origin',(86.2432055158401,68.5948,14.1727754274658));
#82822=CARTESIAN_POINT('',(86.2012171833879,65.6896,14.293719505839));
#82823=CARTESIAN_POINT('',(86.2012171833879,65.0896,14.293719505839));
#82824=CARTESIAN_POINT('',(86.2432055158401,65.6896,14.1727754274658));
#82825=CARTESIAN_POINT('Origin',(86.1082201178059,65.6896,14.3336447605208));
#82826=CARTESIAN_POINT('Origin',(88.011,65.6896,12.066));
#82827=CARTESIAN_POINT('Origin',(86.2873359353945,68.5948,14.7314737350774));
#82828=CARTESIAN_POINT('',(86.5366105975083,65.6896,14.528564502672));
#82829=CARTESIAN_POINT('',(86.5366105975083,65.0896,14.528564502672));
#82830=CARTESIAN_POINT('',(86.6359,65.6896,14.447743065488));
#82831=CARTESIAN_POINT('',(86.2873359353945,65.6896,14.7314737350774));
#82832=CARTESIAN_POINT('',(86.6359,68.5948,14.447743065488));
#82833=CARTESIAN_POINT('Origin',(86.6359,68.5948,14.447743065488));
#82834=CARTESIAN_POINT('',(86.6155512834742,65.6896,14.5741409289644));
#82835=CARTESIAN_POINT('',(86.6155512834742,65.0896,14.5741409289644));
#82836=CARTESIAN_POINT('',(86.6359,65.6896,14.447743065488));
#82837=CARTESIAN_POINT('Origin',(86.5309,65.6896,14.6296084002827));
#82838=CARTESIAN_POINT('Origin',(88.011,65.6896,12.066));
#82839=CARTESIAN_POINT('Origin',(86.7763769223032,68.5948,14.9902903234834));
#82840=CARTESIAN_POINT('',(86.9866297237434,65.6896,14.7471776474381));
#82841=CARTESIAN_POINT('',(86.9866297237434,65.0896,14.7471776474381));
#82842=CARTESIAN_POINT('',(87.0703762018258,65.6896,14.6503426456854));
#82843=CARTESIAN_POINT('',(86.7763769223032,65.6896,14.9902903234834));
#82844=CARTESIAN_POINT('',(87.0703762018258,68.5948,14.6503426456854));
#82845=CARTESIAN_POINT('Origin',(87.0703762018258,68.5948,14.6503426456854));
#82846=CARTESIAN_POINT('',(87.0722853866809,65.6896,14.7783537591437));
#82847=CARTESIAN_POINT('',(87.0722853866809,65.0896,14.7783537591437));
#82848=CARTESIAN_POINT('',(87.0703762018258,65.6896,14.6503426456854));
#82849=CARTESIAN_POINT('Origin',(86.9985519717274,65.6896,14.8476780960505));
#82850=CARTESIAN_POINT('Origin',(88.011,65.6896,12.066));
#82851=CARTESIAN_POINT('Origin',(87.3029313066783,68.5948,15.1602538301726));
#82852=CARTESIAN_POINT('',(87.4677738224661,65.6896,14.8843245661282));
#82853=CARTESIAN_POINT('',(87.4677738224661,65.0896,14.8843245661282));
#82854=CARTESIAN_POINT('',(87.5334327817804,65.6896,14.7744182823342));
#82855=CARTESIAN_POINT('',(87.3029313066783,65.6896,15.1602538301726));
#82856=CARTESIAN_POINT('',(87.5334327817804,68.5948,14.7744182823342));
#82857=CARTESIAN_POINT('Origin',(87.5334327817804,68.5948,14.7744182823342));
#82858=CARTESIAN_POINT('',(87.5575418584009,65.6896,14.9001530928687));
#82859=CARTESIAN_POINT('',(87.5575418584009,65.0896,14.9001530928687));
#82860=CARTESIAN_POINT('',(87.5334327817804,65.6896,14.7744182823342));
#82861=CARTESIAN_POINT('Origin',(87.4969666644703,65.6896,14.9812279104668));
#82862=CARTESIAN_POINT('Origin',(88.011,65.6896,12.066));
#82863=CARTESIAN_POINT('Origin',(87.851,68.5948,15.2362));
#82864=CARTESIAN_POINT('',(87.9654235737076,65.6896,14.9358381190176));
#82865=CARTESIAN_POINT('',(87.9654235737076,65.0896,14.9358381190176));
#82866=CARTESIAN_POINT('',(88.011,65.6896,14.8162));
#82867=CARTESIAN_POINT('',(87.851,65.6896,15.2362));
#82868=CARTESIAN_POINT('',(88.011,68.5948,14.8162));
#82869=CARTESIAN_POINT('Origin',(88.011,68.5948,14.8162));
#82870=CARTESIAN_POINT('',(88.0565764262924,65.6896,14.9358381190176));
#82871=CARTESIAN_POINT('',(88.0565764262924,65.0896,14.9358381190176));
#82872=CARTESIAN_POINT('',(88.011,65.6896,14.8162));
#82873=CARTESIAN_POINT('Origin',(88.011,65.6896,15.0262));
#82874=CARTESIAN_POINT('Origin',(88.011,65.6896,12.066));
#82875=CARTESIAN_POINT('Origin',(88.4039302123577,68.5948,15.215821247026));
#82876=CARTESIAN_POINT('',(88.4644581415992,65.6896,14.9001530928687));
#82877=CARTESIAN_POINT('',(88.4644581415992,65.0896,14.9001530928687));
#82878=CARTESIAN_POINT('',(88.4885672182196,65.6896,14.7744182823342));
#82879=CARTESIAN_POINT('',(88.4039302123577,65.6896,15.215821247026));
#82880=CARTESIAN_POINT('',(88.4885672182196,68.5948,14.7744182823342));
#82881=CARTESIAN_POINT('Origin',(88.4885672182196,68.5948,14.7744182823342));
#82882=CARTESIAN_POINT('',(88.5542261775338,65.6896,14.8843245661282));
#82883=CARTESIAN_POINT('',(88.5542261775338,65.0896,14.8843245661282));
#82884=CARTESIAN_POINT('',(88.4885672182196,65.6896,14.7744182823342));
#82885=CARTESIAN_POINT('Origin',(88.5250333355296,65.6896,14.9812279104668));
#82886=CARTESIAN_POINT('Origin',(88.011,65.6896,12.066));
#82887=CARTESIAN_POINT('Origin',(88.9449214390453,68.5948,15.0997367693476));
#82888=CARTESIAN_POINT('',(88.9497146133191,65.6896,14.7783537591437));
#82889=CARTESIAN_POINT('',(88.9497146133191,65.0896,14.7783537591437));
#82890=CARTESIAN_POINT('',(88.9516237981743,65.6896,14.6503426456854));
#82891=CARTESIAN_POINT('',(88.9449214390453,65.6896,15.0997367693476));
#82892=CARTESIAN_POINT('',(88.9516237981743,68.5948,14.6503426456854));
#82893=CARTESIAN_POINT('Origin',(88.9516237981743,68.5948,14.6503426456854));
#82894=CARTESIAN_POINT('',(89.0353702762567,65.6896,14.7471776474381));
#82895=CARTESIAN_POINT('',(89.0353702762567,65.0896,14.7471776474381));
#82896=CARTESIAN_POINT('',(88.9516237981743,65.6896,14.6503426456854));
#82897=CARTESIAN_POINT('Origin',(89.0234480282727,65.6896,14.8476780960504));
#82898=CARTESIAN_POINT('Origin',(88.011,65.6896,12.066));
#82899=CARTESIAN_POINT('Origin',(89.4575359353945,68.5948,14.8914737350774));
#82900=CARTESIAN_POINT('',(89.4064487165259,65.6896,14.5741409289644));
#82901=CARTESIAN_POINT('',(89.4064487165259,65.0896,14.5741409289644));
#82902=CARTESIAN_POINT('',(89.3861,65.6896,14.447743065488));
#82903=CARTESIAN_POINT('',(89.4575359353945,65.6896,14.8914737350774));
#82904=CARTESIAN_POINT('',(89.3861,68.5948,14.447743065488));
#82905=CARTESIAN_POINT('Origin',(89.3861,68.5948,14.447743065488));
#82906=CARTESIAN_POINT('',(89.4853894024917,65.6896,14.528564502672));
#82907=CARTESIAN_POINT('',(89.4853894024917,65.0896,14.528564502672));
#82908=CARTESIAN_POINT('',(89.3861,65.6896,14.447743065488));
#82909=CARTESIAN_POINT('Origin',(89.4911,65.6896,14.6296084002827));
#82910=CARTESIAN_POINT('Origin',(88.011,65.6896,12.066));
#82911=CARTESIAN_POINT('Origin',(89.9261981693292,68.5948,14.5973601111256));
#82912=CARTESIAN_POINT('',(89.8207828166121,65.6896,14.293719505839));
#82913=CARTESIAN_POINT('',(89.8207828166121,65.0896,14.293719505839));
#82914=CARTESIAN_POINT('',(89.7787944841599,65.6896,14.1727754274658));
#82915=CARTESIAN_POINT('',(89.9261981693292,65.6896,14.5973601111256));
#82916=CARTESIAN_POINT('',(89.7787944841599,68.5948,14.1727754274658));
#82917=CARTESIAN_POINT('Origin',(89.7787944841599,68.5948,14.1727754274658));
#82918=CARTESIAN_POINT('',(89.8906099528091,65.6896,14.2351275816099));
#82919=CARTESIAN_POINT('',(89.8906099528091,65.0896,14.2351275816099));
#82920=CARTESIAN_POINT('',(89.7787944841599,65.6896,14.1727754274658));
#82921=CARTESIAN_POINT('Origin',(89.9137798821941,65.6896,14.3336447605208));
#82922=CARTESIAN_POINT('Origin',(88.011,65.6896,12.066));
#82923=CARTESIAN_POINT('Origin',(90.3366680760259,68.5948,14.2263323911273));
#82924=CARTESIAN_POINT('',(90.1801275816099,65.6896,13.9456099528092));
#82925=CARTESIAN_POINT('',(90.1801275816099,65.0896,13.9456099528092));
#82926=CARTESIAN_POINT('',(90.1177754274658,65.6896,13.8337944841599));
#82927=CARTESIAN_POINT('',(90.3366680760259,65.6896,14.2263323911273));
#82928=CARTESIAN_POINT('',(90.1177754274658,68.5948,13.8337944841599));
#82929=CARTESIAN_POINT('Origin',(90.1177754274658,68.5948,13.8337944841599));
#82930=CARTESIAN_POINT('',(90.238719505839,65.6896,13.8757828166121));
#82931=CARTESIAN_POINT('',(90.238719505839,65.0896,13.8757828166121));
#82932=CARTESIAN_POINT('',(90.1177754274658,65.6896,13.8337944841599));
#82933=CARTESIAN_POINT('Origin',(90.2786447605208,65.6896,13.9687798821941));
#82934=CARTESIAN_POINT('Origin',(88.011,65.6896,12.066));
#82935=CARTESIAN_POINT('Origin',(90.6764737350774,68.5948,13.7896640646055));
#82936=CARTESIAN_POINT('',(90.473564502672,65.6896,13.5403894024917));
#82937=CARTESIAN_POINT('',(90.473564502672,65.0896,13.5403894024917));
#82938=CARTESIAN_POINT('',(90.392743065488,65.6896,13.4411));
#82939=CARTESIAN_POINT('',(90.6764737350774,65.6896,13.7896640646055));
#82940=CARTESIAN_POINT('',(90.392743065488,68.5948,13.4411));
#82941=CARTESIAN_POINT('Origin',(90.392743065488,68.5948,13.4411));
#82942=CARTESIAN_POINT('',(90.5191409289644,65.6896,13.4614487165259));
#82943=CARTESIAN_POINT('',(90.5191409289644,65.0896,13.4614487165259));
#82944=CARTESIAN_POINT('',(90.392743065488,65.6896,13.4411));
#82945=CARTESIAN_POINT('Origin',(90.5746084002827,65.6896,13.5461));
#82946=CARTESIAN_POINT('Origin',(88.011,65.6896,12.066));
#82947=CARTESIAN_POINT('Origin',(90.9352903234834,68.5948,13.3006230776968));
#82948=CARTESIAN_POINT('',(90.6921776474381,65.6896,13.0903702762567));
#82949=CARTESIAN_POINT('',(90.6921776474381,65.0896,13.0903702762567));
#82950=CARTESIAN_POINT('',(90.5953426456854,65.6896,13.0066237981743));
#82951=CARTESIAN_POINT('',(90.9352903234834,65.6896,13.3006230776968));
#82952=CARTESIAN_POINT('',(90.5953426456854,68.5948,13.0066237981743));
#82953=CARTESIAN_POINT('Origin',(90.5953426456854,68.5948,13.0066237981743));
#82954=CARTESIAN_POINT('',(90.7233537591437,65.6896,13.0047146133191));
#82955=CARTESIAN_POINT('',(90.7233537591437,65.0896,13.0047146133191));
#82956=CARTESIAN_POINT('',(90.5953426456854,65.6896,13.0066237981743));
#82957=CARTESIAN_POINT('Origin',(90.7926780960505,65.6896,13.0784480282726));
#82958=CARTESIAN_POINT('Origin',(88.011,65.6896,12.066));
#82959=CARTESIAN_POINT('Origin',(91.1052538301726,68.5948,12.7740686933217));
#82960=CARTESIAN_POINT('',(90.8293245661282,65.6896,12.6092261775338));
#82961=CARTESIAN_POINT('',(90.8293245661282,65.0896,12.6092261775338));
#82962=CARTESIAN_POINT('',(90.7194182823342,65.6896,12.5435672182196));
#82963=CARTESIAN_POINT('',(91.1052538301726,65.6896,12.7740686933217));
#82964=CARTESIAN_POINT('',(90.7194182823342,68.5948,12.5435672182196));
#82965=CARTESIAN_POINT('Origin',(90.7194182823342,68.5948,12.5435672182196));
#82966=CARTESIAN_POINT('',(90.8451530928687,65.6896,12.5194581415991));
#82967=CARTESIAN_POINT('',(90.8451530928687,65.0896,12.5194581415991));
#82968=CARTESIAN_POINT('',(90.7194182823342,65.6896,12.5435672182196));
#82969=CARTESIAN_POINT('Origin',(90.9262279104668,65.6896,12.5800333355296));
#82970=CARTESIAN_POINT('Origin',(88.011,65.6896,12.066));
#82971=CARTESIAN_POINT('Origin',(91.1812,68.5948,12.226));
#82972=CARTESIAN_POINT('',(90.8808381190176,65.6896,12.1115764262924));
#82973=CARTESIAN_POINT('',(90.8808381190176,65.0896,12.1115764262924));
#82974=CARTESIAN_POINT('',(90.7612,65.6896,12.066));
#82975=CARTESIAN_POINT('',(91.1812,65.6896,12.226));
#82976=CARTESIAN_POINT('',(90.7612,68.5948,12.066));
#82977=CARTESIAN_POINT('Origin',(90.7612,68.5948,12.066));
#82978=CARTESIAN_POINT('',(90.8808381190176,65.6896,12.0204235737076));
#82979=CARTESIAN_POINT('',(90.8808381190176,65.0896,12.0204235737076));
#82980=CARTESIAN_POINT('',(90.7612,65.6896,12.066));
#82981=CARTESIAN_POINT('Origin',(90.9712,65.6896,12.066));
#82982=CARTESIAN_POINT('Origin',(88.011,65.6896,12.066));
#82983=CARTESIAN_POINT('Origin',(88.011,65.0896,12.066));
#82984=CARTESIAN_POINT('',(85.1408,65.0896,12.066));
#82985=CARTESIAN_POINT('Origin',(88.011,68.5948,12.066));
#82986=CARTESIAN_POINT('',(86.4070487834076,68.5948,12.066));
#82987=CARTESIAN_POINT('',(87.2090243917038,68.5948,10.6769375));
#82988=CARTESIAN_POINT('',(86.6075426854816,68.5948,11.718734375));
#82989=CARTESIAN_POINT('',(88.8129756082962,68.5948,10.6769375));
#82990=CARTESIAN_POINT('',(87.6100121958519,68.5948,10.6769375));
#82991=CARTESIAN_POINT('',(89.6149512165924,68.5948,12.066));
#82992=CARTESIAN_POINT('',(89.0134695103703,68.5948,11.024203125));
#82993=CARTESIAN_POINT('',(88.8129756082962,68.5948,13.4550625));
#82994=CARTESIAN_POINT('',(89.4144573145184,68.5948,12.413265625));
#82995=CARTESIAN_POINT('',(87.2090243917038,68.5948,13.4550625));
#82996=CARTESIAN_POINT('',(88.4119878041481,68.5948,13.4550625));
#82997=CARTESIAN_POINT('',(87.0085304896297,68.5948,13.107796875));
#82998=CARTESIAN_POINT('Origin',(89.6149512165924,66.7948,12.066));
#82999=CARTESIAN_POINT('',(86.4070487834076,66.7948,12.066));
#83000=CARTESIAN_POINT('',(87.2090243917038,66.7948,10.6769375));
#83001=CARTESIAN_POINT('',(86.4070487834076,66.7948,12.066));
#83002=CARTESIAN_POINT('Origin',(88.011,66.7948,12.066));
#83003=CARTESIAN_POINT('Origin',(89.6149512165924,66.7948,12.066));
#83004=CARTESIAN_POINT('',(88.8129756082962,66.7948,10.6769375));
#83005=CARTESIAN_POINT('',(87.2090243917038,66.7948,10.6769375));
#83006=CARTESIAN_POINT('Origin',(88.011,66.7948,12.066));
#83007=CARTESIAN_POINT('Origin',(89.6149512165924,66.7948,12.066));
#83008=CARTESIAN_POINT('',(89.6149512165924,66.7948,12.066));
#83009=CARTESIAN_POINT('',(88.8129756082962,66.7948,10.6769375));
#83010=CARTESIAN_POINT('Origin',(88.011,66.7948,12.066));
#83011=CARTESIAN_POINT('Origin',(89.6149512165924,66.7948,12.066));
#83012=CARTESIAN_POINT('',(88.8129756082962,66.7948,13.4550625));
#83013=CARTESIAN_POINT('',(89.6149512165924,66.7948,12.066));
#83014=CARTESIAN_POINT('Origin',(88.011,66.7948,12.066));
#83015=CARTESIAN_POINT('Origin',(89.6149512165924,66.7948,12.066));
#83016=CARTESIAN_POINT('',(87.2090243917038,66.7948,13.4550625));
#83017=CARTESIAN_POINT('',(88.8129756082962,66.7948,13.4550625));
#83018=CARTESIAN_POINT('Origin',(88.011,66.7948,12.066));
#83019=CARTESIAN_POINT('Origin',(89.6149512165924,66.7948,12.066));
#83020=CARTESIAN_POINT('',(87.2090243917038,66.7948,13.4550625));
#83021=CARTESIAN_POINT('Origin',(88.011,66.7948,12.066));
#83022=CARTESIAN_POINT('Origin',(88.011,66.7948,12.066));
#83023=CARTESIAN_POINT('',(88.011,65.8310488791083,12.066));
#83024=CARTESIAN_POINT('',(86.4070487834076,66.7948,12.066));
#83025=CARTESIAN_POINT('Origin',(86.4070487834076,68.5948,12.066));
#83026=CARTESIAN_POINT('',(86.4070487834076,68.5948,12.066));
#83027=CARTESIAN_POINT('',(87.2090243917038,68.5948,10.6769375));
#83028=CARTESIAN_POINT('Origin',(87.2090243917038,68.5948,13.4550625));
#83029=CARTESIAN_POINT('',(87.2090243917038,68.5948,13.4550625));
#83030=CARTESIAN_POINT('Origin',(88.8129756082962,68.5948,13.4550625));
#83031=CARTESIAN_POINT('',(88.8129756082962,68.5948,13.4550625));
#83032=CARTESIAN_POINT('Origin',(89.6149512165924,68.5948,12.066));
#83033=CARTESIAN_POINT('',(89.6149512165924,68.5948,12.066));
#83034=CARTESIAN_POINT('Origin',(88.8129756082962,68.5948,10.6769375));
#83035=CARTESIAN_POINT('',(88.8129756082962,68.5948,10.6769375));
#83036=CARTESIAN_POINT('Origin',(87.2090243917038,68.5948,10.6769375));
#83037=CARTESIAN_POINT('',(0.,0.,0.));
#83038=CARTESIAN_POINT('Origin',(88.011,65.0396,12.066));
#83039=CARTESIAN_POINT('',(86.0298,64.9896,12.066));
#83040=CARTESIAN_POINT('Origin',(88.011,64.9896,12.066));
#83041=CARTESIAN_POINT('',(85.9298,65.0896,12.066));
#83042=CARTESIAN_POINT('',(85.9798,65.0396,12.066));
#83043=CARTESIAN_POINT('Origin',(88.011,65.0896,12.066));
#83044=CARTESIAN_POINT('Origin',(92.7735,65.0896,12.066));
#83045=CARTESIAN_POINT('',(83.2485,65.0896,12.066));
#83046=CARTESIAN_POINT('Origin',(88.011,65.0896,12.066));
#83047=CARTESIAN_POINT('Origin',(88.011,64.5423,12.066));
#83048=CARTESIAN_POINT('',(83.2485,63.995,12.066));
#83049=CARTESIAN_POINT('Origin',(88.011,63.995,12.066));
#83050=CARTESIAN_POINT('',(83.2485,64.5423,12.066));
#83051=CARTESIAN_POINT('Origin',(88.011,63.92,12.066));
#83052=CARTESIAN_POINT('',(83.3985,63.845,12.066));
#83053=CARTESIAN_POINT('',(83.3235,63.92,12.066));
#83054=CARTESIAN_POINT('Origin',(88.011,63.845,12.066));
#83055=CARTESIAN_POINT('Origin',(89.9922,63.845,12.066));
#83056=CARTESIAN_POINT('',(86.0298,63.845,12.066));
#83057=CARTESIAN_POINT('Origin',(88.011,63.845,12.066));
#83058=CARTESIAN_POINT('Origin',(88.011,64.4173,12.066));
#83059=CARTESIAN_POINT('',(86.0298,64.4173,12.066));
#83060=CARTESIAN_POINT('',(0.,0.,0.));
#83061=CARTESIAN_POINT('Origin',(88.011,52.9504,12.066));
#83062=CARTESIAN_POINT('',(86.2085,52.8254,12.066));
#83063=CARTESIAN_POINT('Origin',(88.011,52.8254,12.066));
#83064=CARTESIAN_POINT('',(85.9585,53.0754,12.066));
#83065=CARTESIAN_POINT('',(86.0835,52.9504,12.066));
#83066=CARTESIAN_POINT('Origin',(88.011,53.0754,12.066));
#83067=CARTESIAN_POINT('Origin',(88.011,53.0754,12.066));
#83068=CARTESIAN_POINT('',(86.2085,50.1254,12.066));
#83069=CARTESIAN_POINT('',(86.2085,53.0754,12.066));
#83070=CARTESIAN_POINT('Origin',(88.011,50.1254,12.066));
#83071=CARTESIAN_POINT('Origin',(88.011,53.0754,12.066));
#83072=CARTESIAN_POINT('',(84.2406875,53.0754,12.066));
#83073=CARTESIAN_POINT('Origin',(88.011,53.0754,12.066));
#83074=CARTESIAN_POINT('Origin',(88.011,49.516,12.066));
#83075=CARTESIAN_POINT('',(84.411,48.9066,12.066));
#83076=CARTESIAN_POINT('Origin',(88.011,48.9066,12.066));
#83077=CARTESIAN_POINT('',(84.411,50.1254,12.066));
#83078=CARTESIAN_POINT('',(84.411,49.516,12.066));
#83079=CARTESIAN_POINT('Origin',(88.011,50.1254,12.066));
#83080=CARTESIAN_POINT('Origin',(88.011,48.8066,12.066));
#83081=CARTESIAN_POINT('',(84.611,48.7066,12.066));
#83082=CARTESIAN_POINT('',(84.511,48.8066,12.066));
#83083=CARTESIAN_POINT('Origin',(88.011,48.7066,12.066));
#83084=CARTESIAN_POINT('Origin',(89.911,48.7066,12.066));
#83085=CARTESIAN_POINT('',(86.111,48.7066,12.066));
#83086=CARTESIAN_POINT('Origin',(88.011,48.7066,12.066));
#83087=CARTESIAN_POINT('Origin',(88.011,49.416,12.066));
#83088=CARTESIAN_POINT('',(86.111,50.1254,12.066));
#83089=CARTESIAN_POINT('Origin',(88.011,50.1254,12.066));
#83090=CARTESIAN_POINT('',(86.111,49.416,12.066));
#83091=CARTESIAN_POINT('Origin',(88.011,50.1254,12.066));
#83092=CARTESIAN_POINT('Origin',(88.011,52.6965412344379,12.066));
#83093=CARTESIAN_POINT('',(85.7196411191537,52.6063576034707,16.03475));
#83094=CARTESIAN_POINT('',(83.4282822383073,52.6063576034707,12.066));
#83095=CARTESIAN_POINT('Ctrl Pts',(85.7196411191537,52.6063576034707,16.03475));
#83096=CARTESIAN_POINT('Ctrl Pts',(84.5739616787304,53.2678159368036,14.0503749999999));
#83097=CARTESIAN_POINT('Ctrl Pts',(83.4282822383073,52.6063576034707,12.066));
#83098=CARTESIAN_POINT('',(90.3023588808463,52.6063576034707,16.03475));
#83099=CARTESIAN_POINT('Ctrl Pts',(90.3023588808463,52.6063576034707,16.03475));
#83100=CARTESIAN_POINT('Ctrl Pts',(88.0109999999998,53.2678159368036,16.03475));
#83101=CARTESIAN_POINT('Ctrl Pts',(85.7196411191537,52.6063576034707,16.03475));
#83102=CARTESIAN_POINT('',(92.5937177616926,52.6063576034707,12.066));
#83103=CARTESIAN_POINT('Ctrl Pts',(92.5937177616926,52.6063576034707,12.066));
#83104=CARTESIAN_POINT('Ctrl Pts',(91.4480383212694,53.2678159368036,14.0503750000001));
#83105=CARTESIAN_POINT('Ctrl Pts',(90.3023588808463,52.6063576034707,16.03475));
#83106=CARTESIAN_POINT('',(90.3023588808463,52.6063576034707,8.09725));
#83107=CARTESIAN_POINT('Ctrl Pts',(90.3023588808463,52.6063576034707,8.09725));
#83108=CARTESIAN_POINT('Ctrl Pts',(91.4480383212696,53.2678159368036,10.0816250000001));
#83109=CARTESIAN_POINT('Ctrl Pts',(92.5937177616926,52.6063576034707,12.066));
#83110=CARTESIAN_POINT('',(85.7196411191537,52.6063576034707,8.09725));
#83111=CARTESIAN_POINT('Ctrl Pts',(85.7196411191537,52.6063576034707,8.09725));
#83112=CARTESIAN_POINT('Ctrl Pts',(88.0110000000002,53.2678159368036,8.09725));
#83113=CARTESIAN_POINT('Ctrl Pts',(90.3023588808463,52.6063576034707,8.09725));
#83114=CARTESIAN_POINT('Ctrl Pts',(83.4282822383073,52.6063576034707,12.066));
#83115=CARTESIAN_POINT('Ctrl Pts',(84.5739616787306,53.2678159368036,10.0816249999999));
#83116=CARTESIAN_POINT('Ctrl Pts',(85.7196411191537,52.6063576034707,8.09725000000001));
#83117=CARTESIAN_POINT('',(83.5844848691537,52.6965412344379,12.066));
#83118=CARTESIAN_POINT('Origin',(83.4282822383073,50.1254,12.066));
#83119=CARTESIAN_POINT('',(83.4282822383073,50.1254,12.066));
#83120=CARTESIAN_POINT('',(83.4282822383073,50.1254,12.066));
#83121=CARTESIAN_POINT('',(85.7196411191537,50.1254,16.03475));
#83122=CARTESIAN_POINT('',(85.7196411191537,50.1254,16.03475));
#83123=CARTESIAN_POINT('',(85.7196411191537,50.1254,16.03475));
#83124=CARTESIAN_POINT('Origin',(85.7196411191537,50.1254,8.09725));
#83125=CARTESIAN_POINT('',(85.7196411191537,50.1254,8.09725));
#83126=CARTESIAN_POINT('',(85.7196411191537,50.1254,8.09725));
#83127=CARTESIAN_POINT('',(83.4282822383073,50.1254,12.066));
#83128=CARTESIAN_POINT('Origin',(90.3023588808463,50.1254,8.09725));
#83129=CARTESIAN_POINT('',(90.3023588808463,50.1254,8.09725));
#83130=CARTESIAN_POINT('',(90.3023588808463,50.1254,8.09725));
#83131=CARTESIAN_POINT('',(85.7196411191537,50.1254,8.09725));
#83132=CARTESIAN_POINT('Origin',(92.5937177616926,50.1254,12.066));
#83133=CARTESIAN_POINT('',(92.5937177616926,50.1254,12.066));
#83134=CARTESIAN_POINT('',(92.5937177616926,50.1254,12.066));
#83135=CARTESIAN_POINT('',(90.3023588808463,50.1254,8.09725));
#83136=CARTESIAN_POINT('Origin',(90.3023588808463,50.1254,16.03475));
#83137=CARTESIAN_POINT('',(90.3023588808463,50.1254,16.03475));
#83138=CARTESIAN_POINT('',(90.3023588808463,50.1254,16.03475));
#83139=CARTESIAN_POINT('',(92.5937177616926,50.1254,12.066));
#83140=CARTESIAN_POINT('Origin',(85.7196411191537,50.1254,16.03475));
#83141=CARTESIAN_POINT('',(90.3023588808463,50.1254,16.03475));
#83142=CARTESIAN_POINT('Origin',(88.011,50.1254,12.066));
#83143=CARTESIAN_POINT('',(0.,0.,0.));
#83144=CARTESIAN_POINT('',(0.,0.,0.));
#83145=CARTESIAN_POINT('',(0.,0.,0.));
#83146=CARTESIAN_POINT('',(0.,0.,0.));
#83147=CARTESIAN_POINT('',(0.,0.,0.));
#83148=CARTESIAN_POINT('',(0.,0.,0.));
#83149=CARTESIAN_POINT('',(0.,0.,0.));
#83150=CARTESIAN_POINT('',(0.,0.,0.));
#83151=CARTESIAN_POINT('',(0.,0.,0.));
#83152=CARTESIAN_POINT('',(0.,0.,0.));
#83153=CARTESIAN_POINT('',(0.,0.,0.));
#83154=CARTESIAN_POINT('',(0.,0.,0.));
#83155=CARTESIAN_POINT('',(0.,0.,0.));
#83156=CARTESIAN_POINT('',(0.,0.,0.));
#83157=CARTESIAN_POINT('',(0.,0.,0.));
#83158=CARTESIAN_POINT('',(0.,0.,0.));
#83159=CARTESIAN_POINT('',(0.,0.,0.));
#83160=CARTESIAN_POINT('',(0.,0.,0.));
#83161=CARTESIAN_POINT('',(0.,0.,-26.94));
#83162=CARTESIAN_POINT('',(0.,0.,26.94));
#83163=CARTESIAN_POINT('',(0.,0.,0.));
#83164=CARTESIAN_POINT('',(0.,-26.9494,4.82));
#83165=CARTESIAN_POINT('',(0.,-26.9494,-31.76));
#83166=CARTESIAN_POINT('',(0.,-26.9494,31.76));
#83167=CARTESIAN_POINT('',(0.,-26.9494,-4.82));
#83168=CARTESIAN_POINT('',(-58.1754,55.875,4.82));
#83169=CARTESIAN_POINT('',(-58.1754,55.875,-31.76));
#83170=CARTESIAN_POINT('',(-85.1154,55.875,4.82));
#83171=CARTESIAN_POINT('',(-85.1154,55.875,-31.76));
#83172=CARTESIAN_POINT('',(0.,0.,-15.74));
#83173=CARTESIAN_POINT('',(67.32,0.,0.));
#83174=CARTESIAN_POINT('',(67.32,0.,-15.74));
#83175=CARTESIAN_POINT('',(-176.022,0.,0.));
#83176=CARTESIAN_POINT('',(0.,0.,-24.132));
#83177=CARTESIAN_POINT('',(-176.022,0.,-24.132));
#83178=CARTESIAN_POINT('',(-176.022,0.,0.));
#83179=CARTESIAN_POINT('',(0.,0.,-24.132));
#83180=CARTESIAN_POINT('',(-176.022,0.,-24.132));
#83181=CARTESIAN_POINT('',(0.,118.165,24.132));
#83182=CARTESIAN_POINT('',(-176.022,118.165,24.132));
#83183=CARTESIAN_POINT('',(0.,118.165,0.));
#83184=CARTESIAN_POINT('',(-176.022,118.165,0.));
#83185=CARTESIAN_POINT('',(-176.022,0.,0.));
#83186=CARTESIAN_POINT('',(0.,0.,-24.132));
#83187=CARTESIAN_POINT('',(-176.022,0.,-24.132));
#83188=UNCERTAINTY_MEASURE_WITH_UNIT(LENGTH_MEASURE(0.01),#83220,
'DISTANCE_ACCURACY_VALUE',
'Maximum model space distance between geometric entities at asserted c
onnectivities');
#83189=UNCERTAINTY_MEASURE_WITH_UNIT(LENGTH_MEASURE(0.01),#83220,
'DISTANCE_ACCURACY_VALUE',
'Maximum model space distance between geometric entities at asserted c
onnectivities');
#83190=UNCERTAINTY_MEASURE_WITH_UNIT(LENGTH_MEASURE(0.01),#83220,
'DISTANCE_ACCURACY_VALUE',
'Maximum model space distance between geometric entities at asserted c
onnectivities');
#83191=UNCERTAINTY_MEASURE_WITH_UNIT(LENGTH_MEASURE(0.01),#83220,
'DISTANCE_ACCURACY_VALUE',
'Maximum model space distance between geometric entities at asserted c
onnectivities');
#83192=UNCERTAINTY_MEASURE_WITH_UNIT(LENGTH_MEASURE(0.01),#83220,
'DISTANCE_ACCURACY_VALUE',
'Maximum model space distance between geometric entities at asserted c
onnectivities');
#83193=UNCERTAINTY_MEASURE_WITH_UNIT(LENGTH_MEASURE(0.01),#83220,
'DISTANCE_ACCURACY_VALUE',
'Maximum model space distance between geometric entities at asserted c
onnectivities');
#83194=UNCERTAINTY_MEASURE_WITH_UNIT(LENGTH_MEASURE(0.01),#83220,
'DISTANCE_ACCURACY_VALUE',
'Maximum model space distance between geometric entities at asserted c
onnectivities');
#83195=UNCERTAINTY_MEASURE_WITH_UNIT(LENGTH_MEASURE(0.01),#83220,
'DISTANCE_ACCURACY_VALUE',
'Maximum model space distance between geometric entities at asserted c
onnectivities');
#83196=UNCERTAINTY_MEASURE_WITH_UNIT(LENGTH_MEASURE(0.01),#83220,
'DISTANCE_ACCURACY_VALUE',
'Maximum model space distance between geometric entities at asserted c
onnectivities');
#83197=UNCERTAINTY_MEASURE_WITH_UNIT(LENGTH_MEASURE(0.01),#83220,
'DISTANCE_ACCURACY_VALUE',
'Maximum model space distance between geometric entities at asserted c
onnectivities');
#83198=UNCERTAINTY_MEASURE_WITH_UNIT(LENGTH_MEASURE(0.01),#83220,
'DISTANCE_ACCURACY_VALUE',
'Maximum model space distance between geometric entities at asserted c
onnectivities');
#83199=UNCERTAINTY_MEASURE_WITH_UNIT(LENGTH_MEASURE(0.01),#83220,
'DISTANCE_ACCURACY_VALUE',
'Maximum model space distance between geometric entities at asserted c
onnectivities');
#83200=UNCERTAINTY_MEASURE_WITH_UNIT(LENGTH_MEASURE(0.01),#83220,
'DISTANCE_ACCURACY_VALUE',
'Maximum model space distance between geometric entities at asserted c
onnectivities');
#83201=UNCERTAINTY_MEASURE_WITH_UNIT(LENGTH_MEASURE(0.01),#83220,
'DISTANCE_ACCURACY_VALUE',
'Maximum model space distance between geometric entities at asserted c
onnectivities');
#83202=UNCERTAINTY_MEASURE_WITH_UNIT(LENGTH_MEASURE(0.01),#83220,
'DISTANCE_ACCURACY_VALUE',
'Maximum model space distance between geometric entities at asserted c
onnectivities');
#83203=UNCERTAINTY_MEASURE_WITH_UNIT(LENGTH_MEASURE(0.01),#83220,
'DISTANCE_ACCURACY_VALUE',
'Maximum model space distance between geometric entities at asserted c
onnectivities');
#83204=(
GEOMETRIC_REPRESENTATION_CONTEXT(3)
GLOBAL_UNCERTAINTY_ASSIGNED_CONTEXT((#83188))
GLOBAL_UNIT_ASSIGNED_CONTEXT((#83220,#83222,#83223))
REPRESENTATION_CONTEXT('','3D')
);
#83205=(
GEOMETRIC_REPRESENTATION_CONTEXT(3)
GLOBAL_UNCERTAINTY_ASSIGNED_CONTEXT((#83189))
GLOBAL_UNIT_ASSIGNED_CONTEXT((#83220,#83222,#83223))
REPRESENTATION_CONTEXT('','3D')
);
#83206=(
GEOMETRIC_REPRESENTATION_CONTEXT(3)
GLOBAL_UNCERTAINTY_ASSIGNED_CONTEXT((#83190))
GLOBAL_UNIT_ASSIGNED_CONTEXT((#83220,#83222,#83223))
REPRESENTATION_CONTEXT('','3D')
);
#83207=(
GEOMETRIC_REPRESENTATION_CONTEXT(3)
GLOBAL_UNCERTAINTY_ASSIGNED_CONTEXT((#83191))
GLOBAL_UNIT_ASSIGNED_CONTEXT((#83220,#83222,#83223))
REPRESENTATION_CONTEXT('','3D')
);
#83208=(
GEOMETRIC_REPRESENTATION_CONTEXT(3)
GLOBAL_UNCERTAINTY_ASSIGNED_CONTEXT((#83192))
GLOBAL_UNIT_ASSIGNED_CONTEXT((#83220,#83222,#83223))
REPRESENTATION_CONTEXT('','3D')
);
#83209=(
GEOMETRIC_REPRESENTATION_CONTEXT(3)
GLOBAL_UNCERTAINTY_ASSIGNED_CONTEXT((#83193))
GLOBAL_UNIT_ASSIGNED_CONTEXT((#83220,#83222,#83223))
REPRESENTATION_CONTEXT('','3D')
);
#83210=(
GEOMETRIC_REPRESENTATION_CONTEXT(3)
GLOBAL_UNCERTAINTY_ASSIGNED_CONTEXT((#83194))
GLOBAL_UNIT_ASSIGNED_CONTEXT((#83220,#83222,#83223))
REPRESENTATION_CONTEXT('','3D')
);
#83211=(
GEOMETRIC_REPRESENTATION_CONTEXT(3)
GLOBAL_UNCERTAINTY_ASSIGNED_CONTEXT((#83195))
GLOBAL_UNIT_ASSIGNED_CONTEXT((#83220,#83222,#83223))
REPRESENTATION_CONTEXT('','3D')
);
#83212=(
GEOMETRIC_REPRESENTATION_CONTEXT(3)
GLOBAL_UNCERTAINTY_ASSIGNED_CONTEXT((#83196))
GLOBAL_UNIT_ASSIGNED_CONTEXT((#83220,#83222,#83223))
REPRESENTATION_CONTEXT('','3D')
);
#83213=(
GEOMETRIC_REPRESENTATION_CONTEXT(3)
GLOBAL_UNCERTAINTY_ASSIGNED_CONTEXT((#83197))
GLOBAL_UNIT_ASSIGNED_CONTEXT((#83220,#83222,#83223))
REPRESENTATION_CONTEXT('','3D')
);
#83214=(
GEOMETRIC_REPRESENTATION_CONTEXT(3)
GLOBAL_UNCERTAINTY_ASSIGNED_CONTEXT((#83198))
GLOBAL_UNIT_ASSIGNED_CONTEXT((#83220,#83222,#83223))
REPRESENTATION_CONTEXT('','3D')
);
#83215=(
GEOMETRIC_REPRESENTATION_CONTEXT(3)
GLOBAL_UNCERTAINTY_ASSIGNED_CONTEXT((#83199))
GLOBAL_UNIT_ASSIGNED_CONTEXT((#83220,#83222,#83223))
REPRESENTATION_CONTEXT('','3D')
);
#83216=(
GEOMETRIC_REPRESENTATION_CONTEXT(3)
GLOBAL_UNCERTAINTY_ASSIGNED_CONTEXT((#83200))
GLOBAL_UNIT_ASSIGNED_CONTEXT((#83220,#83222,#83223))
REPRESENTATION_CONTEXT('','3D')
);
#83217=(
GEOMETRIC_REPRESENTATION_CONTEXT(3)
GLOBAL_UNCERTAINTY_ASSIGNED_CONTEXT((#83201))
GLOBAL_UNIT_ASSIGNED_CONTEXT((#83220,#83222,#83223))
REPRESENTATION_CONTEXT('','3D')
);
#83218=(
GEOMETRIC_REPRESENTATION_CONTEXT(3)
GLOBAL_UNCERTAINTY_ASSIGNED_CONTEXT((#83202))
GLOBAL_UNIT_ASSIGNED_CONTEXT((#83220,#83222,#83223))
REPRESENTATION_CONTEXT('','3D')
);
#83219=(
GEOMETRIC_REPRESENTATION_CONTEXT(3)
GLOBAL_UNCERTAINTY_ASSIGNED_CONTEXT((#83203))
GLOBAL_UNIT_ASSIGNED_CONTEXT((#83220,#83222,#83223))
REPRESENTATION_CONTEXT('','3D')
);
#83220=(
LENGTH_UNIT()
NAMED_UNIT(*)
SI_UNIT(.MILLI.,.METRE.)
);
#83221=(
LENGTH_UNIT()
NAMED_UNIT(*)
SI_UNIT($,.METRE.)
);
#83222=(
NAMED_UNIT(*)
PLANE_ANGLE_UNIT()
SI_UNIT($,.RADIAN.)
);
#83223=(
NAMED_UNIT(*)
SI_UNIT($,.STERADIAN.)
SOLID_ANGLE_UNIT()
);
#83224=SHAPE_DEFINITION_REPRESENTATION(#83239,#83299);
#83225=SHAPE_DEFINITION_REPRESENTATION(#83240,#83300);
#83226=SHAPE_DEFINITION_REPRESENTATION(#83241,#83301);
#83227=SHAPE_DEFINITION_REPRESENTATION(#83242,#83302);
#83228=SHAPE_DEFINITION_REPRESENTATION(#83243,#83303);
#83229=SHAPE_DEFINITION_REPRESENTATION(#83244,#83304);
#83230=SHAPE_DEFINITION_REPRESENTATION(#83245,#83305);
#83231=SHAPE_DEFINITION_REPRESENTATION(#83246,#83306);
#83232=SHAPE_DEFINITION_REPRESENTATION(#83247,#83307);
#83233=SHAPE_DEFINITION_REPRESENTATION(#83248,#83308);
#83234=SHAPE_DEFINITION_REPRESENTATION(#83249,#83309);
#83235=SHAPE_DEFINITION_REPRESENTATION(#83250,#83310);
#83236=SHAPE_DEFINITION_REPRESENTATION(#83251,#83311);
#83237=SHAPE_DEFINITION_REPRESENTATION(#83252,#83312);
#83238=SHAPE_DEFINITION_REPRESENTATION(#83253,#83313);
#83239=PRODUCT_DEFINITION_SHAPE('',$,#83315);
#83240=PRODUCT_DEFINITION_SHAPE('',$,#83316);
#83241=PRODUCT_DEFINITION_SHAPE('',$,#83317);
#83242=PRODUCT_DEFINITION_SHAPE('',$,#83318);
#83243=PRODUCT_DEFINITION_SHAPE('',$,#83319);
#83244=PRODUCT_DEFINITION_SHAPE('',$,#83320);
#83245=PRODUCT_DEFINITION_SHAPE('',$,#83321);
#83246=PRODUCT_DEFINITION_SHAPE('',$,#83322);
#83247=PRODUCT_DEFINITION_SHAPE('',$,#83323);
#83248=PRODUCT_DEFINITION_SHAPE('',$,#83324);
#83249=PRODUCT_DEFINITION_SHAPE('',$,#83325);
#83250=PRODUCT_DEFINITION_SHAPE('',$,#83326);
#83251=PRODUCT_DEFINITION_SHAPE('',$,#83327);
#83252=PRODUCT_DEFINITION_SHAPE('',$,#83328);
#83253=PRODUCT_DEFINITION_SHAPE('',$,#83329);
#83254=PRODUCT_DEFINITION_SHAPE($,$,#146);
#83255=PRODUCT_DEFINITION_SHAPE($,$,#147);
#83256=PRODUCT_DEFINITION_SHAPE($,$,#148);
#83257=PRODUCT_DEFINITION_SHAPE($,$,#149);
#83258=PRODUCT_DEFINITION_SHAPE($,$,#150);
#83259=PRODUCT_DEFINITION_SHAPE($,$,#151);
#83260=PRODUCT_DEFINITION_SHAPE($,$,#152);
#83261=PRODUCT_DEFINITION_SHAPE($,$,#153);
#83262=PRODUCT_DEFINITION_SHAPE($,$,#154);
#83263=PRODUCT_DEFINITION_SHAPE($,$,#155);
#83264=PRODUCT_DEFINITION_SHAPE($,$,#156);
#83265=PRODUCT_DEFINITION_SHAPE($,$,#157);
#83266=PRODUCT_DEFINITION_SHAPE($,$,#158);
#83267=PRODUCT_DEFINITION_SHAPE($,$,#159);
#83268=PRODUCT_DEFINITION_SHAPE($,$,#160);
#83269=PRODUCT_DEFINITION_SHAPE($,$,#161);
#83270=PRODUCT_DEFINITION_SHAPE($,$,#162);
#83271=PRODUCT_DEFINITION_SHAPE($,$,#163);
#83272=PRODUCT_DEFINITION_SHAPE($,$,#164);
#83273=PRODUCT_DEFINITION_SHAPE($,$,#165);
#83274=PRODUCT_DEFINITION_SHAPE($,$,#166);
#83275=PRODUCT_DEFINITION_SHAPE($,$,#167);
#83276=PRODUCT_DEFINITION_SHAPE($,$,#168);
#83277=PRODUCT_DEFINITION_SHAPE($,$,#169);
#83278=PRODUCT_DEFINITION_SHAPE($,$,#170);
#83279=PRODUCT_DEFINITION_SHAPE($,$,#171);
#83280=PRODUCT_DEFINITION_SHAPE($,$,#172);
#83281=PRODUCT_DEFINITION_SHAPE($,$,#173);
#83282=PRODUCT_DEFINITION_SHAPE($,$,#174);
#83283=PRODUCT_DEFINITION_SHAPE($,$,#175);
#83284=PRODUCT_DEFINITION_SHAPE($,$,#176);
#83285=PRODUCT_DEFINITION_SHAPE($,$,#177);
#83286=PRODUCT_DEFINITION_SHAPE($,$,#178);
#83287=PRODUCT_DEFINITION_SHAPE($,$,#179);
#83288=PRODUCT_DEFINITION_SHAPE($,$,#180);
#83289=PRODUCT_DEFINITION_SHAPE($,$,#181);
#83290=PRODUCT_DEFINITION_SHAPE($,$,#182);
#83291=PRODUCT_DEFINITION_SHAPE($,$,#183);
#83292=PRODUCT_DEFINITION_SHAPE($,$,#184);
#83293=PRODUCT_DEFINITION_SHAPE($,$,#185);
#83294=PRODUCT_DEFINITION_SHAPE($,$,#186);
#83295=PRODUCT_DEFINITION_SHAPE($,$,#187);
#83296=PRODUCT_DEFINITION_SHAPE($,$,#188);
#83297=PRODUCT_DEFINITION_SHAPE($,$,#189);
#83298=PRODUCT_DEFINITION_SHAPE($,$,#190);
#83299=SHAPE_REPRESENTATION('',(#27098,#29210,#29211,#29212,#29213,#29214,
#29215,#29216,#29217,#29218,#29219,#29220,#29221,#29222,#29223,#29224,#29225,
#29226,#29227,#29228,#29229,#29230,#29231,#29232,#29233,#29234,#29235,#29236,
#29237,#29238,#29239,#29240,#29241,#29242,#29243,#29244,#29245,#29246,#29247,
#29248,#29249,#29250,#29251,#29252,#29253,#29254),#83204);
#83300=SHAPE_REPRESENTATION('',(#27099),#83205);
#83301=SHAPE_REPRESENTATION('',(#27207),#83206);
#83302=SHAPE_REPRESENTATION('',(#27360),#83207);
#83303=SHAPE_REPRESENTATION('',(#27453),#83208);
#83304=SHAPE_REPRESENTATION('',(#27595),#83209);
#83305=SHAPE_REPRESENTATION('',(#27872),#83210);
#83306=SHAPE_REPRESENTATION('',(#28000),#83211);
#83307=SHAPE_REPRESENTATION('',(#28335),#83212);
#83308=SHAPE_REPRESENTATION('',(#28406),#83213);
#83309=SHAPE_REPRESENTATION('',(#28461),#83214);
#83310=SHAPE_REPRESENTATION('',(#28693),#83215);
#83311=SHAPE_REPRESENTATION('',(#28927),#83216);
#83312=SHAPE_REPRESENTATION('',(#29171),#83217);
#83313=SHAPE_REPRESENTATION('',(#29184),#83218);
#83314=PRODUCT_DEFINITION_CONTEXT('part definition',#83361,'design');
#83315=PRODUCT_DEFINITION('MAS-260',
'MAS-260',#83330,#83314);
#83316=PRODUCT_DEFINITION('90 Degree Quad Hub Mount B',
'90 Degree Quad Hub Mount B',#83331,#83314);
#83317=PRODUCT_DEFINITION('Large Servo Plate A','Large Servo Plate A',#83332,
#83314);
#83318=PRODUCT_DEFINITION('Winch Servo','Winch Servo',#83333,#83314);
#83319=PRODUCT_DEFINITION('16T 32P Metal Servo Gear',
'16T 32P Metal Servo Gear',#83334,#83314);
#83320=PRODUCT_DEFINITION('ISO 4762 - M3 x 6 - Servo Gear Screw',
'ISO 4762 - M3 x 6 - Servo Gear Screw',#83335,#83314);
#83321=PRODUCT_DEFINITION('Aluminum Beam (cut to 21 holes)',
'Aluminum Beam (cut to 21 holes)',#83336,#83314);
#83322=PRODUCT_DEFINITION('32P Beam Gear Rack Acetal (cut to 70T)',
'32P Beam Gear Rack Acetal (cut to 70T)',#83337,#83314);
#83323=PRODUCT_DEFINITION('Beam Bracket W Acetal',
'Beam Bracket W Acetal',#83338,#83314);
#83324=PRODUCT_DEFINITION('90 Degree Dual Side Mount',
'90 Degree Dual Side Mount',#83339,#83314);
#83325=PRODUCT_DEFINITION('ASME B18.3 SHCS 6-32 UNC x 0.25',
'ASME B18.3 SHCS 6-32 UNC x 0.25',#83340,#83314);
#83326=PRODUCT_DEFINITION('ASME B18.3 SHCS 6-32 UNC x 0.3125',
'ASME B18.3 SHCS 6-32 UNC x 0.3125',#83341,#83314);
#83327=PRODUCT_DEFINITION('ASME B18.3 SHCS 6-32 UNC x 0.625',
'ASME B18.3 SHCS 6-32 UNC x 0.625',#83342,#83314);
#83328=PRODUCT_DEFINITION('ASME B18.22.1 Plain Washer No.6 Narrow',
'ASME B18.22.1 Plain Washer No.6 Narrow',#83343,#83314);
#83329=PRODUCT_DEFINITION(
'ASME B18.16.6 Nylon Insert Lock Nut 6-32 UNC',
'ASME B18.16.6 Nylon Insert Lock Nut 6-32 UNC',#83344,#83314);
#83330=PRODUCT_DEFINITION_FORMATION('',$,#83363);
#83331=PRODUCT_DEFINITION_FORMATION('',$,#83364);
#83332=PRODUCT_DEFINITION_FORMATION('',$,#83365);
#83333=PRODUCT_DEFINITION_FORMATION('',$,#83366);
#83334=PRODUCT_DEFINITION_FORMATION('',$,#83367);
#83335=PRODUCT_DEFINITION_FORMATION('',$,#83368);
#83336=PRODUCT_DEFINITION_FORMATION('',$,#83369);
#83337=PRODUCT_DEFINITION_FORMATION('',$,#83370);
#83338=PRODUCT_DEFINITION_FORMATION('',$,#83371);
#83339=PRODUCT_DEFINITION_FORMATION('',$,#83372);
#83340=PRODUCT_DEFINITION_FORMATION('',$,#83373);
#83341=PRODUCT_DEFINITION_FORMATION('',$,#83374);
#83342=PRODUCT_DEFINITION_FORMATION('',$,#83375);
#83343=PRODUCT_DEFINITION_FORMATION('',$,#83376);
#83344=PRODUCT_DEFINITION_FORMATION('',$,#83377);
#83345=PRODUCT_RELATED_PRODUCT_CATEGORY(
'MAS-260','MAS-260',(#83363));
#83346=PRODUCT_RELATED_PRODUCT_CATEGORY('90 Degree Quad Hub Mount B',
'90 Degree Quad Hub Mount B',(#83364));
#83347=PRODUCT_RELATED_PRODUCT_CATEGORY('Large Servo Plate A',
'Large Servo Plate A',(#83365));
#83348=PRODUCT_RELATED_PRODUCT_CATEGORY('Winch Servo','Winch Servo',(#83366));
#83349=PRODUCT_RELATED_PRODUCT_CATEGORY('16T 32P Metal Servo Gear',
'16T 32P Metal Servo Gear',(#83367));
#83350=PRODUCT_RELATED_PRODUCT_CATEGORY(
'ISO 4762 - M3 x 6 - Servo Gear Screw',
'ISO 4762 - M3 x 6 - Servo Gear Screw',(#83368));
#83351=PRODUCT_RELATED_PRODUCT_CATEGORY(
'Aluminum Beam (cut to 21 holes)','Aluminum Beam (cut to 21 holes)',(#83369));
#83352=PRODUCT_RELATED_PRODUCT_CATEGORY(
'32P Beam Gear Rack Acetal (cut to 70T)',
'32P Beam Gear Rack Acetal (cut to 70T)',(#83370));
#83353=PRODUCT_RELATED_PRODUCT_CATEGORY('Beam Bracket W Acetal',
'Beam Bracket W Acetal',(#83371));
#83354=PRODUCT_RELATED_PRODUCT_CATEGORY('90 Degree Dual Side Mount',
'90 Degree Dual Side Mount',(#83372));
#83355=PRODUCT_RELATED_PRODUCT_CATEGORY(
'ASME B18.3 SHCS 6-32 UNC x 0.25','ASME B18.3 SHCS 6-32 UNC x 0.25',(#83373));
#83356=PRODUCT_RELATED_PRODUCT_CATEGORY(
'ASME B18.3 SHCS 6-32 UNC x 0.3125','ASME B18.3 SHCS 6-32 UNC x 0.3125',
(#83374));
#83357=PRODUCT_RELATED_PRODUCT_CATEGORY(
'ASME B18.3 SHCS 6-32 UNC x 0.625','ASME B18.3 SHCS 6-32 UNC x 0.625',(#83375));
#83358=PRODUCT_RELATED_PRODUCT_CATEGORY(
'ASME B18.22.1 Plain Washer No.6 Narrow',
'ASME B18.22.1 Plain Washer No.6 Narrow',(#83376));
#83359=PRODUCT_RELATED_PRODUCT_CATEGORY(
'ASME B18.16.6 Nylon Insert Lock Nut 6-32 UNC',
'ASME B18.16.6 Nylon Insert Lock Nut 6-32 UNC',(#83377));
#83360=APPLICATION_PROTOCOL_DEFINITION('international standard',
'automotive_design',2009,#83361);
#83361=APPLICATION_CONTEXT(
'Core Data for Automotive Mechanical Design Process');
#83362=PRODUCT_CONTEXT('part definition',#83361,'mechanical');
#83363=PRODUCT('MAS-260',
'MAS-260',$,(#83362));
#83364=PRODUCT('90 Degree Quad Hub Mount B',
'90 Degree Quad Hub Mount B',$,(#83362));
#83365=PRODUCT('Large Servo Plate A','Large Servo Plate A',$,(#83362));
#83366=PRODUCT('Winch Servo','Winch Servo',$,(#83362));
#83367=PRODUCT('16T 32P Metal Servo Gear','16T 32P Metal Servo Gear',$,
(#83362));
#83368=PRODUCT('ISO 4762 - M3 x 6 - Servo Gear Screw',
'ISO 4762 - M3 x 6 - Servo Gear Screw',$,(#83362));
#83369=PRODUCT('Aluminum Beam (cut to 21 holes)',
'Aluminum Beam (cut to 21 holes)',$,(#83362));
#83370=PRODUCT('32P Beam Gear Rack Acetal (cut to 70T)',
'32P Beam Gear Rack Acetal (cut to 70T)',$,(#83362));
#83371=PRODUCT('Beam Bracket W Acetal','Beam Bracket W Acetal',$,(#83362));
#83372=PRODUCT('90 Degree Dual Side Mount','90 Degree Dual Side Mount',
$,(#83362));
#83373=PRODUCT('ASME B18.3 SHCS 6-32 UNC x 0.25',
'ASME B18.3 SHCS 6-32 UNC x 0.25',$,(#83362));
#83374=PRODUCT('ASME B18.3 SHCS 6-32 UNC x 0.3125',
'ASME B18.3 SHCS 6-32 UNC x 0.3125',$,(#83362));
#83375=PRODUCT('ASME B18.3 SHCS 6-32 UNC x 0.625',
'ASME B18.3 SHCS 6-32 UNC x 0.625',$,(#83362));
#83376=PRODUCT('ASME B18.22.1 Plain Washer No.6 Narrow',
'ASME B18.22.1 Plain Washer No.6 Narrow',$,(#83362));
#83377=PRODUCT('ASME B18.16.6 Nylon Insert Lock Nut 6-32 UNC',
'ASME B18.16.6 Nylon Insert Lock Nut 6-32 UNC',$,(#83362));
#83378=PRESENTATION_STYLE_ASSIGNMENT((#83393));
#83379=PRESENTATION_STYLE_ASSIGNMENT((#83394));
#83380=PRESENTATION_STYLE_ASSIGNMENT((#83395));
#83381=PRESENTATION_STYLE_ASSIGNMENT((#83396));
#83382=PRESENTATION_STYLE_ASSIGNMENT((#83397));
#83383=PRESENTATION_STYLE_ASSIGNMENT((#83398));
#83384=PRESENTATION_STYLE_ASSIGNMENT((#83399));
#83385=PRESENTATION_STYLE_ASSIGNMENT((#83400));
#83386=PRESENTATION_STYLE_ASSIGNMENT((#83401));
#83387=PRESENTATION_STYLE_ASSIGNMENT((#83402));
#83388=PRESENTATION_STYLE_ASSIGNMENT((#83403));
#83389=PRESENTATION_STYLE_ASSIGNMENT((#83404));
#83390=PRESENTATION_STYLE_ASSIGNMENT((#83405));
#83391=PRESENTATION_STYLE_ASSIGNMENT((#83406));
#83392=PRESENTATION_STYLE_ASSIGNMENT((#83407));
#83393=SURFACE_STYLE_USAGE(.BOTH.,#83408);
#83394=SURFACE_STYLE_USAGE(.BOTH.,#83409);
#83395=SURFACE_STYLE_USAGE(.BOTH.,#83410);
#83396=SURFACE_STYLE_USAGE(.BOTH.,#83411);
#83397=SURFACE_STYLE_USAGE(.BOTH.,#83412);
#83398=SURFACE_STYLE_USAGE(.BOTH.,#83413);
#83399=SURFACE_STYLE_USAGE(.BOTH.,#83414);
#83400=SURFACE_STYLE_USAGE(.BOTH.,#83415);
#83401=SURFACE_STYLE_USAGE(.BOTH.,#83416);
#83402=SURFACE_STYLE_USAGE(.BOTH.,#83417);
#83403=SURFACE_STYLE_USAGE(.BOTH.,#83418);
#83404=SURFACE_STYLE_USAGE(.BOTH.,#83419);
#83405=SURFACE_STYLE_USAGE(.BOTH.,#83420);
#83406=SURFACE_STYLE_USAGE(.BOTH.,#83421);
#83407=SURFACE_STYLE_USAGE(.BOTH.,#83422);
#83408=SURFACE_SIDE_STYLE('',(#83423));
#83409=SURFACE_SIDE_STYLE('',(#83424));
#83410=SURFACE_SIDE_STYLE('',(#83425));
#83411=SURFACE_SIDE_STYLE('',(#83426));
#83412=SURFACE_SIDE_STYLE('',(#83427));
#83413=SURFACE_SIDE_STYLE('',(#83428));
#83414=SURFACE_SIDE_STYLE('',(#83429));
#83415=SURFACE_SIDE_STYLE('',(#83430));
#83416=SURFACE_SIDE_STYLE('',(#83431));
#83417=SURFACE_SIDE_STYLE('',(#83432));
#83418=SURFACE_SIDE_STYLE('',(#83433));
#83419=SURFACE_SIDE_STYLE('',(#83434));
#83420=SURFACE_SIDE_STYLE('',(#83435));
#83421=SURFACE_SIDE_STYLE('',(#83436));
#83422=SURFACE_SIDE_STYLE('',(#83437));
#83423=SURFACE_STYLE_FILL_AREA(#83438);
#83424=SURFACE_STYLE_FILL_AREA(#83439);
#83425=SURFACE_STYLE_FILL_AREA(#83440);
#83426=SURFACE_STYLE_FILL_AREA(#83441);
#83427=SURFACE_STYLE_FILL_AREA(#83442);
#83428=SURFACE_STYLE_FILL_AREA(#83443);
#83429=SURFACE_STYLE_FILL_AREA(#83444);
#83430=SURFACE_STYLE_FILL_AREA(#83445);
#83431=SURFACE_STYLE_FILL_AREA(#83446);
#83432=SURFACE_STYLE_FILL_AREA(#83447);
#83433=SURFACE_STYLE_FILL_AREA(#83448);
#83434=SURFACE_STYLE_FILL_AREA(#83449);
#83435=SURFACE_STYLE_FILL_AREA(#83450);
#83436=SURFACE_STYLE_FILL_AREA(#83451);
#83437=SURFACE_STYLE_FILL_AREA(#83452);
#83438=FILL_AREA_STYLE('Steel - Satin',(#83453));
#83439=FILL_AREA_STYLE('Opaque(222,225,230)',(#83454));
#83440=FILL_AREA_STYLE('Opaque(218,221,226)',(#83455));
#83441=FILL_AREA_STYLE('Opaque(190,194,200)',(#83456));
#83442=FILL_AREA_STYLE('Opaque(238,239,241)',(#83457));
#83443=FILL_AREA_STYLE('Opaque(196,201,207)',(#83458));
#83444=FILL_AREA_STYLE('Opaque(228,231,235)',(#83459));
#83445=FILL_AREA_STYLE('Opaque(206,210,216)',(#83460));
#83446=FILL_AREA_STYLE('Opaque(200,204,210)',(#83461));
#83447=FILL_AREA_STYLE('Opaque(212,215,220)',(#83462));
#83448=FILL_AREA_STYLE('Opaque(199,204,210)',(#83463));
#83449=FILL_AREA_STYLE('Opaque(201,205,211)',(#83464));
#83450=FILL_AREA_STYLE('Opaque(197,202,208)',(#83465));
#83451=FILL_AREA_STYLE('Opaque(234,236,239)',(#83466));
#83452=FILL_AREA_STYLE('Opaque(203,207,213)',(#83467));
#83453=FILL_AREA_STYLE_COLOUR('Steel - Satin',#83468);
#83454=FILL_AREA_STYLE_COLOUR('Opaque(222,225,230)',#83469);
#83455=FILL_AREA_STYLE_COLOUR('Opaque(218,221,226)',#83470);
#83456=FILL_AREA_STYLE_COLOUR('Opaque(190,194,200)',#83471);
#83457=FILL_AREA_STYLE_COLOUR('Opaque(238,239,241)',#83472);
#83458=FILL_AREA_STYLE_COLOUR('Opaque(196,201,207)',#83473);
#83459=FILL_AREA_STYLE_COLOUR('Opaque(228,231,235)',#83474);
#83460=FILL_AREA_STYLE_COLOUR('Opaque(206,210,216)',#83475);
#83461=FILL_AREA_STYLE_COLOUR('Opaque(200,204,210)',#83476);
#83462=FILL_AREA_STYLE_COLOUR('Opaque(212,215,220)',#83477);
#83463=FILL_AREA_STYLE_COLOUR('Opaque(199,204,210)',#83478);
#83464=FILL_AREA_STYLE_COLOUR('Opaque(201,205,211)',#83479);
#83465=FILL_AREA_STYLE_COLOUR('Opaque(197,202,208)',#83480);
#83466=FILL_AREA_STYLE_COLOUR('Opaque(234,236,239)',#83481);
#83467=FILL_AREA_STYLE_COLOUR('Opaque(203,207,213)',#83482);
#83468=COLOUR_RGB('Steel - Satin', 0.66274510, 0.83137255, 0.94901961);
#83469=COLOUR_RGB('Opaque(222,225,230)', 0.66274510, 0.83137255, 0.94901961);
#83470=COLOUR_RGB('Opaque(218,221,226)', 0.31764706, 0.68627451, 0.89019608);
#83471=COLOUR_RGB('Opaque(190,194,200)', 0.40784314, 0.44705882, 0.49803922);
#83472=COLOUR_RGB('Opaque(238,239,241)', 0.72549020, 0.75294118, 0.79215686);
#83473=COLOUR_RGB('Opaque(196,201,207)', 0.08235294, 0.09019608, 0.10196078);
#83474=COLOUR_RGB('Opaque(228,231,235)', 0.09019608, 0.27058824, 0.51372549);
#83475=COLOUR_RGB('Opaque(206,210,216)', 0.66274510, 0.83137255, 0.94901961);
#83476=COLOUR_RGB('Opaque(200,204,210)', 0.31764706, 0.68627451, 0.89019608);
#83477=COLOUR_RGB('Opaque(212,215,220)', 0.40784314, 0.44705882, 0.49803922);
#83478=COLOUR_RGB('Opaque(199,204,210)', 0.72549020, 0.75294118, 0.79215686);
#83479=COLOUR_RGB('Opaque(201,205,211)', 0.08235294, 0.09019608, 0.10196078);
#83480=COLOUR_RGB('Opaque(197,202,208)', 0.09019608, 0.27058824, 0.51372549);
#83481=COLOUR_RGB('Opaque(234,236,239)', 0.66274510, 0.83137255, 0.94901961);
#83482=COLOUR_RGB('Opaque(203,207,213)', 0.31764706, 0.68627451, 0.89019608);
ENDSEC;
END-ISO-10303-21;
